#63533=CARTESIAN_POINT('Ctrl Pts',(-17.12616407896,-20.9460001987665,-5.54684314796685));
#63534=CARTESIAN_POINT('Ctrl Pts',(-17.1948942620563,-20.999513169412,-5.55115931070577));
#63535=CARTESIAN_POINT('Ctrl Pts',(-17.2661134846746,-21.0493576657609,
-5.55547547344469));
#63536=CARTESIAN_POINT('Ctrl Pts',(-17.3350127486071,-21.097578482884,-5.55965103763637));
#63537=CARTESIAN_POINT('Ctrl Pts',(-17.4062409575147,-21.1423659457519,
-5.56382660182805));
#63538=CARTESIAN_POINT('Ctrl Pts',(-17.4794157978407,-21.183505877136,-5.56800216601973));
#63539=CARTESIAN_POINT('Ctrl Pts',(-17.5562865253949,-21.2267236886533,
-5.57238862803227));
#63540=CARTESIAN_POINT('Ctrl Pts',(-17.6353051780177,-21.2659155519541,
-5.57677509004481));
#63541=CARTESIAN_POINT('Ctrl Pts',(-17.7160039105556,-21.3008899424784,
-5.58116155205735));
#63542=CARTESIAN_POINT('Ctrl Pts',(-17.7967026430936,-21.3358643330026,
-5.5855480140699));
#63543=CARTESIAN_POINT('Ctrl Pts',(-17.8790808853744,-21.3666211190642,
-5.58993447608243));
#63544=CARTESIAN_POINT('Ctrl Pts',(-17.9626538344086,-21.393029514944,-5.59432093809497));
#63545=CARTESIAN_POINT('Ctrl Pts',(-18.042381468173,-21.4182228213826,-5.59850557248802));
#63546=CARTESIAN_POINT('Ctrl Pts',(-18.123493045634,-21.4395528703718,-5.60269020688107));
#63547=CARTESIAN_POINT('Ctrl Pts',(-18.2055793173495,-21.4568695738795,
-5.60687484127412));
#63548=CARTESIAN_POINT('Ctrl Pts',(-18.2875487494174,-21.474161629203,-5.61105351935806));
#63549=CARTESIAN_POINT('Ctrl Pts',(-18.370489673737,-21.4874515917234,-5.615232197442));
#63550=CARTESIAN_POINT('Ctrl Pts',(-18.4539769469565,-21.4966388918203,
-5.61941087552594));
#63551=CARTESIAN_POINT('Ctrl Pts',(-18.5389606695472,-21.5059908676685,
-5.62366445341137));
#63552=CARTESIAN_POINT('Ctrl Pts',(-18.624510060566,-21.511091508697,-5.62791803129681));
#63553=CARTESIAN_POINT('Ctrl Pts',(-18.7101649534091,-21.5118890387191,
-5.63217160918224));
#63554=CARTESIAN_POINT('Ctrl Pts',(-18.7941592590127,-21.5126711070654,
-5.63634272316019));
#63555=CARTESIAN_POINT('Ctrl Pts',(-18.87825453103,-21.5093154194064,-5.64051383713815));
#63556=CARTESIAN_POINT('Ctrl Pts',(-18.9620126684401,-21.5018255279589,
-5.6446849511161));
#63557=CARTESIAN_POINT('Ctrl Pts',(-19.0457426999984,-21.4943381498168,
-5.64885466543647));
#63558=CARTESIAN_POINT('Ctrl Pts',(-19.1291353638018,-21.4827193639704,
-5.65302437975684));
#63559=CARTESIAN_POINT('Ctrl Pts',(-19.2117557819361,-21.4670247340387,
-5.65719409407722));
#63560=CARTESIAN_POINT('Ctrl Pts',(-19.2943732600814,-21.4513306625894,
-5.66136366002126));
#63561=CARTESIAN_POINT('Ctrl Pts',(-19.3762180954026,-21.4315611221138,
-5.66553322596531));
#63562=CARTESIAN_POINT('Ctrl Pts',(-19.4568650837657,-21.4078228907379,
-5.66970279190935));
#63563=CARTESIAN_POINT('Ctrl Pts',(-19.5403475207508,-21.3832500524311,
-5.67401895464827));
#63564=CARTESIAN_POINT('Ctrl Pts',(-19.6225458049915,-21.3544244012911,
-5.67833511738719));
#63565=CARTESIAN_POINT('Ctrl Pts',(-19.7030067527822,-21.3215201862534,
-5.68265128012611));
#63566=CARTESIAN_POINT('Ctrl Pts',(-19.7808466936617,-21.2896878225597,
-5.68682684431779));
#63567=CARTESIAN_POINT('Ctrl Pts',(-19.8570603406958,-21.2540387751659,
-5.69100240850947));
#63568=CARTESIAN_POINT('Ctrl Pts',(-19.9312606656523,-21.214778579199,-5.69517797270115));
#63569=CARTESIAN_POINT('Ctrl Pts',(-20.0092086726279,-21.173535444066,-5.69956443471369));
#63570=CARTESIAN_POINT('Ctrl Pts',(-20.0849341253745,-21.1283070744553,
-5.70395089672623));
#63571=CARTESIAN_POINT('Ctrl Pts',(-20.1580227463384,-21.0793831854912,
-5.70833735873878));
#63572=CARTESIAN_POINT('Ctrl Pts',(-20.2311113673023,-21.0304592965271,
-5.71272382075132));
#63573=CARTESIAN_POINT('Ctrl Pts',(-20.3015627371329,-20.977840296355,-5.71711028276386));
#63574=CARTESIAN_POINT('Ctrl Pts',(-20.3690044710744,-20.9218630357379,
-5.72149674477641));
#63575=CARTESIAN_POINT('Ctrl Pts',(-20.4324580482223,-20.8691959820087,
-5.72562381401755));
#63576=CARTESIAN_POINT('Ctrl Pts',(-20.493497997814,-20.8133485129555,-5.72975088325869));
#63577=CARTESIAN_POINT('Ctrl Pts',(-20.5517814829091,-20.7545732940418,
-5.73387795249983));
#63578=CARTESIAN_POINT('Ctrl Pts',(-20.6102782700971,-20.6955829734199,
-5.73802012571948));
#63579=CARTESIAN_POINT('Ctrl Pts',(-20.6659979620833,-20.6336436795686,
-5.74216229893913));
#63580=CARTESIAN_POINT('Ctrl Pts',(-20.7186255971236,-20.5690532580103,
-5.74630447215879));
#63581=CARTESIAN_POINT('Ctrl Pts',(-20.7709257203661,-20.5048647949491,
-5.75042086784546));
#63582=CARTESIAN_POINT('Ctrl Pts',(-20.8201718394842,-20.4380584608902,
-5.75453726353214));
#63583=CARTESIAN_POINT('Ctrl Pts',(-20.8660914253506,-20.368963709467,-5.75865365921881));
#63584=CARTESIAN_POINT('Ctrl Pts',(-20.9119829684086,-20.299911153783,-5.76276754104798));
#63585=CARTESIAN_POINT('Ctrl Pts',(-20.9545517475122,-20.228573347296,-5.76688142287715));
#63586=CARTESIAN_POINT('Ctrl Pts',(-20.993566969393,-20.1553108953334,-5.77099530470633));
#63587=CARTESIAN_POINT('Ctrl Pts',(-21.0325708263852,-20.0820697842621,
-5.77510798818761));
#63588=CARTESIAN_POINT('Ctrl Pts',(-21.0680229592545,-20.006905559054,-5.7792206716689));
#63589=CARTESIAN_POINT('Ctrl Pts',(-21.0997379788823,-19.9302043831808,
-5.78333335515018));
#63590=CARTESIAN_POINT('Ctrl Pts',(-21.1318415000294,-19.8525636359715,
-5.78749641803529));
#63591=CARTESIAN_POINT('Ctrl Pts',(-21.1601155043872,-19.7733484709675,
-5.7916594809204));
#63592=CARTESIAN_POINT('Ctrl Pts',(-21.1844181339265,-19.6929797358392,
-5.79582254380551));
#63593=CARTESIAN_POINT('Ctrl Pts',(-21.2084475698834,-19.6135144512045,
-5.79993880837766));
#63594=CARTESIAN_POINT('Ctrl Pts',(-21.2285944016387,-19.5329218806182,
-5.80405507294981));
#63595=CARTESIAN_POINT('Ctrl Pts',(-21.2447724368935,-19.45162162697,-5.80817133752195));
#63596=CARTESIAN_POINT('Ctrl Pts',(-21.2612263672263,-19.3689349046021,
-5.81235779956354));
#63597=CARTESIAN_POINT('Ctrl Pts',(-21.2735747867911,-19.2855166404038,
-5.81654426160514));
#63598=CARTESIAN_POINT('Ctrl Pts',(-21.281781944964,-19.2018142528271,-5.82073072364673));
#63599=CARTESIAN_POINT('Ctrl Pts',(-21.2899891031369,-19.1181118652504,
-5.82491718568832));
#63600=CARTESIAN_POINT('Ctrl Pts',(-21.2940550344004,-19.0341258661346,
-5.82910364772991));
#63601=CARTESIAN_POINT('Ctrl Pts',(-21.2939994369002,-18.9503020392335,
-5.8332901097715));
#63602=CARTESIAN_POINT('Ctrl Pts',(-21.2967673690372,-18.950300203358,-5.8332901097715));
#63603=CARTESIAN_POINT('Ctrl Pts',(-21.2975539709192,-18.8475231740461,
-5.83841759033362));
#63604=CARTESIAN_POINT('Ctrl Pts',(-21.2452320420947,-17.8958349639979,
-5.88593700645621));
#63605=CARTESIAN_POINT('Ctrl Pts',(-20.0538051353946,-16.2277743551153,
-5.97584835813928));
#63606=CARTESIAN_POINT('Ctrl Pts',(-18.0187464898779,-16.3260865960557,
-6.06521460732434));
#63607=CARTESIAN_POINT('Ctrl Pts',(-17.2449841505655,-16.8629690205255,
-6.11218892094892));
#63608=CARTESIAN_POINT('Ctrl Pts',(-17.1725993332886,-16.9194746534894,
-6.11677129901302));
#63609=CARTESIAN_POINT('',(-21.2939992944986,-18.9539005700933,-5.76670989019962));
#63610=CARTESIAN_POINT('Ctrl Pts',(-21.293999294499,-18.9539005695104,-5.76670989022851));
#63611=CARTESIAN_POINT('Ctrl Pts',(-21.2940618231948,-18.8696766480678,
-5.77088500205647));
#63612=CARTESIAN_POINT('Ctrl Pts',(-21.2899635861128,-18.7854119279347,
-5.77506011388444));
#63613=CARTESIAN_POINT('Ctrl Pts',(-21.2817191504239,-18.7015461508316,
-5.7792352257124));
#63614=CARTESIAN_POINT('Ctrl Pts',(-21.2734754980237,-18.6176883416611,
-5.78340994087069));
#63615=CARTESIAN_POINT('Ctrl Pts',(-21.2610864747303,-18.5342298557722,
-5.78758465602898));
#63616=CARTESIAN_POINT('Ctrl Pts',(-21.2446185572459,-18.4516056954637,
-5.79175937118727));
#63617=CARTESIAN_POINT('Ctrl Pts',(-21.2281473245846,-18.3689649019827,
-5.79593492676267));
#63618=CARTESIAN_POINT('Ctrl Pts',(-21.2075956572652,-18.2871592164316,
-5.80011048233806));
#63619=CARTESIAN_POINT('Ctrl Pts',(-21.1830809475489,-18.2066125085882,
-5.80428603791345));
#63620=CARTESIAN_POINT('Ctrl Pts',(-21.1585369190254,-18.1259694694636,
-5.8084665873195));
#63621=CARTESIAN_POINT('Ctrl Pts',(-21.1300205198882,-18.0465888526481,
-5.81264713672554));
#63622=CARTESIAN_POINT('Ctrl Pts',(-21.0976986239761,-17.9688780263805,
-5.81682768613158));
#63623=CARTESIAN_POINT('Ctrl Pts',(-21.065355928357,-17.8911171918331,-5.8210109257945));
#63624=CARTESIAN_POINT('Ctrl Pts',(-21.0292030575735,-17.8150287001824,
-5.82519416545742));
#63625=CARTESIAN_POINT('Ctrl Pts',(-20.9894534545794,-17.740996402059,-5.82937740512034));
#63626=CARTESIAN_POINT('Ctrl Pts',(-20.949632004209,-17.6668302906149,-5.83356820598567));
#63627=CARTESIAN_POINT('Ctrl Pts',(-20.9062010761476,-17.5947281861657,
-5.83775900685099));
#63628=CARTESIAN_POINT('Ctrl Pts',(-20.859418003607,-17.5250457926257,-5.84194980771632));
#63629=CARTESIAN_POINT('Ctrl Pts',(-20.8291383592866,-17.4799449051208,
-5.84466224092621));
#63630=CARTESIAN_POINT('Ctrl Pts',(-20.7974553185201,-17.435857034571,-5.84737467413609));
#63631=CARTESIAN_POINT('Ctrl Pts',(-20.7644472985012,-17.392870830236,-5.85008710734598));
#63632=CARTESIAN_POINT('Ctrl Pts',(-20.7135238341689,-17.3265534188316,
-5.85427174173903));
#63633=CARTESIAN_POINT('Ctrl Pts',(-20.6592531496868,-17.262610070515,-5.85845637613208));
#63634=CARTESIAN_POINT('Ctrl Pts',(-20.6018847443059,-17.2013982228989,
-5.86264101052513));
#63635=CARTESIAN_POINT('Ctrl Pts',(-20.5445979957492,-17.1402735027715,
-5.86681968860907));
#63636=CARTESIAN_POINT('Ctrl Pts',(-20.4842225962896,-17.0818728934348,
-5.87099836669301));
#63637=CARTESIAN_POINT('Ctrl Pts',(-20.4210494366143,-17.0265223453856,
-5.87517704477696));
#63638=CARTESIAN_POINT('Ctrl Pts',(-20.3567439434536,-16.9701796785424,
-5.87943062266239));
#63639=CARTESIAN_POINT('Ctrl Pts',(-20.2895396974698,-16.9169978755988,
-5.88368420054783));
#63640=CARTESIAN_POINT('Ctrl Pts',(-20.2197842460677,-16.867282951061,-5.88793777843326));
#63641=CARTESIAN_POINT('Ctrl Pts',(-20.1513811402077,-16.8185318473461,
-5.89210889241121));
#63642=CARTESIAN_POINT('Ctrl Pts',(-20.0805252582504,-16.7731146765031,
-5.89628000638917));
#63643=CARTESIAN_POINT('Ctrl Pts',(-20.0075777510545,-16.7312794610715,
-5.90045112036712));
#63644=CARTESIAN_POINT('Ctrl Pts',(-19.9346547220991,-16.6894582838504,
-5.90462083468749));
#63645=CARTESIAN_POINT('Ctrl Pts',(-19.8596418605523,-16.6512169036013,
-5.90879054900787));
#63646=CARTESIAN_POINT('Ctrl Pts',(-19.7829274662086,-16.6167588624227,
-5.91296026332824));
#63647=CARTESIAN_POINT('Ctrl Pts',(-19.7062158016923,-16.5823020474091,
-5.91712982927229));
#63648=CARTESIAN_POINT('Ctrl Pts',(-19.6278031447566,-16.5516284915072,
-5.92129939521634));
#63649=CARTESIAN_POINT('Ctrl Pts',(-19.5480992,-16.5248942147983,-5.92546896116038));
#63650=CARTESIAN_POINT('Ctrl Pts',(-19.4655929628713,-16.4972199939008,
-5.9297851238993));
#63651=CARTESIAN_POINT('Ctrl Pts',(-19.3817034451241,-16.4737673840696,
-5.93410128663822));
#63652=CARTESIAN_POINT('Ctrl Pts',(-19.2969019322694,-16.4546531248848,
-5.93841744937714));
#63653=CARTESIAN_POINT('Ctrl Pts',(-19.2148628197763,-16.4361615106825,
-5.94259301356882));
#63654=CARTESIAN_POINT('Ctrl Pts',(-19.1319706883696,-16.4217299783601,
-5.9467685777605));
#63655=CARTESIAN_POINT('Ctrl Pts',(-19.0486605152115,-16.411411729507,-5.95094414195218));
#63656=CARTESIAN_POINT('Ctrl Pts',(-18.9611425432584,-16.4005723304336,
-5.95533060396472));
#63657=CARTESIAN_POINT('Ctrl Pts',(-18.8731637715279,-16.3942727005953,
-5.95971706597726));
#63658=CARTESIAN_POINT('Ctrl Pts',(-18.7852297301449,-16.3925126461048,
-5.9641035279898));
#63659=CARTESIAN_POINT('Ctrl Pts',(-18.6972956887618,-16.3907525916143,
-5.96848999000234));
#63660=CARTESIAN_POINT('Ctrl Pts',(-18.609406955249,-16.3935320181048,-5.97287645201488));
#63661=CARTESIAN_POINT('Ctrl Pts',(-18.5220617179687,-16.4007880988421,
-5.97726291402742));
#63662=CARTESIAN_POINT('Ctrl Pts',(-18.4387429644685,-16.4077096851948,
-5.98144716675304));
#63663=CARTESIAN_POINT('Ctrl Pts',(-18.3556086019078,-16.4187300407395,
-5.98563141947867));
#63664=CARTESIAN_POINT('Ctrl Pts',(-18.273094108763,-16.4338328571314,-5.98981567220429));
#63665=CARTESIAN_POINT('Ctrl Pts',(-18.190691343874,-16.4489152236451,-5.99399425926754));
#63666=CARTESIAN_POINT('Ctrl Pts',(-18.1089072302701,-16.4680689925798,
-5.99817284633079));
#63667=CARTESIAN_POINT('Ctrl Pts',(-18.0281732667358,-16.4912260114733,
-6.00235143339404));
#63668=CARTESIAN_POINT('Ctrl Pts',(-17.9475320674901,-16.5143564226754,
-6.00652521921084));
#63669=CARTESIAN_POINT('Ctrl Pts',(-17.8679390598742,-16.541480815389,-6.01069900502764));
#63670=CARTESIAN_POINT('Ctrl Pts',(-17.7898152017669,-16.572480076405,-6.01487279084444));
#63671=CARTESIAN_POINT('Ctrl Pts',(-17.7117448631501,-16.603458101083,-6.01904371736965));
#63672=CARTESIAN_POINT('Ctrl Pts',(-17.6351421012726,-16.6383055523455,
-6.02321464389486));
#63673=CARTESIAN_POINT('Ctrl Pts',(-17.5604112612823,-16.6768539668067,
-6.02738557042007));
#63674=CARTESIAN_POINT('Ctrl Pts',(-17.4856945971113,-16.7153950689542,
-6.03155570575518));
#63675=CARTESIAN_POINT('Ctrl Pts',(-17.4128495626117,-16.7576355380395,
-6.0357258410903));
#63676=CARTESIAN_POINT('Ctrl Pts',(-17.3422580869924,-16.8033598608474,
-6.03989597642541));
#63677=CARTESIAN_POINT('Ctrl Pts',(-17.2847682206377,-16.8405978585563,
-6.04329214460284));
#63678=CARTESIAN_POINT('Ctrl Pts',(-17.2287727032861,-16.8801455850515,
-6.04668831278028));
#63679=CARTESIAN_POINT('Ctrl Pts',(-17.1744641548914,-16.9218650419685,
-6.05008448095771));
#63680=CARTESIAN_POINT('Ctrl Pts',(-17.1744641548914,-16.9218650419685,
-5.25018234058848));
#63681=CARTESIAN_POINT('Ctrl Pts',(-17.1078622797925,-16.9730281487153,
-5.25435377231504));
#63682=CARTESIAN_POINT('Ctrl Pts',(-17.0437276383886,-17.0275129995409,
-5.25852520404159));
#63683=CARTESIAN_POINT('Ctrl Pts',(-16.9824037471442,-17.0850477866369,
-5.26269663576815));
#63684=CARTESIAN_POINT('Ctrl Pts',(-16.9211031913488,-17.1425606801436,
-5.26686648014873));
#63685=CARTESIAN_POINT('Ctrl Pts',(-16.8626115968344,-17.2031208907266,
-5.27103632452931));
#63686=CARTESIAN_POINT('Ctrl Pts',(-16.8072380311628,-17.2664175144946,
-5.27520616890989));
#63687=CARTESIAN_POINT('Ctrl Pts',(-16.7518689259269,-17.329709039611,-5.27937567740234));
#63688=CARTESIAN_POINT('Ctrl Pts',(-16.6996176528133,-17.3957361932332,
-5.2835451858948));
#63689=CARTESIAN_POINT('Ctrl Pts',(-16.6507542226063,-17.4641535593445,
-5.28771469438725));
#63690=CARTESIAN_POINT('Ctrl Pts',(-16.6018800708253,-17.5325859375384,
-5.29188511774986));
#63691=CARTESIAN_POINT('Ctrl Pts',(-16.556395504268,-17.603409194585,-5.29605554111247));
#63692=CARTESIAN_POINT('Ctrl Pts',(-16.514527493463,-17.676248538027,-5.30022596447508));
#63693=CARTESIAN_POINT('Ctrl Pts',(-16.4726122042834,-17.7491701334243,
-5.30440109718101));
#63694=CARTESIAN_POINT('Ctrl Pts',(-16.4343218488226,-17.8241119583259,
-5.30857622988695));
#63695=CARTESIAN_POINT('Ctrl Pts',(-16.3998373803061,-17.9006747102711,
-5.31275136259289));
#63696=CARTESIAN_POINT('Ctrl Pts',(-16.3653298237343,-17.9772887225407,
-5.31692929063536));
#63697=CARTESIAN_POINT('Ctrl Pts',(-16.3346333926338,-18.0555253938272,
-5.32110721867783));
#63698=CARTESIAN_POINT('Ctrl Pts',(-16.307879983328,-18.134967770095,-5.32528514672029));
#63699=CARTESIAN_POINT('Ctrl Pts',(-16.2810838554183,-18.2145369962668,
-5.3294697458846));
#63700=CARTESIAN_POINT('Ctrl Pts',(-16.2582434356432,-18.2953153270739,
-5.3336543450489));
#63701=CARTESIAN_POINT('Ctrl Pts',(-16.2394399881205,-18.3768736250774,
-5.3378389442132));
#63702=CARTESIAN_POINT('Ctrl Pts',(-16.2341302779918,-18.3999040252453,
-5.33902058968222));
#63703=CARTESIAN_POINT('Ctrl Pts',(-16.2291421521855,-18.4229965796705,
-5.34020223515123));
#63704=CARTESIAN_POINT('Ctrl Pts',(-16.2244766916358,-18.4461415565825,
-5.34138388062024));
#63705=CARTESIAN_POINT('Ctrl Pts',(-16.2079546068079,-18.5281062989289,
-5.34556851501329));
#63706=CARTESIAN_POINT('Ctrl Pts',(-16.1954216323759,-18.6110338790213,
-5.34975314940633));
#63707=CARTESIAN_POINT('Ctrl Pts',(-16.1869832270606,-18.6945013429833,
-5.35393778379938));
#63708=CARTESIAN_POINT('Ctrl Pts',(-16.1785568327709,-18.7778500013414,
-5.35811646188331));
#63709=CARTESIAN_POINT('Ctrl Pts',(-16.1742134770096,-18.8617365633851,
-5.36229513996724));
#63710=CARTESIAN_POINT('Ctrl Pts',(-16.174007684269,-18.9457275683916,-5.36647381805118));
#63711=CARTESIAN_POINT('Ctrl Pts',(-16.1737982028414,-19.0312240517999,
-5.37072739593661));
#63712=CARTESIAN_POINT('Ctrl Pts',(-16.1778761703229,-19.1168282866473,
-5.37498097382205));
#63713=CARTESIAN_POINT('Ctrl Pts',(-16.1862438519478,-19.2020772082025,
-5.37923455170749));
#63714=CARTESIAN_POINT('Ctrl Pts',(-16.1944493097363,-19.2856734130638,
-5.38340566568544));
#63715=CARTESIAN_POINT('Ctrl Pts',(-16.2067795899914,-19.3689274796561,
-5.38757677966339));
#63716=CARTESIAN_POINT('Ctrl Pts',(-16.2231843067497,-19.4514041995496,
-5.39174789364134));
#63717=CARTESIAN_POINT('Ctrl Pts',(-16.2395835187467,-19.5338532435831,
-5.39591760796171));
#63718=CARTESIAN_POINT('Ctrl Pts',(-16.2600543622647,-19.6155250081436,
-5.40008732228208));
#63719=CARTESIAN_POINT('Ctrl Pts',(-16.2844950829499,-19.6959930519482,
-5.40425703660244));
#63720=CARTESIAN_POINT('Ctrl Pts',(-16.3089349339293,-19.7764582323547,
-5.40842660254649));
#63721=CARTESIAN_POINT('Ctrl Pts',(-16.3373442466931,-19.8557193372403,
-5.41259616849054));
#63722=CARTESIAN_POINT('Ctrl Pts',(-16.3695713807102,-19.9333650209191,
-5.41676573443458));
#63723=CARTESIAN_POINT('Ctrl Pts',(-16.4029315810029,-20.0137406310497,
-5.42108189717351));
#63724=CARTESIAN_POINT('Ctrl Pts',(-16.4403828646775,-20.0923846228539,
-5.42539805991243));
#63725=CARTESIAN_POINT('Ctrl Pts',(-16.4817035150007,-20.1688650474311,
-5.42971422265136));
#63726=CARTESIAN_POINT('Ctrl Pts',(-16.5216781494857,-20.2428541302221,
-5.43388978684304));
#63727=CARTESIAN_POINT('Ctrl Pts',(-16.5652736482193,-20.3148180591345,
-5.43806535103472));
#63728=CARTESIAN_POINT('Ctrl Pts',(-16.6122442629254,-20.3843940073146,
-5.44224091522641));
#63729=CARTESIAN_POINT('Ctrl Pts',(-16.6615872517182,-20.4574840712362,
-5.44662737723895));
#63730=CARTESIAN_POINT('Ctrl Pts',(-16.7146549198489,-20.5279381144878,
-5.4510138392515));
#63731=CARTESIAN_POINT('Ctrl Pts',(-16.7711149075846,-20.5953752200801,
-5.45540030126404));
#63732=CARTESIAN_POINT('Ctrl Pts',(-16.8275748953203,-20.6628123256725,
-5.45978676327659));
#63733=CARTESIAN_POINT('Ctrl Pts',(-16.8874267520076,-20.7272321203105,
-5.46417322528913));
#63734=CARTESIAN_POINT('Ctrl Pts',(-16.9502957329767,-20.788300380603,-5.46855968730168));
#63735=CARTESIAN_POINT('Ctrl Pts',(-17.0102720189371,-20.8465587997145,
-5.47274432169472));
#63736=CARTESIAN_POINT('Ctrl Pts',(-17.0732171288673,-20.9019841740837,
-5.47692895608777));
#63737=CARTESIAN_POINT('Ctrl Pts',(-17.1388325082967,-20.9542588927042,
-5.48111359048082));
#63738=CARTESIAN_POINT('Ctrl Pts',(-17.204354492355,-21.006459204733,-5.48529226856475));
#63739=CARTESIAN_POINT('Ctrl Pts',(-17.2725388396022,-21.0555174845771,
-5.48947094664869));
#63740=CARTESIAN_POINT('Ctrl Pts',(-17.3430505912408,-21.1011532616992,
-5.49364962473263));
#63741=CARTESIAN_POINT('Ctrl Pts',(-17.4148262153517,-21.1476070273285,
-5.49790320261807));
#63742=CARTESIAN_POINT('Ctrl Pts',(-17.4890131561474,-21.190514050739,-5.5021567805035));
#63743=CARTESIAN_POINT('Ctrl Pts',(-17.5652232755989,-21.2296217790709,
-5.50641035838894));
#63744=CARTESIAN_POINT('Ctrl Pts',(-17.6399559131731,-21.2679713277767,
-5.5105814723669));
#63745=CARTESIAN_POINT('Ctrl Pts',(-17.7166335547755,-21.3026673605994,
-5.51475258634485));
#63746=CARTESIAN_POINT('Ctrl Pts',(-17.7948629860233,-21.3335166740921,
-5.51892370032281));
#63747=CARTESIAN_POINT('Ctrl Pts',(-17.8730661666299,-21.3643556357998,
-5.52309341464318));
#63748=CARTESIAN_POINT('Ctrl Pts',(-17.9528196751245,-21.3913502731114,
-5.52726312896355));
#63749=CARTESIAN_POINT('Ctrl Pts',(-18.0337098641723,-21.4143553207574,
-5.53143284328393));
#63750=CARTESIAN_POINT('Ctrl Pts',(-18.1145971747999,-21.4373595497851,
-5.53560240922797));
#63751=CARTESIAN_POINT('Ctrl Pts',(-18.1966206428405,-21.4563743463907,
-5.53977197517201));
#63752=CARTESIAN_POINT('Ctrl Pts',(-18.2793523115258,-21.4713045626452,
-5.54394154111605));
#63753=CARTESIAN_POINT('Ctrl Pts',(-18.3649927236217,-21.4867597068849,
-5.54825770385497));
#63754=CARTESIAN_POINT('Ctrl Pts',(-18.4513915445807,-21.497837605271,-5.55257386659389));
#63755=CARTESIAN_POINT('Ctrl Pts',(-18.5380655626724,-21.5044908807416,
-5.55689002933282));
#63756=CARTESIAN_POINT('Ctrl Pts',(-18.6219161837412,-21.5109274264635,
-5.5610655935245));
#63757=CARTESIAN_POINT('Ctrl Pts',(-18.7060238760283,-21.5132232209822,
-5.56524115771618));
#63758=CARTESIAN_POINT('Ctrl Pts',(-18.7899505406875,-21.5113885084131,
-5.56941672190786));
#63759=CARTESIAN_POINT('Ctrl Pts',(-18.8781161416618,-21.5094611288736,
-5.5738031839204));
#63760=CARTESIAN_POINT('Ctrl Pts',(-18.9660813646935,-21.5029750554617,
-5.57818964593294));
#63761=CARTESIAN_POINT('Ctrl Pts',(-19.0533460188562,-21.492003566974,-5.58257610794549));
#63762=CARTESIAN_POINT('Ctrl Pts',(-19.140610673019,-21.4810320784863,-5.58696256995803));
#63763=CARTESIAN_POINT('Ctrl Pts',(-19.2271742005006,-21.4655753517935,
-5.59134903197057));
#63764=CARTESIAN_POINT('Ctrl Pts',(-19.3125527301388,-21.4457675790757,
-5.59573549398311));
#63765=CARTESIAN_POINT('Ctrl Pts',(-19.394002867067,-21.4268711913428,-5.59992012837616));
#63766=CARTESIAN_POINT('Ctrl Pts',(-19.4746778298126,-21.4039450190917,
-5.60410476276921));
#63767=CARTESIAN_POINT('Ctrl Pts',(-19.55414895591,-21.3770681825713,-5.60828939716226));
#63768=CARTESIAN_POINT('Ctrl Pts',(-19.6335069646959,-21.350229601901,-5.6124680752462));
#63769=CARTESIAN_POINT('Ctrl Pts',(-19.7116641083503,-21.3194516726887,
-5.61664675333015));
#63770=CARTESIAN_POINT('Ctrl Pts',(-19.7882032486926,-21.2848642288924,
-5.62082543141409));
#63771=CARTESIAN_POINT('Ctrl Pts',(-19.8661142981179,-21.2496568300237,
-5.62507900929953));
#63772=CARTESIAN_POINT('Ctrl Pts',(-19.9423482986086,-21.2105021111285,
-5.62933258718496));
#63773=CARTESIAN_POINT('Ctrl Pts',(-20.0164828014234,-21.167589732792,-5.63358616507039));
#63774=CARTESIAN_POINT('Ctrl Pts',(-20.0891800622396,-21.1255092946461,
-5.63775727904835));
#63775=CARTESIAN_POINT('Ctrl Pts',(-20.1598580881702,-21.079815837063,-5.6419283930263));
#63776=CARTESIAN_POINT('Ctrl Pts',(-20.2281415862037,-21.0307354137496,
-5.64609950700425));
#63777=CARTESIAN_POINT('Ctrl Pts',(-20.2964021710499,-20.9816714598463,
-5.65026922132462));
#63778=CARTESIAN_POINT('Ctrl Pts',(-20.3622694505382,-20.9292230656518,
-5.65443893564499));
#63779=CARTESIAN_POINT('Ctrl Pts',(-20.4253973801084,-20.8736594137782,
-5.65860864996536));
#63780=CARTESIAN_POINT('Ctrl Pts',(-20.4885230633161,-20.8180977390977,
-5.6627782159094));
#63781=CARTESIAN_POINT('Ctrl Pts',(-20.5489092456569,-20.7594213317292,
-5.66694778185344));
#63782=CARTESIAN_POINT('Ctrl Pts',(-20.6062442778983,-20.6979385338199,
-5.67111734779749));
#63783=CARTESIAN_POINT('Ctrl Pts',(-20.6655951391429,-20.6342940765832,
-5.67543351053641));
#63784=CARTESIAN_POINT('Ctrl Pts',(-20.7216759416721,-20.5676425973539,
-5.67974967327533));
#63785=CARTESIAN_POINT('Ctrl Pts',(-20.7741852955294,-20.4983647564225,
-5.68406583601425));
#63786=CARTESIAN_POINT('Ctrl Pts',(-20.8249841627079,-20.4313436338726,
-5.68824140020593));
#63787=CARTESIAN_POINT('Ctrl Pts',(-20.8724404611872,-20.3618650450197,
-5.69241696439762));
#63788=CARTESIAN_POINT('Ctrl Pts',(-20.9163256700511,-20.2903029066083,
-5.6965925285893));
#63789=CARTESIAN_POINT('Ctrl Pts',(-20.9624274164874,-20.2151263347086,
-5.70097899060184));
#63790=CARTESIAN_POINT('Ctrl Pts',(-21.0045875620259,-20.1376507144176,
-5.70536545261438));
#63791=CARTESIAN_POINT('Ctrl Pts',(-21.0425969786767,-20.0583362915701,
-5.70975191462692));
#63792=CARTESIAN_POINT('Ctrl Pts',(-21.0806063953274,-19.9790218687225,
-5.71413837663946));
#63793=CARTESIAN_POINT('Ctrl Pts',(-21.1144649298774,-19.897869208087,-5.718524838652));
#63794=CARTESIAN_POINT('Ctrl Pts',(-21.144023506431,-19.8153578044185,-5.72291130066454));
#63795=CARTESIAN_POINT('Ctrl Pts',(-21.1768030234138,-19.7238552940413,
-5.72777574688623));
#63796=CARTESIAN_POINT('Ctrl Pts',(-21.2043967060823,-19.6304025057852,
-5.73264019310792));
#63797=CARTESIAN_POINT('Ctrl Pts',(-21.2266026211961,-19.5355513454757,
-5.7375046393296));
#63798=CARTESIAN_POINT('Ctrl Pts',(-21.2488226674987,-19.4406398246877,
-5.74237218114127));
#63799=CARTESIAN_POINT('Ctrl Pts',(-21.2656479288596,-19.3443282665163,
-5.74723972295294));
#63800=CARTESIAN_POINT('Ctrl Pts',(-21.2769239065511,-19.2471914725919,
-5.75210726476461));
#63801=CARTESIAN_POINT('Ctrl Pts',(-21.2881998842426,-19.1500546786674,
-5.75697480657628));
#63802=CARTESIAN_POINT('Ctrl Pts',(-21.2939263955806,-19.0520927805187,
-5.76184234838795));
#63803=CARTESIAN_POINT('Ctrl Pts',(-21.2939992944986,-18.9539005700933,
-5.76670989019962));
#63804=CARTESIAN_POINT('Origin',(-18.734,-18.952,1.76670989022851));
#63805=CARTESIAN_POINT('',(-17.1718943060142,-16.9185142398779,-4.45010593052277));
#63806=CARTESIAN_POINT('',(-17.1769969348074,-16.9251725137323,-4.51667470085173));
#63807=CARTESIAN_POINT('',(-17.1744641548914,-16.9218650419685,1.76670989022851));
#63808=CARTESIAN_POINT('',(-21.2938494922829,-18.9508032548851,-5.03329016024732));
#63809=CARTESIAN_POINT('Ctrl Pts',(-17.1769969348074,-16.9251725137323,
-4.51667470085173));
#63810=CARTESIAN_POINT('Ctrl Pts',(-16.8552506861943,-17.1716046543912,
-4.53675462878232));
#63811=CARTESIAN_POINT('Ctrl Pts',(-16.0276178705895,-18.1629200290128,
-4.59922649227339));
#63812=CARTESIAN_POINT('Ctrl Pts',(-16.1629700483809,-20.5498410269921,
-4.70409029132494));
#63813=CARTESIAN_POINT('Ctrl Pts',(-18.6858816905041,-21.9787103574595,
-4.83126609800637));
#63814=CARTESIAN_POINT('Ctrl Pts',(-20.9008594909828,-20.8156360190963,
-4.94099937082189));
#63815=CARTESIAN_POINT('Ctrl Pts',(-21.288210216193,-19.4541225063383,-5.00834070807693));
#63816=CARTESIAN_POINT('Ctrl Pts',(-21.2903252254699,-18.9508059208324,
-5.0332901097715));
#63817=CARTESIAN_POINT('Ctrl Pts',(-21.2939997202205,-18.9508031412445,
-5.03329016239894));
#63818=CARTESIAN_POINT('Ctrl Pts',(-21.2939564765218,-18.8583078019835,
-5.03786858507833));
#63819=CARTESIAN_POINT('Ctrl Pts',(-21.2888961385929,-18.7659792628466,
-5.04244700775773));
#63820=CARTESIAN_POINT('Ctrl Pts',(-21.2788976615006,-18.6743385289801,
-5.04702543043713));
#63821=CARTESIAN_POINT('Ctrl Pts',(-21.2688681118673,-18.5824130006966,
-5.05161808160601));
#63822=CARTESIAN_POINT('Ctrl Pts',(-21.2538698091559,-18.4911798450256,
-5.05621073277489));
#63823=CARTESIAN_POINT('Ctrl Pts',(-21.2340326305246,-18.40114897993,-5.06080338394377));
#63824=CARTESIAN_POINT('Ctrl Pts',(-21.2141037578095,-18.3107019620212,
-5.06541726388461));
#63825=CARTESIAN_POINT('Ctrl Pts',(-21.1892913049386,-18.2214686542029,
-5.07003114382545));
#63826=CARTESIAN_POINT('Ctrl Pts',(-21.1597755903596,-18.1339457321084,
-5.0746450237663));
#63827=CARTESIAN_POINT('Ctrl Pts',(-21.1363775884172,-18.0645636578345,
-5.07830258630061));
#63828=CARTESIAN_POINT('Ctrl Pts',(-21.1100249393917,-17.9962560714796,
-5.08196014883493));
#63829=CARTESIAN_POINT('Ctrl Pts',(-21.0808281256644,-17.9292596866307,
-5.08561771136924));
#63830=CARTESIAN_POINT('Ctrl Pts',(-21.0474239145964,-17.8526088095457,
-5.08980234576229));
#63831=CARTESIAN_POINT('Ctrl Pts',(-21.0101982941979,-17.7774535557438,
-5.09398698015533));
#63832=CARTESIAN_POINT('Ctrl Pts',(-20.9693070771845,-17.7042010295369,
-5.09817161454838));
#63833=CARTESIAN_POINT('Ctrl Pts',(-20.9284740637572,-17.6310527692342,
-5.10235029263232));
#63834=CARTESIAN_POINT('Ctrl Pts',(-20.8839860396696,-17.5598022552459,
-5.10652897071627));
#63835=CARTESIAN_POINT('Ctrl Pts',(-20.8360465870686,-17.4908360304904,
-5.11070764880022));
#63836=CARTESIAN_POINT('Ctrl Pts',(-20.7872478542333,-17.4206336357213,
-5.11496122668565));
#63837=CARTESIAN_POINT('Ctrl Pts',(-20.7348729347517,-17.352798669429,-5.11921480457109));
#63838=CARTESIAN_POINT('Ctrl Pts',(-20.6791852047646,-17.2877120083456,
-5.12346838245653));
#63839=CARTESIAN_POINT('Ctrl Pts',(-20.6245770900889,-17.2238871791935,
-5.12763949643448));
#63840=CARTESIAN_POINT('Ctrl Pts',(-20.5667837820755,-17.1627054093254,
-5.13181061041243));
#63841=CARTESIAN_POINT('Ctrl Pts',(-20.5060958601737,-17.1044945839443,
-5.13598172439038));
#63842=CARTESIAN_POINT('Ctrl Pts',(-20.4454283026902,-17.0463032917677,
-5.14015143871076));
#63843=CARTESIAN_POINT('Ctrl Pts',(-20.3818683920876,-16.9910812823424,
-5.14432115303113));
#63844=CARTESIAN_POINT('Ctrl Pts',(-20.3157437934271,-16.9391198316952,
-5.1484908673515));
#63845=CARTESIAN_POINT('Ctrl Pts',(-20.2496215477636,-16.8871602300594,
-5.15266043329554));
#63846=CARTESIAN_POINT('Ctrl Pts',(-20.1809351577375,-16.8384612400848,
-5.15682999923958));
#63847=CARTESIAN_POINT('Ctrl Pts',(-20.1100445342429,-16.7932731901002,
-5.16099956518362));
#63848=CARTESIAN_POINT('Ctrl Pts',(-20.0366614838791,-16.7464963840235,
-5.16531572792255));
#63849=CARTESIAN_POINT('Ctrl Pts',(-19.9609167591474,-16.703482284346,-5.16963189066146));
#63850=CARTESIAN_POINT('Ctrl Pts',(-19.8832395142303,-16.6644579700185,
-5.17394805340038));
#63851=CARTESIAN_POINT('Ctrl Pts',(-19.8080925973962,-16.6267048686257,
-5.17812361759206));
#63852=CARTESIAN_POINT('Ctrl Pts',(-19.731137580502,-16.5926857570977,-5.18229918178375));
#63853=CARTESIAN_POINT('Ctrl Pts',(-19.6527837251096,-16.5625572895602,
-5.18647474597543));
#63854=CARTESIAN_POINT('Ctrl Pts',(-19.5704724027499,-16.5309071047511,
-5.19086120798797));
#63855=CARTESIAN_POINT('Ctrl Pts',(-19.4866177726054,-16.5035511069691,
-5.19524767000051));
#63856=CARTESIAN_POINT('Ctrl Pts',(-19.4017104542219,-16.4806111699446,
-5.19963413201305));
#63857=CARTESIAN_POINT('Ctrl Pts',(-19.3168031358384,-16.45767123292,-5.20402059402559));
#63858=CARTESIAN_POINT('Ctrl Pts',(-19.2308437124363,-16.439147404523,-5.20840705603813));
#63859=CARTESIAN_POINT('Ctrl Pts',(-19.1443308019265,-16.4250990060965,
-5.21279351805067));
#63860=CARTESIAN_POINT('Ctrl Pts',(-19.0590101764576,-16.4112442168689,
-5.21711952766357));
#63861=CARTESIAN_POINT('Ctrl Pts',(-18.9728228820038,-16.4016888933807,
-5.22144553727647));
#63862=CARTESIAN_POINT('Ctrl Pts',(-18.886240530398,-16.3965308022001,-5.22577154688938));
#63863=CARTESIAN_POINT('Ctrl Pts',(-18.8026253638558,-16.3915494792733,
-5.22994930375942));
#63864=CARTESIAN_POINT('Ctrl Pts',(-18.7186422840508,-16.3906689763345,
-5.23412706062947));
#63865=CARTESIAN_POINT('Ctrl Pts',(-18.6347264524453,-16.3939255752117,
-5.23830481749952));
#63866=CARTESIAN_POINT('Ctrl Pts',(-18.5508928195399,-16.3971789841283,
-5.24247848210023));
#63867=CARTESIAN_POINT('Ctrl Pts',(-18.4671267610676,-16.404561430684,-5.24665214670094));
#63868=CARTESIAN_POINT('Ctrl Pts',(-18.3838655026501,-16.4160572100764,
-5.25082581130166));
#63869=CARTESIAN_POINT('Ctrl Pts',(-18.3006608220041,-16.4275451778456,
-5.25499663980973));
#63870=CARTESIAN_POINT('Ctrl Pts',(-18.2179607144013,-16.4431408635637,
-5.2591674683178));
#63871=CARTESIAN_POINT('Ctrl Pts',(-18.1361979753704,-16.4627766794944,
-5.26333829682587));
#63872=CARTESIAN_POINT('Ctrl Pts',(-18.0544662678843,-16.4824050430121,
-5.26750754237265));
#63873=CARTESIAN_POINT('Ctrl Pts',(-17.9736716684704,-16.5060703811549,
-5.27167678791943));
#63874=CARTESIAN_POINT('Ctrl Pts',(-17.8942361136643,-16.5336541572376,
-5.27584603346621));
#63875=CARTESIAN_POINT('Ctrl Pts',(-17.8147812266298,-16.5612446463829,
-5.28001629368214));
#63876=CARTESIAN_POINT('Ctrl Pts',(-17.7366864815223,-16.5927553328241,
-5.28418655389806));
#63877=CARTESIAN_POINT('Ctrl Pts',(-17.6603570885801,-16.6280183092894,
-5.28835681411399));
#63878=CARTESIAN_POINT('Ctrl Pts',(-17.5840157549879,-16.6632868021469,
-5.29252772670794));
#63879=CARTESIAN_POINT('Ctrl Pts',(-17.5094407357015,-16.7023085494237,
-5.29669863930189));
#63880=CARTESIAN_POINT('Ctrl Pts',(-17.4370140419547,-16.7448689607018,
-5.30086955189584));
#63881=CARTESIAN_POINT('Ctrl Pts',(-17.3645257074469,-16.787465594207,-5.30504401426147));
#63882=CARTESIAN_POINT('Ctrl Pts',(-17.2941897360827,-16.8336066562081,
-5.3092184766271));
#63883=CARTESIAN_POINT('Ctrl Pts',(-17.226359753212,-16.883033860532,-5.31339293899273));
#63884=CARTESIAN_POINT('Ctrl Pts',(-17.2088933290245,-16.895761514006,-5.31446787558194));
#63885=CARTESIAN_POINT('Ctrl Pts',(-17.1915929037904,-16.9087068537485,
-5.31554281217115));
#63886=CARTESIAN_POINT('Ctrl Pts',(-17.1744641548914,-16.9218650419685,
-5.31661774876036));
#63887=CARTESIAN_POINT('',(-21.2942629789487,-18.9528355653121,-4.96670989022851));
#63888=CARTESIAN_POINT('Ctrl Pts',(-21.2939998636668,-18.952835479442,-4.96670989022851));
#63889=CARTESIAN_POINT('Ctrl Pts',(-21.2940269378476,-18.8698772454869,
-4.97085977152528));
#63890=CARTESIAN_POINT('Ctrl Pts',(-21.2900172964774,-18.7867551328103,
-4.97500965282205));
#63891=CARTESIAN_POINT('Ctrl Pts',(-21.2819493183893,-18.7038986680417,
-4.97915953411883));
#63892=CARTESIAN_POINT('Ctrl Pts',(-21.273892503302,-18.6211568449806,-4.98330367356456));
#63893=CARTESIAN_POINT('Ctrl Pts',(-21.2617885455565,-18.5386804021309,
-4.98744781301029));
#63894=CARTESIAN_POINT('Ctrl Pts',(-21.2456678375727,-18.456899329729,-4.99159195245603));
#63895=CARTESIAN_POINT('Ctrl Pts',(-21.2295645603719,-18.3752066844683,
-4.99573161098224));
#63896=CARTESIAN_POINT('Ctrl Pts',(-21.2094532518122,-18.294208373011,-4.99987126950845));
#63897=CARTESIAN_POINT('Ctrl Pts',(-21.1854159920051,-18.2143282341436,
-5.00401092803467));
#63898=CARTESIAN_POINT('Ctrl Pts',(-21.1613926712713,-18.1344944173246,
-5.00814818599592));
#63899=CARTESIAN_POINT('Ctrl Pts',(-21.1334480518403,-18.0557779336931,
-5.01228544395717));
#63900=CARTESIAN_POINT('Ctrl Pts',(-21.1017147974227,-17.9785902003445,
-5.01642270191842));
#63901=CARTESIAN_POINT('Ctrl Pts',(-21.069990038471,-17.9014231313041,-5.02055885227397));
#63902=CARTESIAN_POINT('Ctrl Pts',(-21.0344788364885,-17.8257844328049,
-5.02469500262952));
#63903=CARTESIAN_POINT('Ctrl Pts',(-20.9953624823967,-17.7520667838548,
-5.02883115298507));
#63904=CARTESIAN_POINT('Ctrl Pts',(-20.9562443890682,-17.678345857185,-5.03296748724695));
#63905=CARTESIAN_POINT('Ctrl Pts',(-20.9135210465752,-17.6065465624556,
-5.03710382150882));
#63906=CARTESIAN_POINT('Ctrl Pts',(-20.8674196102011,-17.5370368319954,
-5.0412401557707));
#63907=CARTESIAN_POINT('Ctrl Pts',(-20.8212714994527,-17.4674567279542,
-5.04538067777222));
#63908=CARTESIAN_POINT('Ctrl Pts',(-20.7717387262313,-17.4001712070023,
-5.04952119977375));
#63909=CARTESIAN_POINT('Ctrl Pts',(-20.7190913321281,-17.3355185113618,
-5.05366172177528));
#63910=CARTESIAN_POINT('Ctrl Pts',(-20.6664157771983,-17.2708312333193,
-5.05780445852121));
#63911=CARTESIAN_POINT('Ctrl Pts',(-20.6106225991452,-17.208779931402,-5.06194719526715));
#63912=CARTESIAN_POINT('Ctrl Pts',(-20.5520199344772,-17.1496672011409,
-5.06608993201309));
#63913=CARTESIAN_POINT('Ctrl Pts',(-20.493317306161,-17.0904536371683,-5.07023973538444));
#63914=CARTESIAN_POINT('Ctrl Pts',(-20.4317959684771,-17.034188968823,-5.07438953875579));
#63915=CARTESIAN_POINT('Ctrl Pts',(-20.3677981562822,-16.9811363353776,
-5.07853934212713));
#63916=CARTESIAN_POINT('Ctrl Pts',(-20.324139169833,-16.9449440949673,-5.08137031717055));
#63917=CARTESIAN_POINT('Ctrl Pts',(-20.2793283343474,-16.9102458437321,
-5.08420129221396));
#63918=CARTESIAN_POINT('Ctrl Pts',(-20.2334815623284,-16.8771132454428,
-5.08703226725737));
#63919=CARTESIAN_POINT('Ctrl Pts',(-20.1657126925719,-16.8281379601764,
-5.09121690165042));
#63920=CARTESIAN_POINT('Ctrl Pts',(-20.0954157767523,-16.7823951726099,
-5.09540153604348));
#63921=CARTESIAN_POINT('Ctrl Pts',(-20.0229321512533,-16.7401559934151,
-5.09958617043653));
#63922=CARTESIAN_POINT('Ctrl Pts',(-19.9505516972235,-16.6979769364637,
-5.10376484852047));
#63923=CARTESIAN_POINT('Ctrl Pts',(-19.8759911100092,-16.6592918118669,
-5.10794352660442));
#63924=CARTESIAN_POINT('Ctrl Pts',(-19.7996223782741,-16.6243297168797,
-5.11212220468836));
#63925=CARTESIAN_POINT('Ctrl Pts',(-19.721884791908,-16.5887409514667,-5.1163757825738));
#63926=CARTESIAN_POINT('Ctrl Pts',(-19.6422739922293,-16.5570102814914,
-5.12062936045923));
#63927=CARTESIAN_POINT('Ctrl Pts',(-19.5612105522306,-16.5293314914586,
-5.12488293834467));
#63928=CARTESIAN_POINT('Ctrl Pts',(-19.4817186851985,-16.5021893087813,
-5.12905405232262));
#63929=CARTESIAN_POINT('Ctrl Pts',(-19.4008304551545,-16.478943456341,-5.13322516630058));
#63930=CARTESIAN_POINT('Ctrl Pts',(-19.3189628776792,-16.4597282588495,
-5.13739628027853));
#63931=CARTESIAN_POINT('Ctrl Pts',(-19.2371227716601,-16.4405195092031,
-5.1415659945989));
#63932=CARTESIAN_POINT('Ctrl Pts',(-19.1543044183624,-16.4253388333996,
-5.14573570891928));
#63933=CARTESIAN_POINT('Ctrl Pts',(-19.0709381209924,-16.4142701675273,
-5.14990542323965));
#63934=CARTESIAN_POINT('Ctrl Pts',(-18.9875747901529,-16.4032018955255,
-5.1540749891837));
#63935=CARTESIAN_POINT('Ctrl Pts',(-18.9036640101516,-16.3962454022305,
-5.15824455512775));
#63936=CARTESIAN_POINT('Ctrl Pts',(-18.8196429975838,-16.3934329641448,
-5.1624141210718));
#63937=CARTESIAN_POINT('Ctrl Pts',(-18.7326679098654,-16.3905216442056,
-5.16673028381072));
#63938=CARTESIAN_POINT('Ctrl Pts',(-18.6455752209301,-16.3920512290413,
-5.17104644654963));
#63939=CARTESIAN_POINT('Ctrl Pts',(-18.5588499153532,-16.3979987376964,
-5.17536260928855));
#63940=CARTESIAN_POINT('Ctrl Pts',(-18.4749496774835,-16.4037525068827,
-5.17953817348023));
#63941=CARTESIAN_POINT('Ctrl Pts',(-18.3913937177404,-16.413640690019,-5.18371373767191));
#63942=CARTESIAN_POINT('Ctrl Pts',(-18.3086140512033,-16.4275898125371,
-5.18788930186359));
#63943=CARTESIAN_POINT('Ctrl Pts',(-18.2216533804995,-16.4422434720727,
-5.19227576387612));
#63944=CARTESIAN_POINT('Ctrl Pts',(-18.1355500550634,-16.461378961618,-5.19666222588866));
#63945=CARTESIAN_POINT('Ctrl Pts',(-18.0507884164764,-16.4848514572205,
-5.2010486879012));
#63946=CARTESIAN_POINT('Ctrl Pts',(-17.9660267778894,-16.508323952823,-5.20543514991373));
#63947=CARTESIAN_POINT('Ctrl Pts',(-17.8826073525323,-16.5361331988247,
-5.20982161192627));
#63948=CARTESIAN_POINT('Ctrl Pts',(-17.8009895271363,-16.5680764572817,
-5.21420807393881));
#63949=CARTESIAN_POINT('Ctrl Pts',(-17.723133526379,-16.5985474278393,-5.21839236074274));
#63950=CARTESIAN_POINT('Ctrl Pts',(-17.6466269368475,-16.6328931302907,
-5.22257664754668));
#63951=CARTESIAN_POINT('Ctrl Pts',(-17.571882376384,-16.6709733388491,-5.22676093435062));
#63952=CARTESIAN_POINT('Ctrl Pts',(-17.4972521228362,-16.7089953113144,
-5.23093882212142));
#63953=CARTESIAN_POINT('Ctrl Pts',(-17.4243789496429,-16.7507402336439,
-5.23511670989222));
#63954=CARTESIAN_POINT('Ctrl Pts',(-17.3536566219057,-16.7960194438374,
-5.23929459766302));
#63955=CARTESIAN_POINT('Ctrl Pts',(-17.2922215486713,-16.835352589157,-5.24292384530484));
#63956=CARTESIAN_POINT('Ctrl Pts',(-17.2324094154131,-16.8773518875695,
-5.24655309294666));
#63957=CARTESIAN_POINT('Ctrl Pts',(-17.1744641548914,-16.9218650419685,
-5.25018234058848));
#63958=CARTESIAN_POINT('Ctrl Pts',(-17.1718943060138,-16.9185142398782,
-4.45010593052279));
#63959=CARTESIAN_POINT('Ctrl Pts',(-17.1663500824386,-16.9227662676902,
-4.45045503163193));
#63960=CARTESIAN_POINT('Ctrl Pts',(-16.4898975644531,-17.4463825557267,
-4.49319606830155));
#63961=CARTESIAN_POINT('Ctrl Pts',(-15.7195029136897,-19.2278589222636,
-4.57832904053164));
#63962=CARTESIAN_POINT('Ctrl Pts',(-17.3342635996422,-21.6360321976239,
-4.70550484721307));
#63963=CARTESIAN_POINT('Ctrl Pts',(-20.2331955554845,-21.5817725214897,
-4.83268065389451));
#63964=CARTESIAN_POINT('Ctrl Pts',(-21.2762380205877,-19.8928505327429,
-4.91974900156632));
#63965=CARTESIAN_POINT('Ctrl Pts',(-21.298094862478,-18.9985742441059,-4.96442541367765));
#63966=CARTESIAN_POINT('Ctrl Pts',(-21.2979001547653,-18.9528367523378,
-4.96670989022851));
#63967=CARTESIAN_POINT('Origin',(-18.734,-18.952,1.76670989022851));
#63968=CARTESIAN_POINT('',(-17.1744641548915,-16.9218650419685,-3.65004595805791));
#63969=CARTESIAN_POINT('',(-17.1744641548914,-16.9218650419685,-3.71676815084982));
#63970=CARTESIAN_POINT('',(-17.1744641548914,-16.9218650419685,1.76670989022851));
#63971=CARTESIAN_POINT('',(-21.2939990418858,-18.954214846262,-4.23329008725046));
#63972=CARTESIAN_POINT('Ctrl Pts',(-17.1744641548914,-16.9218650419685,
-3.71676815084982));
#63973=CARTESIAN_POINT('Ctrl Pts',(-17.1078987377222,-16.9730001419821,
-3.72094076265801));
#63974=CARTESIAN_POINT('Ctrl Pts',(-17.0437863852809,-17.027462162245,-3.7251133744662));
#63975=CARTESIAN_POINT('Ctrl Pts',(-16.9824730190864,-17.0849827973123,
-3.72928598627439));
#63976=CARTESIAN_POINT('Ctrl Pts',(-16.9211916370527,-17.1424734266998,
-3.73345642143668));
#63977=CARTESIAN_POINT('Ctrl Pts',(-16.8627066771082,-17.2030191888223,
-3.73762685659898));
#63978=CARTESIAN_POINT('Ctrl Pts',(-16.8073301088088,-17.2663122678333,
-3.74179729176127));
#63979=CARTESIAN_POINT('Ctrl Pts',(-16.7519658159504,-17.3295913165336,
-3.74596680245438));
#63980=CARTESIAN_POINT('Ctrl Pts',(-16.6997088486859,-17.3956161261854,
-3.75013631314748));
#63981=CARTESIAN_POINT('Ctrl Pts',(-16.6508325531442,-17.4640438889671,
-3.75430582384059));
#63982=CARTESIAN_POINT('Ctrl Pts',(-16.601952430527,-17.5324770097288,-3.75847566101164));
#63983=CARTESIAN_POINT('Ctrl Pts',(-16.5564537715699,-17.6033130821118,
-3.76264549818268));
#63984=CARTESIAN_POINT('Ctrl Pts',(-16.5145672435831,-17.6761793857507,
-3.76681533535373));
#63985=CARTESIAN_POINT('Ctrl Pts',(-16.4726368174248,-17.7491220551721,
-3.77098954262265));
#63986=CARTESIAN_POINT('Ctrl Pts',(-16.4343263111264,-17.8240988048856,
-3.77516374989157));
#63987=CARTESIAN_POINT('Ctrl Pts',(-16.3998206964041,-17.9007117528173,
-3.7793379571605));
#63988=CARTESIAN_POINT('Ctrl Pts',(-16.365296345968,-17.9773662997259,-3.78351443092296));
#63989=CARTESIAN_POINT('Ctrl Pts',(-16.3345811690697,-18.0556583854633,
-3.78769090468543));
#63990=CARTESIAN_POINT('Ctrl Pts',(-16.3078112708355,-18.1351718354053,
-3.7918673784479));
#63991=CARTESIAN_POINT('Ctrl Pts',(-16.2809948736771,-18.2148233990543,
-3.7960511066846));
#63992=CARTESIAN_POINT('Ctrl Pts',(-16.2581375680449,-18.295700121177,-3.8002348349213));
#63993=CARTESIAN_POINT('Ctrl Pts',(-16.2393249922832,-18.3773726373784,
-3.80441856315799));
#63994=CARTESIAN_POINT('Ctrl Pts',(-16.2251740524992,-18.4388072263162,
-3.80756559029029));
#63995=CARTESIAN_POINT('Ctrl Pts',(-16.2133106237547,-18.5006918164137,
-3.81071261742259));
#63996=CARTESIAN_POINT('Ctrl Pts',(-16.2037517912764,-18.5628419315354,
-3.81385964455489));
#63997=CARTESIAN_POINT('Ctrl Pts',(-16.1910413132713,-18.645483579777,-3.818044278948));
#63998=CARTESIAN_POINT('Ctrl Pts',(-16.182360236898,-18.7289023900138,-3.82222891334111));
#63999=CARTESIAN_POINT('Ctrl Pts',(-16.1777943305987,-18.812670980335,-3.82641354773422));
#64000=CARTESIAN_POINT('Ctrl Pts',(-16.1732349233019,-18.8963203364364,
-3.83059222581822));
#64001=CARTESIAN_POINT('Ctrl Pts',(-16.1727790761929,-18.9803180282762,
-3.83477090390222));
#64002=CARTESIAN_POINT('Ctrl Pts',(-16.1764611917473,-19.0642285359493,
-3.83894958198623));
#64003=CARTESIAN_POINT('Ctrl Pts',(-16.1802093065767,-19.1496430791654,
-3.84320315987165));
#64004=CARTESIAN_POINT('Ctrl Pts',(-16.1882452624471,-19.2349668053837,
-3.84745673775707));
#64005=CARTESIAN_POINT('Ctrl Pts',(-16.2005498883094,-19.319737041342,-3.85171031564249));
#64006=CARTESIAN_POINT('Ctrl Pts',(-16.2126159649891,-19.4028638408622,
-3.8558814296205));
#64007=CARTESIAN_POINT('Ctrl Pts',(-16.2287866065493,-19.4854579433578,
-3.86005254359851));
#64008=CARTESIAN_POINT('Ctrl Pts',(-16.2489913365584,-19.5670869390747,
-3.86422365757652));
#64009=CARTESIAN_POINT('Ctrl Pts',(-16.2691892866753,-19.6486885433937,
-3.86839337189695));
#64010=CARTESIAN_POINT('Ctrl Pts',(-16.2934185263771,-19.7293252379219,
-3.87256308621738));
#64011=CARTESIAN_POINT('Ctrl Pts',(-16.3215576717043,-19.8085757483417,
-3.87673280053781));
#64012=CARTESIAN_POINT('Ctrl Pts',(-16.3496958157199,-19.8878234386882,
-3.88090236648191));
#64013=CARTESIAN_POINT('Ctrl Pts',(-16.3817434340022,-19.9656846097684,
-3.88507193242601));
#64014=CARTESIAN_POINT('Ctrl Pts',(-16.4175300086123,-20.0417553757611,
-3.88924149837011));
#64015=CARTESIAN_POINT('Ctrl Pts',(-16.4545747950371,-20.1205006960405,
-3.89355766110896));
#64016=CARTESIAN_POINT('Ctrl Pts',(-16.4956261286209,-20.1973268901834,
-3.89787382384781));
#64017=CARTESIAN_POINT('Ctrl Pts',(-16.5404425366712,-20.2718127348509,
-3.90218998658666));
#64018=CARTESIAN_POINT('Ctrl Pts',(-16.5837990549445,-20.3438722109651,
-3.90636555077841));
#64019=CARTESIAN_POINT('Ctrl Pts',(-16.6306788183654,-20.4137411050177,
-3.91054111497015));
#64020=CARTESIAN_POINT('Ctrl Pts',(-16.6808195479049,-20.4810683539772,
-3.91471667916189));
#64021=CARTESIAN_POINT('Ctrl Pts',(-16.7334927664927,-20.551796142223,-3.9191031411743));
#64022=CARTESIAN_POINT('Ctrl Pts',(-16.789764658884,-20.6197183310682,-3.9234896031867));
#64023=CARTESIAN_POINT('Ctrl Pts',(-16.8492855900872,-20.6844697957156,
-3.92787606519911));
#64024=CARTESIAN_POINT('Ctrl Pts',(-16.9088065212903,-20.7492212603631,
-3.93226252721152));
#64025=CARTESIAN_POINT('Ctrl Pts',(-16.9715760238564,-20.8108016487772,
-3.93664898922392));
#64026=CARTESIAN_POINT('Ctrl Pts',(-17.0372042845901,-20.8688944415816,
-3.94103545123633));
#64027=CARTESIAN_POINT('Ctrl Pts',(-17.0998128917647,-20.9243142988764,
-3.94522008562936));
#64028=CARTESIAN_POINT('Ctrl Pts',(-17.1652560078682,-20.9767667301136,
-3.94940472002239));
#64029=CARTESIAN_POINT('Ctrl Pts',(-17.2332206971795,-21.0259482838841,
-3.95358935441542));
#64030=CARTESIAN_POINT('Ctrl Pts',(-17.3010886471678,-21.0750598338001,
-3.95776803249934));
#64031=CARTESIAN_POINT('Ctrl Pts',(-17.3714706716863,-21.1209094865295,
-3.96194671058326));
#64032=CARTESIAN_POINT('Ctrl Pts',(-17.4440191888247,-21.1632325763699,
-3.96612538866718));
#64033=CARTESIAN_POINT('Ctrl Pts',(-17.5178680859937,-21.206314277179,-3.97037896655262));
#64034=CARTESIAN_POINT('Ctrl Pts',(-17.5939615474698,-21.2457414247196,
-3.97463254443806));
#64035=CARTESIAN_POINT('Ctrl Pts',(-17.6719001613339,-21.2812797025487,
-3.9788861223235));
#64036=CARTESIAN_POINT('Ctrl Pts',(-17.7483277830831,-21.3161290015147,
-3.98305723630144));
#64037=CARTESIAN_POINT('Ctrl Pts',(-17.8265292140563,-21.3472386721818,
-3.98722835027937));
#64038=CARTESIAN_POINT('Ctrl Pts',(-17.906102718525,-21.3744339188771,-3.9913994642573));
#64039=CARTESIAN_POINT('Ctrl Pts',(-17.9856495213358,-21.4016200399448,
-3.99556917857765));
#64040=CARTESIAN_POINT('Ctrl Pts',(-18.0665670483056,-21.4248941970682,
-3.999738892898));
#64041=CARTESIAN_POINT('Ctrl Pts',(-18.1484353715664,-21.4441304271501,
-4.00390860721835));
#64042=CARTESIAN_POINT('Ctrl Pts',(-18.2303007816012,-21.4633659727244,
-4.00807817316238));
#64043=CARTESIAN_POINT('Ctrl Pts',(-18.3131164726259,-21.4785637725468,
-4.01224773910642));
#64044=CARTESIAN_POINT('Ctrl Pts',(-18.3964505424552,-21.4896485894842,
-4.01641730505045));
#64045=CARTESIAN_POINT('Ctrl Pts',(-18.4827145353767,-21.5011231349106,
-4.02073346778939));
#64046=CARTESIAN_POINT('Ctrl Pts',(-18.5695335149128,-21.5081900216474,
-4.02504963052834));
#64047=CARTESIAN_POINT('Ctrl Pts',(-18.656422594307,-21.5108242898108,-4.02936579326728));
#64048=CARTESIAN_POINT('Ctrl Pts',(-18.7404812710781,-21.5133727469659,
-4.03354135745894));
#64049=CARTESIAN_POINT('Ctrl Pts',(-18.8246050807773,-21.5117729919952,
-4.0377169216506));
#64050=CARTESIAN_POINT('Ctrl Pts',(-18.9083568682882,-21.5060555362953,
-4.04189248584226));
#64051=CARTESIAN_POINT('Ctrl Pts',(-18.9963387594866,-21.5000493054998,
-4.04627894785484));
#64052=CARTESIAN_POINT('Ctrl Pts',(-19.0839094794603,-21.4894985417946,
-4.05066540986743));
#64053=CARTESIAN_POINT('Ctrl Pts',(-19.1705727652476,-21.474499597749,-4.05505187188001));
#64054=CARTESIAN_POINT('Ctrl Pts',(-19.2572360510348,-21.4595006537035,
-4.0594383338926));
#64055=CARTESIAN_POINT('Ctrl Pts',(-19.3429913536082,-21.4400537318181,
-4.06382479590518));
#64056=CARTESIAN_POINT('Ctrl Pts',(-19.4273615317731,-21.4163152773656,
-4.06821125791777));
#64057=CARTESIAN_POINT('Ctrl Pts',(-19.5078497129731,-21.3936690643915,
-4.07239589231081));
#64058=CARTESIAN_POINT('Ctrl Pts',(-19.5873770243866,-21.3670332665356,
-4.07658052670385));
#64059=CARTESIAN_POINT('Ctrl Pts',(-19.6655189252301,-21.336506760724,-4.08076516109689));
#64060=CARTESIAN_POINT('Ctrl Pts',(-19.7435496007498,-21.3060237056149,
-4.08494383918084));
#64061=CARTESIAN_POINT('Ctrl Pts',(-19.820198357802,-21.2716611086064,-4.08912251726478));
#64062=CARTESIAN_POINT('Ctrl Pts',(-19.8950545149195,-21.2335679725542,
-4.09330119534872));
#64063=CARTESIAN_POINT('Ctrl Pts',(-19.9712524148552,-21.1947920444153,
-4.09755477323416));
#64064=CARTESIAN_POINT('Ctrl Pts',(-20.0455923539257,-21.152150652534,-4.10180835111959));
#64065=CARTESIAN_POINT('Ctrl Pts',(-20.1176611149874,-21.1058528080795,
-4.10606192900503));
#64066=CARTESIAN_POINT('Ctrl Pts',(-20.1883326824852,-21.0604525376826,
-4.11023304298298));
#64067=CARTESIAN_POINT('Ctrl Pts',(-20.2568199436825,-21.0115365845692,
-4.11440415696092));
#64068=CARTESIAN_POINT('Ctrl Pts',(-20.3227584711504,-20.9593481313285,
-4.11857527093886));
#64069=CARTESIAN_POINT('Ctrl Pts',(-20.3886748723086,-20.9071771904272,
-4.12274498525923));
#64070=CARTESIAN_POINT('Ctrl Pts',(-20.4520438778608,-20.8517362155432,
-4.1269146995796));
#64071=CARTESIAN_POINT('Ctrl Pts',(-20.512532273786,-20.7933101181229,-4.13108441389997));
#64072=CARTESIAN_POINT('Ctrl Pts',(-20.5730185172742,-20.7348860997541,
-4.13525397984399));
#64073=CARTESIAN_POINT('Ctrl Pts',(-20.6306240246485,-20.6734774902644,
-4.13942354578802));
#64074=CARTESIAN_POINT('Ctrl Pts',(-20.6850517529254,-20.6094067266084,
-4.14359311173205));
#64075=CARTESIAN_POINT('Ctrl Pts',(-20.7413930929849,-20.5430833139418,
-4.14790927447098));
#64076=CARTESIAN_POINT('Ctrl Pts',(-20.7943286933419,-20.47390746331,-4.1522254372099));
#64077=CARTESIAN_POINT('Ctrl Pts',(-20.8435751066795,-20.4022733774286,
-4.15654159994883));
#64078=CARTESIAN_POINT('Ctrl Pts',(-20.8912173232822,-20.3329727643606,
-4.16071716414051));
#64079=CARTESIAN_POINT('Ctrl Pts',(-20.9354068051746,-20.261372036261,-4.16489272833218));
#64080=CARTESIAN_POINT('Ctrl Pts',(-20.9759325838393,-20.1878552866415,
-4.16906829252385));
#64081=CARTESIAN_POINT('Ctrl Pts',(-21.0185052232437,-20.1106253807678,
-4.17345475453641));
#64082=CARTESIAN_POINT('Ctrl Pts',(-21.0570340704736,-20.0312813353546,
-4.17784121654897));
#64083=CARTESIAN_POINT('Ctrl Pts',(-21.0913315250628,-19.9502925828359,
-4.18222767856152));
#64084=CARTESIAN_POINT('Ctrl Pts',(-21.125628979652,-19.8693038303172,-4.18661414057408));
#64085=CARTESIAN_POINT('Ctrl Pts',(-21.1556949146933,-19.7866709419479,
-4.19100060258664));
#64086=CARTESIAN_POINT('Ctrl Pts',(-21.1814026084241,-19.7028797988221,
-4.19538706459919));
#64087=CARTESIAN_POINT('Ctrl Pts',(-21.2113658472603,-19.6052182170354,
-4.20049964335886));
#64088=CARTESIAN_POINT('Ctrl Pts',(-21.235501378659,-19.5056900725396,-4.20561222211854));
#64089=CARTESIAN_POINT('Ctrl Pts',(-21.253614967081,-19.4049242957285,-4.2107248008782));
#64090=CARTESIAN_POINT('Ctrl Pts',(-21.2714816855059,-19.3055318551366,
-4.21576770033001));
#64091=CARTESIAN_POINT('Ctrl Pts',(-21.283489454374,-19.2049352741372,-4.22081059978182));
#64092=CARTESIAN_POINT('Ctrl Pts',(-21.2894978367355,-19.1037590407195,
-4.22585349923363));
#64093=CARTESIAN_POINT('Ctrl Pts',(-21.2924512874039,-19.0540253526423,
-4.22833236190591));
#64094=CARTESIAN_POINT('Ctrl Pts',(-21.2939558375883,-19.0041519285412,
-4.23081122457819));
#64095=CARTESIAN_POINT('Ctrl Pts',(-21.2939990418858,-18.954214846262,-4.23329008725046));
#64096=CARTESIAN_POINT('Ctrl Pts',(-21.2923872764654,-18.9542129983989,
-4.2332901097715));
#64097=CARTESIAN_POINT('Ctrl Pts',(-21.2874612769029,-18.3551143891762,
-4.26304769694121));
#64098=CARTESIAN_POINT('Ctrl Pts',(-20.7784813193811,-16.8950156348367,
-4.3351972196714));
#64099=CARTESIAN_POINT('Ctrl Pts',(-18.7708036927661,-16.1157767610087,
-4.42965875003148));
#64100=CARTESIAN_POINT('Ctrl Pts',(-17.5345084148665,-16.6513470387785,
-4.49436269322185));
#64101=CARTESIAN_POINT('Ctrl Pts',(-17.1769969348074,-16.9251725137323,
-4.51667470085173));
#64102=CARTESIAN_POINT('',(-21.2939989159607,-18.9496440968075,-4.16670989022851));
#64103=CARTESIAN_POINT('Ctrl Pts',(-21.2939116738757,-18.9496434105868,
-4.1667099283594));
#64104=CARTESIAN_POINT('Ctrl Pts',(-21.2957663705073,-18.7480072535544,
-4.17674049240205));
#64105=CARTESIAN_POINT('Ctrl Pts',(-21.1817725642886,-17.6962740222633,
-4.22916299200517));
#64106=CARTESIAN_POINT('Ctrl Pts',(-19.7363287120773,-16.0997001271578,
-4.32362832605963));
#64107=CARTESIAN_POINT('Ctrl Pts',(-17.839594487521,-16.4064353701673,-4.40806309607145));
#64108=CARTESIAN_POINT('Ctrl Pts',(-17.1718943060138,-16.9185142398782,
-4.45010593052279));
#64109=CARTESIAN_POINT('Ctrl Pts',(-17.1744641548914,-16.9218650419685,
-3.65004595805791));
#64110=CARTESIAN_POINT('Ctrl Pts',(-17.1077768163659,-16.9730938011375,
-3.65422167904487));
#64111=CARTESIAN_POINT('Ctrl Pts',(-17.0436659066504,-17.0275737769818,
-3.65839740003182));
#64112=CARTESIAN_POINT('Ctrl Pts',(-16.9824501210915,-17.0850042791438,
-3.66257312101877));
#64113=CARTESIAN_POINT('Ctrl Pts',(-16.9200836608067,-17.1435143039604,
-3.66682733314258));
#64114=CARTESIAN_POINT('Ctrl Pts',(-16.8607226247173,-17.2050865495661,
-3.67108154526638));
#64115=CARTESIAN_POINT('Ctrl Pts',(-16.8046620040762,-17.2693666776494,
-3.67533575739019));
#64116=CARTESIAN_POINT('Ctrl Pts',(-16.7486013834351,-17.3336468057327,
-3.67958996951399));
#64117=CARTESIAN_POINT('Ctrl Pts',(-16.6958414336857,-17.4006343840734,
-3.68384418163779));
#64118=CARTESIAN_POINT('Ctrl Pts',(-16.6466304638567,-17.4699445288448,
-3.6880983937616));
#64119=CARTESIAN_POINT('Ctrl Pts',(-16.5982243404926,-17.538121104715,-3.69228302815506));
#64120=CARTESIAN_POINT('Ctrl Pts',(-16.5530717694468,-17.6087985715455,
-3.69646766254853));
#64121=CARTESIAN_POINT('Ctrl Pts',(-16.5114409937958,-17.6816333348436,
-3.70065229694199));
#64122=CARTESIAN_POINT('Ctrl Pts',(-16.469869474401,-17.7543644268713,-3.70483097502635));
#64123=CARTESIAN_POINT('Ctrl Pts',(-16.4318100196565,-17.8292463201219,
-3.70900965311071));
#64124=CARTESIAN_POINT('Ctrl Pts',(-16.3974886040354,-17.9059051206856,
-3.71318833119507));
#64125=CARTESIAN_POINT('Ctrl Pts',(-16.3625520017101,-17.9839379751461,
-3.7174419090804));
#64126=CARTESIAN_POINT('Ctrl Pts',(-16.3314890444372,-18.0638116724915,
-3.72169548696573));
#64127=CARTESIAN_POINT('Ctrl Pts',(-16.3044899883694,-18.1451040318687,
-3.72594906485107));
#64128=CARTESIAN_POINT('Ctrl Pts',(-16.2780143616844,-18.2248203802406,
-3.73012017882945));
#64129=CARTESIAN_POINT('Ctrl Pts',(-16.2554466207296,-18.3059004177645,
-3.73429129280783));
#64130=CARTESIAN_POINT('Ctrl Pts',(-16.2369175937362,-18.3879260187458,
-3.73846240678621));
#64131=CARTESIAN_POINT('Ctrl Pts',(-16.2183947843368,-18.4699240952445,
-3.74263212110702));
#64132=CARTESIAN_POINT('Ctrl Pts',(-16.2039080986716,-18.5528666566986,
-3.74680183542783));
#64133=CARTESIAN_POINT('Ctrl Pts',(-16.1935378668542,-18.6363227121694,
-3.75097154974863));
#64134=CARTESIAN_POINT('Ctrl Pts',(-16.1831680040541,-18.7197757979158,
-3.75514111569312));
#64135=CARTESIAN_POINT('Ctrl Pts',(-16.1769143597415,-18.8037418847219,
-3.75931068163761));
#64136=CARTESIAN_POINT('Ctrl Pts',(-16.174805548368,-18.8877835010606,-3.76348024758209));
#64137=CARTESIAN_POINT('Ctrl Pts',(-16.1726225937887,-18.9747799169337,
-3.7677964103205));
#64138=CARTESIAN_POINT('Ctrl Pts',(-16.1748813730051,-19.0618567451386,
-3.77211257305891));
#64139=CARTESIAN_POINT('Ctrl Pts',(-16.1815548449752,-19.1485292105273,
-3.77642873579733));
#64140=CARTESIAN_POINT('Ctrl Pts',(-16.1880109292993,-19.2323783294909,
-3.78060429998945));
#64141=CARTESIAN_POINT('Ctrl Pts',(-16.1985983999138,-19.3158485639561,
-3.78477986418157));
#64142=CARTESIAN_POINT('Ctrl Pts',(-16.2132401674605,-19.3985085292081,
-3.78895542837369));
#64143=CARTESIAN_POINT('Ctrl Pts',(-16.2286214558734,-19.485343452771,-3.79334189038525));
#64144=CARTESIAN_POINT('Ctrl Pts',(-16.2484772384201,-19.5712835336828,
-3.7977283523968));
#64145=CARTESIAN_POINT('Ctrl Pts',(-16.272658640717,-19.6558456599874,-3.80211481440836));
#64146=CARTESIAN_POINT('Ctrl Pts',(-16.2968400430139,-19.7404077862919,
-3.80650127641991));
#64147=CARTESIAN_POINT('Ctrl Pts',(-16.3253468050044,-19.8235914337677,
-3.81088773843147));
#64148=CARTESIAN_POINT('Ctrl Pts',(-16.3579723492966,-19.9049389293615,
-3.81527420044303));
#64149=CARTESIAN_POINT('Ctrl Pts',(-16.3890967439393,-19.9825435061125,
-3.81945883483596));
#64150=CARTESIAN_POINT('Ctrl Pts',(-16.4240850782656,-20.0587660450939,
-3.8236434692289));
#64151=CARTESIAN_POINT('Ctrl Pts',(-16.4627936385718,-20.133195015147,-3.82782810362183));
#64152=CARTESIAN_POINT('Ctrl Pts',(-16.5014471020335,-20.2075180447734,
-3.83200678170565));
#64153=CARTESIAN_POINT('Ctrl Pts',(-16.5438100629347,-20.280052171735,-3.83618545978947));
#64154=CARTESIAN_POINT('Ctrl Pts',(-16.5896904513639,-20.3504050055789,
-3.84036413787329));
#64155=CARTESIAN_POINT('Ctrl Pts',(-16.6363932127838,-20.4220188634104,
-3.84461771575875));
#64156=CARTESIAN_POINT('Ctrl Pts',(-16.6867405623481,-20.49137201211,-3.84887129364422));
#64157=CARTESIAN_POINT('Ctrl Pts',(-16.7404804948179,-20.5580759578732,
-3.85312487152969));
#64158=CARTESIAN_POINT('Ctrl Pts',(-16.79317857383,-20.6234867174835,-3.85729598550753));
#64159=CARTESIAN_POINT('Ctrl Pts',(-16.8491385640368,-20.6863497027056,
-3.86146709948537));
#64160=CARTESIAN_POINT('Ctrl Pts',(-16.9080797027391,-20.7463285841926,
-3.86563821346321));
#64161=CARTESIAN_POINT('Ctrl Pts',(-16.967001063173,-20.8062873391867,-3.86980792778346));
#64162=CARTESIAN_POINT('Ctrl Pts',(-17.028901263212,-20.8633635846445,-3.87397764210372));
#64163=CARTESIAN_POINT('Ctrl Pts',(-17.0934613888496,-20.9172564884321,
-3.87814735642397));
#64164=CARTESIAN_POINT('Ctrl Pts',(-17.1580192171609,-20.9711474744791,
-3.88231692236791));
#64165=CARTESIAN_POINT('Ctrl Pts',(-17.2252364291759,-21.0218550499285,
-3.88648648831184));
#64166=CARTESIAN_POINT('Ctrl Pts',(-17.2947606690316,-21.0691183595145,
-3.89065605425577));
#64167=CARTESIAN_POINT('Ctrl Pts',(-17.3667292953974,-21.1180433887629,
-3.89497221699483));
#64168=CARTESIAN_POINT('Ctrl Pts',(-17.4411697620694,-21.1632771484776,
-3.89928837973389));
#64169=CARTESIAN_POINT('Ctrl Pts',(-17.5176598130617,-21.2045799763025,
-3.90360454247294));
#64170=CARTESIAN_POINT('Ctrl Pts',(-17.5916582086839,-21.2445373688529,
-3.90778010666451));
#64171=CARTESIAN_POINT('Ctrl Pts',(-17.6675742634434,-21.2808158363469,
-3.91195567085607));
#64172=CARTESIAN_POINT('Ctrl Pts',(-17.7450035240558,-21.3132466983714,
-3.91613123504764));
#64173=CARTESIAN_POINT('Ctrl Pts',(-17.8263435525583,-21.3473155661427,
-3.92051769706044));
#64174=CARTESIAN_POINT('Ctrl Pts',(-17.9093531188135,-21.3771377310941,
-3.92490415907325));
#64175=CARTESIAN_POINT('Ctrl Pts',(-17.9935454192395,-21.4025768736832,
-3.92929062108605));
#64176=CARTESIAN_POINT('Ctrl Pts',(-18.0777377196656,-21.4280160162723,
-3.93367708309886));
#64177=CARTESIAN_POINT('Ctrl Pts',(-18.1631121727114,-21.4490720714144,
-3.93806354511166));
#64178=CARTESIAN_POINT('Ctrl Pts',(-18.249172131343,-21.4656710082613,-3.94245000712447));
#64179=CARTESIAN_POINT('Ctrl Pts',(-18.3312723437006,-21.4815062034173,
-3.94663464151747));
#64180=CARTESIAN_POINT('Ctrl Pts',(-18.4143019582715,-21.4933443659487,
-3.95081927591047));
#64181=CARTESIAN_POINT('Ctrl Pts',(-18.4978371529754,-21.5010835823262,
-3.95500391030347));
#64182=CARTESIAN_POINT('Ctrl Pts',(-18.5812534456692,-21.5088117828872,
-3.95918258838737));
#64183=CARTESIAN_POINT('Ctrl Pts',(-18.6651734349296,-21.5124525840588,
-3.96336126647127));
#64184=CARTESIAN_POINT('Ctrl Pts',(-18.7491632186829,-21.511955092731,-3.96753994455516));
#64185=CARTESIAN_POINT('Ctrl Pts',(-18.8346584589487,-21.5114486842287,
-3.97179352244061));
#64186=CARTESIAN_POINT('Ctrl Pts',(-18.920225547037,-21.5066540748902,-3.97604710032606));
#64187=CARTESIAN_POINT('Ctrl Pts',(-19.0054014154825,-21.4975728769128,
-3.9803006782115));
#64188=CARTESIAN_POINT('Ctrl Pts',(-19.0889259835099,-21.4886677356789,
-3.9844717921894));
#64189=CARTESIAN_POINT('Ctrl Pts',(-19.1720738871333,-21.4756407813847,
-3.9886429061673));
#64190=CARTESIAN_POINT('Ctrl Pts',(-19.2544103550736,-21.4585460423324,
-3.9928140201452));
#64191=CARTESIAN_POINT('Ctrl Pts',(-19.3367191942171,-21.4414570395848,
-3.99698373446553));
#64192=CARTESIAN_POINT('Ctrl Pts',(-19.4182166883875,-21.4203030563999,
-4.00115344878585));
#64193=CARTESIAN_POINT('Ctrl Pts',(-19.4984772632651,-21.3951894142597,
-4.00532316310618));
#64194=CARTESIAN_POINT('Ctrl Pts',(-19.5787349821266,-21.3700766657708,
-4.00949272905015));
#64195=CARTESIAN_POINT('Ctrl Pts',(-19.6577554304208,-21.3410046766653,
-4.01366229499412));
#64196=CARTESIAN_POINT('Ctrl Pts',(-19.7351285466046,-21.3081285264546,
-4.0178318609381));
#64197=CARTESIAN_POINT('Ctrl Pts',(-19.815222006106,-21.2740964913586,-4.02214802367708));
#64198=CARTESIAN_POINT('Ctrl Pts',(-19.8935496523612,-21.2359880155544,
-4.02646418641606));
#64199=CARTESIAN_POINT('Ctrl Pts',(-19.9696814080998,-21.1940284248146,
-4.03078034915504));
#64200=CARTESIAN_POINT('Ctrl Pts',(-20.0433331799007,-21.1534356633309,
-4.03495591334667));
#64201=CARTESIAN_POINT('Ctrl Pts',(-20.1149295504515,-21.1092391216322,
-4.03913147753829));
#64202=CARTESIAN_POINT('Ctrl Pts',(-20.1841097633271,-21.061687577416,-4.04330704172992));
#64203=CARTESIAN_POINT('Ctrl Pts',(-20.2567841042977,-21.0117343177424,
-4.04769350374258));
#64204=CARTESIAN_POINT('Ctrl Pts',(-20.3267913293724,-20.9580785813378,
-4.05207996575524));
#64205=CARTESIAN_POINT('Ctrl Pts',(-20.3937533178434,-20.9010559057933,
-4.0564664277679));
#64206=CARTESIAN_POINT('Ctrl Pts',(-20.4607153063143,-20.8440332302489,
-4.06085288978057));
#64207=CARTESIAN_POINT('Ctrl Pts',(-20.524631688673,-20.7836440693278,-4.06523935179323));
#64208=CARTESIAN_POINT('Ctrl Pts',(-20.5851713910718,-20.7202659530956,
-4.06962581380589));
#64209=CARTESIAN_POINT('Ctrl Pts',(-20.6421808499863,-20.66058359639,-4.07375648865202));
#64210=CARTESIAN_POINT('Ctrl Pts',(-20.6964202744403,-20.5980163329693,
-4.07788716349815));
#64211=CARTESIAN_POINT('Ctrl Pts',(-20.747578131795,-20.5328551822216,-4.08201783834428));
#64212=CARTESIAN_POINT('Ctrl Pts',(-20.7986699217385,-20.467778183328,-4.08614317866296));
#64213=CARTESIAN_POINT('Ctrl Pts',(-20.8466877493678,-20.4001143092104,
-4.09026851898165));
#64214=CARTESIAN_POINT('Ctrl Pts',(-20.8913569516645,-20.3301911997632,
-4.09439385930034));
#64215=CARTESIAN_POINT('Ctrl Pts',(-20.9359826817961,-20.2603361396387,
-4.09851518482882));
#64216=CARTESIAN_POINT('Ctrl Pts',(-20.9772659998208,-20.188226602647,-4.10263651035731));
#64217=CARTESIAN_POINT('Ctrl Pts',(-21.0149735460513,-20.1142218730579,
-4.10675783588579));
#64218=CARTESIAN_POINT('Ctrl Pts',(-21.0526563884391,-20.0402656271644,
-4.11087646135587));
#64219=CARTESIAN_POINT('Ctrl Pts',(-21.0867678956212,-19.9644170734847,
-4.11499508682595));
#64220=CARTESIAN_POINT('Ctrl Pts',(-21.1171197545789,-19.8870616211436,
-4.11911371229603));
#64221=CARTESIAN_POINT('Ctrl Pts',(-21.1474714047475,-19.8097067009274,
-4.12323230943426));
#64222=CARTESIAN_POINT('Ctrl Pts',(-21.1740632676919,-19.730845335542,-4.12735090657249));
#64223=CARTESIAN_POINT('Ctrl Pts',(-21.1967549321189,-19.6508834983916,
-4.13146950371072));
#64224=CARTESIAN_POINT('Ctrl Pts',(-21.2194452848828,-19.5709262833344,
-4.13558786277862));
#64225=CARTESIAN_POINT('Ctrl Pts',(-21.238235765403,-19.4898691801177,-4.13970622184653));
#64226=CARTESIAN_POINT('Ctrl Pts',(-21.2530362470693,-19.4081319830388,
-4.14382458091443));
#64227=CARTESIAN_POINT('Ctrl Pts',(-21.2678499327185,-19.3263218655936,
-4.14794661410211));
#64228=CARTESIAN_POINT('Ctrl Pts',(-21.2786664327327,-19.2438309098082,
-4.15206864728979));
#64229=CARTESIAN_POINT('Ctrl Pts',(-21.2854471635996,-19.1610869947161,
-4.15619068047747));
#64230=CARTESIAN_POINT('Ctrl Pts',(-21.2912151852698,-19.090700969273,-4.15969708372782));
#64231=CARTESIAN_POINT('Ctrl Pts',(-21.2940637843831,-19.0201321760509,
-4.16320348697816));
#64232=CARTESIAN_POINT('Ctrl Pts',(-21.2939989159607,-18.9496440968075,
-4.16670989022851));
#64233=CARTESIAN_POINT('Origin',(-18.734,-18.952,1.76670989022851));
#64234=CARTESIAN_POINT('',(-17.1767158332877,-16.9247660182631,-2.85017128494026));
#64235=CARTESIAN_POINT('',(-17.1744641548914,-16.9218650419685,-2.9166563088035));
#64236=CARTESIAN_POINT('',(-17.1744641548914,-16.9218650419685,1.76670989022851));
#64237=CARTESIAN_POINT('',(-21.2939999971965,-18.9521198080496,-3.43329010980363));
#64238=CARTESIAN_POINT('Ctrl Pts',(-17.1744641548914,-16.9218650419685,
-2.9166563088035));
#64239=CARTESIAN_POINT('Ctrl Pts',(-17.1375640854123,-16.9502114239723,
-2.91898053846395));
#64240=CARTESIAN_POINT('Ctrl Pts',(-17.1014709448253,-16.9795381858104,
-2.9213047681244));
#64241=CARTESIAN_POINT('Ctrl Pts',(-17.0662376770538,-17.0097927931961,
-2.92362899778485));
#64242=CARTESIAN_POINT('Ctrl Pts',(-17.0028023176014,-17.0642643769008,
-2.92781363217407));
#64243=CARTESIAN_POINT('Ctrl Pts',(-16.9419203976444,-17.1219484370566,
-2.93199826656328));
#64244=CARTESIAN_POINT('Ctrl Pts',(-16.8839351856056,-17.1825763134456,
-2.9361829009525));
#64245=CARTESIAN_POINT('Ctrl Pts',(-16.8260325083402,-17.2431178935555,
-2.94036157903253));
#64246=CARTESIAN_POINT('Ctrl Pts',(-16.7710186644549,-17.3065946373125,
-2.94454025711256));
#64247=CARTESIAN_POINT('Ctrl Pts',(-16.7192032202856,-17.3726982756761,
-2.9487189351926));
#64248=CARTESIAN_POINT('Ctrl Pts',(-16.6664590214574,-17.4399867743277,
-2.952972513079));
#64249=CARTESIAN_POINT('Ctrl Pts',(-16.6170293785859,-17.5099969539576,
-2.95722609096541));
#64250=CARTESIAN_POINT('Ctrl Pts',(-16.5712008555433,-17.5823650629685,
-2.96147966885181));
#64251=CARTESIAN_POINT('Ctrl Pts',(-16.5262608079009,-17.6533301748861,
-2.96565078282569));
#64252=CARTESIAN_POINT('Ctrl Pts',(-16.4847837540971,-17.7265621993711,
-2.96982189679958));
#64253=CARTESIAN_POINT('Ctrl Pts',(-16.4469976092765,-17.8016869709401,
-2.97399301077346));
#64254=CARTESIAN_POINT('Ctrl Pts',(-16.4092241439622,-17.8767865336655,
-2.97816272508971));
#64255=CARTESIAN_POINT('Ctrl Pts',(-16.3751393344499,-17.9537771714644,
-2.98233243940597));
#64256=CARTESIAN_POINT('Ctrl Pts',(-16.3449251982367,-18.0322600413271,
-2.98650215372222));
#64257=CARTESIAN_POINT('Ctrl Pts',(-16.3147121371724,-18.1107401184316,
-2.9906717196621));
#64258=CARTESIAN_POINT('Ctrl Pts',(-16.2883696400365,-18.1907118923997,
-2.99484128560198));
#64259=CARTESIAN_POINT('Ctrl Pts',(-16.2660311035624,-18.2717577444641,
-2.99901085154186));
#64260=CARTESIAN_POINT('Ctrl Pts',(-16.2429071716547,-18.355653068883,-3.00332701428556));
#64261=CARTESIAN_POINT('Ctrl Pts',(-16.2240741377505,-18.4406988974033,
-3.00764317702926));
#64262=CARTESIAN_POINT('Ctrl Pts',(-16.2096228114113,-18.5264182690326,
-3.01195933977297));
#64263=CARTESIAN_POINT('Ctrl Pts',(-16.1956422355373,-18.6093453409713,
-3.01613490396041));
#64264=CARTESIAN_POINT('Ctrl Pts',(-16.185762291265,-18.6929022752325,-3.02031046814786));
#64265=CARTESIAN_POINT('Ctrl Pts',(-16.1800123293529,-18.7766518372414,
-3.0244860323353));
#64266=CARTESIAN_POINT('Ctrl Pts',(-16.173971950515,-18.8646313908073,-3.02887249435713));
#64267=CARTESIAN_POINT('Ctrl Pts',(-16.172489739197,-18.9528229589758,-3.03325895637896));
#64268=CARTESIAN_POINT('Ctrl Pts',(-16.1755378747839,-19.0407217776812,
-3.0376454184008));
#64269=CARTESIAN_POINT('Ctrl Pts',(-16.1785860103708,-19.1286205963865,
-3.04203188042263));
#64270=CARTESIAN_POINT('Ctrl Pts',(-16.1861643670755,-19.216226094126,-3.04641834244446));
#64271=CARTESIAN_POINT('Ctrl Pts',(-16.1981829862586,-19.3030442604849,
-3.05080480446629));
#64272=CARTESIAN_POINT('Ctrl Pts',(-16.2096486109408,-19.3858677941965,
-3.05498943886226));
#64273=CARTESIAN_POINT('Ctrl Pts',(-16.2251975483163,-19.4682831419491,
-3.05917407325822));
#64274=CARTESIAN_POINT('Ctrl Pts',(-16.2447897023432,-19.5498562486412,
-3.06335870765419));
#64275=CARTESIAN_POINT('Ctrl Pts',(-16.264353969364,-19.6313132461135,-3.06753738574109));
#64276=CARTESIAN_POINT('Ctrl Pts',(-16.2879499152426,-19.7119299402847,
-3.07171606382799));
#64277=CARTESIAN_POINT('Ctrl Pts',(-16.3154858968853,-19.7912791746703,
-3.07589474191489));
#64278=CARTESIAN_POINT('Ctrl Pts',(-16.3435154411845,-19.872050686984,-3.0801483197996));
#64279=CARTESIAN_POINT('Ctrl Pts',(-16.3756275947397,-19.9515083765662,
-3.0844018976843));
#64280=CARTESIAN_POINT('Ctrl Pts',(-16.411671611611,-20.0292143967114,-3.088655475569));
#64281=CARTESIAN_POINT('Ctrl Pts',(-16.4470168449129,-20.105413934094,-3.09282658954999));
#64282=CARTESIAN_POINT('Ctrl Pts',(-16.4861426458315,-20.1799286784567,
-3.09699770353098));
#64283=CARTESIAN_POINT('Ctrl Pts',(-16.528857766552,-20.252364460551,-3.10116881751197));
#64284=CARTESIAN_POINT('Ctrl Pts',(-16.5715585538015,-20.3247759361195,
-3.1053385318354));
#64285=CARTESIAN_POINT('Ctrl Pts',(-16.6178460353525,-20.3951094389607,
-3.10950824615883));
#64286=CARTESIAN_POINT('Ctrl Pts',(-16.6674833699697,-20.4629960350075,
-3.11367796048227));
#64287=CARTESIAN_POINT('Ctrl Pts',(-16.7171189382778,-20.5308802153581,
-3.11784752642939));
#64288=CARTESIAN_POINT('Ctrl Pts',(-16.7701038504332,-20.596317291184,-3.12201709237651));
#64289=CARTESIAN_POINT('Ctrl Pts',(-16.8261591602626,-20.6589690478243,
-3.12618665832363));
#64290=CARTESIAN_POINT('Ctrl Pts',(-16.8841853055431,-20.7238235628371,
-3.13050282105897));
#64291=CARTESIAN_POINT('Ctrl Pts',(-16.9455014243904,-20.7856928577369,
-3.13481898379432));
#64292=CARTESIAN_POINT('Ctrl Pts',(-17.0097556215867,-20.8442424061177,
-3.13913514652966));
#64293=CARTESIAN_POINT('Ctrl Pts',(-17.0719167451653,-20.9008847092073,
-3.14331071072443));
#64294=CARTESIAN_POINT('Ctrl Pts',(-17.1368270773973,-20.9544199625766,
-3.14748627491921));
#64295=CARTESIAN_POINT('Ctrl Pts',(-17.2041348602072,-21.0045868200996,
-3.15166183911398));
#64296=CARTESIAN_POINT('Ctrl Pts',(-17.2748421989537,-21.0572874862135,
-3.15604830111961));
#64297=CARTESIAN_POINT('Ctrl Pts',(-17.3481950580325,-21.1062702142998,
-3.16043476312523));
#64298=CARTESIAN_POINT('Ctrl Pts',(-17.4237539519795,-21.1512851778809,
-3.16482122513085));
#64299=CARTESIAN_POINT('Ctrl Pts',(-17.4993128459265,-21.1963001414621,
-3.16920768713647));
#64300=CARTESIAN_POINT('Ctrl Pts',(-17.5770772261123,-21.2373471369617,
-3.1735941491421));
#64301=CARTESIAN_POINT('Ctrl Pts',(-17.6565830150582,-21.2742344068933,
-3.17798061114772));
#64302=CARTESIAN_POINT('Ctrl Pts',(-17.7324306249074,-21.3094244389056,
-3.18216524554016));
#64303=CARTESIAN_POINT('Ctrl Pts',(-17.8101452346756,-21.3409601078314,
-3.1863498799326));
#64304=CARTESIAN_POINT('Ctrl Pts',(-17.889340169487,-21.3686401823022,-3.19053451432504));
#64305=CARTESIAN_POINT('Ctrl Pts',(-17.968422380111,-21.3962808576131,-3.19471319240837));
#64306=CARTESIAN_POINT('Ctrl Pts',(-18.0489802999383,-21.4200766888,-3.19889187049171));
#64307=CARTESIAN_POINT('Ctrl Pts',(-18.1306051532971,-21.4398735214983,
-3.20307054857504));
#64308=CARTESIAN_POINT('Ctrl Pts',(-18.2136930735046,-21.4600251981986,
-3.20732412646063));
#64309=CARTESIAN_POINT('Ctrl Pts',(-18.2978861156725,-21.4760328992744,
-3.21157770434622));
#64310=CARTESIAN_POINT('Ctrl Pts',(-18.3827345240933,-21.4877863800873,
-3.21583128223181));
#64311=CARTESIAN_POINT('Ctrl Pts',(-18.4659379805337,-21.4993119967374,
-3.22000239620915));
#64312=CARTESIAN_POINT('Ctrl Pts',(-18.5497711422163,-21.5067468078098,
-3.22417351018649));
#64313=CARTESIAN_POINT('Ctrl Pts',(-18.6337990563677,-21.5100382661124,
-3.22834462416383));
#64314=CARTESIAN_POINT('Ctrl Pts',(-18.717798774141,-21.5133286199344,-3.23251433848359));
#64315=CARTESIAN_POINT('Ctrl Pts',(-18.801992655297,-21.5124783642369,-3.23668405280335));
#64316=CARTESIAN_POINT('Ctrl Pts',(-18.8859422870023,-21.5074869480043,
-3.24085376712312));
#64317=CARTESIAN_POINT('Ctrl Pts',(-18.9698889314194,-21.5024957093878,
-3.24502333306655));
#64318=CARTESIAN_POINT('Ctrl Pts',(-19.0535908844953,-21.4933636313811,
-3.24919289900999));
#64319=CARTESIAN_POINT('Ctrl Pts',(-19.1366127729516,-21.4801421943902,
-3.25336246495342));
#64320=CARTESIAN_POINT('Ctrl Pts',(-19.2225536086144,-21.4664559079809,
-3.25767862769307));
#64321=CARTESIAN_POINT('Ctrl Pts',(-19.3077651468763,-21.4483874314135,
-3.26199479043271));
#64322=CARTESIAN_POINT('Ctrl Pts',(-19.3917756297605,-21.4260515800794,
-3.26631095317236));
#64323=CARTESIAN_POINT('Ctrl Pts',(-19.4730494799758,-21.4044433167598,
-3.27048651736344));
#64324=CARTESIAN_POINT('Ctrl Pts',(-19.5531988875815,-21.378841616957,-3.27466208155452));
#64325=CARTESIAN_POINT('Ctrl Pts',(-19.6318137018703,-21.3494007918439,
-3.2788376457456));
#64326=CARTESIAN_POINT('Ctrl Pts',(-19.7143991635779,-21.3184729806291,
-3.28322410775952));
#64327=CARTESIAN_POINT('Ctrl Pts',(-19.7952903977543,-21.2833082561225,
-3.28761056977345));
#64328=CARTESIAN_POINT('Ctrl Pts',(-19.8740394547188,-21.2441409297171,
-3.29199703178738));
#64329=CARTESIAN_POINT('Ctrl Pts',(-19.9527885116833,-21.2049736033117,
-3.2963834938013));
#64330=CARTESIAN_POINT('Ctrl Pts',(-20.0293949232976,-21.161804026126,-3.30076995581523));
#64331=CARTESIAN_POINT('Ctrl Pts',(-20.103446255522,-21.1149186191895,-3.30515641782916));
#64332=CARTESIAN_POINT('Ctrl Pts',(-20.1740903761505,-21.070190479346,-3.30934105222176));
#64333=CARTESIAN_POINT('Ctrl Pts',(-20.2426723273843,-21.0219144506012,
-3.31352568661436));
#64334=CARTESIAN_POINT('Ctrl Pts',(-20.3088136057118,-20.97030674261,-3.31771032100697));
#64335=CARTESIAN_POINT('Ctrl Pts',(-20.374860740116,-20.9187724918035,-3.32188899909045));
#64336=CARTESIAN_POINT('Ctrl Pts',(-20.4384737424745,-20.8639162618918,
-3.32606767717394));
#64337=CARTESIAN_POINT('Ctrl Pts',(-20.4993017308436,-20.8059983276909,
-3.33024635525743));
#64338=CARTESIAN_POINT('Ctrl Pts',(-20.5612200171964,-20.7470422561363,
-3.33449993314298));
#64339=CARTESIAN_POINT('Ctrl Pts',(-20.6202520574043,-20.6849138964936,
-3.33875351102852));
#64340=CARTESIAN_POINT('Ctrl Pts',(-20.6760617089388,-20.6199317488056,
-3.34300708891407));
#64341=CARTESIAN_POINT('Ctrl Pts',(-20.7307893814671,-20.5562094068616,
-3.34717820289155));
#64342=CARTESIAN_POINT('Ctrl Pts',(-20.7824181813927,-20.4897433069906,
-3.35134931686903));
#64343=CARTESIAN_POINT('Ctrl Pts',(-20.8306684931562,-20.4208707328441,
-3.3555204308465));
#64344=CARTESIAN_POINT('Ctrl Pts',(-20.8789026140616,-20.352021269555,-3.3596901451664));
#64345=CARTESIAN_POINT('Ctrl Pts',(-20.923760234583,-20.2807673121879,-3.36385985948629));
#64346=CARTESIAN_POINT('Ctrl Pts',(-20.965003586852,-20.2074771983009,-3.36802957380619));
#64347=CARTESIAN_POINT('Ctrl Pts',(-21.0062454715054,-20.1341896923909,
-3.37219913974974));
#64348=CARTESIAN_POINT('Ctrl Pts',(-21.0438731187515,-20.0588665753507,
-3.3763687056933));
#64349=CARTESIAN_POINT('Ctrl Pts',(-21.0776941561667,-19.9819017925755,
-3.38053827163685));
#64350=CARTESIAN_POINT('Ctrl Pts',(-21.1127042995432,-19.9022310229647,
-3.38485443437633));
#64351=CARTESIAN_POINT('Ctrl Pts',(-21.1436349596428,-19.8208014806364,
-3.38917059711581));
#64352=CARTESIAN_POINT('Ctrl Pts',(-21.1703273243944,-19.7380719867856,
-3.39348675985529));
#64353=CARTESIAN_POINT('Ctrl Pts',(-21.1961501881654,-19.6580373975152,
-3.39766232404647));
#64354=CARTESIAN_POINT('Ctrl Pts',(-21.2180065643708,-19.5767867151054,
-3.40183788823765));
#64355=CARTESIAN_POINT('Ctrl Pts',(-21.2358041974883,-19.4947483371046,
-3.40601345242883));
#64356=CARTESIAN_POINT('Ctrl Pts',(-21.2545007467516,-19.4085663956271,
-3.41039991444246));
#64357=CARTESIAN_POINT('Ctrl Pts',(-21.2687176692139,-19.3215156705805,
-3.41478637645609));
#64358=CARTESIAN_POINT('Ctrl Pts',(-21.2784095170101,-19.2340996450695,
-3.41917283846971));
#64359=CARTESIAN_POINT('Ctrl Pts',(-21.2881013648063,-19.1466836195585,
-3.42355930048334));
#64360=CARTESIAN_POINT('Ctrl Pts',(-21.293268179777,-19.0589028772671,-3.42794576249697));
#64361=CARTESIAN_POINT('Ctrl Pts',(-21.2939275539577,-18.9712592442245,
-3.43233222451059));
#64362=CARTESIAN_POINT('Ctrl Pts',(-21.2939755504833,-18.9648795739236,
-3.43265151959756));
#64363=CARTESIAN_POINT('Ctrl Pts',(-21.2939996986147,-18.958499723977,-3.43297081468453));
#64364=CARTESIAN_POINT('Ctrl Pts',(-21.2939999971965,-18.9521198086916,
-3.4332901097715));
#64365=CARTESIAN_POINT('Ctrl Pts',(-21.2939999971965,-18.9521198080496,
-3.43329010980363));
#64366=CARTESIAN_POINT('Ctrl Pts',(-21.294003905102,-18.8686175883755,-3.43746913841141));
#64367=CARTESIAN_POINT('Ctrl Pts',(-21.2899179933662,-18.784957797327,-3.44164816701919));
#64368=CARTESIAN_POINT('Ctrl Pts',(-21.2817219740999,-18.7015748760837,
-3.44582719562697));
#64369=CARTESIAN_POINT('Ctrl Pts',(-21.2735376207105,-18.6183106386626,
-3.45000027597723));
#64370=CARTESIAN_POINT('Ctrl Pts',(-21.2612548239782,-18.5353229435677,
-3.45417335632749));
#64371=CARTESIAN_POINT('Ctrl Pts',(-21.2449053023278,-18.4530465324881,
-3.45834643667775));
#64372=CARTESIAN_POINT('Ctrl Pts',(-21.228391285294,-18.3699423241145,-3.46256150311585));
#64373=CARTESIAN_POINT('Ctrl Pts',(-21.2077282378307,-18.287564271427,-3.46677656955394));
#64374=CARTESIAN_POINT('Ctrl Pts',(-21.1830026840864,-18.2063554108441,
-3.47099163599204));
#64375=CARTESIAN_POINT('Ctrl Pts',(-21.1585674190593,-18.1260999774808,
-3.47515721572331));
#64376=CARTESIAN_POINT('Ctrl Pts',(-21.1301646741428,-18.0469868800103,
-3.47932279545459));
#64377=CARTESIAN_POINT('Ctrl Pts',(-21.0979289771719,-17.9694320426113,
-3.48348837518587));
#64378=CARTESIAN_POINT('Ctrl Pts',(-21.0657039544922,-17.8919028861496,
-3.48765257555777));
#64379=CARTESIAN_POINT('Ctrl Pts',(-21.0296486772609,-17.815931390789,-3.49181677592968));
#64380=CARTESIAN_POINT('Ctrl Pts',(-20.9899463178963,-17.7419147919381,
-3.49598097630159));
#64381=CARTESIAN_POINT('Ctrl Pts',(-20.9502451090693,-17.6679003380199,
-3.50014505599882));
#64382=CARTESIAN_POINT('Ctrl Pts',(-20.9068972472216,-17.5958410741357,
-3.50430913569606));
#64383=CARTESIAN_POINT('Ctrl Pts',(-20.8601318431732,-17.5261096166098,
-3.50847321539329));
#64384=CARTESIAN_POINT('Ctrl Pts',(-20.8123689128482,-17.4548907569624,
-3.51272611670985));
#64385=CARTESIAN_POINT('Ctrl Pts',(-20.7610412266544,-17.3861005826242,
-3.51697901802641));
#64386=CARTESIAN_POINT('Ctrl Pts',(-20.7064383509254,-17.3201032655836,
-3.52123191934298));
#64387=CARTESIAN_POINT('Ctrl Pts',(-20.6528987388226,-17.2553910923328,
-3.52540200532764));
#64388=CARTESIAN_POINT('Ctrl Pts',(-20.5962107113946,-17.1933642853479,
-3.52957209131231));
#64389=CARTESIAN_POINT('Ctrl Pts',(-20.5366855500211,-17.1343298407728,
-3.53374217729697));
#64390=CARTESIAN_POINT('Ctrl Pts',(-20.4753871892412,-17.0735368147901,
-3.53803648627948));
#64391=CARTESIAN_POINT('Ctrl Pts',(-20.4110803806519,-17.0159176096093,
-3.54233079526199));
#64392=CARTESIAN_POINT('Ctrl Pts',(-20.344141220394,-16.9617625140732,-3.5466251042445));
#64393=CARTESIAN_POINT('Ctrl Pts',(-20.277202060136,-16.9076074185371,-3.55091941322701));
#64394=CARTESIAN_POINT('Ctrl Pts',(-20.2076310154015,-16.8569166856669,
-3.55521372220952));
#64395=CARTESIAN_POINT('Ctrl Pts',(-20.1358342086541,-16.8099307080659,
-3.55950803119203));
#64396=CARTESIAN_POINT('Ctrl Pts',(-20.065871057879,-16.7641447297733,-3.56369266558497));
#64397=CARTESIAN_POINT('Ctrl Pts',(-19.9935321931096,-16.7217048000893,
-3.56787729997791));
#64398=CARTESIAN_POINT('Ctrl Pts',(-19.9191711337668,-16.6828659396841,
-3.57206193437085));
#64399=CARTESIAN_POINT('Ctrl Pts',(-19.844915918188,-16.6440823615894,-3.57624061245468));
#64400=CARTESIAN_POINT('Ctrl Pts',(-19.7686446296087,-16.6088898827212,
-3.58041929053851));
#64401=CARTESIAN_POINT('Ctrl Pts',(-19.6907394622033,-16.5775001365629,
-3.58459796862235));
#64402=CARTESIAN_POINT('Ctrl Pts',(-19.6114379006591,-16.545547751763,-3.58885154650781));
#64403=CARTESIAN_POINT('Ctrl Pts',(-19.5304437130242,-16.5175360325718,
-3.59310512439327));
#64404=CARTESIAN_POINT('Ctrl Pts',(-19.4481859912091,-16.4936390887502,
-3.59735870227874));
#64405=CARTESIAN_POINT('Ctrl Pts',(-19.3675229958468,-16.4702054338166,
-3.60152981625657));
#64406=CARTESIAN_POINT('Ctrl Pts',(-19.2856454833716,-16.4507285663624,
-3.60570093023441));
#64407=CARTESIAN_POINT('Ctrl Pts',(-19.202976239882,-16.4353233647474,-3.60987204421224));
#64408=CARTESIAN_POINT('Ctrl Pts',(-19.1203347368553,-16.4199233324967,
-3.6140417585325));
#64409=CARTESIAN_POINT('Ctrl Pts',(-19.0369024823163,-16.408592336823,-3.61821147285276));
#64410=CARTESIAN_POINT('Ctrl Pts',(-18.9531132034113,-16.4013943064262,
-3.62238118717302));
#64411=CARTESIAN_POINT('Ctrl Pts',(-18.8693269060884,-16.3941965321663,
-3.62655075311694));
#64412=CARTESIAN_POINT('Ctrl Pts',(-18.785184068077,-16.3911314692988,-3.63072031906087));
#64413=CARTESIAN_POINT('Ctrl Pts',(-18.7011229313378,-16.3922111223079,
-3.63488988500479));
#64414=CARTESIAN_POINT('Ctrl Pts',(-18.6141063087262,-16.3933287345849,
-3.63920604774385));
#64415=CARTESIAN_POINT('Ctrl Pts',(-18.5271777668963,-16.398887935209,-3.6435222104829));
#64416=CARTESIAN_POINT('Ctrl Pts',(-18.4408207068908,-16.4088433193977,
-3.64783837322196));
#64417=CARTESIAN_POINT('Ctrl Pts',(-18.3572767190367,-16.418474407993,-3.65201393741352));
#64418=CARTESIAN_POINT('Ctrl Pts',(-18.2742680097319,-16.4322195436239,
-3.65618950160509));
#64419=CARTESIAN_POINT('Ctrl Pts',(-18.1922227301014,-16.4499853338117,
-3.66036506579666));
#64420=CARTESIAN_POINT('Ctrl Pts',(-18.1060335384334,-16.4686484318294,
-3.66475152780946));
#64421=CARTESIAN_POINT('Ctrl Pts',(-18.0209082233736,-16.4917488722623,
-3.66913798982226));
#64422=CARTESIAN_POINT('Ctrl Pts',(-17.9373239039191,-16.5191195676866,
-3.67352445183506));
#64423=CARTESIAN_POINT('Ctrl Pts',(-17.8537395844646,-16.5464902631109,
-3.67791091384786));
#64424=CARTESIAN_POINT('Ctrl Pts',(-17.7716967745984,-16.578130933778,-3.68229737586066));
#64425=CARTESIAN_POINT('Ctrl Pts',(-17.6916449845523,-16.6138177954293,
-3.68668383787345));
#64426=CARTESIAN_POINT('Ctrl Pts',(-17.6152736995718,-16.6478638983293,
-3.6908686254996));
#64427=CARTESIAN_POINT('Ctrl Pts',(-17.5404300949984,-16.6857190326274,
-3.69505341312575));
#64428=CARTESIAN_POINT('Ctrl Pts',(-17.4675200004886,-16.7272239638926,
-3.6992382007519));
#64429=CARTESIAN_POINT('Ctrl Pts',(-17.3947226532098,-16.7686647124668,
-3.70341651707638));
#64430=CARTESIAN_POINT('Ctrl Pts',(-17.3238532703242,-16.813743815844,-3.70759483340085));
#64431=CARTESIAN_POINT('Ctrl Pts',(-17.2552965767961,-16.8622545164051,
-3.71177314972532));
#64432=CARTESIAN_POINT('Ctrl Pts',(-17.2279776972385,-16.8815853492922,
-3.71343815010015));
#64433=CARTESIAN_POINT('Ctrl Pts',(-17.2010258025195,-16.9014605652034,
-3.71510315047499));
#64434=CARTESIAN_POINT('Ctrl Pts',(-17.1744641548914,-16.9218650419685,
-3.71676815084982));
#64435=CARTESIAN_POINT('',(-21.2936055506457,-18.9523823947329,-3.36670986511492));
#64436=CARTESIAN_POINT('Ctrl Pts',(-21.2939999715072,-18.9523819467093,
-3.36670989022851));
#64437=CARTESIAN_POINT('Ctrl Pts',(-21.2940130064034,-18.8650154810554,
-3.3710315430356));
#64438=CARTESIAN_POINT('Ctrl Pts',(-21.2895493128086,-18.777713537132,-3.37535319584269));
#64439=CARTESIAN_POINT('Ctrl Pts',(-21.2806546261691,-18.690944038544,-3.37967484864978));
#64440=CARTESIAN_POINT('Ctrl Pts',(-21.2713805337795,-18.6004733587877,
-3.3841808429622));
#64441=CARTESIAN_POINT('Ctrl Pts',(-21.2572890869443,-18.5105820575898,
-3.38868683727461));
#64442=CARTESIAN_POINT('Ctrl Pts',(-21.2384911684206,-18.4217887333304,
-3.39319283158702));
#64443=CARTESIAN_POINT('Ctrl Pts',(-21.2204017935412,-18.3363422660907,
-3.39752898296562));
#64444=CARTESIAN_POINT('Ctrl Pts',(-21.1979545494933,-18.2519128648075,
-3.40186513434422));
#64445=CARTESIAN_POINT('Ctrl Pts',(-21.1712990035407,-18.1689459997295,
-3.40620128572282));
#64446=CARTESIAN_POINT('Ctrl Pts',(-21.1446099328527,-18.0858747870536,
-3.41054289068799));
#64447=CARTESIAN_POINT('Ctrl Pts',(-21.1137021554184,-18.0042701592823,
-3.41488449565315));
#64448=CARTESIAN_POINT('Ctrl Pts',(-21.078773161122,-17.9245571437388,-3.41922610061831));
#64449=CARTESIAN_POINT('Ctrl Pts',(-21.043770395337,-17.8446757709914,-3.42357687523372));
#64450=CARTESIAN_POINT('Ctrl Pts',(-21.004729634837,-17.7666943545291,-3.42792764984912));
#64451=CARTESIAN_POINT('Ctrl Pts',(-20.9618940508663,-17.6910130460174,
-3.43227842446453));
#64452=CARTESIAN_POINT('Ctrl Pts',(-20.9570751477607,-17.6824990756493,
-3.4327678764426));
#64453=CARTESIAN_POINT('Ctrl Pts',(-20.9522082623988,-17.6740141830165,
-3.43325732842066));
#64454=CARTESIAN_POINT('Ctrl Pts',(-20.9472937739975,-17.6655589131313,
-3.43374678039873));
#64455=CARTESIAN_POINT('Ctrl Pts',(-20.9052767057113,-17.5932694654538,
-3.43793141479118));
#64456=CARTESIAN_POINT('Ctrl Pts',(-20.8596361007271,-17.5229061642046,
-3.44211604918361));
#64457=CARTESIAN_POINT('Ctrl Pts',(-20.8105736599317,-17.4548554395524,
-3.44630068357606));
#64458=CARTESIAN_POINT('Ctrl Pts',(-20.7615810534481,-17.3869015766837,
-3.45047936165939));
#64459=CARTESIAN_POINT('Ctrl Pts',(-20.709176552354,-17.3212541220957,-3.45465803974273));
#64460=CARTESIAN_POINT('Ctrl Pts',(-20.6536069384427,-17.258273575254,-3.45883671782607));
#64461=CARTESIAN_POINT('Ctrl Pts',(-20.597041279129,-17.1941641473619,-3.46309029571166));
#64462=CARTESIAN_POINT('Ctrl Pts',(-20.5371961639064,-17.132818593104,-3.46734387359724));
#64463=CARTESIAN_POINT('Ctrl Pts',(-20.47437711685,-17.0745848910949,-3.47159745148283));
#64464=CARTESIAN_POINT('Ctrl Pts',(-20.4127759396133,-17.0174801630435,
-3.47576856546017));
#64465=CARTESIAN_POINT('Ctrl Pts',(-20.3483154653818,-16.9633680324696,
-3.47993967943751));
#64466=CARTESIAN_POINT('Ctrl Pts',(-20.2813221318917,-16.9125407039713,
-3.48411079341485));
#64467=CARTESIAN_POINT('Ctrl Pts',(-20.2143512786617,-16.8617304310738,
-3.48828050773461));
#64468=CARTESIAN_POINT('Ctrl Pts',(-20.144849620325,-16.8142030489945,-3.49245022205437));
#64469=CARTESIAN_POINT('Ctrl Pts',(-20.0731762130978,-16.7702101223369,
-3.49661993637414));
#64470=CARTESIAN_POINT('Ctrl Pts',(-20.0015053563181,-16.7262187611365,
-3.50078950231757));
#64471=CARTESIAN_POINT('Ctrl Pts',(-19.9276632968148,-16.6857618452166,
-3.504959068261));
#64472=CARTESIAN_POINT('Ctrl Pts',(-19.852036401666,-16.6490465474635,-3.50912863420443));
#64473=CARTESIAN_POINT('Ctrl Pts',(-19.7737505581551,-16.6110403851227,
-3.51344479694407));
#64474=CARTESIAN_POINT('Ctrl Pts',(-19.6935525085948,-16.5770440773061,
-3.51776095968372));
#64475=CARTESIAN_POINT('Ctrl Pts',(-19.6118947218445,-16.5472337208457,
-3.52207712242336));
#64476=CARTESIAN_POINT('Ctrl Pts',(-19.5328969289333,-16.5183944336205,
-3.52625268661445));
#64477=CARTESIAN_POINT('Ctrl Pts',(-19.4525335041398,-16.4934726654687,
-3.53042825080553));
#64478=CARTESIAN_POINT('Ctrl Pts',(-19.3712290384546,-16.4725768508481,
-3.53460381499661));
#64479=CARTESIAN_POINT('Ctrl Pts',(-19.2858180774515,-16.4506256382961,
-3.53899027701054));
#64480=CARTESIAN_POINT('Ctrl Pts',(-19.1993690855433,-16.4331178853207,
-3.54337673902446));
#64481=CARTESIAN_POINT('Ctrl Pts',(-19.1123834602669,-16.4201180997139,
-3.54776320103839));
#64482=CARTESIAN_POINT('Ctrl Pts',(-19.0253978349906,-16.4071183141071,
-3.55214966305231));
#64483=CARTESIAN_POINT('Ctrl Pts',(-18.937876161197,-16.3986264761921,-3.55653612506623));
#64484=CARTESIAN_POINT('Ctrl Pts',(-18.8503205710795,-16.3946440363642,
-3.56092258708016));
#64485=CARTESIAN_POINT('Ctrl Pts',(-18.7668123251306,-16.3908456887752,
-3.5651062805281));
#64486=CARTESIAN_POINT('Ctrl Pts',(-18.68296246577,-16.3911349078501,-3.56928997397603));
#64487=CARTESIAN_POINT('Ctrl Pts',(-18.5992048029022,-16.3955512414994,
-3.57347366742397));
#64488=CARTESIAN_POINT('Ctrl Pts',(-18.5155577245137,-16.3999617443035,
-3.57765183717956));
#64489=CARTESIAN_POINT('Ctrl Pts',(-18.432003055976,-16.4084885197961,-3.58183000693514));
#64490=CARTESIAN_POINT('Ctrl Pts',(-18.3489773389922,-16.4211192144808,
-3.58600817669073));
#64491=CARTESIAN_POINT('Ctrl Pts',(-18.2660363238864,-16.4337370234765,
-3.59018208392577));
#64492=CARTESIAN_POINT('Ctrl Pts',(-18.1836236408616,-16.4504503679989,
-3.59435599116082));
#64493=CARTESIAN_POINT('Ctrl Pts',(-18.1021720696082,-16.4711949963012,
-3.59852989839586));
#64494=CARTESIAN_POINT('Ctrl Pts',(-18.0183963696073,-16.4925315491822,
-3.6028229033677));
#64495=CARTESIAN_POINT('Ctrl Pts',(-17.935637962523,-16.5181329065888,-3.60711590833953));
#64496=CARTESIAN_POINT('Ctrl Pts',(-17.8543574201688,-16.5478725217352,
-3.61140891331137));
#64497=CARTESIAN_POINT('Ctrl Pts',(-17.7754110233124,-16.5767580999032,
-3.61557863541702));
#64498=CARTESIAN_POINT('Ctrl Pts',(-17.6978592079438,-16.6095472799744,
-3.61974835752268));
#64499=CARTESIAN_POINT('Ctrl Pts',(-17.6221076630951,-16.6460738452561,
-3.62391807962833));
#64500=CARTESIAN_POINT('Ctrl Pts',(-17.5429965894828,-16.6842203385134,
-3.62827272603326));
#64501=CARTESIAN_POINT('Ctrl Pts',(-17.4658496781218,-16.7264432229003,
-3.63262737243819));
#64502=CARTESIAN_POINT('Ctrl Pts',(-17.3911026572817,-16.7724985141275,
-3.63698201884312));
#64503=CARTESIAN_POINT('Ctrl Pts',(-17.3163556364417,-16.8185538053548,
-3.64133666524805));
#64504=CARTESIAN_POINT('Ctrl Pts',(-17.2440089783775,-16.8684411823186,
-3.64569131165298));
#64505=CARTESIAN_POINT('Ctrl Pts',(-17.1744641548914,-16.9218650419685,
-3.65004595805791));
#64506=CARTESIAN_POINT('Ctrl Pts',(-17.1767158332876,-16.9247660182631,
-2.85017128494026));
#64507=CARTESIAN_POINT('Ctrl Pts',(-16.7788811275464,-17.2333456901826,
-2.87512870785117));
#64508=CARTESIAN_POINT('Ctrl Pts',(-15.9356499015846,-18.3705873270218,
-2.94247806632256));
#64509=CARTESIAN_POINT('Ctrl Pts',(-16.3642905680513,-20.8355519717216,
-3.05221936035442));
#64510=CARTESIAN_POINT('Ctrl Pts',(-19.0350903593913,-21.9640815770127,
-3.17939516703586));
#64511=CARTESIAN_POINT('Ctrl Pts',(-21.0089153287167,-20.6164715882702,
-3.28422525530707));
#64512=CARTESIAN_POINT('Ctrl Pts',(-21.2903730986671,-19.3569817773889,
-3.34666340801782));
#64513=CARTESIAN_POINT('Ctrl Pts',(-21.2898370719784,-18.9523866753572,
-3.36670962516808));
#64514=CARTESIAN_POINT('Origin',(-18.734,-18.952,1.76670989022851));
#64515=CARTESIAN_POINT('',(-17.1744641548914,-16.9218650419685,-2.05017637359282));
#64516=CARTESIAN_POINT('',(-17.1744641548914,-16.9218650419685,-2.11663751509287));
#64517=CARTESIAN_POINT('',(-17.1744641548914,-16.9218650419685,1.76670989022851));
#64518=CARTESIAN_POINT('',(-21.2939989850553,-18.9497204131755,-2.63329010980608));
#64519=CARTESIAN_POINT('Ctrl Pts',(-17.1744641548914,-16.9218650419685,
-2.11663751509287));
#64520=CARTESIAN_POINT('Ctrl Pts',(-17.1077528165205,-16.9731122376552,
-2.12081218003139));
#64521=CARTESIAN_POINT('Ctrl Pts',(-17.0436083247207,-17.0276217853659,
-2.1249868449699));
#64522=CARTESIAN_POINT('Ctrl Pts',(-16.9823525759525,-17.085095797362,-2.12916150990842));
#64523=CARTESIAN_POINT('Ctrl Pts',(-16.9210594741501,-17.1426048563336,
-2.13333872050844));
#64524=CARTESIAN_POINT('Ctrl Pts',(-16.8626589411317,-17.2030816470779,
-2.13751593110846));
#64525=CARTESIAN_POINT('Ctrl Pts',(-16.8074345510184,-17.2661929022601,
-2.14169314170848));
#64526=CARTESIAN_POINT('Ctrl Pts',(-16.7521184201283,-17.3294090001678,
-2.14587729164354));
#64527=CARTESIAN_POINT('Ctrl Pts',(-16.6999892500854,-17.3952679385715,
-2.15006144157861));
#64528=CARTESIAN_POINT('Ctrl Pts',(-16.6512887918949,-17.4634053528132,
-2.15424559151367));
#64529=CARTESIAN_POINT('Ctrl Pts',(-16.6267354913389,-17.4977581797299,
-2.15635511357453));
#64530=CARTESIAN_POINT('Ctrl Pts',(-16.6030530181617,-17.5326897371648,
-2.15846463563539));
#64531=CARTESIAN_POINT('Ctrl Pts',(-16.5802679097402,-17.5681509896722,
-2.16057415769624));
#64532=CARTESIAN_POINT('Ctrl Pts',(-16.5350693576943,-17.6384950599053,
-2.16475879183957));
#64533=CARTESIAN_POINT('Ctrl Pts',(-16.493236628805,-17.7111867434462,-2.1689434259829));
#64534=CARTESIAN_POINT('Ctrl Pts',(-16.4550217747166,-17.78587039799,-2.17312806012622));
#64535=CARTESIAN_POINT('Ctrl Pts',(-16.4168613147862,-17.860447749511,-2.17730673795607));
#64536=CARTESIAN_POINT('Ctrl Pts',(-16.3823087086902,-17.9370110341541,
-2.18148541578591));
#64537=CARTESIAN_POINT('Ctrl Pts',(-16.3515723823109,-18.015176299151,-2.18566409361575));
#64538=CARTESIAN_POINT('Ctrl Pts',(-16.3202851270053,-18.094742626363,-2.18991767156416));
#64539=CARTESIAN_POINT('Ctrl Pts',(-16.2929525719636,-18.17596852444,-2.19417124951258));
#64540=CARTESIAN_POINT('Ctrl Pts',(-16.2697452280173,-18.2584234586145,
-2.19842482746099));
#64541=CARTESIAN_POINT('Ctrl Pts',(-16.2469878054909,-18.3392798366959,
-2.20259594117589));
#64542=CARTESIAN_POINT('Ctrl Pts',(-16.2281972006544,-18.4213175582041,
-2.20676705489078));
#64543=CARTESIAN_POINT('Ctrl Pts',(-16.2134847477736,-18.5041128900111,
-2.21093816860568));
#64544=CARTESIAN_POINT('Ctrl Pts',(-16.1987772318086,-18.5868804389882,
-2.21510788266023));
#64545=CARTESIAN_POINT('Ctrl Pts',(-16.1881452304225,-18.6704046408108,
-2.21927759671478));
#64546=CARTESIAN_POINT('Ctrl Pts',(-16.1816490383963,-18.7542512482957,
-2.22344731076934));
#64547=CARTESIAN_POINT('Ctrl Pts',(-16.1751530775363,-18.8380948721096,
-2.22761687644513));
#64548=CARTESIAN_POINT('Ctrl Pts',(-16.1727926681059,-18.9222604200508,
-2.23178644212093));
#64549=CARTESIAN_POINT('Ctrl Pts',(-16.1745761446872,-19.0063095650504,
-2.23595600779672));
#64550=CARTESIAN_POINT('Ctrl Pts',(-16.1764223263562,-19.0933137861386,
-2.24027217084513));
#64551=CARTESIAN_POINT('Ctrl Pts',(-16.1827092038591,-19.1801927391925,
-2.24458833389355));
#64552=CARTESIAN_POINT('Ctrl Pts',(-16.1933873263743,-19.2664634201504,
-2.24890449694196));
#64553=CARTESIAN_POINT('Ctrl Pts',(-16.2037176087591,-19.3499238313372,
-2.25308006086206));
#64554=CARTESIAN_POINT('Ctrl Pts',(-16.218157311486,-19.4328145349869,-2.25725562478215));
#64555=CARTESIAN_POINT('Ctrl Pts',(-16.2366094603544,-19.5147081770233,
-2.26143118870225));
#64556=CARTESIAN_POINT('Ctrl Pts',(-16.2559935873087,-19.600738089599,-2.26581765131482));
#64557=CARTESIAN_POINT('Ctrl Pts',(-16.2798059943325,-19.6856670076962,
-2.27020411392739));
#64558=CARTESIAN_POINT('Ctrl Pts',(-16.3078756047366,-19.7690192278692,
-2.27459057653996));
#64559=CARTESIAN_POINT('Ctrl Pts',(-16.3359452151407,-19.8523714480422,
-2.27897703915254));
#64560=CARTESIAN_POINT('Ctrl Pts',(-16.3682717448824,-19.9341464586679,
-2.28336350176511));
#64561=CARTESIAN_POINT('Ctrl Pts',(-16.4046276535555,-20.0138966388589,
-2.28774996437768));
#64562=CARTESIAN_POINT('Ctrl Pts',(-16.4393107693605,-20.0899773871051,
-2.29193459890665));
#64563=CARTESIAN_POINT('Ctrl Pts',(-16.4777897133297,-20.1644987286687,
-2.29611923343562));
#64564=CARTESIAN_POINT('Ctrl Pts',(-16.5199018772369,-20.2370562255314,
-2.30030386796459));
#64565=CARTESIAN_POINT('Ctrl Pts',(-16.5619540997103,-20.3095104458109,
-2.30448254618615));
#64566=CARTESIAN_POINT('Ctrl Pts',(-16.6076290410699,-20.380005979242,-2.30866122440772));
#64567=CARTESIAN_POINT('Ctrl Pts',(-16.6567166746768,-20.4481597462618,
-2.31283990262929));
#64568=CARTESIAN_POINT('Ctrl Pts',(-16.7066841667901,-20.5175351177317,
-2.31709348048053));
#64569=CARTESIAN_POINT('Ctrl Pts',(-16.7601876992645,-20.5844835062087,
-2.32134705833178));
#64570=CARTESIAN_POINT('Ctrl Pts',(-16.8169575547711,-20.6486284988738,
-2.32560063618302));
#64571=CARTESIAN_POINT('Ctrl Pts',(-16.8726268181782,-20.7115299183165,
-2.32977175030178));
#64572=CARTESIAN_POINT('Ctrl Pts',(-16.931436568049,-20.7717353099527,-2.33394286442054));
#64573=CARTESIAN_POINT('Ctrl Pts',(-16.9930907749213,-20.8289217005608,
-2.3381139785393));
#64574=CARTESIAN_POINT('Ctrl Pts',(-17.0547242931429,-20.8860889017359,
-2.34228369300136));
#64575=CARTESIAN_POINT('Ctrl Pts',(-17.1192000357421,-20.9402388012432,
-2.34645340746342));
#64576=CARTESIAN_POINT('Ctrl Pts',(-17.1861855059002,-20.9910856509364,
-2.35062312192549));
#64577=CARTESIAN_POINT('Ctrl Pts',(-17.253168592439,-21.041930691289,-2.35479268801191));
#64578=CARTESIAN_POINT('Ctrl Pts',(-17.3226608620329,-21.0894726380556,
-2.35896225409833));
#64579=CARTESIAN_POINT('Ctrl Pts',(-17.3942982622585,-21.1334672250329,
-2.36313182018476));
#64580=CARTESIAN_POINT('Ctrl Pts',(-17.4684543397166,-21.1790086041077,
-2.36744798275762));
#64581=CARTESIAN_POINT('Ctrl Pts',(-17.5449087502468,-21.2207482563335,
-2.37176414533048));
#64582=CARTESIAN_POINT('Ctrl Pts',(-17.6232285972719,-21.2584663212112,
-2.37608030790335));
#64583=CARTESIAN_POINT('Ctrl Pts',(-17.6989971890216,-21.2949557267432,
-2.38025587223768));
#64584=CARTESIAN_POINT('Ctrl Pts',(-17.7765110983774,-21.3276813875021,
-2.38443143657202));
#64585=CARTESIAN_POINT('Ctrl Pts',(-17.8553584978293,-21.3564935247705,
-2.38860700090636));
#64586=CARTESIAN_POINT('Ctrl Pts',(-17.9381882831052,-21.3867608913529,
-2.39299346259849));
#64587=CARTESIAN_POINT('Ctrl Pts',(-18.0224892495074,-21.4127088296275,
-2.39737992429061));
#64588=CARTESIAN_POINT('Ctrl Pts',(-18.1077688055337,-21.4342236988389,
-2.40176638598274));
#64589=CARTESIAN_POINT('Ctrl Pts',(-18.1930483615599,-21.4557385680502,
-2.40615284767487));
#64590=CARTESIAN_POINT('Ctrl Pts',(-18.2793059232703,-21.4728203301016,
-2.41053930936699));
#64591=CARTESIAN_POINT('Ctrl Pts',(-18.3660419494156,-21.4854180217663,
-2.41492577105912));
#64592=CARTESIAN_POINT('Ctrl Pts',(-18.4487871282886,-21.4974360758149,
-2.41911040544306));
#64593=CARTESIAN_POINT('Ctrl Pts',(-18.5322757027619,-21.5054183621378,
-2.42329503982701));
#64594=CARTESIAN_POINT('Ctrl Pts',(-18.6160795877487,-21.5092826938715,
-2.42747967421095));
#64595=CARTESIAN_POINT('Ctrl Pts',(-18.6997641882823,-21.5131415252074,
-2.43165835228601));
#64596=CARTESIAN_POINT('Ctrl Pts',(-18.7837627522466,-21.5128940235268,
-2.43583703036108));
#64597=CARTESIAN_POINT('Ctrl Pts',(-18.867639486945,-21.5085094342734,-2.44001570843614));
#64598=CARTESIAN_POINT('Ctrl Pts',(-18.9530196520584,-21.504046254397,-2.44426928632383));
#64599=CARTESIAN_POINT('Ctrl Pts',(-19.0382731002339,-21.4952961442205,
-2.44852286421151));
#64600=CARTESIAN_POINT('Ctrl Pts',(-19.1229373349508,-21.4822821481964,
-2.45277644209919));
#64601=CARTESIAN_POINT('Ctrl Pts',(-19.2059601880607,-21.469520453912,-2.45694755606889));
#64602=CARTESIAN_POINT('Ctrl Pts',(-19.2884159943129,-21.4526587990527,
-2.46111867003858));
#64603=CARTESIAN_POINT('Ctrl Pts',(-19.3698729492297,-21.4317712782509,
-2.46528978400827));
#64604=CARTESIAN_POINT('Ctrl Pts',(-19.4513025704834,-21.4108907664571,
-2.46945949832063));
#64605=CARTESIAN_POINT('Ctrl Pts',(-19.531733560818,-21.3859871858369,-2.47362921263299));
#64606=CARTESIAN_POINT('Ctrl Pts',(-19.6107456770632,-21.3571854435264,
-2.47779892694536));
#64607=CARTESIAN_POINT('Ctrl Pts',(-19.6897549817234,-21.3283847261035,
-2.48196849288167));
#64608=CARTESIAN_POINT('Ctrl Pts',(-19.7673450807596,-21.2956862811396,
-2.48613805881798));
#64609=CARTESIAN_POINT('Ctrl Pts',(-19.8431135302991,-21.2592640024296,
-2.4903076247543));
#64610=CARTESIAN_POINT('Ctrl Pts',(-19.9215459053798,-21.2215611611752,
-2.49462378750315));
#64611=CARTESIAN_POINT('Ctrl Pts',(-19.9980256738089,-21.1798679825043,
-2.498939950252));
#64612=CARTESIAN_POINT('Ctrl Pts',(-20.0721336489201,-21.1344294576522,
-2.50325611300086));
#64613=CARTESIAN_POINT('Ctrl Pts',(-20.1438275642515,-21.0904710881427,
-2.50743167718554));
#64614=CARTESIAN_POINT('Ctrl Pts',(-20.2133014733422,-21.0430079392836,
-2.51160724137021));
#64615=CARTESIAN_POINT('Ctrl Pts',(-20.2802065215954,-20.9923052204452,
-2.51578280555489));
#64616=CARTESIAN_POINT('Ctrl Pts',(-20.3504907851969,-20.9390416274998,
-2.52016926758584));
#64617=CARTESIAN_POINT('Ctrl Pts',(-20.4179394151663,-20.8822029788412,
-2.52455572961678));
#64618=CARTESIAN_POINT('Ctrl Pts',(-20.482190227081,-20.8221419544886,-2.52894219164772));
#64619=CARTESIAN_POINT('Ctrl Pts',(-20.5464410389958,-20.7620809301359,
-2.53332865367867));
#64620=CARTESIAN_POINT('Ctrl Pts',(-20.6074936847468,-20.6987980004696,
-2.53771511570961));
#64621=CARTESIAN_POINT('Ctrl Pts',(-20.6650349200516,-20.6326856153193,
-2.54210157774055));
#64622=CARTESIAN_POINT('Ctrl Pts',(-20.7194682477086,-20.5701440813393,
-2.54625111891256));
#64623=CARTESIAN_POINT('Ctrl Pts',(-20.7709705307815,-20.5048282635486,
-2.55040066008456));
#64624=CARTESIAN_POINT('Ctrl Pts',(-20.8192426277936,-20.4370465256121,
-2.55455020125656));
#64625=CARTESIAN_POINT('Ctrl Pts',(-20.8674506257188,-20.3693547930364,
-2.55869423237583));
#64626=CARTESIAN_POINT('Ctrl Pts',(-20.9124366796727,-20.2992040148273,
-2.5628382634951));
#64627=CARTESIAN_POINT('Ctrl Pts',(-20.9539402798274,-20.226937313753,-2.56698229461437));
#64628=CARTESIAN_POINT('Ctrl Pts',(-20.9954017278076,-20.1547440086875,
-2.57112211694398));
#64629=CARTESIAN_POINT('Ctrl Pts',(-21.0333875106771,-20.0804394498645,
-2.57526193927359));
#64630=CARTESIAN_POINT('Ctrl Pts',(-21.0676798966755,-20.0043963796272,
-2.5794017616032));
#64631=CARTESIAN_POINT('Ctrl Pts',(-21.1019481578627,-19.9284068059507,
-2.5835386715536));
#64632=CARTESIAN_POINT('Ctrl Pts',(-21.1325279904582,-19.8506815753028,
-2.58767558150399));
#64633=CARTESIAN_POINT('Ctrl Pts',(-21.1592478841602,-19.771617410977,-2.59181249145439));
#64634=CARTESIAN_POINT('Ctrl Pts',(-21.185962767488,-19.6925680723481,-2.59594862567316));
#64635=CARTESIAN_POINT('Ctrl Pts',(-21.2088189905539,-19.6121807387845,
-2.60008475989194));
#64636=CARTESIAN_POINT('Ctrl Pts',(-21.2276938748169,-19.5308703297809,
-2.60422089411071));
#64637=CARTESIAN_POINT('Ctrl Pts',(-21.2465668271854,-19.4495682431134,
-2.60835660498518));
#64638=CARTESIAN_POINT('Ctrl Pts',(-21.2614591515706,-19.3673437264561,
-2.61249231585964));
#64639=CARTESIAN_POINT('Ctrl Pts',(-21.2722989879432,-19.2846232821176,
-2.61662802673411));
#64640=CARTESIAN_POINT('Ctrl Pts',(-21.2831447249165,-19.2018578093952,
-2.62076598885829));
#64641=CARTESIAN_POINT('Ctrl Pts',(-21.2899335186421,-19.1185963356274,
-2.62490395098247));
#64642=CARTESIAN_POINT('Ctrl Pts',(-21.2926453380223,-19.0352708485401,
-2.62904191310665));
#64643=CARTESIAN_POINT('Ctrl Pts',(-21.2935733586036,-19.0067557610229,
-2.6304579786616));
#64644=CARTESIAN_POINT('Ctrl Pts',(-21.2940243746442,-18.9782331861905,
-2.63187404421655));
#64645=CARTESIAN_POINT('Ctrl Pts',(-21.2939989850559,-18.9497204138719,
-2.6332901097715));
#64646=CARTESIAN_POINT('Ctrl Pts',(-21.2939989850553,-18.9497204131756,
-2.63329010980608));
#64647=CARTESIAN_POINT('Ctrl Pts',(-21.2939071256071,-18.8465613267959,
-2.63841342883209));
#64648=CARTESIAN_POINT('Ctrl Pts',(-21.287576105512,-18.7436786900576,-2.6435367478581));
#64649=CARTESIAN_POINT('Ctrl Pts',(-21.275128076311,-18.6417289897787,-2.64866006688411));
#64650=CARTESIAN_POINT('Ctrl Pts',(-21.262474961387,-18.538099631808,-2.65386779441926));
#64651=CARTESIAN_POINT('Ctrl Pts',(-21.243501668497,-18.4354341184935,-2.65907552195442));
#64652=CARTESIAN_POINT('Ctrl Pts',(-21.2183850428296,-18.3343990293364,
-2.66428324948958));
#64653=CARTESIAN_POINT('Ctrl Pts',(-21.2103562166424,-18.3021019691982,
-2.66594796113372));
#64654=CARTESIAN_POINT('Ctrl Pts',(-21.2017000060005,-18.2699713447231,
-2.66761267277785));
#64655=CARTESIAN_POINT('Ctrl Pts',(-21.1924232051049,-18.2380284707345,
-2.66927738442199));
#64656=CARTESIAN_POINT('Ctrl Pts',(-21.1691038390101,-18.1577327328991,
-2.67346201883518));
#64657=CARTESIAN_POINT('Ctrl Pts',(-21.1418030734485,-18.078431236944,-2.67764665324838));
#64658=CARTESIAN_POINT('Ctrl Pts',(-21.1106233366666,-18.0005476808522,
-2.68183128766158));
#64659=CARTESIAN_POINT('Ctrl Pts',(-21.0794879803785,-17.922774982357,-2.68600996576594));
#64660=CARTESIAN_POINT('Ctrl Pts',(-21.0444847892945,-17.8464166382494,
-2.69018864387031));
#64661=CARTESIAN_POINT('Ctrl Pts',(-21.0057661997858,-17.7718820679649,
-2.69436732197467));
#64662=CARTESIAN_POINT('Ctrl Pts',(-20.9663536076263,-17.6960115195364,
-2.69862089985503));
#64663=CARTESIAN_POINT('Ctrl Pts',(-20.923091244402,-17.6220312333054,-2.7028744777354));
#64664=CARTESIAN_POINT('Ctrl Pts',(-20.8761915739221,-17.5503526618235,
-2.70712805561576));
#64665=CARTESIAN_POINT('Ctrl Pts',(-20.8302011447859,-17.4800637188825,
-2.71129916961464));
#64666=CARTESIAN_POINT('Ctrl Pts',(-20.7807134458741,-17.4119884433551,
-2.71547028361352));
#64667=CARTESIAN_POINT('Ctrl Pts',(-20.727974702693,-17.3464892136705,-2.7196413976124));
#64668=CARTESIAN_POINT('Ctrl Pts',(-20.6752536565046,-17.2810119628826,
-2.72381111195385));
#64669=CARTESIAN_POINT('Ctrl Pts',(-20.6192840209005,-17.2181093992114,
-2.7279808262953));
#64670=CARTESIAN_POINT('Ctrl Pts',(-20.560353487424,-17.1581123393662,-2.73215054063674));
#64671=CARTESIAN_POINT('Ctrl Pts',(-20.5014250509472,-17.0981174144723,
-2.73632010660198));
#64672=CARTESIAN_POINT('Ctrl Pts',(-20.4395362490537,-17.0410281154373,
-2.74048967256722));
#64673=CARTESIAN_POINT('Ctrl Pts',(-20.3750119946106,-16.987138774991,-2.74465923853245));
#64674=CARTESIAN_POINT('Ctrl Pts',(-20.308219147702,-16.9313547524166,-2.7489754012467));
#64675=CARTESIAN_POINT('Ctrl Pts',(-20.2386024799444,-16.8790002342649,
-2.75329156396095));
#64676=CARTESIAN_POINT('Ctrl Pts',(-20.1665585535975,-16.8303553571546,
-2.75760772667519));
#64677=CARTESIAN_POINT('Ctrl Pts',(-20.0968614498202,-16.7832950812909,
-2.76178329088814));
#64678=CARTESIAN_POINT('Ctrl Pts',(-20.0248932222052,-16.7397066785479,
-2.76595885510109));
#64679=CARTESIAN_POINT('Ctrl Pts',(-19.9510397172924,-16.6997978939418,
-2.77013441931403));
#64680=CARTESIAN_POINT('Ctrl Pts',(-19.8734560486543,-16.6578734121683,
-2.77452088127893));
#64681=CARTESIAN_POINT('Ctrl Pts',(-19.7937921742853,-16.6200102829178,
-2.77890734324383));
#64682=CARTESIAN_POINT('Ctrl Pts',(-19.7125190809675,-16.5863921694029,
-2.78329380520873));
#64683=CARTESIAN_POINT('Ctrl Pts',(-19.6312459876497,-16.552774055888,-2.78768026717362));
#64684=CARTESIAN_POINT('Ctrl Pts',(-19.5483642476805,-16.5234010802283,
-2.79206672913852));
#64685=CARTESIAN_POINT('Ctrl Pts',(-19.464360786173,-16.4983958913426,-2.79645319110342));
#64686=CARTESIAN_POINT('Ctrl Pts',(-19.3842194543361,-16.4745403370097,
-2.80063798179669));
#64687=CARTESIAN_POINT('Ctrl Pts',(-19.3027589678988,-16.4545709643748,
-2.80482277248996));
#64688=CARTESIAN_POINT('Ctrl Pts',(-19.2203910787736,-16.4386310023219,
-2.80900756318323));
#64689=CARTESIAN_POINT('Ctrl Pts',(-19.138141261341,-16.4227138896867,-2.81318635511502));
#64690=CARTESIAN_POINT('Ctrl Pts',(-19.0549870728687,-16.4108148007743,
-2.81736514704681));
#64691=CARTESIAN_POINT('Ctrl Pts',(-18.9713553167887,-16.4030271767647,
-2.82154393897861));
#64692=CARTESIAN_POINT('Ctrl Pts',(-18.8878237953098,-16.3952488864033,
-2.82571772253126));
#64693=CARTESIAN_POINT('Ctrl Pts',(-18.8038162997764,-16.3915723068654,
-2.82989150608392));
#64694=CARTESIAN_POINT('Ctrl Pts',(-18.7197682827838,-16.3920395592461,
-2.83406528963658));
#64695=CARTESIAN_POINT('Ctrl Pts',(-18.6357753750601,-16.392506505255,-2.8382363364898));
#64696=CARTESIAN_POINT('Ctrl Pts',(-18.5517424573058,-16.3971118856058,
-2.84240738334303));
#64697=CARTESIAN_POINT('Ctrl Pts',(-18.4681074911956,-16.4058458071512,
-2.84657843019625));
#64698=CARTESIAN_POINT('Ctrl Pts',(-18.3845022745217,-16.4145766219907,
-2.85074799338423));
#64699=CARTESIAN_POINT('Ctrl Pts',(-18.3012951853525,-16.4274330128497,
-2.85491755657221));
#64700=CARTESIAN_POINT('Ctrl Pts',(-18.2189201971835,-16.444353135561,-2.85908711976019));
#64701=CARTESIAN_POINT('Ctrl Pts',(-18.1365498000672,-16.4612723152535,
-2.8632564505635));
#64702=CARTESIAN_POINT('Ctrl Pts',(-18.055011861932,-16.4822546823771,-2.86742578136681));
#64703=CARTESIAN_POINT('Ctrl Pts',(-17.9747299315152,-16.5071873357856,
-2.87159511217012));
#64704=CARTESIAN_POINT('Ctrl Pts',(-17.894383666535,-16.5321399691742,-2.87576778409983));
#64705=CARTESIAN_POINT('Ctrl Pts',(-17.8152958594281,-16.5610490742598,
-2.87994045602953));
#64706=CARTESIAN_POINT('Ctrl Pts',(-17.7378740400419,-16.5937521182247,
-2.88411312795923));
#64707=CARTESIAN_POINT('Ctrl Pts',(-17.6604189341378,-16.6264692224438,
-2.8882875938757));
#64708=CARTESIAN_POINT('Ctrl Pts',(-17.5846316580742,-16.6629833163545,
-2.89246205979216));
#64709=CARTESIAN_POINT('Ctrl Pts',(-17.5108968677673,-16.7030849887285,
-2.89663652570862));
#64710=CARTESIAN_POINT('Ctrl Pts',(-17.4370550940829,-16.7432448454728,
-2.90081704844658));
#64711=CARTESIAN_POINT('Ctrl Pts',(-17.3652721468036,-16.7870024370522,
-2.90499757118454));
#64712=CARTESIAN_POINT('Ctrl Pts',(-17.2959049510485,-16.8341041975156,
-2.9091780939225));
#64713=CARTESIAN_POINT('Ctrl Pts',(-17.2545430745508,-16.8621897670402,
-2.91167083221616));
#64714=CARTESIAN_POINT('Ctrl Pts',(-17.2140395108878,-16.8914635230867,
-2.91416357050983));
#64715=CARTESIAN_POINT('Ctrl Pts',(-17.1744641548914,-16.9218650419685,
-2.9166563088035));
#64716=CARTESIAN_POINT('',(-21.2939990581247,-18.9541959965425,-2.56670989022851));
#64717=CARTESIAN_POINT('Ctrl Pts',(-21.2953147714723,-18.9541844553181,
-2.56671052139392));
#64718=CARTESIAN_POINT('Ctrl Pts',(-21.288986792687,-18.2584132339351,-2.60137099436598));
#64719=CARTESIAN_POINT('Ctrl Pts',(-20.6359183782719,-16.7012242333178,
-2.67842340289853));
#64720=CARTESIAN_POINT('Ctrl Pts',(-18.5512406649392,-16.1584580776078,
-2.77291032408065));
#64721=CARTESIAN_POINT('Ctrl Pts',(-17.4546313149639,-16.7092014460441,
-2.8327367722907));
#64722=CARTESIAN_POINT('Ctrl Pts',(-17.1767158332876,-16.9247660182631,
-2.85017128494026));
#64723=CARTESIAN_POINT('Ctrl Pts',(-17.1744641548914,-16.9218650419685,
-2.05017637359282));
#64724=CARTESIAN_POINT('Ctrl Pts',(-17.1080052683081,-16.9729183059117,
-2.05435390665174));
#64725=CARTESIAN_POINT('Ctrl Pts',(-17.0439627308144,-17.0273100309957,
-2.05853143971067));
#64726=CARTESIAN_POINT('Ctrl Pts',(-16.9826883158293,-17.0847808417631,
-2.06270897276959));
#64727=CARTESIAN_POINT('Ctrl Pts',(-16.9214786472874,-17.1421909252172,
-2.06688209158143));
#64728=CARTESIAN_POINT('Ctrl Pts',(-16.8630316217416,-17.2026733145463,
-2.07105521039328));
#64729=CARTESIAN_POINT('Ctrl Pts',(-16.8076661469867,-17.2659282676188,
-2.07522832920512));
#64730=CARTESIAN_POINT('Ctrl Pts',(-16.7523324560721,-17.3291469077122,
-2.07939905234092));
#64731=CARTESIAN_POINT('Ctrl Pts',(-16.700077106004,-17.3951346061225,-2.08356977547672));
#64732=CARTESIAN_POINT('Ctrl Pts',(-16.6511815089029,-17.4635554652107,
-2.08774049861252));
#64733=CARTESIAN_POINT('Ctrl Pts',(-16.6022993137412,-17.5319575706226,
-2.09191007858244));
#64734=CARTESIAN_POINT('Ctrl Pts',(-16.5567753097313,-17.6027911379656,
-2.09607965855236));
#64735=CARTESIAN_POINT('Ctrl Pts',(-16.5148491823605,-17.6756890470696,
-2.10024923852227));
#64736=CARTESIAN_POINT('Ctrl Pts',(-16.4729219698532,-17.7485888429253,
-2.10441892640972));
#64737=CARTESIAN_POINT('Ctrl Pts',(-16.434593047127,-17.8235526871958,-2.10858861429716));
#64738=CARTESIAN_POINT('Ctrl Pts',(-16.4000568074652,-17.9001876716732,
-2.11275830218461));
#64739=CARTESIAN_POINT('Ctrl Pts',(-16.3654854752132,-17.9769005256618,
-2.11693222693019));
#64740=CARTESIAN_POINT('Ctrl Pts',(-16.3347147131887,-18.0552874912678,
-2.12110615167577));
#64741=CARTESIAN_POINT('Ctrl Pts',(-16.307891067568,-18.1349348569584,-2.12528007642135));
#64742=CARTESIAN_POINT('Ctrl Pts',(-16.2810541182091,-18.2146217253965,
-2.12945607131067));
#64743=CARTESIAN_POINT('Ctrl Pts',(-16.2581683100149,-18.2955697959418,
-2.13363206619998));
#64744=CARTESIAN_POINT('Ctrl Pts',(-16.239329813502,-18.3773517070432,-2.13780806108929));
#64745=CARTESIAN_POINT('Ctrl Pts',(-16.2204575476003,-18.4592802182279,
-2.14199154175622));
#64746=CARTESIAN_POINT('Ctrl Pts',(-16.205647171031,-18.542045102734,-2.14617502242315));
#64747=CARTESIAN_POINT('Ctrl Pts',(-16.1949433667954,-18.6252104448122,
-2.15035850309007));
#64748=CARTESIAN_POINT('Ctrl Pts',(-16.1850243937153,-18.7022778846793,
-2.15423523992151));
#64749=CARTESIAN_POINT('Ctrl Pts',(-16.1786313142725,-18.7796888613376,
-2.15811197675294));
#64750=CARTESIAN_POINT('Ctrl Pts',(-16.1757597065435,-18.8570968865864,
-2.16198871358438));
#64751=CARTESIAN_POINT('Ctrl Pts',(-16.172660029791,-18.9406528172576,-2.16617334887092));
#64752=CARTESIAN_POINT('Ctrl Pts',(-16.1736524807757,-19.0245162611934,
-2.17035798415747));
#64753=CARTESIAN_POINT('Ctrl Pts',(-16.1787729919005,-19.1082527986266,
-2.17454261944402));
#64754=CARTESIAN_POINT('Ctrl Pts',(-16.1838862146257,-19.1918701476969,
-2.17872129843186));
#64755=CARTESIAN_POINT('Ctrl Pts',(-16.1931157985219,-19.2753604938156,
-2.18289997741971));
#64756=CARTESIAN_POINT('Ctrl Pts',(-16.2064457143536,-19.3582872544277,
-2.18707865640756));
#64757=CARTESIAN_POINT('Ctrl Pts',(-16.2200145556947,-19.4427003949071,
-2.19133223406832));
#64758=CARTESIAN_POINT('Ctrl Pts',(-16.2378321873097,-19.5265290651159,
-2.19558581172908));
#64759=CARTESIAN_POINT('Ctrl Pts',(-16.2598262336471,-19.6093158859262,
-2.19983938938984));
#64760=CARTESIAN_POINT('Ctrl Pts',(-16.2813938883893,-19.6904977449191,
-2.20401050429063));
#64761=CARTESIAN_POINT('Ctrl Pts',(-16.3069773456877,-19.7706773249541,
-2.20818161919142));
#64762=CARTESIAN_POINT('Ctrl Pts',(-16.3364567550223,-19.8494332222854,
-2.21235273409221));
#64763=CARTESIAN_POINT('Ctrl Pts',(-16.3659262722942,-19.9281626924159,
-2.21652244934048));
#64764=CARTESIAN_POINT('Ctrl Pts',(-16.3992889841105,-20.0054689981388,
-2.22069216458874));
#64765=CARTESIAN_POINT('Ctrl Pts',(-16.4363757553429,-20.0809476650243,
-2.224861879837));
#64766=CARTESIAN_POINT('Ctrl Pts',(-16.4734612069031,-20.1564236461247,
-2.22903144671276));
#64767=CARTESIAN_POINT('Ctrl Pts',(-16.5142702507692,-20.2300717051833,
-2.23320101358851));
#64768=CARTESIAN_POINT('Ctrl Pts',(-16.5585869497193,-20.3015103040246,
-2.23737058046427));
#64769=CARTESIAN_POINT('Ctrl Pts',(-16.6044617473107,-20.3754605606929,
-2.2416867421144));
#64770=CARTESIAN_POINT('Ctrl Pts',(-16.6540951659904,-20.4470426511764,
-2.24600290376453));
#64771=CARTESIAN_POINT('Ctrl Pts',(-16.7071987886738,-20.515865994824,-2.25031906541466));
#64772=CARTESIAN_POINT('Ctrl Pts',(-16.758572590857,-20.5824474569441,-2.25449463053808));
#64773=CARTESIAN_POINT('Ctrl Pts',(-16.8131936465655,-20.646446814372,-2.25867019566151));
#64774=CARTESIAN_POINT('Ctrl Pts',(-16.8707609580349,-20.7075455768783,
-2.26284576078493));
#64775=CARTESIAN_POINT('Ctrl Pts',(-16.9312358151196,-20.7717302475935,
-2.26723222069841));
#64776=CARTESIAN_POINT('Ctrl Pts',(-16.994961954188,-20.8327132054428,-2.27161868061189));
#64777=CARTESIAN_POINT('Ctrl Pts',(-17.0615499837251,-20.8901720622953,
-2.27600514052537));
#64778=CARTESIAN_POINT('Ctrl Pts',(-17.1281380132622,-20.9476309191478,
-2.28039160043886));
#64779=CARTESIAN_POINT('Ctrl Pts',(-17.1975874283579,-21.0015653791984,
-2.28477806035234));
#64780=CARTESIAN_POINT('Ctrl Pts',(-17.2694745299266,-21.0517059669168,
-2.28916452026582));
#64781=CARTESIAN_POINT('Ctrl Pts',(-17.3380540324737,-21.0995395349439,
-2.29334915467512));
#64782=CARTESIAN_POINT('Ctrl Pts',(-17.4091070955212,-21.1440987240517,
-2.29753378908443));
#64783=CARTESIAN_POINT('Ctrl Pts',(-17.4822878905414,-21.1851181775792,
-2.30171842349373));
#64784=CARTESIAN_POINT('Ctrl Pts',(-17.5553645218076,-21.2260792450197,
-2.30589710159675));
#64785=CARTESIAN_POINT('Ctrl Pts',(-17.6305624715103,-21.2635103616649,
-2.31007577969977));
#64786=CARTESIAN_POINT('Ctrl Pts',(-17.7075059666942,-21.2971886916808,
-2.31425445780279));
#64787=CARTESIAN_POINT('Ctrl Pts',(-17.7858286182921,-21.331470681366,-2.31850803568381));
#64788=CARTESIAN_POINT('Ctrl Pts',(-17.8659596132195,-21.3618637479389,
-2.32276161356483));
#64789=CARTESIAN_POINT('Ctrl Pts',(-17.947475192358,-21.3881811769579,-2.32701519144585));
#64790=CARTESIAN_POINT('Ctrl Pts',(-18.0274104335102,-21.4139883914482,
-2.33118630544973));
#64791=CARTESIAN_POINT('Ctrl Pts',(-18.1086765942978,-21.4358764386359,
-2.33535741945361));
#64792=CARTESIAN_POINT('Ctrl Pts',(-18.1908544682179,-21.453717995959,-2.33952853345749));
#64793=CARTESIAN_POINT('Ctrl Pts',(-18.2730047666085,-21.471553566386,-2.3436982478063));
#64794=CARTESIAN_POINT('Ctrl Pts',(-18.3560657213573,-21.4853452461106,
-2.3478679621551));
#64795=CARTESIAN_POINT('Ctrl Pts',(-18.4396056840043,-21.4950163166424,
-2.35203767650391));
#64796=CARTESIAN_POINT('Ctrl Pts',(-18.5231426739907,-21.5046870430418,
-2.35620724247888));
#64797=CARTESIAN_POINT('Ctrl Pts',(-18.6071581809069,-21.5102373997233,
-2.36037680845384));
#64798=CARTESIAN_POINT('Ctrl Pts',(-18.6912145089616,-21.5116424363095,
-2.36454637442881));
#64799=CARTESIAN_POINT('Ctrl Pts',(-18.7782261525852,-21.5130968722283,
-2.36886253713868));
#64800=CARTESIAN_POINT('Ctrl Pts',(-18.8652810139474,-21.5101090568401,
-2.37317869984855));
#64801=CARTESIAN_POINT('Ctrl Pts',(-18.9518945613347,-21.5027100893949,
-2.37749486255842));
#64802=CARTESIAN_POINT('Ctrl Pts',(-19.0356866828293,-21.4955521424246,
-2.38167042678695));
#64803=CARTESIAN_POINT('Ctrl Pts',(-19.1190653399573,-21.4842661264592,
-2.38584599101548));
#64804=CARTESIAN_POINT('Ctrl Pts',(-19.2015998086145,-21.4689327402582,
-2.39002155524401));
#64805=CARTESIAN_POINT('Ctrl Pts',(-19.2883028950859,-21.4528249015417,
-2.39440801719455));
#64806=CARTESIAN_POINT('Ctrl Pts',(-19.3740737042372,-21.4322502184736,
-2.39879447914509));
#64807=CARTESIAN_POINT('Ctrl Pts',(-19.4584303876454,-21.4073616054374,
-2.40318094109563));
#64808=CARTESIAN_POINT('Ctrl Pts',(-19.5427870710536,-21.3824729924011,
-2.40756740304617));
#64809=CARTESIAN_POINT('Ctrl Pts',(-19.6257291066931,-21.3532707138335,
-2.41195386499671));
#64810=CARTESIAN_POINT('Ctrl Pts',(-19.7068005673137,-21.3199651720906,
-2.41634032694725));
#64811=CARTESIAN_POINT('Ctrl Pts',(-19.7841418063303,-21.2881920691418,
-2.42052496109048));
#64812=CARTESIAN_POINT('Ctrl Pts',(-19.8600687027268,-21.2525667345391,
-2.4247095952337));
#64813=CARTESIAN_POINT('Ctrl Pts',(-19.9341709431478,-21.2132363227278,
-2.42889422937693));
#64814=CARTESIAN_POINT('Ctrl Pts',(-20.0081677081176,-21.1739618929342,
-2.43307290720666));
#64815=CARTESIAN_POINT('Ctrl Pts',(-20.0803445730473,-21.1309930750319,
-2.4372515850364));
#64816=CARTESIAN_POINT('Ctrl Pts',(-20.1503107695072,-21.0845252177121,
-2.44143026286614));
#64817=CARTESIAN_POINT('Ctrl Pts',(-20.2215310651425,-21.0372244538674,
-2.44568384081458));
#64818=CARTESIAN_POINT('Ctrl Pts',(-20.2904602140006,-20.9862981588784,
-2.44993741876302));
#64819=CARTESIAN_POINT('Ctrl Pts',(-20.3567118459237,-20.932001582095,-2.45419099671146));
#64820=CARTESIAN_POINT('Ctrl Pts',(-20.4216790556215,-20.8787576545515,
-2.45836211042625));
#64821=CARTESIAN_POINT('Ctrl Pts',(-20.4840712679219,-20.8222732635721,
-2.46253322414104));
#64822=CARTESIAN_POINT('Ctrl Pts',(-20.5435545161742,-20.7628319781232,
-2.46670433785583));
#64823=CARTESIAN_POINT('Ctrl Pts',(-20.6030178042074,-20.7034106388123,
-2.47087405191028));
#64824=CARTESIAN_POINT('Ctrl Pts',(-20.6595737416717,-20.6410347004966,
-2.47504376596472));
#64825=CARTESIAN_POINT('Ctrl Pts',(-20.7129241773316,-20.5760255848885,
-2.47921348001916));
#64826=CARTESIAN_POINT('Ctrl Pts',(-20.7662727145228,-20.5110187826217,
-2.48338304569485));
#64827=CARTESIAN_POINT('Ctrl Pts',(-20.8164156855257,-20.4433793455188,
-2.48755261137053));
#64828=CARTESIAN_POINT('Ctrl Pts',(-20.8630951945853,-20.3734618012432,
-2.49172217704622));
#64829=CARTESIAN_POINT('Ctrl Pts',(-20.9114159041743,-20.3010860325135,
-2.49603834009476));
#64830=CARTESIAN_POINT('Ctrl Pts',(-20.9560247758173,-20.226269417489,-2.5003545031433));
#64831=CARTESIAN_POINT('Ctrl Pts',(-20.9966856911225,-20.1494362042253,
-2.50467066619184));
#64832=CARTESIAN_POINT('Ctrl Pts',(-21.036022076007,-20.0751058349709,-2.50884623011182));
#64833=CARTESIAN_POINT('Ctrl Pts',(-21.0716636082435,-19.9988886784647,
-2.5130217940318));
#64834=CARTESIAN_POINT('Ctrl Pts',(-21.1034449999269,-19.9211905861704,
-2.51719735795179));
#64835=CARTESIAN_POINT('Ctrl Pts',(-21.1368316008925,-19.839568131463,-2.52158382056461));
#64836=CARTESIAN_POINT('Ctrl Pts',(-21.1659576672678,-19.756311755636,-2.52597028317742));
#64837=CARTESIAN_POINT('Ctrl Pts',(-21.1906909603509,-19.6719093868885,
-2.53035674579024));
#64838=CARTESIAN_POINT('Ctrl Pts',(-21.215424253434,-19.5875070181411,-2.53474320840306));
#64839=CARTESIAN_POINT('Ctrl Pts',(-21.2357647130118,-19.5019592385496,
-2.53912967101588));
#64840=CARTESIAN_POINT('Ctrl Pts',(-21.2516424693651,-19.4157632978678,
-2.54351613362869));
#64841=CARTESIAN_POINT('Ctrl Pts',(-21.2744558895146,-19.2919155598001,
-2.54981867489014));
#64842=CARTESIAN_POINT('Ctrl Pts',(-21.2881358177162,-19.1663368452798,
-2.55612121615159));
#64843=CARTESIAN_POINT('Ctrl Pts',(-21.2924829866165,-19.0401181433864,
-2.56242375741304));
#64844=CARTESIAN_POINT('Ctrl Pts',(-21.2934684379609,-19.0115058689788,
-2.56385246835153));
#64845=CARTESIAN_POINT('Ctrl Pts',(-21.2939744691011,-18.982860830915,-2.56528117929002));
#64846=CARTESIAN_POINT('Ctrl Pts',(-21.2939990581247,-18.9541959965425,
-2.56670989022851));
#64847=CARTESIAN_POINT('Origin',(-18.734,-18.952,1.76670989022851));
#64848=CARTESIAN_POINT('',(-17.1744641548914,-16.9218650419685,-1.2500388607805));
#64849=CARTESIAN_POINT('',(-17.1763037562513,-16.9242236971174,-1.31677679576761));
#64850=CARTESIAN_POINT('',(-17.1744641548914,-16.9218650419685,1.76670989022851));
#64851=CARTESIAN_POINT('',(-21.2937660511389,-18.9530076677181,-1.83329006740113));
#64852=CARTESIAN_POINT('Ctrl Pts',(-17.1763037562512,-16.9242236971175,
-1.31677679576762));
#64853=CARTESIAN_POINT('Ctrl Pts',(-16.7482596907349,-17.2576787930677,
-1.34369096971429));
#64854=CARTESIAN_POINT('Ctrl Pts',(-15.9020682097871,-18.4571854904752,
-1.41299707922144));
#64855=CARTESIAN_POINT('Ctrl Pts',(-16.4540143580209,-20.9432205748173,
-1.52469512428907));
#64856=CARTESIAN_POINT('Ctrl Pts',(-19.1741877112253,-21.9469162432243,
-1.65187093097051));
#64857=CARTESIAN_POINT('Ctrl Pts',(-21.0477247446925,-20.5363391578402,
-1.75473569408639));
#64858=CARTESIAN_POINT('Ctrl Pts',(-21.2914430930582,-19.3178333754147,
-1.81520852164178));
#64859=CARTESIAN_POINT('Ctrl Pts',(-21.2901593318677,-18.9530194399495,
-1.8332894136367));
#64860=CARTESIAN_POINT('Ctrl Pts',(-21.293999801981,-18.9530069047618,-1.83329010977149));
#64861=CARTESIAN_POINT('Ctrl Pts',(-21.2940336318731,-18.8669962707737,
-1.83754657623943));
#64862=CARTESIAN_POINT('Ctrl Pts',(-21.2897284501564,-18.7810104793984,
-1.84180304270736));
#64863=CARTESIAN_POINT('Ctrl Pts',(-21.2811180404876,-18.6955049945465,
-1.8460595091753));
#64864=CARTESIAN_POINT('Ctrl Pts',(-21.272502628509,-18.6099498343665,-1.85031844848306));
#64865=CARTESIAN_POINT('Ctrl Pts',(-21.2595770560965,-18.5248759662227,
-1.85457738779083));
#64866=CARTESIAN_POINT('Ctrl Pts',(-21.2424267247842,-18.4407316102198,
-1.8588363270986));
#64867=CARTESIAN_POINT('Ctrl Pts',(-21.2252479656664,-18.3564477793963,
-1.8631023258792));
#64868=CARTESIAN_POINT('Ctrl Pts',(-21.2038305496871,-18.273096962458,-1.8673683246598));
#64869=CARTESIAN_POINT('Ctrl Pts',(-21.1783105998859,-18.191115191842,-1.87163432344041));
#64870=CARTESIAN_POINT('Ctrl Pts',(-21.1527682035212,-18.1090613125802,
-1.87590407446243));
#64871=CARTESIAN_POINT('Ctrl Pts',(-21.1231162337396,-18.0283792845701,
-1.88017382548446));
#64872=CARTESIAN_POINT('Ctrl Pts',(-21.0895392521437,-17.949485744934,-1.88444357650648));
#64873=CARTESIAN_POINT('Ctrl Pts',(-21.0558918636089,-17.8704267749242,
-1.88872228068881));
#64874=CARTESIAN_POINT('Ctrl Pts',(-21.0183032087881,-17.7931641756621,
-1.89300098487114));
#64875=CARTESIAN_POINT('Ctrl Pts',(-20.9770042486984,-17.7180907892714,
-1.89727968905346));
#64876=CARTESIAN_POINT('Ctrl Pts',(-20.9482314701846,-17.6657875372232,
-1.90026064081344));
#64877=CARTESIAN_POINT('Ctrl Pts',(-20.917658721245,-17.614546342522,-1.90324159257341));
#64878=CARTESIAN_POINT('Ctrl Pts',(-20.8853760799725,-17.5644910946152,
-1.90622254433338));
#64879=CARTESIAN_POINT('Ctrl Pts',(-20.8400579766697,-17.4942239539453,
-1.91040717961954));
#64880=CARTESIAN_POINT('Ctrl Pts',(-20.7912093745918,-17.4260486192458,
-1.9145918149057));
#64881=CARTESIAN_POINT('Ctrl Pts',(-20.7390496453448,-17.3603417704474,
-1.91877645019186));
#64882=CARTESIAN_POINT('Ctrl Pts',(-20.6869641588708,-17.294728447032,-1.92295512917932));
#64883=CARTESIAN_POINT('Ctrl Pts',(-20.6315771902452,-17.2315769876738,
-1.92713380816678));
#64884=CARTESIAN_POINT('Ctrl Pts',(-20.5731519433967,-17.1712360827161,
-1.93131248715424));
#64885=CARTESIAN_POINT('Ctrl Pts',(-20.513679481987,-17.1098136269271,-1.9355660648151));
#64886=CARTESIAN_POINT('Ctrl Pts',(-20.4510590117389,-17.05130387858,-1.93981964247596));
#64887=CARTESIAN_POINT('Ctrl Pts',(-20.3856118360818,-16.9960403013062,
-1.94407322013681));
#64888=CARTESIAN_POINT('Ctrl Pts',(-20.321433464053,-16.94184810147,-1.94824433503721));
#64889=CARTESIAN_POINT('Ctrl Pts',(-20.2545373771257,-16.8907776413735,
-1.9524154499376));
#64890=CARTESIAN_POINT('Ctrl Pts',(-20.1852631886002,-16.8431057026456,
-1.95658656483799));
#64891=CARTESIAN_POINT('Ctrl Pts',(-20.1160122456088,-16.7954497606359,
-1.96075628008585));
#64892=CARTESIAN_POINT('Ctrl Pts',(-20.0443851644975,-16.751190335713,-1.96492599533372));
#64893=CARTESIAN_POINT('Ctrl Pts',(-19.9707522609747,-16.7105621032529,
-1.96909571058158));
#64894=CARTESIAN_POINT('Ctrl Pts',(-19.8971219775585,-16.6699353164821,
-1.97326527745694));
#64895=CARTESIAN_POINT('Ctrl Pts',(-19.8214864168391,-16.6329396867698,
-1.9774348443323));
#64896=CARTESIAN_POINT('Ctrl Pts',(-19.7442411213498,-16.5997642812138,
-1.98160441120766));
#64897=CARTESIAN_POINT('Ctrl Pts',(-19.6642800145859,-16.5654224856546,
-1.98592057285825));
#64898=CARTESIAN_POINT('Ctrl Pts',(-19.5825943566344,-16.5351747549186,
-1.99023673450885));
#64899=CARTESIAN_POINT('Ctrl Pts',(-19.4996442818956,-16.5091760534986,
-1.99455289615945));
#64900=CARTESIAN_POINT('Ctrl Pts',(-19.4193962589829,-16.4840242450908,
-1.99872846128247));
#64901=CARTESIAN_POINT('Ctrl Pts',(-19.3379653976298,-16.462848969509,-2.0029040264055));
#64902=CARTESIAN_POINT('Ctrl Pts',(-19.2557808529988,-16.4457388920059,
-2.00707959152852));
#64903=CARTESIAN_POINT('Ctrl Pts',(-19.169445422947,-16.4277646377701,-2.01146605144291));
#64904=CARTESIAN_POINT('Ctrl Pts',(-19.082278749795,-16.414277123413,-2.01585251135729));
#64905=CARTESIAN_POINT('Ctrl Pts',(-18.9947846786654,-16.4053175794039,
-2.02023897127167));
#64906=CARTESIAN_POINT('Ctrl Pts',(-18.9072906075359,-16.3963580353947,
-2.02462543118606));
#64907=CARTESIAN_POINT('Ctrl Pts',(-18.8194697217397,-16.3919264150073,
-2.02901189110044));
#64908=CARTESIAN_POINT('Ctrl Pts',(-18.7318236815548,-16.3920009250709,
-2.03339835101482));
#64909=CARTESIAN_POINT('Ctrl Pts',(-18.6482254298241,-16.3920719940095,
-2.03758222948047));
#64910=CARTESIAN_POINT('Ctrl Pts',(-18.5644751184203,-16.3962424237152,
-2.04176610794612));
#64911=CARTESIAN_POINT('Ctrl Pts',(-18.481007980681,-16.4045316413818,-2.04594998641176));
#64912=CARTESIAN_POINT('Ctrl Pts',(-18.3976520608444,-16.4128098138703,
-2.05012828996254));
#64913=CARTESIAN_POINT('Ctrl Pts',(-18.3145790190413,-16.4251958328771,
-2.05430659351331));
#64914=CARTESIAN_POINT('Ctrl Pts',(-18.2322243990186,-16.4416571456752,
-2.05848489706408));
#64915=CARTESIAN_POINT('Ctrl Pts',(-18.1499547982016,-16.4581014645543,
-2.06265888712218));
#64916=CARTESIAN_POINT('Ctrl Pts',(-18.0684025947205,-16.478612631518,-2.06683287718028));
#64917=CARTESIAN_POINT('Ctrl Pts',(-17.987997155221,-16.5031064221609,-2.07100686723839));
#64918=CARTESIAN_POINT('Ctrl Pts',(-17.9076457851775,-16.527583741705,-2.0751780504544));
#64919=CARTESIAN_POINT('Ctrl Pts',(-17.8284400864782,-16.5560382324587,
-2.07934923367041));
#64920=CARTESIAN_POINT('Ctrl Pts',(-17.7507969267065,-16.5883351090592,
-2.08352041688642));
#64921=CARTESIAN_POINT('Ctrl Pts',(-17.6731854101898,-16.620618823157,-2.08768990014826));
#64922=CARTESIAN_POINT('Ctrl Pts',(-17.5971355906324,-16.6567416327186,
-2.09185938341009));
#64923=CARTESIAN_POINT('Ctrl Pts',(-17.5230455881934,-16.6965201369717,
-2.09602886667192));
#64924=CARTESIAN_POINT('Ctrl Pts',(-17.448941785493,-16.7363060505073,-2.10019912655621));
#64925=CARTESIAN_POINT('Ctrl Pts',(-17.3767989370841,-16.7797488058129,
-2.10436938644049));
#64926=CARTESIAN_POINT('Ctrl Pts',(-17.3069908375485,-16.8266188929325,
-2.10853964632478));
#64927=CARTESIAN_POINT('Ctrl Pts',(-17.2618060573289,-16.8569565557462,
-2.11123893591414));
#64928=CARTESIAN_POINT('Ctrl Pts',(-17.217598927097,-16.8887292038021,-2.11393822550351));
#64929=CARTESIAN_POINT('Ctrl Pts',(-17.1744641548914,-16.9218650419685,
-2.11663751509287));
#64930=CARTESIAN_POINT('',(-21.2939995273704,-18.9504444089713,-1.76670989019937));
#64931=CARTESIAN_POINT('Ctrl Pts',(-21.29399952737,-18.9504444083884,-1.7667098902285));
#64932=CARTESIAN_POINT('Ctrl Pts',(-21.2939437779003,-18.8586988530854,
-1.77129369133236));
#64933=CARTESIAN_POINT('Ctrl Pts',(-21.2889563823031,-18.7671041917188,
-1.77587749243622));
#64934=CARTESIAN_POINT('Ctrl Pts',(-21.2790836671927,-18.6760486872856,
-1.78046129354008));
#64935=CARTESIAN_POINT('Ctrl Pts',(-21.2700706759119,-18.5929223680962,
-1.78464593362342));
#64936=CARTESIAN_POINT('Ctrl Pts',(-21.2569640808322,-18.5100833893621,
-1.78883057370677));
#64937=CARTESIAN_POINT('Ctrl Pts',(-21.2397911341478,-18.4279668025532,
-1.79301521379011));
#64938=CARTESIAN_POINT('Ctrl Pts',(-21.2226426307479,-18.3459670972049,
-1.79719389762437));
#64939=CARTESIAN_POINT('Ctrl Pts',(-21.2014393656626,-18.2646881878446,
-1.80137258145863));
#64940=CARTESIAN_POINT('Ctrl Pts',(-21.1762603194833,-18.1845597535461,
-1.80555126529289));
#64941=CARTESIAN_POINT('Ctrl Pts',(-21.1506300008844,-18.1029952143143,
-1.80980484174825));
#64942=CARTESIAN_POINT('Ctrl Pts',(-21.1208800336003,-18.0226232755941,
-1.81405841820361));
#64943=CARTESIAN_POINT('Ctrl Pts',(-21.0871481586077,-17.9438860463016,
-1.81831199465897));
#64944=CARTESIAN_POINT('Ctrl Pts',(-21.0540701842775,-17.866675157493,-1.82248311449243));
#64945=CARTESIAN_POINT('Ctrl Pts',(-21.0171634947162,-17.7910366074843,
-1.82665423432589));
#64946=CARTESIAN_POINT('Ctrl Pts',(-20.9766076064455,-17.7173700459194,
-1.83082535415935));
#64947=CARTESIAN_POINT('Ctrl Pts',(-20.9360653268187,-17.6437282033794,
-1.83499507436165));
#64948=CARTESIAN_POINT('Ctrl Pts',(-20.8918765020354,-17.5720574377846,
-1.83916479456395));
#64949=CARTESIAN_POINT('Ctrl Pts',(-20.8442669678557,-17.5027335219578,
-1.84333451476625));
#64950=CARTESIAN_POINT('Ctrl Pts',(-20.7966591276122,-17.4334120726597,
-1.84750408661088));
#64951=CARTESIAN_POINT('Ctrl Pts',(-20.7456310810944,-17.3664376858416,
-1.8516736584555));
#64952=CARTESIAN_POINT('Ctrl Pts',(-20.6914516584179,-17.3021566726028,
-1.85584323030013));
#64953=CARTESIAN_POINT('Ctrl Pts',(-20.6353675232618,-17.2356158189659,
-1.86015938612691));
#64954=CARTESIAN_POINT('Ctrl Pts',(-20.5759066443104,-17.1719616467127,
-1.8644755419537));
#64955=CARTESIAN_POINT('Ctrl Pts',(-20.5134108747745,-17.111538933111,-1.86879169778048));
#64956=CARTESIAN_POINT('Ctrl Pts',(-20.4529507162969,-17.0530843070278,
-1.87296726785888));
#64957=CARTESIAN_POINT('Ctrl Pts',(-20.3896507223166,-16.9976541361553,
-1.87714283793729));
#64958=CARTESIAN_POINT('Ctrl Pts',(-20.3238547745764,-16.9455200485037,
-1.88131840801569));
#64959=CARTESIAN_POINT('Ctrl Pts',(-20.2547359371302,-16.8907530354344,
-1.88570485671667));
#64960=CARTESIAN_POINT('Ctrl Pts',(-20.182862878563,-16.8396241326094,-1.89009130541764));
#64961=CARTESIAN_POINT('Ctrl Pts',(-20.1086675044515,-16.7923960427418,
-1.89447775411861));
#64962=CARTESIAN_POINT('Ctrl Pts',(-20.03447213034,-16.7451679528743,-1.89886420281958));
#64963=CARTESIAN_POINT('Ctrl Pts',(-19.9579549830438,-16.7018408956605,
-1.90325065152055));
#64964=CARTESIAN_POINT('Ctrl Pts',(-19.8795742651273,-16.6626202580004,
-1.90763710022152));
#64965=CARTESIAN_POINT('Ctrl Pts',(-19.8047997208725,-16.6252041002467,
-1.91182173531074));
#64966=CARTESIAN_POINT('Ctrl Pts',(-19.7280509965214,-16.5913855369158,
-1.91600637039996));
#64967=CARTESIAN_POINT('Ctrl Pts',(-19.649708651428,-16.5613771385474,-1.92019100548918));
#64968=CARTESIAN_POINT('Ctrl Pts',(-19.5714778164139,-16.5314114532082,
-1.92436968429779));
#64969=CARTESIAN_POINT('Ctrl Pts',(-19.4916582921575,-16.5052453236535,
-1.9285483631064));
#64970=CARTESIAN_POINT('Ctrl Pts',(-19.4106541203679,-16.4830449170977,
-1.93272704191501));
#64971=CARTESIAN_POINT('Ctrl Pts',(-19.3281980247581,-16.4604465890721,
-1.93698061962285));
#64972=CARTESIAN_POINT('Ctrl Pts',(-19.2445148259725,-16.4419577675855,
-1.94123419733068));
#64973=CARTESIAN_POINT('Ctrl Pts',(-19.1600508251799,-16.4277019402686,
-1.94548777503851));
#64974=CARTESIAN_POINT('Ctrl Pts',(-19.0772243047194,-16.4137224867517,
-1.94965888980624));
#64975=CARTESIAN_POINT('Ctrl Pts',(-18.9936474609865,-16.4038134443357,
-1.95383000457398));
#64976=CARTESIAN_POINT('Ctrl Pts',(-18.9097535040447,-16.3980401910335,
-1.95800111934171));
#64977=CARTESIAN_POINT('Ctrl Pts',(-18.8258876980693,-16.3922688749706,
-1.96217083447453));
#64978=CARTESIAN_POINT('Ctrl Pts',(-18.7417054487798,-16.3906306234225,
-1.96634054960734));
#64979=CARTESIAN_POINT('Ctrl Pts',(-18.6576449613786,-16.3931389431864,
-1.97051026474016));
#64980=CARTESIAN_POINT('Ctrl Pts',(-18.5735874647729,-16.3956471737067,
-1.97467983151832));
#64981=CARTESIAN_POINT('Ctrl Pts',(-18.4896521812446,-16.4023016676361,
-1.97884939829647));
#64982=CARTESIAN_POINT('Ctrl Pts',(-18.4062758154027,-16.4130638332502,
-1.98301896507463));
#64983=CARTESIAN_POINT('Ctrl Pts',(-18.319968075054,-16.4242043787278,-1.98733512689366));
#64984=CARTESIAN_POINT('Ctrl Pts',(-18.2342598093425,-16.439746750557,-1.99165128871268));
#64985=CARTESIAN_POINT('Ctrl Pts',(-18.1496259627856,-16.4595901250738,
-1.99596745053171));
#64986=CARTESIAN_POINT('Ctrl Pts',(-18.0677490201717,-16.4787871118902,
-2.00014301560344));
#64987=CARTESIAN_POINT('Ctrl Pts',(-17.9868780138239,-16.502009022233,-2.00431858067517));
#64988=CARTESIAN_POINT('Ctrl Pts',(-17.9074274756713,-16.5291137331635,
-2.0084941457469));
#64989=CARTESIAN_POINT('Ctrl Pts',(-17.8239641319307,-16.5575874207934,
-2.01288060593957));
#64990=CARTESIAN_POINT('Ctrl Pts',(-17.742069063372,-16.590346235575,-2.01726706613225));
#64991=CARTESIAN_POINT('Ctrl Pts',(-17.662196947742,-16.6271692067657,-2.02165352632493));
#64992=CARTESIAN_POINT('Ctrl Pts',(-17.5823248321119,-16.6639921779564,
-2.0260399865176));
#64993=CARTESIAN_POINT('Ctrl Pts',(-17.504476147719,-16.7048789684268,-2.03042644671028));
#64994=CARTESIAN_POINT('Ctrl Pts',(-17.4290716122241,-16.7495554711238,
-2.03481290690295));
#64995=CARTESIAN_POINT('Ctrl Pts',(-17.3571349233601,-16.792177306176,-2.03899763425421));
#64996=CARTESIAN_POINT('Ctrl Pts',(-17.2871547394863,-16.8384065836607,
-2.04318236160547));
#64997=CARTESIAN_POINT('Ctrl Pts',(-17.2195158141186,-16.8880383601638,
-2.04736708895673));
#64998=CARTESIAN_POINT('Ctrl Pts',(-17.2043800615047,-16.8991446024179,
-2.04830351716876));
#64999=CARTESIAN_POINT('Ctrl Pts',(-17.1893614580268,-16.9104210351831,
-2.04923994538079));
#65000=CARTESIAN_POINT('Ctrl Pts',(-17.1744641548914,-16.9218650419685,
-2.05017637359282));
#65001=CARTESIAN_POINT('Ctrl Pts',(-17.1744641548914,-16.9218650419685,
-1.2500388607805));
#65002=CARTESIAN_POINT('Ctrl Pts',(-17.1078165570043,-16.9730632726498,
-1.25422272801441));
#65003=CARTESIAN_POINT('Ctrl Pts',(-17.0437742835163,-17.0274842711545,
-1.25840659524833));
#65004=CARTESIAN_POINT('Ctrl Pts',(-16.9826475255332,-17.0848191008424,
-1.26259046248224));
#65005=CARTESIAN_POINT('Ctrl Pts',(-16.9380009581382,-17.1266960696561,
-1.26564633059294));
#65006=CARTESIAN_POINT('Ctrl Pts',(-16.8949089970119,-17.1701266834957,
-1.26870219870364));
#65007=CARTESIAN_POINT('Ctrl Pts',(-16.8534788456906,-17.2149795084125,
-1.27175806681434));
#65008=CARTESIAN_POINT('Ctrl Pts',(-16.7967468035303,-17.2763983609397,
-1.2759425950616));
#65009=CARTESIAN_POINT('Ctrl Pts',(-16.7429212561054,-17.3407138418484,
-1.28012712330885));
#65010=CARTESIAN_POINT('Ctrl Pts',(-16.6923122163234,-17.4076195436403,
-1.28431165155611));
#65011=CARTESIAN_POINT('Ctrl Pts',(-16.6417752336977,-17.4744299850868,
-1.2884902218716));
#65012=CARTESIAN_POINT('Ctrl Pts',(-16.5944459372434,-17.5438229582135,
-1.29266879218709));
#65013=CARTESIAN_POINT('Ctrl Pts',(-16.5505962988509,-17.6154565933691,
-1.29684736250257));
#65014=CARTESIAN_POINT('Ctrl Pts',(-16.5059592554184,-17.6883765489466,
-1.30110096712729));
#65015=CARTESIAN_POINT('Ctrl Pts',(-16.4649284015663,-17.7636180793202,
-1.30535457175201));
#65016=CARTESIAN_POINT('Ctrl Pts',(-16.4277464893493,-17.8407868140581,
-1.30960817637672));
#65017=CARTESIAN_POINT('Ctrl Pts',(-16.3912866203068,-17.9164569933188,
-1.31377917938137));
#65018=CARTESIAN_POINT('Ctrl Pts',(-16.3585277513987,-17.9939797629346,
-1.31795018238602));
#65019=CARTESIAN_POINT('Ctrl Pts',(-16.3296531528721,-18.0729572031431,
-1.32212118539066));
#65020=CARTESIAN_POINT('Ctrl Pts',(-16.3007882503651,-18.1519081229202,
-1.32629078778269));
#65021=CARTESIAN_POINT('Ctrl Pts',(-16.2758051856693,-18.2323123114455,
-1.33046039017473));
#65022=CARTESIAN_POINT('Ctrl Pts',(-16.2548387934267,-18.3137526249001,
-1.33462999256676));
#65023=CARTESIAN_POINT('Ctrl Pts',(-16.2338731513477,-18.3951900244743,
-1.33879944577318));
#65024=CARTESIAN_POINT('Ctrl Pts',(-16.2169240098583,-18.477663029525,-1.3429688989796));
#65025=CARTESIAN_POINT('Ctrl Pts',(-16.2040757430117,-18.5607414487807,
-1.34713835218602));
#65026=CARTESIAN_POINT('Ctrl Pts',(-16.1907749845688,-18.6467457324343,
-1.3514546456285));
#65027=CARTESIAN_POINT('Ctrl Pts',(-16.181869424783,-18.7333983482173,-1.35577093907098));
#65028=CARTESIAN_POINT('Ctrl Pts',(-16.1773942991259,-18.8202149846984,
-1.36008723251346));
#65029=CARTESIAN_POINT('Ctrl Pts',(-16.1730651991088,-18.90419874991,-1.36426268309241));
#65030=CARTESIAN_POINT('Ctrl Pts',(-16.1728817996142,-18.9883355251162,
-1.36843813367136));
#65031=CARTESIAN_POINT('Ctrl Pts',(-16.1768228581885,-19.0721876258056,
-1.37261358425031));
#65032=CARTESIAN_POINT('Ctrl Pts',(-16.1809633215807,-19.1602823716003,
-1.37700029912456));
#65033=CARTESIAN_POINT('Ctrl Pts',(-16.1896565615449,-19.2480622945844,
-1.3813870139988));
#65034=CARTESIAN_POINT('Ctrl Pts',(-16.2028167371298,-19.3350290978058,
-1.38577372887305));
#65035=CARTESIAN_POINT('Ctrl Pts',(-16.2159769127148,-19.4219959010273,
-1.39016044374729));
#65036=CARTESIAN_POINT('Ctrl Pts',(-16.2336038329925,-19.5081490310293,
-1.39454715862153));
#65037=CARTESIAN_POINT('Ctrl Pts',(-16.2555511525982,-19.593008042705,-1.39893387349578));
#65038=CARTESIAN_POINT('Ctrl Pts',(-16.276487610888,-19.6739585729016,-1.40311854272393));
#65039=CARTESIAN_POINT('Ctrl Pts',(-16.3014331778146,-19.7540329167562,
-1.40730321195209));
#65040=CARTESIAN_POINT('Ctrl Pts',(-16.3302979840591,-19.8328045291445,
-1.41148788118024));
#65041=CARTESIAN_POINT('Ctrl Pts',(-16.3591217073558,-19.9114640268001,
-1.41566659441667));
#65042=CARTESIAN_POINT('Ctrl Pts',(-16.3918534329631,-19.988824047698,-1.4198453076531));
#65043=CARTESIAN_POINT('Ctrl Pts',(-16.4283528834957,-20.064470841935,-1.42402402088953));
#65044=CARTESIAN_POINT('Ctrl Pts',(-16.4655061714862,-20.1414727444521,
-1.42827759002651));
#65045=CARTESIAN_POINT('Ctrl Pts',(-16.506563383349,-20.2166989674673,-1.4325311591635));
#65046=CARTESIAN_POINT('Ctrl Pts',(-16.551324307012,-20.2897319683851,-1.43678472830049));
#65047=CARTESIAN_POINT('Ctrl Pts',(-16.595217918491,-20.3613498418582,-1.4409558779511));
#65048=CARTESIAN_POINT('Ctrl Pts',(-16.642672740131,-20.430858319068,-1.44512702760171));
#65049=CARTESIAN_POINT('Ctrl Pts',(-16.6934533571751,-20.4978878997056,
-1.44929817725232));
#65050=CARTESIAN_POINT('Ctrl Pts',(-16.7442169358474,-20.564894989972,-1.45346792736108));
#65051=CARTESIAN_POINT('Ctrl Pts',(-16.7983038161653,-20.6294244691448,
-1.45763767746983));
#65052=CARTESIAN_POINT('Ctrl Pts',(-16.8554362029378,-20.6911371597339,
-1.46180742757859));
#65053=CARTESIAN_POINT('Ctrl Pts',(-16.9125665576473,-20.7528476553495,
-1.46597702937926));
#65054=CARTESIAN_POINT('Ctrl Pts',(-16.9727418902975,-20.8117412245847,
-1.47014663117994));
#65055=CARTESIAN_POINT('Ctrl Pts',(-17.0356461226138,-20.8675140582014,
-1.47431623298061));
#65056=CARTESIAN_POINT('Ctrl Pts',(-17.100760794443,-20.9252467357051,-1.47863235358033));
#65057=CARTESIAN_POINT('Ctrl Pts',(-17.1687993304482,-20.9796349174704,
-1.48294847418005));
#65058=CARTESIAN_POINT('Ctrl Pts',(-17.2393736359262,-21.0303868821313,
-1.48726459477976));
#65059=CARTESIAN_POINT('Ctrl Pts',(-17.3076502404839,-21.0794865055453,
-1.49144019463036));
#65060=CARTESIAN_POINT('Ctrl Pts',(-17.3782996119825,-21.1251828324923,
-1.49561579448095));
#65061=CARTESIAN_POINT('Ctrl Pts',(-17.4509422068433,-21.1672568021383,
-1.49979139433154));
#65062=CARTESIAN_POINT('Ctrl Pts',(-17.5272517449746,-21.2114546339639,
-1.50417777530582));
#65063=CARTESIAN_POINT('Ctrl Pts',(-17.6057605149863,-21.2516545112966,
-1.5085641562801));
#65064=CARTESIAN_POINT('Ctrl Pts',(-17.6860031954809,-21.2876589429362,
-1.51295053725438));
#65065=CARTESIAN_POINT('Ctrl Pts',(-17.7662458759755,-21.3236633745758,
-1.51733691822866));
#65066=CARTESIAN_POINT('Ctrl Pts',(-17.8482218986034,-21.3554722215575,
-1.52172329920294));
#65067=CARTESIAN_POINT('Ctrl Pts',(-17.9314482087024,-21.3829485025983,
-1.52610968017722));
#65068=CARTESIAN_POINT('Ctrl Pts',(-18.01084679095,-21.4091611000027,-1.53029432359276));
#65069=CARTESIAN_POINT('Ctrl Pts',(-18.0916786888191,-21.4315284615327,
-1.53447896700831));
#65070=CARTESIAN_POINT('Ctrl Pts',(-18.1735366063454,-21.4498952708977,
-1.53866361042385));
#65071=CARTESIAN_POINT('Ctrl Pts',(-18.2552780145749,-21.4682359385759,
-1.54284229778925));
#65072=CARTESIAN_POINT('Ctrl Pts',(-18.3380420967243,-21.4825872643746,
-1.54702098515466));
#65073=CARTESIAN_POINT('Ctrl Pts',(-18.4214050302511,-21.4928432428797,
-1.55119967252006));
#65074=CARTESIAN_POINT('Ctrl Pts',(-18.5062619503251,-21.5032830236249,
-1.5554532481175));
#65075=CARTESIAN_POINT('Ctrl Pts',(-18.5917389405056,-21.5094790670787,
-1.55970682371494));
#65076=CARTESIAN_POINT('Ctrl Pts',(-18.6773765369535,-21.5113737092173,
-1.56396039931238));
#65077=CARTESIAN_POINT('Ctrl Pts',(-18.7613541250249,-21.513231625409,-1.56813152314313));
#65078=CARTESIAN_POINT('Ctrl Pts',(-18.8454856674055,-21.510953399411,-1.57230264697389));
#65079=CARTESIAN_POINT('Ctrl Pts',(-18.9293330517837,-21.5045369730683,
-1.57647377080464));
#65080=CARTESIAN_POINT('Ctrl Pts',(-19.0131523042948,-21.4981226995185,
-1.58064349517013));
#65081=CARTESIAN_POINT('Ctrl Pts',(-19.0966871298398,-21.4875730181186,
-1.58481321953563));
#65082=CARTESIAN_POINT('Ctrl Pts',(-19.179501972955,-21.4729379191272,-1.58898294390113));
#65083=CARTESIAN_POINT('Ctrl Pts',(-19.2623138727389,-21.4583033402833,
-1.59315252007));
#65084=CARTESIAN_POINT('Ctrl Pts',(-19.3444053881076,-21.4395837134394,
-1.59732209623888));
#65085=CARTESIAN_POINT('Ctrl Pts',(-19.4253499807632,-21.4168803630397,
-1.60149167240775));
#65086=CARTESIAN_POINT('Ctrl Pts',(-19.5091400560411,-21.3933789112856,
-1.60580782361199));
#65087=CARTESIAN_POINT('Ctrl Pts',(-19.5917005611986,-21.3656085745896,
-1.61012397481624));
#65088=CARTESIAN_POINT('Ctrl Pts',(-19.6725761234496,-21.3337377816398,
-1.61444012602048));
#65089=CARTESIAN_POINT('Ctrl Pts',(-19.7508175799528,-21.3029050159575,
-1.61861570078383));
#65090=CARTESIAN_POINT('Ctrl Pts',(-19.8274817556368,-21.2682350333859,
-1.62279127554719));
#65091=CARTESIAN_POINT('Ctrl Pts',(-19.9021790201189,-21.2299283959234,
-1.62696685031055));
#65092=CARTESIAN_POINT('Ctrl Pts',(-19.9806484631081,-21.1896872903713,
-1.63135328973523));
#65093=CARTESIAN_POINT('Ctrl Pts',(-20.0569466040008,-21.1454328549357,
-1.63573972915991));
#65094=CARTESIAN_POINT('Ctrl Pts',(-20.1306554964563,-21.0974494690434,
-1.6401261685846));
#65095=CARTESIAN_POINT('Ctrl Pts',(-20.2043643889117,-21.049466083151,-1.64451260800928));
#65096=CARTESIAN_POINT('Ctrl Pts',(-20.2754836084046,-20.9977541495255,
-1.64889904743396));
#65097=CARTESIAN_POINT('Ctrl Pts',(-20.34363649293,-20.9426457144927,-1.65328548685865));
#65098=CARTESIAN_POINT('Ctrl Pts',(-20.4078056269716,-20.8907585408379,
-1.65741552510087));
#65099=CARTESIAN_POINT('Ctrl Pts',(-20.469597781961,-20.8356563927705,-1.6615455633431));
#65100=CARTESIAN_POINT('Ctrl Pts',(-20.5286666481821,-20.7775880208587,
-1.66567560158532));
#65101=CARTESIAN_POINT('Ctrl Pts',(-20.5888757444006,-20.7183987318922,
-1.66988536361091));
#65102=CARTESIAN_POINT('Ctrl Pts',(-20.6462548721938,-20.6561277358796,
-1.67409512563649));
#65103=CARTESIAN_POINT('Ctrl Pts',(-20.70047016696,-20.5910836105752,-1.67830488766208));
#65104=CARTESIAN_POINT('Ctrl Pts',(-20.7535207637169,-20.5274368172154,
-1.68242421208196));
#65105=CARTESIAN_POINT('Ctrl Pts',(-20.8035417749399,-20.4611352293305,
-1.68654353650185));
#65106=CARTESIAN_POINT('Ctrl Pts',(-20.8502568537434,-20.3925057892921,
-1.69066286092173));
#65107=CARTESIAN_POINT('Ctrl Pts',(-20.8969436352055,-20.3239179210705,
-1.69477969008884));
#65108=CARTESIAN_POINT('Ctrl Pts',(-20.940328192166,-20.2530053887166,-1.69889651925596));
#65109=CARTESIAN_POINT('Ctrl Pts',(-20.9801755792367,-20.1801267309364,
-1.70301334842307));
#65110=CARTESIAN_POINT('Ctrl Pts',(-21.0200115219931,-20.1072690041715,
-1.70712899522189));
#65111=CARTESIAN_POINT('Ctrl Pts',(-21.0563120854056,-20.0324466882332,
-1.71124464202071));
#65112=CARTESIAN_POINT('Ctrl Pts',(-21.0888874490411,-19.9560443726991,
-1.71536028881953));
#65113=CARTESIAN_POINT('Ctrl Pts',(-21.122756810271,-19.8766071129166,-1.71963942226786));
#65114=CARTESIAN_POINT('Ctrl Pts',(-21.1525985823987,-19.7954621912662,
-1.72391855571618));
#65115=CARTESIAN_POINT('Ctrl Pts',(-21.1782545829907,-19.7130647367531,
-1.7281976891645));
#65116=CARTESIAN_POINT('Ctrl Pts',(-21.2029529666689,-19.6337427887209,
-1.73231710284076));
#65117=CARTESIAN_POINT('Ctrl Pts',(-21.2237724306601,-19.5532606399815,
-1.73643651651702));
#65118=CARTESIAN_POINT('Ctrl Pts',(-21.2406233757609,-19.4720377410235,
-1.74055593019328));
#65119=CARTESIAN_POINT('Ctrl Pts',(-21.257483616485,-19.3907700364207,-1.74467761629503));
#65120=CARTESIAN_POINT('Ctrl Pts',(-21.2703709111432,-19.3087612356736,
-1.74879930239678));
#65121=CARTESIAN_POINT('Ctrl Pts',(-21.2792473404998,-19.2264375624415,
-1.75292098849853));
#65122=CARTESIAN_POINT('Ctrl Pts',(-21.2881358445687,-19.1440019033387,
-1.75704828137884));
#65123=CARTESIAN_POINT('Ctrl Pts',(-21.2930025792327,-19.061250988371,-1.76117557425916));
#65124=CARTESIAN_POINT('Ctrl Pts',(-21.2938616786583,-18.9786117668865,
-1.76530286713947));
#65125=CARTESIAN_POINT('Ctrl Pts',(-21.293959302996,-18.969221003687,-1.76577187482611));
#65126=CARTESIAN_POINT('Ctrl Pts',(-21.2940052315708,-18.95983167724,-1.76624088251274));
#65127=CARTESIAN_POINT('Ctrl Pts',(-21.2939995273704,-18.9504444089713,
-1.76670989019937));
#65128=CARTESIAN_POINT('Origin',(-18.734,-18.952,1.76670989022851));
#65129=CARTESIAN_POINT('',(-17.1769962711794,-16.9251779373085,-0.450077505597091));
#65130=CARTESIAN_POINT('',(-17.1722616763361,-16.9190322283098,-0.516748667021866));
#65131=CARTESIAN_POINT('',(-17.1744641548914,-16.9218650419685,1.76670989022851));
#65132=CARTESIAN_POINT('',(-21.2914666238416,-18.9551442278135,-0.166709890228505));
#65133=CARTESIAN_POINT('Ctrl Pts',(-21.2914666238416,-18.9551442278135,
-0.166709890228505));
#65134=CARTESIAN_POINT('Ctrl Pts',(-21.2869488473544,-18.3666789556461,
-0.195923797939959));
#65135=CARTESIAN_POINT('Ctrl Pts',(-20.7940986851072,-16.9152596074165,
-0.267529641211892));
#65136=CARTESIAN_POINT('Ctrl Pts',(-18.7954429923518,-16.112385634392,-0.361985513001419));
#65137=CARTESIAN_POINT('Ctrl Pts',(-17.5432453230646,-16.6451528738997,
-0.427227477079495));
#65138=CARTESIAN_POINT('Ctrl Pts',(-17.1769962711794,-16.9251779373085,
-0.450077505597091));
#65139=CARTESIAN_POINT('',(-19.3957372685685,-21.4249949024184,0.));
#65140=CARTESIAN_POINT('Ctrl Pts',(-19.3957372685684,-21.4249949024184,
8.32667268468867E-16));
#65141=CARTESIAN_POINT('Ctrl Pts',(-20.2191097516036,-21.2046724677036,
-0.0423919355604773));
#65142=CARTESIAN_POINT('Ctrl Pts',(-21.1334435320312,-20.3367930039316,
-0.0979618989699793));
#65143=CARTESIAN_POINT('Ctrl Pts',(-21.2935045362274,-19.2205935412502,
-0.153531862379481));
#65144=CARTESIAN_POINT('Ctrl Pts',(-21.2914666238416,-18.9551442278135,
-0.166709890228505));
#65145=CARTESIAN_POINT('',(-18.0722323438033,-21.4249867709335,-1.75387482315159E-11));
#65146=CARTESIAN_POINT('Origin',(-18.734,-18.952,0.));
#65147=CARTESIAN_POINT('',(-21.2939992553243,-18.9500473764188,-0.233290109771496));
#65148=CARTESIAN_POINT('Ctrl Pts',(-18.0722323438033,-21.4249867709335,
-1.75386372092134E-11));
#65149=CARTESIAN_POINT('Ctrl Pts',(-18.1529469590682,-21.4465858843588,
-0.0041815927697939));
#65150=CARTESIAN_POINT('Ctrl Pts',(-18.2348713083479,-21.4642696834585,
-0.00836318552204911));
#65151=CARTESIAN_POINT('Ctrl Pts',(-18.3175904330397,-21.4779063863382,
-0.0125447782743044));
#65152=CARTESIAN_POINT('Ctrl Pts',(-18.400191764092,-21.4915236702881,-0.0167204163572945));
#65153=CARTESIAN_POINT('Ctrl Pts',(-18.4835851718185,-21.5011052307698,
-0.0208960544402849));
#65154=CARTESIAN_POINT('Ctrl Pts',(-18.5673419980692,-21.5065694569521,
-0.025071692523275));
#65155=CARTESIAN_POINT('Ctrl Pts',(-18.6514951828607,-21.5120595412382,
-0.0292670907845262));
#65156=CARTESIAN_POINT('Ctrl Pts',(-18.7360147805747,-21.5133930942776,
-0.0334624890457766));
#65157=CARTESIAN_POINT('Ctrl Pts',(-18.8204570723937,-21.5105396566466,
-0.0376578873070279));
#65158=CARTESIAN_POINT('Ctrl Pts',(-18.9043499961556,-21.5077047830247,
-0.0418259909775909));
#65159=CARTESIAN_POINT('Ctrl Pts',(-18.9881661507819,-21.5007372505448,
-0.0459940946481546));
#65160=CARTESIAN_POINT('Ctrl Pts',(-19.0714685200795,-21.4896593541993,
-0.0501621983187175));
#65161=CARTESIAN_POINT('Ctrl Pts',(-19.1547428065988,-21.4785851924188,
-0.0543288968439942));
#65162=CARTESIAN_POINT('Ctrl Pts',(-19.2375031954147,-21.4634034794687,
-0.0584955953692703));
#65163=CARTESIAN_POINT('Ctrl Pts',(-19.3193181247986,-21.4441883341317,
-0.0626622938945471));
#65164=CARTESIAN_POINT('Ctrl Pts',(-19.4011301114166,-21.424973879936,-0.0668288425496348));
#65165=CARTESIAN_POINT('Ctrl Pts',(-19.4819962578844,-21.4017263881227,
-0.0709953912047227));
#65166=CARTESIAN_POINT('Ctrl Pts',(-19.5614968770271,-21.3745707251823,
-0.0751619398598105));
#65167=CARTESIAN_POINT('Ctrl Pts',(-19.6419526867073,-21.347088790163,-0.0793785491042684));
#65168=CARTESIAN_POINT('Ctrl Pts',(-19.72100947348,-21.3156042817862,-0.0835951583487267));
#65169=CARTESIAN_POINT('Ctrl Pts',(-19.7982514704289,-21.280297405335,-0.0878117675931847));
#65170=CARTESIAN_POINT('Ctrl Pts',(-19.8746836538425,-21.2453606900341,
-0.0919841694456243));
#65171=CARTESIAN_POINT('Ctrl Pts',(-19.9493385364599,-21.2066816487831,
-0.096156571298064));
#65172=CARTESIAN_POINT('Ctrl Pts',(-20.0218382563896,-21.1644811017,-0.100328973150504));
#65173=CARTESIAN_POINT('Ctrl Pts',(-20.0954901988232,-21.1216098703703,
-0.104567686090971));
#65174=CARTESIAN_POINT('Ctrl Pts',(-20.1669174627926,-21.0751044941558,
-0.108806399031438));
#65175=CARTESIAN_POINT('Ctrl Pts',(-20.2357562486613,-21.0252409820392,
-0.113045111971905));
#65176=CARTESIAN_POINT('Ctrl Pts',(-20.3045950345299,-20.9753774699226,
-0.117283824912372));
#65177=CARTESIAN_POINT('Ctrl Pts',(-20.3708449996543,-20.922156180229,-0.121522537852839));
#65178=CARTESIAN_POINT('Ctrl Pts',(-20.4341804646243,-20.8658929927532,
-0.125761250793306));
#65179=CARTESIAN_POINT('Ctrl Pts',(-20.4958618762422,-20.8110991607781,
-0.129889266554068));
#65180=CARTESIAN_POINT('Ctrl Pts',(-20.5550187782048,-20.7532072778741,
-0.13401728231483));
#65181=CARTESIAN_POINT('Ctrl Pts',(-20.6113174681947,-20.6924824399031,
-0.138145298075592));
#65182=CARTESIAN_POINT('Ctrl Pts',(-20.6675250873049,-20.6318558327154,
-0.142266636202703));
#65183=CARTESIAN_POINT('Ctrl Pts',(-20.7208833621661,-20.5684057202645,
-0.146387974329814));
#65184=CARTESIAN_POINT('Ctrl Pts',(-20.7710928145058,-20.5024363466744,
-0.150509312456925));
#65185=CARTESIAN_POINT('Ctrl Pts',(-20.8212566402015,-20.4365269211813,
-0.154626905416173));
#65186=CARTESIAN_POINT('Ctrl Pts',(-20.8682770342032,-20.36810315048,-0.158744498375422));
#65187=CARTESIAN_POINT('Ctrl Pts',(-20.9118931740675,-20.2975041145794,
-0.16286209133467));
#65188=CARTESIAN_POINT('Ctrl Pts',(-20.9554836015079,-20.2269466979588,
-0.166977256905893));
#65189=CARTESIAN_POINT('Ctrl Pts',(-20.9956735091388,-20.1542169629417,
-0.171092422477116));
#65190=CARTESIAN_POINT('Ctrl Pts',(-21.0322449112854,-20.0796836115466,
-0.17520758804834));
#65191=CARTESIAN_POINT('Ctrl Pts',(-21.0688064249755,-20.0051704130511,
-0.179321640929509));
#65192=CARTESIAN_POINT('Ctrl Pts',(-21.1017511684254,-19.9288549919469,
-0.183435693810678));
#65193=CARTESIAN_POINT('Ctrl Pts',(-21.1309074516109,-19.8511299507926,
-0.187549746691848));
#65194=CARTESIAN_POINT('Ctrl Pts',(-21.1600799699193,-19.7733616299242,
-0.19166609040528));
#65195=CARTESIAN_POINT('Ctrl Pts',(-21.1854596434762,-19.6941825637462,
-0.195782434118713));
#65196=CARTESIAN_POINT('Ctrl Pts',(-21.2069235785594,-19.6140037572439,
-0.199898777832145));
#65197=CARTESIAN_POINT('Ctrl Pts',(-21.2283934303839,-19.5338028486778,
-0.204016256255548));
#65198=CARTESIAN_POINT('Ctrl Pts',(-21.245945290129,-19.452602113539,-0.20813373467895));
#65199=CARTESIAN_POINT('Ctrl Pts',(-21.25950720014,-19.3708238078727,-0.212251213102353));
#65200=CARTESIAN_POINT('Ctrl Pts',(-21.2730871839159,-19.28893651742,-0.216374178830769));
#65201=CARTESIAN_POINT('Ctrl Pts',(-21.2826665420701,-19.2064705900184,
-0.220497144559185));
#65202=CARTESIAN_POINT('Ctrl Pts',(-21.2882251767647,-19.1238538518088,
-0.224620110287602));
#65203=CARTESIAN_POINT('Ctrl Pts',(-21.2921215111921,-19.0659435088809,
-0.227510110115567));
#65204=CARTESIAN_POINT('Ctrl Pts',(-21.2940434271759,-19.0079591563185,
-0.230400109943531));
#65205=CARTESIAN_POINT('Ctrl Pts',(-21.2939992553243,-18.9500473764188,
-0.233290109771496));
#65206=CARTESIAN_POINT('Ctrl Pts',(-21.2960080607363,-18.9500458442149,
-0.233290109771496));
#65207=CARTESIAN_POINT('Ctrl Pts',(-21.2971423972504,-18.8187089636245,
-0.239839092339242));
#65208=CARTESIAN_POINT('Ctrl Pts',(-21.2281784586555,-17.8383740905167,
-0.288780010467466));
#65209=CARTESIAN_POINT('Ctrl Pts',(-19.9618261937418,-16.1848209595297,
-0.380112864156168));
#65210=CARTESIAN_POINT('Ctrl Pts',(-17.9636855639766,-16.3488644542006,
-0.468050067338545));
#65211=CARTESIAN_POINT('Ctrl Pts',(-17.2221126135063,-16.8802618020223,
-0.513595334960445));
#65212=CARTESIAN_POINT('Ctrl Pts',(-17.1722616763361,-16.9190322283098,
-0.516748667021866));
#65213=CARTESIAN_POINT('Origin',(23.734,10.1295,-7.));
#65214=CARTESIAN_POINT('',(22.1191569089489,8.64088535679774,-10.9946458471364));
#65215=CARTESIAN_POINT('',(22.5286570306555,8.64088535511415,-10.994645846509));
#65216=CARTESIAN_POINT('',(23.734,8.64088535679774,-10.9946458471364));
#65217=CARTESIAN_POINT('',(23.534,7.33966741897454,-3.77664721604215));
#65218=CARTESIAN_POINT('Ctrl Pts',(23.534,7.33966741897454,-3.77664721604215));
#65219=CARTESIAN_POINT('Ctrl Pts',(23.51017627993,7.66133406205805,-3.49824266610593));
#65220=CARTESIAN_POINT('Ctrl Pts',(23.486909633093,8.02286895090474,-3.26954919204704));
#65221=CARTESIAN_POINT('Ctrl Pts',(23.4492315066612,8.63411569299029,-3.0005309807086));
#65222=CARTESIAN_POINT('Ctrl Pts',(23.4354446806246,8.8639010841975,-2.92198759519112));
#65223=CARTESIAN_POINT('Ctrl Pts',(23.399949158547,9.47603266342949,-2.76951143292666));
#65224=CARTESIAN_POINT('Ctrl Pts',(23.3787721949749,9.86402116292083,-2.72757919192478));
#65225=CARTESIAN_POINT('Ctrl Pts',(23.3407214533443,10.5425275171154,-2.747133164482));
#65226=CARTESIAN_POINT('Ctrl Pts',(23.3242429944554,10.8311360244973,-2.78512529399453));
#65227=CARTESIAN_POINT('Ctrl Pts',(23.2929661635979,11.3716051953523,-2.91335793594839));
#65228=CARTESIAN_POINT('Ctrl Pts',(23.2783733783153,11.6233081664386,-2.99849923355931));
#65229=CARTESIAN_POINT('Ctrl Pts',(23.2328152819286,12.3725180640175,-3.33254296279843));
#65230=CARTESIAN_POINT('Ctrl Pts',(23.2012866427256,12.8305461368956,-3.65549380921278));
#65231=CARTESIAN_POINT('Ctrl Pts',(23.1549367702088,13.4067359697088,-4.25937645462649));
#65232=CARTESIAN_POINT('Ctrl Pts',(23.1395239514397,13.5793277462794,-4.48008348661314));
#65233=CARTESIAN_POINT('Ctrl Pts',(23.1099688138179,13.8617277895674,-4.92516171922708));
#65234=CARTESIAN_POINT('Ctrl Pts',(23.0959457347052,13.9759147216023,-5.14539286840817));
#65235=CARTESIAN_POINT('Ctrl Pts',(23.0504578182471,14.2830486657584,-5.88990281436943));
#65236=CARTESIAN_POINT('Ctrl Pts',(23.0202677929568,14.3925081775317,-6.44228728766363));
#65237=CARTESIAN_POINT('Ctrl Pts',(22.9756095483293,14.39249658211,-7.23314652577812));
#65238=CARTESIAN_POINT('Ctrl Pts',(22.9623778488159,14.3733770772517,-7.46584216670397));
#65239=CARTESIAN_POINT('Ctrl Pts',(22.9358798283986,14.2959926399339,-7.93359342777265));
#65240=CARTESIAN_POINT('Ctrl Pts',(22.9226192672182,14.2365591328009,-8.16761560319146));
#65241=CARTESIAN_POINT('Ctrl Pts',(22.8884454080608,14.0354961954562,-8.7480497067035));
#65242=CARTESIAN_POINT('Ctrl Pts',(22.867361205658,13.8675338973621,-9.08316268713324));
#65243=CARTESIAN_POINT('Ctrl Pts',(22.83129324382,13.5087614903736,-9.61239330323816));
#65244=CARTESIAN_POINT('Ctrl Pts',(22.816606886244,13.3391139157858,-9.81822440975084));
#65245=CARTESIAN_POINT('Ctrl Pts',(22.7763959093789,12.8279581857622,-10.3319271922136));
#65246=CARTESIAN_POINT('Ctrl Pts',(22.7505181760814,12.4542070728383,-10.6026540019325));
#65247=CARTESIAN_POINT('Ctrl Pts',(22.6994595055266,11.6432335511213,-11.0104357195506));
#65248=CARTESIAN_POINT('Ctrl Pts',(22.6750357731946,11.2124938682904,-11.1475429363853));
#65249=CARTESIAN_POINT('Ctrl Pts',(22.6356443648331,10.5204537580763,-11.2524316658375));
#65250=CARTESIAN_POINT('Ctrl Pts',(22.6214072895926,10.2697555020984,-11.2680612232353));
#65251=CARTESIAN_POINT('Ctrl Pts',(22.5828683772762,9.58434848171878,-11.2503118781594));
#65252=CARTESIAN_POINT('Ctrl Pts',(22.5592032550112,9.15383198149799,-11.1725793563088));
#65253=CARTESIAN_POINT('Ctrl Pts',(22.5327132940792,8.70849794314267,-11.0193555381541));
#65254=CARTESIAN_POINT('Ctrl Pts',(22.5306859582416,8.67460721925019,-11.007212382501));
#65255=CARTESIAN_POINT('Ctrl Pts',(22.5286570306555,8.64088535511415,-10.994645846509));
#65256=CARTESIAN_POINT('',(23.533999981869,7.33961491412,-10.2235360410646));
#65257=CARTESIAN_POINT('Origin',(23.534,10.1295,-7.));
#65258=CARTESIAN_POINT('',(22.2043183294109,10.1294634651143,-11.262893868652));
#65259=CARTESIAN_POINT('Ctrl Pts',(23.533999981869,7.33961491412,-10.2235360410646));
#65260=CARTESIAN_POINT('Ctrl Pts',(23.5009788547464,6.89416391178422,-9.83730563779938));
#65261=CARTESIAN_POINT('Ctrl Pts',(23.4291758459878,6.10016038128925,-8.79502345374906));
#65262=CARTESIAN_POINT('Ctrl Pts',(23.3185909555934,5.6985094017683,-6.80076298606476));
#65263=CARTESIAN_POINT('Ctrl Pts',(23.2022453106851,6.3076790998453,-4.74899581907506));
#65264=CARTESIAN_POINT('Ctrl Pts',(23.085899665777,7.80672899094502,-3.22136567669558));
#65265=CARTESIAN_POINT('Ctrl Pts',(22.9695540208687,9.84662493401956,-2.57356512891912));
#65266=CARTESIAN_POINT('Ctrl Pts',(22.8532083759605,11.9523856169729,-2.95643327596383));
#65267=CARTESIAN_POINT('Ctrl Pts',(22.7368627310523,13.6336979697146,-4.28082124831138));
#65268=CARTESIAN_POINT('Ctrl Pts',(22.6205170861441,14.4990821903827,-6.2383517396752));
#65269=CARTESIAN_POINT('Ctrl Pts',(22.5041714412359,14.3470299002299,-8.3732307562808));
#65270=CARTESIAN_POINT('Ctrl Pts',(22.3878257963277,13.2129653049274,-10.1883541012585));
#65271=CARTESIAN_POINT('Ctrl Pts',(22.2878747590527,11.6218855899156,-11.109940009747));
#65272=CARTESIAN_POINT('Ctrl Pts',(22.2267056034138,10.5292997601409,-11.262549287517));
#65273=CARTESIAN_POINT('Ctrl Pts',(22.2043183294109,10.1294634667828,-11.26269919276));
#65274=CARTESIAN_POINT('Ctrl Pts',(22.2043183294109,10.1294634642048,-11.2629999998434));
#65275=CARTESIAN_POINT('Ctrl Pts',(22.1969189590874,9.99730152393924,-11.2629988671572));
#65276=CARTESIAN_POINT('Ctrl Pts',(22.189519588764,9.86515952805542,-11.2568474502169));
#65277=CARTESIAN_POINT('Ctrl Pts',(22.1821202184405,9.73360519517336,-11.2445772820755));
#65278=CARTESIAN_POINT('Ctrl Pts',(22.174718676944,9.60201226073271,-11.2323035135386));
#65279=CARTESIAN_POINT('Ctrl Pts',(22.1673171354475,9.47100764621991,-11.2139074381013));
#65280=CARTESIAN_POINT('Ctrl Pts',(22.1599155939509,9.34115385194522,-11.1894724430228));
#65281=CARTESIAN_POINT('Ctrl Pts',(22.1583218981377,9.31319380492507,-11.184211113424));
#65282=CARTESIAN_POINT('Ctrl Pts',(22.1567282023245,9.28528708178846,-11.1786699942205));
#65283=CARTESIAN_POINT('Ctrl Pts',(22.1551345065113,9.25743924154366,-11.1728502289874));
#65284=CARTESIAN_POINT('Ctrl Pts',(22.147885780794,9.1307768295063,-11.1463797560378));
#65285=CARTESIAN_POINT('Ctrl Pts',(22.1406370550766,9.00529749216246,-11.1141331631283));
#65286=CARTESIAN_POINT('Ctrl Pts',(22.1333883293593,8.8815309348635,-11.0762411867384));
#65287=CARTESIAN_POINT('Ctrl Pts',(22.1286445225558,8.80053399009637,-11.0514434191851));
#65288=CARTESIAN_POINT('Ctrl Pts',(22.1239007157524,8.7202703940275,-11.0242288773707));
#65289=CARTESIAN_POINT('Ctrl Pts',(22.1191569089489,8.64088535679774,-10.9946458471364));
#65290=CARTESIAN_POINT('Origin',(23.734,10.1295,-7.));
#65291=CARTESIAN_POINT('',(20.6190482080202,8.64088535679775,-10.9946458471364));
#65292=CARTESIAN_POINT('',(21.0285562485163,8.64088535679775,-10.9946458471364));
#65293=CARTESIAN_POINT('',(23.734,8.64088535679774,-10.9946458471364));
#65294=CARTESIAN_POINT('',(21.113681670589,10.1298201264287,-11.2629999879802));
#65295=CARTESIAN_POINT('Ctrl Pts',(21.0285562485163,8.64088535679774,-10.9946458471364));
#65296=CARTESIAN_POINT('Ctrl Pts',(21.0355842654606,8.75858542230884,-11.0385070673122));
#65297=CARTESIAN_POINT('Ctrl Pts',(21.042612282405,8.878246078405,-11.0771699233389));
#65298=CARTESIAN_POINT('Ctrl Pts',(21.0496402993493,8.99937754862533,-11.1104734818387));
#65299=CARTESIAN_POINT('Ctrl Pts',(21.0566702577254,9.12054248041531,-11.1437862401718));
#65300=CARTESIAN_POINT('Ctrl Pts',(21.0637002161014,9.24317866806857,-11.1717366365414));
#65301=CARTESIAN_POINT('Ctrl Pts',(21.0707301744775,9.36678222315231,-11.1942139421923));
#65302=CARTESIAN_POINT('Ctrl Pts',(21.0774006019609,9.48406436150666,-11.215541698254));
#65303=CARTESIAN_POINT('Ctrl Pts',(21.0840710294444,9.60221707186205,-11.2319422034653));
#65304=CARTESIAN_POINT('Ctrl Pts',(21.0907414569279,9.7208031090756,-11.2433637425218));
#65305=CARTESIAN_POINT('Ctrl Pts',(21.0983881948149,9.8567458722469,-11.2564569836444));
#65306=CARTESIAN_POINT('Ctrl Pts',(21.106034932702,9.99328288766813,-11.2630102411303));
#65307=CARTESIAN_POINT('Ctrl Pts',(21.113681670589,10.1298201264287,-11.2629999879802));
#65308=CARTESIAN_POINT('Ctrl Pts',(22.5286570306555,8.64088535511415,-10.994645846509));
#65309=CARTESIAN_POINT('Ctrl Pts',(22.5118636558758,8.36177046378126,-10.8906329926018));
#65310=CARTESIAN_POINT('Ctrl Pts',(22.4949371726258,8.09422513235076,-10.7576155574016));
#65311=CARTESIAN_POINT('Ctrl Pts',(22.4658689060726,7.65365862514857,-10.4775761889738));
#65312=CARTESIAN_POINT('Ctrl Pts',(22.4535279654699,7.47441140277351,-10.3427282621983));
#65313=CARTESIAN_POINT('Ctrl Pts',(22.4257237608203,7.10029198315386,-10.0121190423));
#65314=CARTESIAN_POINT('Ctrl Pts',(22.4102377872913,6.9121452084373,-9.81026367361129));
#65315=CARTESIAN_POINT('Ctrl Pts',(22.3707645547773,6.48795081170686,-9.25627062175758));
#65316=CARTESIAN_POINT('Ctrl Pts',(22.3475332522488,6.28239420355209,-8.88452324880333));
#65317=CARTESIAN_POINT('Ctrl Pts',(22.2991968287437,5.97938706676746,-8.07143465124029));
#65318=CARTESIAN_POINT('Ctrl Pts',(22.273851585444,5.89022879368264,-7.63244016957764));
#65319=CARTESIAN_POINT('Ctrl Pts',(22.2344146536939,5.85912002685203,-6.9263610284236));
#65320=CARTESIAN_POINT('Ctrl Pts',(22.2200353762392,5.87167646499845,-6.66457609220379));
#65321=CARTESIAN_POINT('Ctrl Pts',(22.1818223710797,5.96723863349493,-5.98591179105523));
#65322=CARTESIAN_POINT('Ctrl Pts',(22.1576958095408,6.08858787963603,-5.57739186590976));
#65323=CARTESIAN_POINT('Ctrl Pts',(22.1205062536004,6.37074684053622,-4.97428398518268));
#65324=CARTESIAN_POINT('Ctrl Pts',(22.1071894019662,6.49179727944132,-4.76418413843906));
#65325=CARTESIAN_POINT('Ctrl Pts',(22.0671850918357,6.90229670185062,-4.17411268177498));
#65326=CARTESIAN_POINT('Ctrl Pts',(22.0400473276349,7.23830147516879,-3.83117576454053));
#65327=CARTESIAN_POINT('Ctrl Pts',(21.9977748536775,7.85232129043855,-3.38513612330148));
#65328=CARTESIAN_POINT('Ctrl Pts',(21.9822603591102,8.0965069728334,-3.24237784686094));
#65329=CARTESIAN_POINT('Ctrl Pts',(21.9508581575842,8.6070684025483,-3.0083229022697));
#65330=CARTESIAN_POINT('Ctrl Pts',(21.9350483246724,8.87196946541536,-2.91712190086957));
#65331=CARTESIAN_POINT('Ctrl Pts',(21.8879430145404,9.68327455895831,-2.72432043907536));
#65332=CARTESIAN_POINT('Ctrl Pts',(21.8579319608022,10.2425282684304,-2.70258470449789));
#65333=CARTESIAN_POINT('Ctrl Pts',(21.8116740680761,11.0520540128713,-2.82959340678504));
#65334=CARTESIAN_POINT('Ctrl Pts',(21.7966310224467,11.3094654254284,-2.89499238840428));
#65335=CARTESIAN_POINT('Ctrl Pts',(21.7656906411665,11.8324564954503,-3.08116396146755));
#65336=CARTESIAN_POINT('Ctrl Pts',(21.7497498339434,12.0951273402525,-3.20610388733662));
#65337=CARTESIAN_POINT('Ctrl Pts',(21.7178985270123,12.5819652847213,-3.50189737230709));
#65338=CARTESIAN_POINT('Ctrl Pts',(21.7020850761519,12.8060015909147,-3.67018921888465));
#65339=CARTESIAN_POINT('Ctrl Pts',(21.6554218096547,13.414664248813,-4.22878178565749));
#65340=CARTESIAN_POINT('Ctrl Pts',(21.6258177033332,13.7425641809248,-4.672399799817));
#65341=CARTESIAN_POINT('Ctrl Pts',(21.5800184528173,14.091699551123,-5.40491681528636));
#65342=CARTESIAN_POINT('Ctrl Pts',(21.5649766711582,14.1831276533754,-5.65410747919475));
#65343=CARTESIAN_POINT('Ctrl Pts',(21.5244527242273,14.3689368074488,-6.35677233692095));
#65344=CARTESIAN_POINT('Ctrl Pts',(21.4991530720328,14.4136600195989,-6.81960777591371));
#65345=CARTESIAN_POINT('Ctrl Pts',(21.4579890825941,14.3657168863367,-7.54651079827598));
#65346=CARTESIAN_POINT('Ctrl Pts',(21.4429061062594,14.3232719350075,-7.81024381229356));
#65347=CARTESIAN_POINT('Ctrl Pts',(21.4159048305994,14.2016669275244,-8.28002389107006));
#65348=CARTESIAN_POINT('Ctrl Pts',(21.4038280841489,14.1306451549211,-8.48722632324378));
#65349=CARTESIAN_POINT('Ctrl Pts',(21.3837784855311,13.9883604529451,-8.81717803075001));
#65350=CARTESIAN_POINT('Ctrl Pts',(21.3758969361811,13.9263289765945,-8.94345786773658));
#65351=CARTESIAN_POINT('Ctrl Pts',(21.3539492458001,13.7375378316432,-9.28411162819851));
#65352=CARTESIAN_POINT('Ctrl Pts',(21.3398129173365,13.5980747677776,-9.49080140356762));
#65353=CARTESIAN_POINT('Ctrl Pts',(21.3135714918117,13.3034777608084,-9.85429566101133));
#65354=CARTESIAN_POINT('Ctrl Pts',(21.3015202725534,13.1526673276748,-10.0135693682859));
#65355=CARTESIAN_POINT('Ctrl Pts',(21.2602281400547,12.5999537871976,-10.5138599540741));
#65356=CARTESIAN_POINT('Ctrl Pts',(21.2303768190197,12.1475356841319,-10.7918148242534));
#65357=CARTESIAN_POINT('Ctrl Pts',(21.1865848300647,11.4157097369092,-11.0724755597816));
#65358=CARTESIAN_POINT('Ctrl Pts',(21.1723949368264,11.167582150591,-11.1426779064966));
#65359=CARTESIAN_POINT('Ctrl Pts',(21.1433266163339,10.6558371681204,-11.2385692421312));
#65360=CARTESIAN_POINT('Ctrl Pts',(21.1284972322154,10.3931077210865,-11.2629799952814));
#65361=CARTESIAN_POINT('Ctrl Pts',(21.1136182667127,10.1298237102038,-11.2629999877096));
#65362=CARTESIAN_POINT('',(20.7043183293681,10.1330470781642,-11.2629985243062));
#65363=CARTESIAN_POINT('Ctrl Pts',(22.1191569089489,8.64088535679774,-10.9946458471364));
#65364=CARTESIAN_POINT('Ctrl Pts',(22.1119092550574,8.5195997948344,-10.9494484828501));
#65365=CARTESIAN_POINT('Ctrl Pts',(22.1046616011658,8.40036603378345,-10.8987202994482));
#65366=CARTESIAN_POINT('Ctrl Pts',(22.0974139472743,8.28368678979871,-10.8426738858569));
#65367=CARTESIAN_POINT('Ctrl Pts',(22.0901668484829,8.16701648231366,-10.7866317648778));
#65368=CARTESIAN_POINT('Ctrl Pts',(22.0829197496915,8.05290061237157,-10.7252723788802));
#65369=CARTESIAN_POINT('Ctrl Pts',(22.0756726509,7.94181920681921,-10.6588552509149));
#65370=CARTESIAN_POINT('Ctrl Pts',(22.0684237902754,7.83071079640412,-10.5924219763641));
#65371=CARTESIAN_POINT('Ctrl Pts',(22.0611749296508,7.72263862195278,-10.5209286802897));
#65372=CARTESIAN_POINT('Ctrl Pts',(22.0539260690261,7.61805591081906,-10.4446796058441));
#65373=CARTESIAN_POINT('Ctrl Pts',(22.0488803332185,7.54525871443813,-10.3916046875702));
#65374=CARTESIAN_POINT('Ctrl Pts',(22.0438345974108,7.47415165964849,-10.3362264444816));
#65375=CARTESIAN_POINT('Ctrl Pts',(22.0387888616031,7.40487871978231,-10.2786594637725));
#65376=CARTESIAN_POINT('Ctrl Pts',(22.0315394209714,7.30535110199038,-10.1959503357274));
#65377=CARTESIAN_POINT('Ctrl Pts',(22.0242899803397,7.20957401612299,-10.1086907026288));
#65378=CARTESIAN_POINT('Ctrl Pts',(22.017040539708,7.11795438636582,-10.0172441096141));
#65379=CARTESIAN_POINT('Ctrl Pts',(22.0097925532381,7.02635313454589,-9.9258158598272));
#65380=CARTESIAN_POINT('Ctrl Pts',(22.0025445667682,6.93890792009219,-9.83020256976117));
#65381=CARTESIAN_POINT('Ctrl Pts',(21.9952965802982,6.85598915380836,-9.73080496188683));
#65382=CARTESIAN_POINT('Ctrl Pts',(21.9880483796479,6.77306793724778,-9.63140441678055));
#65383=CARTESIAN_POINT('Ctrl Pts',(21.9808001789976,6.6946736606481,-9.52821959371692));
#65384=CARTESIAN_POINT('Ctrl Pts',(21.9735519783473,6.62113693951177,-9.4216848754125));
#65385=CARTESIAN_POINT('Ctrl Pts',(21.9663041219354,6.54760371085093,-9.31515521675567));
#65386=CARTESIAN_POINT('Ctrl Pts',(21.9590562655235,6.47892777135004,-9.2052762668258));
#65387=CARTESIAN_POINT('Ctrl Pts',(21.9518084091116,6.41539671901929,-9.09251184422175));
#65388=CARTESIAN_POINT('Ctrl Pts',(21.9445590323088,6.35185233970911,-8.97972376689949));
#65389=CARTESIAN_POINT('Ctrl Pts',(21.937309655506,6.29345517258953,-8.86404930972801));
#65390=CARTESIAN_POINT('Ctrl Pts',(21.9300602787033,6.24044729171331,-8.74597767229939));
#65391=CARTESIAN_POINT('Ctrl Pts',(21.9275212580338,6.22188181928044,-8.70462427930291));
#65392=CARTESIAN_POINT('Ctrl Pts',(21.9249822373644,6.20397701830355,-8.66297703249341));
#65393=CARTESIAN_POINT('Ctrl Pts',(21.922443216695,6.18674190960378,-8.62105756856911));
#65394=CARTESIAN_POINT('Ctrl Pts',(21.9151754459718,6.13740760526893,-8.50106600792267));
#65395=CARTESIAN_POINT('Ctrl Pts',(21.9079076752487,6.09354713243275,-8.37880167535367));
#65396=CARTESIAN_POINT('Ctrl Pts',(21.9006399045255,6.05534999136786,-8.25477914676757));
#65397=CARTESIAN_POINT('Ctrl Pts',(21.8933734613687,6.01715982757829,-8.13077927273893));
#65398=CARTESIAN_POINT('Ctrl Pts',(21.8861070182118,5.98463103242785,-8.00502217048947));
#65399=CARTESIAN_POINT('Ctrl Pts',(21.878840575055,5.95790341045558,-7.87803809376438));
#65400=CARTESIAN_POINT('Ctrl Pts',(21.871573922425,5.93117501799356,-7.75105035640947));
#65401=CARTESIAN_POINT('Ctrl Pts',(21.8643072697949,5.91024820677359,-7.6228359082289));
#65402=CARTESIAN_POINT('Ctrl Pts',(21.8570406171649,5.89521184619667,-7.49393605918256));
#65403=CARTESIAN_POINT('Ctrl Pts',(21.8497743641547,5.8801763125242,-7.36504329881022));
#65404=CARTESIAN_POINT('Ctrl Pts',(21.8425081111445,5.8710306198732,-7.23546555319564));
#65405=CARTESIAN_POINT('Ctrl Pts',(21.8352418581342,5.86781184389181,-7.10574998859196));
#65406=CARTESIAN_POINT('Ctrl Pts',(21.8279743223649,5.8645924996789,-6.9760115244532));
#65407=CARTESIAN_POINT('Ctrl Pts',(21.8207067865956,5.86730217015556,-6.84613553506541));
#65408=CARTESIAN_POINT('Ctrl Pts',(21.8134392508263,5.87592582273696,-6.7166703006725));
#65409=CARTESIAN_POINT('Ctrl Pts',(21.8109920244798,5.878829699714,-6.67307495520454));
#65410=CARTESIAN_POINT('Ctrl Pts',(21.8085447981333,5.88240372517832,-6.62952616917805));
#65411=CARTESIAN_POINT('Ctrl Pts',(21.8060975717868,5.88664599746917,-6.58604479323473));
#65412=CARTESIAN_POINT('Ctrl Pts',(21.7989003324876,5.89912242773205,-6.45816701512477));
#65413=CARTESIAN_POINT('Ctrl Pts',(21.7917030931884,5.9173874845122,-6.33082262933598));
#65414=CARTESIAN_POINT('Ctrl Pts',(21.7845058538891,5.94137144353383,-6.20454529072198));
#65415=CARTESIAN_POINT('Ctrl Pts',(21.777310240048,5.96534998590645,-6.07829647117027));
#65416=CARTESIAN_POINT('Ctrl Pts',(21.7701146262068,5.9950447885472,-5.95311456770553));
#65417=CARTESIAN_POINT('Ctrl Pts',(21.7629190123656,6.03033483538351,-5.82952404843386));
#65418=CARTESIAN_POINT('Ctrl Pts',(21.7557229447161,6.06562710786945,-5.705925734636));
#65419=CARTESIAN_POINT('Ctrl Pts',(21.7485268770667,6.10651523595494,-5.58391934900157));
#65420=CARTESIAN_POINT('Ctrl Pts',(21.7413308094172,6.15282797750728,-5.46401542145645));
#65421=CARTESIAN_POINT('Ctrl Pts',(21.7341348236115,6.199140192326,-5.34411285762736));
#65422=CARTESIAN_POINT('Ctrl Pts',(21.7269388378059,6.25087676563492,-5.22631303483247));
#65423=CARTESIAN_POINT('Ctrl Pts',(21.7197428520002,6.3078179577087,-5.11110737001062));
#65424=CARTESIAN_POINT('Ctrl Pts',(21.7125445442252,6.36477752331817,-4.99586453112694));
#65425=CARTESIAN_POINT('Ctrl Pts',(21.7053462364502,6.42694490292231,-4.88321784067244));
#65426=CARTESIAN_POINT('Ctrl Pts',(21.6981479286752,6.49405382499079,-4.77363522561758));
#65427=CARTESIAN_POINT('Ctrl Pts',(21.6953492614097,6.52014544947959,-4.73103003461787));
#65428=CARTESIAN_POINT('Ctrl Pts',(21.6925505941441,6.54698356415018,-4.68888773294117));
#65429=CARTESIAN_POINT('Ctrl Pts',(21.6897519268785,6.57455071884714,-4.64723468904552));
#65430=CARTESIAN_POINT('Ctrl Pts',(21.6823654767811,6.64730799692895,-4.53730088807892));
#65431=CARTESIAN_POINT('Ctrl Pts',(21.6749790266836,6.72517120219222,-4.43074005094906));
#65432=CARTESIAN_POINT('Ctrl Pts',(21.6675925765861,6.8078078071312,-4.32801010933154));
#65433=CARTESIAN_POINT('Ctrl Pts',(21.6602070407686,6.89043418347741,-4.22529288341958));
#65434=CARTESIAN_POINT('Ctrl Pts',(21.652821504951,6.97783258068516,-4.12640585384117));
#65435=CARTESIAN_POINT('Ctrl Pts',(21.6454359691335,7.06962978046818,-4.03177439543045));
#65436=CARTESIAN_POINT('Ctrl Pts',(21.6380510733541,7.16141902501109,-3.93715113787961));
#65437=CARTESIAN_POINT('Ctrl Pts',(21.6306661775747,7.2576060910435,-3.84678294446063));
#65438=CARTESIAN_POINT('Ctrl Pts',(21.6232812817953,7.3577801678109,-3.76105909719711));
#65439=CARTESIAN_POINT('Ctrl Pts',(21.6158977417591,7.45793585429648,-3.67535098739542));
#65440=CARTESIAN_POINT('Ctrl Pts',(21.6085142017228,7.56207684856391,-3.59428572780241));
#65441=CARTESIAN_POINT('Ctrl Pts',(21.6011306616865,7.66975832511667,-3.51821311783129));
#65442=CARTESIAN_POINT('Ctrl Pts',(21.5937483307954,7.77742216750874,-3.4421529656818));
#65443=CARTESIAN_POINT('Ctrl Pts',(21.5863659999042,7.88862507567842,-3.3710840148624));
#65444=CARTESIAN_POINT('Ctrl Pts',(21.5789836690131,8.0028919322252,-3.30531366337072));
#65445=CARTESIAN_POINT('Ctrl Pts',(21.5771245399989,8.03166832162039,-3.28875038944878));
#65446=CARTESIAN_POINT('Ctrl Pts',(21.5752654109847,8.06063888910807,-3.27252294045707));
#65447=CARTESIAN_POINT('Ctrl Pts',(21.5734062819705,8.08979577177236,-3.25663578296871));
#65448=CARTESIAN_POINT('Ctrl Pts',(21.5663766750943,8.20004171021903,-3.19656438896128));
#65449=CARTESIAN_POINT('Ctrl Pts',(21.5593470682181,8.31298831198066,-3.14134266250149));
#65450=CARTESIAN_POINT('Ctrl Pts',(21.5523174613419,8.42817722338396,-3.0912060926972));
#65451=CARTESIAN_POINT('Ctrl Pts',(21.5452896275042,8.54333708133278,-3.04108216855934));
#65452=CARTESIAN_POINT('Ctrl Pts',(21.5382617936664,8.6607377697407,-2.99604099920424));
#65453=CARTESIAN_POINT('Ctrl Pts',(21.5312339598286,8.7798993723283,-2.95627063890421));
#65454=CARTESIAN_POINT('Ctrl Pts',(21.5242047012697,8.89908513201198,-2.9164922161378));
#65455=CARTESIAN_POINT('Ctrl Pts',(21.5171754427108,9.02003215567398,-2.88198686387374));
#65456=CARTESIAN_POINT('Ctrl Pts',(21.5101461841518,9.14224366034339,-2.85289330739999));
#65457=CARTESIAN_POINT('Ctrl Pts',(21.5031162567188,9.26446679413621,-2.82379698250799));
#65458=CARTESIAN_POINT('Ctrl Pts',(21.4960863292857,9.38795427288864,-2.80011356232756));
#65459=CARTESIAN_POINT('Ctrl Pts',(21.4890564018526,9.5121981594764,-2.78193084010158));
#65460=CARTESIAN_POINT('Ctrl Pts',(21.4820218975376,9.63652293588892,-2.76373627989101));
#65461=CARTESIAN_POINT('Ctrl Pts',(21.4749873932226,9.76160472207926,-2.75104962078328));
#65462=CARTESIAN_POINT('Ctrl Pts',(21.4679528889076,9.88692926940032,-2.74390690413657));
#65463=CARTESIAN_POINT('Ctrl Pts',(21.4643221382925,9.95161359638359,-2.74022030139992));
#65464=CARTESIAN_POINT('Ctrl Pts',(21.4606913876774,10.0163625427089,-2.73800972683479));
#65465=CARTESIAN_POINT('Ctrl Pts',(21.4570606370622,10.0811053611285,-2.737274702854));
#65466=CARTESIAN_POINT('Ctrl Pts',(21.4494491623812,10.216831654508,-2.73573380483792));
#65467=CARTESIAN_POINT('Ctrl Pts',(21.4418376877003,10.3526182676046,-2.74067973952619));
#65468=CARTESIAN_POINT('Ctrl Pts',(21.4342262130193,10.4878649307102,-2.75208950465796));
#65469=CARTESIAN_POINT('Ctrl Pts',(21.4264336112805,10.6263300017054,-2.76377078316592));
#65470=CARTESIAN_POINT('Ctrl Pts',(21.4186410095417,10.764228814435,-2.78222738393882));
#65471=CARTESIAN_POINT('Ctrl Pts',(21.410848407803,10.9009217006177,-2.80737819976378));
#65472=CARTESIAN_POINT('Ctrl Pts',(21.4032429171247,11.0343324030374,-2.83192510998959));
#65473=CARTESIAN_POINT('Ctrl Pts',(21.3956374264465,11.1665941568544,-2.86284837110384));
#65474=CARTESIAN_POINT('Ctrl Pts',(21.3880319357682,11.2971204731094,-2.90002055727401));
#65475=CARTESIAN_POINT('Ctrl Pts',(21.3801457784992,11.4324636220633,-2.93856451434043));
#65476=CARTESIAN_POINT('Ctrl Pts',(21.3722596212301,11.5659405054026,-2.98382740162559));
#65477=CARTESIAN_POINT('Ctrl Pts',(21.3643734639611,11.6969110187463,-3.03560954265189));
#65478=CARTESIAN_POINT('Ctrl Pts',(21.3564873066921,11.8278815320899,-3.08739168367819));
#65479=CARTESIAN_POINT('Ctrl Pts',(21.3486011494231,11.956345363596,-3.14569299962129));
#65480=CARTESIAN_POINT('Ctrl Pts',(21.340714992154,12.0816810369674,-3.21025618294525));
#65481=CARTESIAN_POINT('Ctrl Pts',(21.3336759604758,12.1935532384943,-3.26788403351437));
#65482=CARTESIAN_POINT('Ctrl Pts',(21.3266369287976,12.3028932792345,-3.33048051016728));
#65483=CARTESIAN_POINT('Ctrl Pts',(21.3195978971194,12.40925055225,-3.39779145252306));
#65484=CARTESIAN_POINT('Ctrl Pts',(21.3125590744663,12.5156046669697,-3.46510039606998));
#65485=CARTESIAN_POINT('Ctrl Pts',(21.3055202518132,12.6189758680056,-3.53712332086819));
#65486=CARTESIAN_POINT('Ctrl Pts',(21.2984814291601,12.7189414344944,-3.61356203994173));
#65487=CARTESIAN_POINT('Ctrl Pts',(21.2914389136867,12.8189594465259,-3.69004086152499));
#65488=CARTESIAN_POINT('Ctrl Pts',(21.2843963982133,12.9155679496317,-3.77093987410838));
#65489=CARTESIAN_POINT('Ctrl Pts',(21.2773538827399,13.0083761165701,-3.85591964074671));
#65490=CARTESIAN_POINT('Ctrl Pts',(21.2703094098651,13.1012100786724,-3.94092302671816));
#65491=CARTESIAN_POINT('Ctrl Pts',(21.2632649369902,13.1902413235328,-4.03000916216276));
#65492=CARTESIAN_POINT('Ctrl Pts',(21.2562204641154,13.2751155328051,-4.12280137637754));
#65493=CARTESIAN_POINT('Ctrl Pts',(21.2491695588495,13.3600672417159,-4.21567832025411));
#65494=CARTESIAN_POINT('Ctrl Pts',(21.2421186535837,13.4408540813723,-4.31226781405213));
#65495=CARTESIAN_POINT('Ctrl Pts',(21.2350677483178,13.5171614727389,-4.41215944345081));
#65496=CARTESIAN_POINT('Ctrl Pts',(21.2315016146271,13.5557554332217,-4.46268159508693));
#65497=CARTESIAN_POINT('Ctrl Pts',(21.2279354809365,13.5932042061302,-4.51404795176234));
#65498=CARTESIAN_POINT('Ctrl Pts',(21.2243693472458,13.6294713302574,-4.56620261990112));
#65499=CARTESIAN_POINT('Ctrl Pts',(21.2173459273525,13.7008986134619,-4.66892006279847));
#65500=CARTESIAN_POINT('Ctrl Pts',(21.2103225074592,13.7678679518273,-4.77488136034603));
#65501=CARTESIAN_POINT('Ctrl Pts',(21.2032990875659,13.8300824556287,-4.88366862493296));
#65502=CARTESIAN_POINT('Ctrl Pts',(21.1962814937663,13.8922453510204,-4.99236564789809));
#65503=CARTESIAN_POINT('Ctrl Pts',(21.1892638999668,13.9496610740247,-5.10388363594717));
#65504=CARTESIAN_POINT('Ctrl Pts',(21.1822463061672,14.0020763560252,-5.21777628599693));
#65505=CARTESIAN_POINT('Ctrl Pts',(21.1752329695233,14.0544598407996,-5.33159984416752));
#65506=CARTESIAN_POINT('Ctrl Pts',(21.1682196328795,14.1018487643949,-5.44779484503741));
#65507=CARTESIAN_POINT('Ctrl Pts',(21.1612062962356,14.1440362326073,-5.5658912743158));
#65508=CARTESIAN_POINT('Ctrl Pts',(21.1541426196187,14.1865265118952,-5.68483537017137));
#65509=CARTESIAN_POINT('Ctrl Pts',(21.1470789430017,14.223740187332,-5.80570794539113));
#65510=CARTESIAN_POINT('Ctrl Pts',(21.1400152663848,14.2555155490246,-5.92800900693764));
#65511=CARTESIAN_POINT('Ctrl Pts',(21.1330043158592,14.2870537267815,-6.04939716472518));
#65512=CARTESIAN_POINT('Ctrl Pts',(21.1259933653335,14.3132344332075,-6.17219216889758));
#65513=CARTESIAN_POINT('Ctrl Pts',(21.1189824148079,14.3339500177816,-6.29589130954337));
#65514=CARTESIAN_POINT('Ctrl Pts',(21.1119707905225,14.3546675931453,-6.41960233780791));
#65515=CARTESIAN_POINT('Ctrl Pts',(21.104959166237,14.3699189367607,-6.54421729408242));
#65516=CARTESIAN_POINT('Ctrl Pts',(21.0979475419516,14.3796478851492,-6.66922522109208));
#65517=CARTESIAN_POINT('Ctrl Pts',(21.0909338264986,14.3893797351281,-6.79427043083558));
#65518=CARTESIAN_POINT('Ctrl Pts',(21.0839201110456,14.3935858804475,-6.91970845912758));
#65519=CARTESIAN_POINT('Ctrl Pts',(21.0769063955927,14.3922622147059,-7.04502555802502));
#65520=CARTESIAN_POINT('Ctrl Pts',(21.069804034079,14.3909218192076,-7.17192653457186));
#65521=CARTESIAN_POINT('Ctrl Pts',(21.0627016725654,14.3839108701113,-7.29870309586766));
#65522=CARTESIAN_POINT('Ctrl Pts',(21.0555993110518,14.37127938786,-7.42482540499111));
#65523=CARTESIAN_POINT('Ctrl Pts',(21.0485733953341,14.358783863728,-7.54959020502676));
#65524=CARTESIAN_POINT('Ctrl Pts',(21.0415474796164,14.3407883237577,-7.67371439178308));
#65525=CARTESIAN_POINT('Ctrl Pts',(21.0345215638987,14.3173929110686,-7.79669439901484));
#65526=CARTESIAN_POINT('Ctrl Pts',(21.0273809794871,14.2936156660999,-7.92168154059925));
#65527=CARTESIAN_POINT('Ctrl Pts',(21.0202403950756,14.264260841247,-8.04548642037499));
#65528=CARTESIAN_POINT('Ctrl Pts',(21.013099810664,14.2294863484673,-8.16759622403539));
#65529=CARTESIAN_POINT('Ctrl Pts',(21.0059592262525,14.1947118556876,-8.28970602769578));
#65530=CARTESIAN_POINT('Ctrl Pts',(20.9988186418409,14.1545178775712,-8.41012037987649));
#65531=CARTESIAN_POINT('Ctrl Pts',(20.9916780574294,14.1091131539846,-8.52834817519842));
#65532=CARTESIAN_POINT('Ctrl Pts',(20.9848875792511,14.0659346454851,-8.64077920575989));
#65533=CARTESIAN_POINT('Ctrl Pts',(20.9780971010728,14.0179001275206,-8.75160660314064));
#65534=CARTESIAN_POINT('Ctrl Pts',(20.9713066228945,13.9651477064359,-8.86036976757665));
#65535=CARTESIAN_POINT('Ctrl Pts',(20.9645253559579,13.9124668436842,-8.96898539545253));
#65536=CARTESIAN_POINT('Ctrl Pts',(20.9577440890213,13.8550809778343,-9.07554198259683));
#65537=CARTESIAN_POINT('Ctrl Pts',(20.9509628220846,13.793177528671,-9.17959536747338));
#65538=CARTESIAN_POINT('Ctrl Pts',(20.9441888767195,13.7313409151793,-9.28353640840212));
#65539=CARTESIAN_POINT('Ctrl Pts',(20.9374149313544,13.6649966269885,-9.38497926183249));
#65540=CARTESIAN_POINT('Ctrl Pts',(20.9306409859893,13.5943792727532,-9.48350168617723));
#65541=CARTESIAN_POINT('Ctrl Pts',(20.9238724821202,13.5238186452894,-9.58194496766671));
#65542=CARTESIAN_POINT('Ctrl Pts',(20.9171039782511,13.4489920202032,-9.67747214528359));
#65543=CARTESIAN_POINT('Ctrl Pts',(20.910335474382,13.370178451617,-9.76968810035086));
#65544=CARTESIAN_POINT('Ctrl Pts',(20.903569799622,13.2913978256411,-9.8618655108588));
#65545=CARTESIAN_POINT('Ctrl Pts',(20.896804124862,13.2086338378673,-9.95073412927473));
#65546=CARTESIAN_POINT('Ctrl Pts',(20.890038450102,13.1222067694605,-10.0359306961828));
#65547=CARTESIAN_POINT('Ctrl Pts',(20.8832740089491,13.035795459577,-10.1211117289289));
#65548=CARTESIAN_POINT('Ctrl Pts',(20.8765095677961,12.9457226947661,-10.2026217459866));
#65549=CARTESIAN_POINT('Ctrl Pts',(20.8697451266432,12.8523461041995,-10.2801338528855));
#65550=CARTESIAN_POINT('Ctrl Pts',(20.8629802282965,12.7589632025141,-10.3576511986577));
#65551=CARTESIAN_POINT('Ctrl Pts',(20.8562153299499,12.6622763543278,-10.4311698294127));
#65552=CARTESIAN_POINT('Ctrl Pts',(20.8494504316032,12.5626761707932,-10.5004032227565));
#65553=CARTESIAN_POINT('Ctrl Pts',(20.8426833849945,12.4630443582094,-10.5696586018671));
#65554=CARTESIAN_POINT('Ctrl Pts',(20.8359163383857,12.3604977161624,-10.6346258000381));
#65555=CARTESIAN_POINT('Ctrl Pts',(20.8291492917769,12.2554550341066,-10.6950621365488));
#65556=CARTESIAN_POINT('Ctrl Pts',(20.8223742557459,12.1502883348272,-10.7555698264038));
#65557=CARTESIAN_POINT('Ctrl Pts',(20.815599219715,12.0426200781834,-10.8115357695555));
#65558=CARTESIAN_POINT('Ctrl Pts',(20.808824183684,11.9328928762342,-10.8627636652982));
#65559=CARTESIAN_POINT('Ctrl Pts',(20.8020445915196,11.8230918840095,-10.9140260112088));
#65560=CARTESIAN_POINT('Ctrl Pts',(20.7952649993552,11.7112295779413,-10.9605438102634));
#65561=CARTESIAN_POINT('Ctrl Pts',(20.7884854071908,11.5977659401151,-11.002169927564));
#65562=CARTESIAN_POINT('Ctrl Pts',(20.7816949968921,11.4841212493811,-11.0438624672861));
#65563=CARTESIAN_POINT('Ctrl Pts',(20.7749045865934,11.3688705257193,-11.0806476224473));
#65564=CARTESIAN_POINT('Ctrl Pts',(20.7681141762946,11.2524863546908,-11.1124288014722));
#65565=CARTESIAN_POINT('Ctrl Pts',(20.7650717067341,11.2003399773581,-11.1266684814808));
#65566=CARTESIAN_POINT('Ctrl Pts',(20.7620292371736,11.1479661589978,-11.1399042936374));
#65567=CARTESIAN_POINT('Ctrl Pts',(20.7589867676131,11.0954077443162,-11.1521309263401));
#65568=CARTESIAN_POINT('Ctrl Pts',(20.7486384526106,10.9166414426865,-11.193717224612));
#65569=CARTESIAN_POINT('Ctrl Pts',(20.7382901376082,10.7352286283145,-11.223745455636));
#65570=CARTESIAN_POINT('Ctrl Pts',(20.7279418226057,10.5523855434177,-11.2419732221183));
#65571=CARTESIAN_POINT('Ctrl Pts',(20.7200673248741,10.4132520268103,-11.2558435484257));
#65572=CARTESIAN_POINT('Ctrl Pts',(20.7121928271425,10.2732902767665,-11.2628818332749));
#65573=CARTESIAN_POINT('Ctrl Pts',(20.7043183294109,10.1330470789259,-11.2629985243055));
#65574=CARTESIAN_POINT('Ctrl Pts',(20.7043183293681,10.1330470781642,-11.2629985243062));
#65575=CARTESIAN_POINT('Ctrl Pts',(20.6972124859225,10.0064934563144,-11.2631038247387));
#65576=CARTESIAN_POINT('Ctrl Pts',(20.6901066424768,9.87976518847473,-11.2575689158587));
#65577=CARTESIAN_POINT('Ctrl Pts',(20.6830007990312,9.75340734194371,-11.2463776695622));
#65578=CARTESIAN_POINT('Ctrl Pts',(20.6761360072116,9.63133593439973,-11.2355660640696));
#65579=CARTESIAN_POINT('Ctrl Pts',(20.6692712153921,9.50961067676056,-11.2194756600415));
#65580=CARTESIAN_POINT('Ctrl Pts',(20.6624064235726,9.38872389838046,-11.1981448006553));
#65581=CARTESIAN_POINT('Ctrl Pts',(20.6555457687443,9.26790997108627,-11.1768267960766));
#65582=CARTESIAN_POINT('Ctrl Pts',(20.6486851139159,9.14793391910229,-11.1502746878193));
#65583=CARTESIAN_POINT('Ctrl Pts',(20.6418244590876,9.0292818698926,-11.1185785249504));
#65584=CARTESIAN_POINT('Ctrl Pts',(20.6349664011617,8.9106747329837,-11.0868943597471));
#65585=CARTESIAN_POINT('Ctrl Pts',(20.6281083432358,8.79339099550801,-11.0500701203385));
#65586=CARTESIAN_POINT('Ctrl Pts',(20.6212502853099,8.67790488099607,-11.0082465755594));
#65587=CARTESIAN_POINT('Ctrl Pts',(20.6205162595467,8.66554427041757,-11.003770153851));
#65588=CARTESIAN_POINT('Ctrl Pts',(20.6197822337835,8.65320423875188,-10.9992365089288));
#65589=CARTESIAN_POINT('Ctrl Pts',(20.6190482080202,8.64088535679775,-10.9946458471364));
#65590=CARTESIAN_POINT('Origin',(23.734,10.1295,-7.));
#65591=CARTESIAN_POINT('',(19.1191572628085,8.64088535679774,-10.9946458471364));
#65592=CARTESIAN_POINT('',(19.5287462306467,8.64088535560039,-10.9946458466902));
#65593=CARTESIAN_POINT('',(23.734,8.64088535679774,-10.9946458471364));
#65594=CARTESIAN_POINT('',(19.613681670589,10.1293184243372,-11.262999996133));
#65595=CARTESIAN_POINT('Ctrl Pts',(19.5287462306467,8.64088535560039,-10.9946458466902));
#65596=CARTESIAN_POINT('Ctrl Pts',(19.5427562929707,8.87611781401766,-11.0823058035117));
#65597=CARTESIAN_POINT('Ctrl Pts',(19.5565690978808,9.11863897266564,-11.1490184691121));
#65598=CARTESIAN_POINT('Ctrl Pts',(19.5847929390305,9.61761196897248,-11.2398990512266));
#65599=CARTESIAN_POINT('Ctrl Pts',(19.5992904570035,9.873209923916,-11.2629888770781));
#65600=CARTESIAN_POINT('Ctrl Pts',(19.6137437552536,10.1293149200936,-11.2629999959823));
#65601=CARTESIAN_POINT('Ctrl Pts',(19.613681670589,10.1293184243372,-11.262999996133));
#65602=CARTESIAN_POINT('Ctrl Pts',(19.6210623037642,10.2610687195736,-11.263005607826));
#65603=CARTESIAN_POINT('Ctrl Pts',(19.6284429369393,10.3928267771473,-11.2568991564636));
#65604=CARTESIAN_POINT('Ctrl Pts',(19.6358235701145,10.5240278125494,-11.2447045604052));
#65605=CARTESIAN_POINT('Ctrl Pts',(19.6432028342893,10.6552045120622,-11.2325122262675));
#65606=CARTESIAN_POINT('Ctrl Pts',(19.650582098464,10.7858240783452,-11.2142340323102));
#65607=CARTESIAN_POINT('Ctrl Pts',(19.6579613626388,10.9153264213143,-11.1899458034161));
#65608=CARTESIAN_POINT('Ctrl Pts',(19.6653396985726,11.044812474126,-11.1656606297492));
#65609=CARTESIAN_POINT('Ctrl Pts',(19.6727180345064,11.1731812706445,-11.1353669878975));
#65610=CARTESIAN_POINT('Ctrl Pts',(19.6800963704403,11.2998820511657,-11.0991919757812));
#65611=CARTESIAN_POINT('Ctrl Pts',(19.6849288196367,11.382864866059,-11.0754991119973));
#65612=CARTESIAN_POINT('Ctrl Pts',(19.6897612688331,11.4651323638681,-11.0492844183613));
#65613=CARTESIAN_POINT('Ctrl Pts',(19.6945937180296,11.5465329042847,-11.0205953226076));
#65614=CARTESIAN_POINT('Ctrl Pts',(19.7016231773756,11.6649411412557,-10.9788631027588));
#65615=CARTESIAN_POINT('Ctrl Pts',(19.7086526367216,11.7815525661295,-10.9318790465684));
#65616=CARTESIAN_POINT('Ctrl Pts',(19.7156820960676,11.8958854944383,-10.8798261926326));
#65617=CARTESIAN_POINT('Ctrl Pts',(19.722709782053,12.0101895793458,-10.8277864703587));
#65618=CARTESIAN_POINT('Ctrl Pts',(19.7297374680383,12.1222159630139,-10.7706806571767));
#65619=CARTESIAN_POINT('Ctrl Pts',(19.7367651540237,12.2315037832726,-10.7087395561171));
#65620=CARTESIAN_POINT('Ctrl Pts',(19.7437942650805,12.3408137648732,-10.6467858946649));
#65621=CARTESIAN_POINT('Ctrl Pts',(19.7508233761373,12.4473837362772,-10.5799951717423));
#65622=CARTESIAN_POINT('Ctrl Pts',(19.7578524871941,12.5507782076321,-10.5086437324479));
#65623=CARTESIAN_POINT('Ctrl Pts',(19.7648822673835,12.6541825215712,-10.4372855008895));
#65624=CARTESIAN_POINT('Ctrl Pts',(19.771912047573,12.7544104201016,-10.3613659117439));
#65625=CARTESIAN_POINT('Ctrl Pts',(19.7789418277624,12.8510567997471,-10.2812036794065));
#65626=CARTESIAN_POINT('Ctrl Pts',(19.7859761861195,12.947766120667,-10.20098924115));
#65627=CARTESIAN_POINT('Ctrl Pts',(19.7930105444766,13.0408889712832,-10.116526891086));
#65628=CARTESIAN_POINT('Ctrl Pts',(19.8000449028336,13.1300544842105,-10.0281746626118));
#65629=CARTESIAN_POINT('Ctrl Pts',(19.803676389535,13.176086170113,-9.9825628347157));
#65630=CARTESIAN_POINT('Ctrl Pts',(19.8073078762364,13.2210637677684,-9.93591490652767));
#65631=CARTESIAN_POINT('Ctrl Pts',(19.8109393629378,13.2649402640227,-9.88828380716734));
#65632=CARTESIAN_POINT('Ctrl Pts',(19.8185510511639,13.3569065129464,-9.788447814911));
#65633=CARTESIAN_POINT('Ctrl Pts',(19.82616273939,13.4440921851538,-9.68422623732347));
#65634=CARTESIAN_POINT('Ctrl Pts',(19.8337744276161,13.5261126987745,-9.57608058385672));
#65635=CARTESIAN_POINT('Ctrl Pts',(19.8415669759686,13.6100820889147,-9.46536529853304));
#65636=CARTESIAN_POINT('Ctrl Pts',(19.8493595243211,13.6886375971267,-9.350537337596));
#65637=CARTESIAN_POINT('Ctrl Pts',(19.8571520726736,13.7614114960694,-9.23212631468719));
#65638=CARTESIAN_POINT('Ctrl Pts',(19.8647577752929,13.8324404597364,-9.11655449063818));
#65639=CARTESIAN_POINT('Ctrl Pts',(19.8723634779121,13.8979617722854,-8.99756971412403));
#65640=CARTESIAN_POINT('Ctrl Pts',(19.8799691805314,13.9576776738065,-8.87569312462606));
#65641=CARTESIAN_POINT('Ctrl Pts',(19.8878551517505,14.0195940941942,-8.74932540750959));
#65642=CARTESIAN_POINT('Ctrl Pts',(19.8957411229696,14.0752688994055,-8.61984891580091));
#65643=CARTESIAN_POINT('Ctrl Pts',(19.9036270941887,14.1244221857155,-8.48787288774221));
#65644=CARTESIAN_POINT('Ctrl Pts',(19.9115130654078,14.1735754720254,-8.35589685968352));
#65645=CARTESIAN_POINT('Ctrl Pts',(19.9193990366269,14.2162070893851,-8.22142157961869));
#65646=CARTESIAN_POINT('Ctrl Pts',(19.9272850078459,14.2520924147731,-8.08508100234748));
#65647=CARTESIAN_POINT('Ctrl Pts',(19.9343239536661,14.2841233281666,-7.9633846494403));
#65648=CARTESIAN_POINT('Ctrl Pts',(19.9413628994862,14.3107676181272,-7.8402454199408));
#65649=CARTESIAN_POINT('Ctrl Pts',(19.9484018453063,14.3319126474473,-7.71616823482706));
#65650=CARTESIAN_POINT('Ctrl Pts',(19.9554405817332,14.3530570477492,-7.59209474073655));
#65651=CARTESIAN_POINT('Ctrl Pts',(19.9624793181602,14.3687024503286,-7.4670837237731));
#65652=CARTESIAN_POINT('Ctrl Pts',(19.9695180545871,14.3787875954937,-7.34164884133137));
#65653=CARTESIAN_POINT('Ctrl Pts',(19.976560483799,14.3888780317039,-7.21614815104951));
#65654=CARTESIAN_POINT('Ctrl Pts',(19.9836029130109,14.3934023507515,-7.09022353254098));
#65655=CARTESIAN_POINT('Ctrl Pts',(19.9906453422228,14.3923512886368,-6.96439254336727));
#65656=CARTESIAN_POINT('Ctrl Pts',(19.9976897288499,14.3912999343835,-6.83852657996872));
#65657=CARTESIAN_POINT('Ctrl Pts',(20.0047341154771,14.384670122848,-6.71275468020004));
#65658=CARTESIAN_POINT('Ctrl Pts',(20.0117785021043,14.3725046893258,-6.58759218441076));
#65659=CARTESIAN_POINT('Ctrl Pts',(20.0188293217025,14.3603281462655,-6.46231538956881));
#65660=CARTESIAN_POINT('Ctrl Pts',(20.0258801413008,14.3426059296771,-6.33764949029167));
#65661=CARTESIAN_POINT('Ctrl Pts',(20.032930960899,14.3194325420246,-6.21410287360031));
#65662=CARTESIAN_POINT('Ctrl Pts',(20.0364975248507,14.3077105900036,-6.15160844961165));
#65663=CARTESIAN_POINT('Ctrl Pts',(20.0400640888024,14.2945946542908,-6.08940024916908));
#65664=CARTESIAN_POINT('Ctrl Pts',(20.043630652754,14.2801018815878,-6.02754279242752));
#65665=CARTESIAN_POINT('Ctrl Pts',(20.0506540757907,14.2515621231407,-5.9057305685185));
#65666=CARTESIAN_POINT('Ctrl Pts',(20.0576774988273,14.2176287610004,-5.78506067889005));
#65667=CARTESIAN_POINT('Ctrl Pts',(20.064700921864,14.178413687597,-5.66603337733305));
#65668=CARTESIAN_POINT('Ctrl Pts',(20.0717185186296,14.1392311450044,-5.54710481471211));
#65669=CARTESIAN_POINT('Ctrl Pts',(20.0787361153952,14.0947757355895,-5.42981649293811));
#65670=CARTESIAN_POINT('Ctrl Pts',(20.0857537121608,14.0452096568303,-5.31465526274116));
#65671=CARTESIAN_POINT('Ctrl Pts',(20.0927670515899,13.9956736481201,-5.19956389693379));
#65672=CARTESIAN_POINT('Ctrl Pts',(20.0997803910189,13.9410332971071,-5.08659740716836));
#65673=CARTESIAN_POINT('Ctrl Pts',(20.106793730448,13.8814994526977,-4.97622404724333));
#65674=CARTESIAN_POINT('Ctrl Pts',(20.1138574059531,13.821538322521,-4.86505851664211));
#65675=CARTESIAN_POINT('Ctrl Pts',(20.1209210814582,13.7566133174844,-4.75652385852162));
#65676=CARTESIAN_POINT('Ctrl Pts',(20.1279847569633,13.6869877988477,-4.65107480726828));
#65677=CARTESIAN_POINT('Ctrl Pts',(20.1349957098057,13.6178819590572,-4.54641281860872));
#65678=CARTESIAN_POINT('Ctrl Pts',(20.1420066626481,13.5441457768754,-4.4447908421696));
#65679=CARTESIAN_POINT('Ctrl Pts',(20.1490176154904,13.4660808058284,-4.34662525711552));
#65680=CARTESIAN_POINT('Ctrl Pts',(20.1560292419106,13.3880083346838,-4.24845024079589));
#65681=CARTESIAN_POINT('Ctrl Pts',(20.1630408683308,13.3056064871499,-4.15373257998509));
#65682=CARTESIAN_POINT('Ctrl Pts',(20.1700524947509,13.2192173973556,-4.06285591016064));
#65683=CARTESIAN_POINT('Ctrl Pts',(20.1770662121528,13.1328025449214,-3.97195213942652));
#65684=CARTESIAN_POINT('Ctrl Pts',(20.1840799295547,13.0423983490892,-3.8848919206958));
#65685=CARTESIAN_POINT('Ctrl Pts',(20.1910936469566,12.9483838509154,-3.80202207089415));
#65686=CARTESIAN_POINT('Ctrl Pts',(20.1981960049244,12.8531811813556,-3.71810489768801));
#65687=CARTESIAN_POINT('Ctrl Pts',(20.2052983628922,12.7542766304511,-3.63848501133126));
#65688=CARTESIAN_POINT('Ctrl Pts',(20.2124007208601,12.6520974127302,-3.56347976969624));
#65689=CARTESIAN_POINT('Ctrl Pts',(20.2194266380452,12.5510179226514,-3.48928178945322));
#65690=CARTESIAN_POINT('Ctrl Pts',(20.2264525552303,12.4467342673697,-3.41959977243168));
#65691=CARTESIAN_POINT('Ctrl Pts',(20.2334784724154,12.3396876781542,-3.35469625033312));
#65692=CARTESIAN_POINT('Ctrl Pts',(20.2406190507746,12.2308941159415,-3.28873351932974));
#65693=CARTESIAN_POINT('Ctrl Pts',(20.2477596291338,12.1192470170137,-3.22770681705742));
#65694=CARTESIAN_POINT('Ctrl Pts',(20.254900207493,12.0052331387805,-3.17184193219762));
#65695=CARTESIAN_POINT('Ctrl Pts',(20.2620407858522,11.8912192605474,-3.11597704733782));
#65696=CARTESIAN_POINT('Ctrl Pts',(20.2691813642114,11.7748390041325,-3.06527409536859));
#65697=CARTESIAN_POINT('Ctrl Pts',(20.2763219425706,11.6565970046819,-3.01990656663797));
#65698=CARTESIAN_POINT('Ctrl Pts',(20.2831124368812,11.5441521039813,-2.97676329024846));
#65699=CARTESIAN_POINT('Ctrl Pts',(20.2899029311918,11.4296496272437,-2.93830180029273));
#65700=CARTESIAN_POINT('Ctrl Pts',(20.2966934255024,11.3135242806343,-2.90472766438319));
#65701=CARTESIAN_POINT('Ctrl Pts',(20.3034747086535,11.1975564555602,-2.87119907106695));
#65702=CARTESIAN_POINT('Ctrl Pts',(20.3102559918046,11.0799705337984,-2.84254477101641));
#65703=CARTESIAN_POINT('Ctrl Pts',(20.3170372749558,10.9612220024664,-2.81892268540592));
#65704=CARTESIAN_POINT('Ctrl Pts',(20.3238112366047,10.8426016795597,-2.79532610369315));
#65705=CARTESIAN_POINT('Ctrl Pts',(20.3305851982536,10.7228216505048,-2.77675101741854));
#65706=CARTESIAN_POINT('Ctrl Pts',(20.3373591599025,10.602352688061,-2.76330561222627));
#65707=CARTESIAN_POINT('Ctrl Pts',(20.3441276801126,10.48198049683,-2.74987100756003));
#65708=CARTESIAN_POINT('Ctrl Pts',(20.3508962003228,10.3609208876254,-2.74155793704571));
#65709=CARTESIAN_POINT('Ctrl Pts',(20.3576647205329,10.2396542166227,-2.73842340810819));
#65710=CARTESIAN_POINT('Ctrl Pts',(20.3644304116747,10.1184382319863,-2.73529018932358));
#65711=CARTESIAN_POINT('Ctrl Pts',(20.3711961028166,9.99701577598613,-2.73733122414958));
#65712=CARTESIAN_POINT('Ctrl Pts',(20.3779617939584,9.8758711148973,-2.74455156433055));
#65713=CARTESIAN_POINT('Ctrl Pts',(20.3847262515225,9.7547485419237,-2.75177058803827));
#65714=CARTESIAN_POINT('Ctrl Pts',(20.3914907090865,9.63390408190446,-2.76416701590755));
#65715=CARTESIAN_POINT('Ctrl Pts',(20.3982551666505,9.51381996728511,-2.78169381181069));
#65716=CARTESIAN_POINT('Ctrl Pts',(20.4050200814275,9.39372773612192,-2.79922179235852));
#65717=CARTESIAN_POINT('Ctrl Pts',(20.4117849962045,9.27439636769387,-2.82188076925702));
#65718=CARTESIAN_POINT('Ctrl Pts',(20.4185499109815,9.15630016132667,-2.8495721818099));
#65719=CARTESIAN_POINT('Ctrl Pts',(20.4253169740298,9.03816645224213,-2.87727238806794));
#65720=CARTESIAN_POINT('Ctrl Pts',(20.4320840370781,8.92126909293508,-2.91000810994903));
#65721=CARTESIAN_POINT('Ctrl Pts',(20.4388511001264,8.8060686569394,-2.94763051040446));
#65722=CARTESIAN_POINT('Ctrl Pts',(20.4456261525318,8.69073221254255,-2.98529732876934));
#65723=CARTESIAN_POINT('Ctrl Pts',(20.4524012049372,8.57709708877692,-3.02786220934678));
#65724=CARTESIAN_POINT('Ctrl Pts',(20.4591762573426,8.46560533251585,-3.07512757716664));
#65725=CARTESIAN_POINT('Ctrl Pts',(20.465955865875,8.3540385996251,-3.12242473027806));
#65726=CARTESIAN_POINT('Ctrl Pts',(20.4727354744074,8.24461847941592,-3.17442847978152));
#65727=CARTESIAN_POINT('Ctrl Pts',(20.4795150829397,8.13776210427539,-3.23089544391052));
#65728=CARTESIAN_POINT('Ctrl Pts',(20.4863055094517,8.03073522222619,-3.28745251036128));
#65729=CARTESIAN_POINT('Ctrl Pts',(20.4930959359638,7.92628060892515,-3.34848679214083));
#65730=CARTESIAN_POINT('Ctrl Pts',(20.4998863624758,7.82478626913523,-3.41371172118535));
#65731=CARTESIAN_POINT('Ctrl Pts',(20.5029286524462,7.77931413105292,-3.44293420774036));
#65732=CARTESIAN_POINT('Ctrl Pts',(20.5059709424165,7.73443575525086,-3.4729973349816));
#65733=CARTESIAN_POINT('Ctrl Pts',(20.5090132323869,7.69018375192213,-3.50387282241288));
#65734=CARTESIAN_POINT('Ctrl Pts',(20.5160528480572,7.58778815547792,-3.57531623091908));
#65735=CARTESIAN_POINT('Ctrl Pts',(20.5230924637274,7.48839576824068,-3.65135791091549));
#65736=CARTESIAN_POINT('Ctrl Pts',(20.5301320793977,7.39243615095284,-3.73172056178803));
#65737=CARTESIAN_POINT('Ctrl Pts',(20.5371627089137,7.29659902727188,-3.81198062876912));
#65738=CARTESIAN_POINT('Ctrl Pts',(20.5441933384298,7.20418624476916,-3.89655044007299));
#65739=CARTESIAN_POINT('Ctrl Pts',(20.5512239679459,7.11559764941311,-3.98511001508732));
#65740=CARTESIAN_POINT('Ctrl Pts',(20.5582471924636,7.0271023598425,-4.07357631488181));
#65741=CARTESIAN_POINT('Ctrl Pts',(20.5652704169812,6.94242351009667,-4.16602373977542));
#65742=CARTESIAN_POINT('Ctrl Pts',(20.5722936414989,6.86192690158119,-4.26209294414699));
#65743=CARTESIAN_POINT('Ctrl Pts',(20.5793524281949,6.78102269755993,-4.3586485960431));
#65744=CARTESIAN_POINT('Ctrl Pts',(20.5864112148909,6.70434351288937,-4.45886255685475));
#65745=CARTESIAN_POINT('Ctrl Pts',(20.5934700015869,6.63222286897191,-4.56233274034623));
#65746=CARTESIAN_POINT('Ctrl Pts',(20.6004830794517,6.56056923879038,-4.66513290767694));
#65747=CARTESIAN_POINT('Ctrl Pts',(20.6074961573164,6.49341550627245,-4.77114692695205));
#65748=CARTESIAN_POINT('Ctrl Pts',(20.6145092351811,6.4310476922353,-4.87994822535157));
#65749=CARTESIAN_POINT('Ctrl Pts',(20.6215200654578,6.36869986616283,-4.9887146545394));
#65750=CARTESIAN_POINT('Ctrl Pts',(20.6285308957345,6.31113509680343,-5.10026624921301));
#65751=CARTESIAN_POINT('Ctrl Pts',(20.6355417260111,6.25859484105923,-5.21414943220723));
#65752=CARTESIAN_POINT('Ctrl Pts',(20.6425517265455,6.20606080353314,-5.32801913695587));
#65753=CARTESIAN_POINT('Ctrl Pts',(20.6495617270799,6.15855025661158,-5.44421952922821));
#65754=CARTESIAN_POINT('Ctrl Pts',(20.6565717276143,6.11625749444774,-5.56227485532575));
#65755=CARTESIAN_POINT('Ctrl Pts',(20.6636661271634,6.07345553582416,-5.68175154411103));
#65756=CARTESIAN_POINT('Ctrl Pts',(20.6707605267125,6.0359979916284,-5.80312775504321));
#65757=CARTESIAN_POINT('Ctrl Pts',(20.6778549262616,6.00403488298935,-5.92589266442861));
#65758=CARTESIAN_POINT('Ctrl Pts',(20.6848699695753,5.97242930594331,-6.04728435526654));
#65759=CARTESIAN_POINT('Ctrl Pts',(20.691885012889,5.94619591700699,-6.17003344375839));
#65760=CARTESIAN_POINT('Ctrl Pts',(20.6989000562027,5.92542852701159,-6.29363462004067));
#65761=CARTESIAN_POINT('Ctrl Pts',(20.7060341338695,5.90430874677111,-6.41933311566898));
#65762=CARTESIAN_POINT('Ctrl Pts',(20.7131682115363,5.88884222559255,-6.54591246948119));
#65763=CARTESIAN_POINT('Ctrl Pts',(20.720302289203,5.87907269796409,-6.67283528596788));
#65764=CARTESIAN_POINT('Ctrl Pts',(20.7274363668698,5.86930317033562,-6.79975810245456));
#65765=CARTESIAN_POINT('Ctrl Pts',(20.7345704445365,5.86523062067719,-6.92702396271638));
#65766=CARTESIAN_POINT('Ctrl Pts',(20.7417045222033,5.86684324052786,-7.05409575700999));
#65767=CARTESIAN_POINT('Ctrl Pts',(20.7487555408127,5.86843708532577,-7.17968810799774));
#65768=CARTESIAN_POINT('Ctrl Pts',(20.7558065594222,5.87558719238043,-7.30531726205016));
#65769=CARTESIAN_POINT('Ctrl Pts',(20.7628575780316,5.88828942330491,-7.43046700701646));
#65770=CARTESIAN_POINT('Ctrl Pts',(20.7699032665315,5.90098205217249,-7.55552214695005));
#65771=CARTESIAN_POINT('Ctrl Pts',(20.7769489550314,5.91921840902034,-7.68009822009394));
#65772=CARTESIAN_POINT('Ctrl Pts',(20.7839946435314,5.94294234854903,-7.80368154829967));
#65773=CARTESIAN_POINT('Ctrl Pts',(20.7910363483395,5.96665287436202,-7.92719500144824));
#65774=CARTESIAN_POINT('Ctrl Pts',(20.7980780531477,5.99584473055009,-8.04971645279611));
#65775=CARTESIAN_POINT('Ctrl Pts',(20.8051197579558,6.03041028946687,-8.17074016972232));
#65776=CARTESIAN_POINT('Ctrl Pts',(20.8121590390629,6.06496395118215,-8.29172223120907));
#65777=CARTESIAN_POINT('Ctrl Pts',(20.81919832017,6.10488752575289,-8.41120721791972));
#65778=CARTESIAN_POINT('Ctrl Pts',(20.8262376012772,6.15002298728712,-8.528702621601));
#65779=CARTESIAN_POINT('Ctrl Pts',(20.8332767281295,6.19515745974894,-8.64619545055594));
#65780=CARTESIAN_POINT('Ctrl Pts',(20.8403158549819,6.24550345864841,-8.76169842478665));
#65781=CARTESIAN_POINT('Ctrl Pts',(20.8473549818343,6.30085412572507,-8.87473725342982));
#65782=CARTESIAN_POINT('Ctrl Pts',(20.8509200435934,6.32888722566361,-8.93198730925843));
#65783=CARTESIAN_POINT('Ctrl Pts',(20.8544851053524,6.35820328570989,-8.98860562121714));
#65784=CARTESIAN_POINT('Ctrl Pts',(20.8580501671115,6.38877083910759,-9.04453279378179));
#65785=CARTESIAN_POINT('Ctrl Pts',(20.8656419313286,6.45386414569605,-9.16362916184931));
#65786=CARTESIAN_POINT('Ctrl Pts',(20.8732336955456,6.52461037034494,-9.27954435589301));
#65787=CARTESIAN_POINT('Ctrl Pts',(20.8808254597627,6.60067979658225,-9.39177694862015));
#65788=CARTESIAN_POINT('Ctrl Pts',(20.8886229891175,6.67881098811066,-9.50705146338692));
#65789=CARTESIAN_POINT('Ctrl Pts',(20.8964205184722,6.7625578532525,-9.61844067454016));
#65790=CARTESIAN_POINT('Ctrl Pts',(20.904218047827,6.85151803388108,-9.72543633750618));
#65791=CARTESIAN_POINT('Ctrl Pts',(20.9118262952094,6.93831874095385,-9.82983472264376));
#65792=CARTESIAN_POINT('Ctrl Pts',(20.9194345425919,7.03008237539708,-9.93005022576152));
#65793=CARTESIAN_POINT('Ctrl Pts',(20.9270427899744,7.12639604911989,-10.0256463210706));
#65794=CARTESIAN_POINT('Ctrl Pts',(20.9349349603153,7.22630393604349,-10.1248098511419));
#65795=CARTESIAN_POINT('Ctrl Pts',(20.9428271306562,7.3311078117208,-10.219002308715));
#65796=CARTESIAN_POINT('Ctrl Pts',(20.950719300997,7.4403062336633,-10.3077796007437));
#65797=CARTESIAN_POINT('Ctrl Pts',(20.9586114713379,7.5495046556058,-10.3965568927723));
#65798=CARTESIAN_POINT('Ctrl Pts',(20.9665036416788,7.66309737480791,-10.4799188219024));
#65799=CARTESIAN_POINT('Ctrl Pts',(20.9743958120197,7.78054523318155,-10.5574682716));
#65800=CARTESIAN_POINT('Ctrl Pts',(20.9814303456134,7.88523011320223,-10.6265904756971));
#65801=CARTESIAN_POINT('Ctrl Pts',(20.9884648792071,7.99304022283171,-10.6911356375115));
#65802=CARTESIAN_POINT('Ctrl Pts',(20.9954994128008,8.10354413328733,-10.75082281988));
#65803=CARTESIAN_POINT('Ctrl Pts',(21.0025299902701,8.213985897873,-10.8104764350032));
#65804=CARTESIAN_POINT('Ctrl Pts',(21.0095605677395,8.32711810832358,-10.8652773293347));
#65805=CARTESIAN_POINT('Ctrl Pts',(21.0165911452088,8.4424828530154,-10.9149894183484));
#65806=CARTESIAN_POINT('Ctrl Pts',(21.020579512978,8.50792797917055,-10.9431905290571));
#65807=CARTESIAN_POINT('Ctrl Pts',(21.0245678807472,8.5740911029662,-10.9697548034393));
#65808=CARTESIAN_POINT('Ctrl Pts',(21.0285562485163,8.64088535679774,-10.9946458471364));
#65809=CARTESIAN_POINT('',(19.2043183294647,10.1295728822702,-11.262999999377));
#65810=CARTESIAN_POINT('Ctrl Pts',(20.6190482080202,8.64088535679775,-10.9946458471364));
#65811=CARTESIAN_POINT('Ctrl Pts',(20.6121906086773,8.52579681219007,-10.9517578166766));
#65812=CARTESIAN_POINT('Ctrl Pts',(20.6053330093343,8.412555906166,-10.9038893145581));
#65813=CARTESIAN_POINT('Ctrl Pts',(20.5984754099914,8.30161734079923,-10.8512353841583));
#65814=CARTESIAN_POINT('Ctrl Pts',(20.5916140006898,8.19061713996373,-10.7985522001832));
#65815=CARTESIAN_POINT('Ctrl Pts',(20.5847525913881,8.0819222045518,-10.7410784518095));
#65816=CARTESIAN_POINT('Ctrl Pts',(20.5778911820865,7.97596448314815,-10.6790560987375));
#65817=CARTESIAN_POINT('Ctrl Pts',(20.5710276626094,7.869974175234,-10.6170146711514));
#65818=CARTESIAN_POINT('Ctrl Pts',(20.5641641431323,7.76672310363603,-10.5504220702988));
#65819=CARTESIAN_POINT('Ctrl Pts',(20.5573006236552,7.66661480714346,-10.4795639851579));
#65820=CARTESIAN_POINT('Ctrl Pts',(20.5504298984386,7.56640141088351,-10.4086315088973));
#65821=CARTESIAN_POINT('Ctrl Pts',(20.5435591732221,7.46933770314235,-10.333424853554));
#65822=CARTESIAN_POINT('Ctrl Pts',(20.5366884480055,7.37579474398677,-10.2542704809227));
#65823=CARTESIAN_POINT('Ctrl Pts',(20.5332241246026,7.32862897147049,-10.2143596510014));
#65824=CARTESIAN_POINT('Ctrl Pts',(20.5297598011996,7.28235772638468,-10.1734457866596));
#65825=CARTESIAN_POINT('Ctrl Pts',(20.5262954777966,7.23702496054344,-10.1315742281033));
#65826=CARTESIAN_POINT('Ctrl Pts',(20.5192443736102,7.14475700001478,-10.0463510293761));
#65827=CARTESIAN_POINT('Ctrl Pts',(20.5121932694238,7.05617966494,-9.95697401157821));
#65828=CARTESIAN_POINT('Ctrl Pts',(20.5051421652374,6.97167381122514,-9.86379167564396));
#65829=CARTESIAN_POINT('Ctrl Pts',(20.4980963907359,6.88723183255123,-9.77067977300234));
#65830=CARTESIAN_POINT('Ctrl Pts',(20.4910506162344,6.80685546329167,-9.67376856212323));
#65831=CARTESIAN_POINT('Ctrl Pts',(20.4840048417328,6.73088887631933,-9.57344349656137));
#65832=CARTESIAN_POINT('Ctrl Pts',(20.4769630507529,6.65496523913739,-9.47317515252287));
#65833=CARTESIAN_POINT('Ctrl Pts',(20.4699212597729,6.58344664850125,-9.36949710276488));
#65834=CARTESIAN_POINT('Ctrl Pts',(20.462879468793,6.51663692385959,-9.26282774268419));
#65835=CARTESIAN_POINT('Ctrl Pts',(20.4558401014794,6.4498501940051,-9.15619509640896));
#65836=CARTESIAN_POINT('Ctrl Pts',(20.4488007341658,6.38776930400394,-9.04657351481714));
#65837=CARTESIAN_POINT('Ctrl Pts',(20.4417613668523,6.33065452248795,-8.93440999738582));
#65838=CARTESIAN_POINT('Ctrl Pts',(20.434722154203,6.27354099585986,-8.82224894433653));
#65839=CARTESIAN_POINT('Ctrl Pts',(20.4276829415537,6.22139353779856,-8.70754640545444));
#65840=CARTESIAN_POINT('Ctrl Pts',(20.4206437289045,6.17442620344216,-8.59077347972034));
#65841=CARTESIAN_POINT('Ctrl Pts',(20.4170790968991,6.15064211400004,-8.53164008950059));
#65842=CARTESIAN_POINT('Ctrl Pts',(20.4135144648938,6.12818565038781,-8.47197612678181));
#65843=CARTESIAN_POINT('Ctrl Pts',(20.4099498328884,6.10707988819629,-8.41184469548072));
#65844=CARTESIAN_POINT('Ctrl Pts',(20.4023582696467,6.06213114504391,-8.28378335202333));
#65845=CARTESIAN_POINT('Ctrl Pts',(20.3947667064051,6.02332867012886,-8.15364975670661));
#65846=CARTESIAN_POINT('Ctrl Pts',(20.3871751431634,5.99082447735158,-8.02202442154324));
#65847=CARTESIAN_POINT('Ctrl Pts',(20.3793775635648,5.95743820071792,-7.88682709848179));
#65848=CARTESIAN_POINT('Ctrl Pts',(20.3715799839662,5.93069696443189,-7.75005621879711));
#65849=CARTESIAN_POINT('Ctrl Pts',(20.3637824043676,5.91070925233697,-7.61235090220622));
#65850=CARTESIAN_POINT('Ctrl Pts',(20.3561743707007,5.89120740761466,-7.47799296824972));
#65851=CARTESIAN_POINT('Ctrl Pts',(20.3485663370339,5.8781345404609,-7.34274577259572));
#65852=CARTESIAN_POINT('Ctrl Pts',(20.340958303367,5.87153877916962,-7.20720820906679));
#65853=CARTESIAN_POINT('Ctrl Pts',(20.3330659508026,5.86469652848814,-7.06660548779349));
#65854=CARTESIAN_POINT('Ctrl Pts',(20.3251735982381,5.86482489394197,-6.92569058452576));
#65855=CARTESIAN_POINT('Ctrl Pts',(20.3172812456736,5.87191837083124,-6.78513336470115));
#65856=CARTESIAN_POINT('Ctrl Pts',(20.3093888931092,5.8790118477205,-6.64457614487654));
#65857=CARTESIAN_POINT('Ctrl Pts',(20.3014965405447,5.89307041607502,-6.50437692574409));
#65858=CARTESIAN_POINT('Ctrl Pts',(20.2936041879802,5.91402841188901,-6.36520216617491));
#65859=CARTESIAN_POINT('Ctrl Pts',(20.2865695905002,5.93270865498951,-6.24115317001707));
#65860=CARTESIAN_POINT('Ctrl Pts',(20.2795349930202,5.95688158865839,-6.11784437235239));
#65861=CARTESIAN_POINT('Ctrl Pts',(20.2725003955402,5.98646729786239,-5.99578437125368));
#65862=CARTESIAN_POINT('Ctrl Pts',(20.2654696839918,6.01603666383682,-5.87379179644538));
#65863=CARTESIAN_POINT('Ctrl Pts',(20.2584389724434,6.05101276049188,-5.75304701753563));
#65864=CARTESIAN_POINT('Ctrl Pts',(20.2514082608949,6.09126461877634,-5.63404831497107));
#65865=CARTESIAN_POINT('Ctrl Pts',(20.2443792951667,6.13150648198313,-5.5150791613845));
#65866=CARTESIAN_POINT('Ctrl Pts',(20.2373503294385,6.17702137841485,-5.39785558600509));
#65867=CARTESIAN_POINT('Ctrl Pts',(20.2303213637103,6.22762857144207,-5.28286041481675));
#65868=CARTESIAN_POINT('Ctrl Pts',(20.2232935368354,6.27822756494623,-5.167883875477));
#65869=CARTESIAN_POINT('Ctrl Pts',(20.2162657099604,6.33391705385406,-5.05513537191307));
#65870=CARTESIAN_POINT('Ctrl Pts',(20.2092378830855,6.39446848337008,-4.94507699176315));
#65871=CARTESIAN_POINT('Ctrl Pts',(20.202208203391,6.45503587669273,-4.83498959577145));
#65872=CARTESIAN_POINT('Ctrl Pts',(20.1951785236966,6.52046758537476,-4.72759407695164));
#65873=CARTESIAN_POINT('Ctrl Pts',(20.1881488440021,6.59048948921103,-4.62332719868191));
#65874=CARTESIAN_POINT('Ctrl Pts',(20.1845187436921,6.626648538538,-4.56948417260053));
#65875=CARTESIAN_POINT('Ctrl Pts',(20.1808886433821,6.66403091020618,-4.51647499565652));
#65876=CARTESIAN_POINT('Ctrl Pts',(20.177258543072,6.70259439411009,-4.46435669536894));
#65877=CARTESIAN_POINT('Ctrl Pts',(20.1698761111912,6.78101985585918,-4.35836518858973));
#65878=CARTESIAN_POINT('Ctrl Pts',(20.1624936793103,6.86435866190934,-4.25602485199227));
#65879=CARTESIAN_POINT('Ctrl Pts',(20.1551112474295,6.95225090147646,-4.15777249926552));
#65880=CARTESIAN_POINT('Ctrl Pts',(20.1477279447581,7.04015350832238,-4.05950855723876));
#65881=CARTESIAN_POINT('Ctrl Pts',(20.1403446420867,7.13261040743368,-3.96533379717853));
#65882=CARTESIAN_POINT('Ctrl Pts',(20.1329613394153,7.22922309246197,-3.87565001006583));
#65883=CARTESIAN_POINT('Ctrl Pts',(20.125576061468,7.32586162455663,-3.78594222959454));
#65884=CARTESIAN_POINT('Ctrl Pts',(20.1181907835206,7.42665793153525,-3.7007280395822));
#65885=CARTESIAN_POINT('Ctrl Pts',(20.1108055055733,7.53117808025158,-3.62037099649164));
#65886=CARTESIAN_POINT('Ctrl Pts',(20.1034200529725,7.63570070075121,-3.54001205304791));
#65887=CARTESIAN_POINT('Ctrl Pts',(20.0960346003717,7.74394708454327,-3.46451067662804));
#65888=CARTESIAN_POINT('Ctrl Pts',(20.0886491477709,7.855451839869,-3.39418886165612));
#65889=CARTESIAN_POINT('Ctrl Pts',(20.0812627355946,7.96697108276045,-3.32385790992663));
#65890=CARTESIAN_POINT('Ctrl Pts',(20.0738763234183,8.08174927371947,-3.25870803300175));
#65891=CARTESIAN_POINT('Ctrl Pts',(20.066489911242,8.19929334163063,-3.19901706712769));
#65892=CARTESIAN_POINT('Ctrl Pts',(20.0646309068826,8.22887670760733,-3.1839941083316));
#65893=CARTESIAN_POINT('Ctrl Pts',(20.0627719025232,8.25863514608028,-3.16931670369317));
#65894=CARTESIAN_POINT('Ctrl Pts',(20.0609128981638,8.28856055418469,-3.15498882227357));
#65895=CARTESIAN_POINT('Ctrl Pts',(20.0537145950365,8.40443556957037,-3.09950942917227));
#65896=CARTESIAN_POINT('Ctrl Pts',(20.0465162919091,8.52285398389169,-3.04925596260064));
#65897=CARTESIAN_POINT('Ctrl Pts',(20.0393179887818,8.6433237577775,-3.00444632409307));
#65898=CARTESIAN_POINT('Ctrl Pts',(20.032121772119,8.76375861289033,-2.95964967388574));
#65899=CARTESIAN_POINT('Ctrl Pts',(20.0249255554562,8.88624330867259,-2.92029382958354));
#65900=CARTESIAN_POINT('Ctrl Pts',(20.0177293387934,9.01026695320274,-2.88654811782648));
#65901=CARTESIAN_POINT('Ctrl Pts',(20.0105333517354,9.13428664059432,-2.85280348277102));
#65902=CARTESIAN_POINT('Ctrl Pts',(20.0033373646774,9.25984483663122,-2.82466872119205));
#65903=CARTESIAN_POINT('Ctrl Pts',(19.9961413776194,9.38641645673583,-2.80226300874746));
#65904=CARTESIAN_POINT('Ctrl Pts',(19.9889458669186,9.51297969810196,-2.77985877950743));
#65905=CARTESIAN_POINT('Ctrl Pts',(19.9817503562177,9.64055587871207,-2.76318290195909));
#65906=CARTESIAN_POINT('Ctrl Pts',(19.9745548455169,9.76861097645808,-2.75230319906341));
#65907=CARTESIAN_POINT('Ctrl Pts',(19.9673575905949,9.89669711528098,-2.74142085888347));
#65908=CARTESIAN_POINT('Ctrl Pts',(19.960160335673,10.0252620483062,-2.73633752911708));
#65909=CARTESIAN_POINT('Ctrl Pts',(19.9529630807511,10.1537676164009,-2.73706907365435));
#65910=CARTESIAN_POINT('Ctrl Pts',(19.9501644715859,10.2037362314554,-2.73735353033525));
#65911=CARTESIAN_POINT('Ctrl Pts',(19.9473658624208,10.2536958590512,-2.73851663601357));
#65912=CARTESIAN_POINT('Ctrl Pts',(19.9445672532556,10.3036148840483,-2.74055719522461));
#65913=CARTESIAN_POINT('Ctrl Pts',(19.9372997188826,10.4332465005499,-2.74585619673975));
#65914=CARTESIAN_POINT('Ctrl Pts',(19.9300321845096,10.5626553456609,-2.75707812798666));
#65915=CARTESIAN_POINT('Ctrl Pts',(19.9227646501365,10.6912947465663,-2.77417988282387));
#65916=CARTESIAN_POINT('Ctrl Pts',(19.91549833993,10.8199124790436,-2.79127875698733));
#65917=CARTESIAN_POINT('Ctrl Pts',(19.9082320297235,10.9477606866541,-2.81425543359745));
#65918=CARTESIAN_POINT('Ctrl Pts',(19.9009657195169,11.0742992481297,-2.84301510939317));
#65919=CARTESIAN_POINT('Ctrl Pts',(19.8936990472744,11.2008441142512,-2.87177621810837));
#65920=CARTESIAN_POINT('Ctrl Pts',(19.8864323750319,11.3260788692529,-2.90632082903432));
#65921=CARTESIAN_POINT('Ctrl Pts',(19.8791657027894,11.4494746488613,-2.94650324702691));
#65922=CARTESIAN_POINT('Ctrl Pts',(19.8718993416436,11.572865145719,-2.98668394475241));
#65923=CARTESIAN_POINT('Ctrl Pts',(19.8646329804978,11.6944164996854,-3.03250185894799));
#65924=CARTESIAN_POINT('Ctrl Pts',(19.857366619352,11.8136161997892,-3.08376180172764));
#65925=CARTESIAN_POINT('Ctrl Pts',(19.8500988473739,11.9328390436335,-3.13503169710623));
#65926=CARTESIAN_POINT('Ctrl Pts',(19.8428310753959,12.0497090072423,-3.19174559577496));
#65927=CARTESIAN_POINT('Ctrl Pts',(19.8355633034179,12.1637343634684,-3.25366051264916));
#65928=CARTESIAN_POINT('Ctrl Pts',(19.8331160717277,12.2021294130214,-3.27450873781707));
#65929=CARTESIAN_POINT('Ctrl Pts',(19.8306688400376,12.2402021300839,-3.29594627973528));
#65930=CARTESIAN_POINT('Ctrl Pts',(19.8282216083474,12.2779343732715,-3.31796269115241));
#65931=CARTESIAN_POINT('Ctrl Pts',(19.8209722370613,12.3897076236044,-3.3831813385709));
#65932=CARTESIAN_POINT('Ctrl Pts',(19.8137228657752,12.4985292694164,-3.45350511738675));
#65933=CARTESIAN_POINT('Ctrl Pts',(19.8064734944891,12.6039381989666,-3.52864225417559));
#65934=CARTESIAN_POINT('Ctrl Pts',(19.7992255471016,12.7093264244276,-3.60376463276527));
#65935=CARTESIAN_POINT('Ctrl Pts',(19.7919775997141,12.8113029891484,-3.68369828266069));
#65936=CARTESIAN_POINT('Ctrl Pts',(19.7847296523266,12.9094366941866,-3.76810876168227));
#65937=CARTESIAN_POINT('Ctrl Pts',(19.7774814460529,13.007573904419,-3.85252225572431));
#65938=CARTESIAN_POINT('Ctrl Pts',(19.7702332397791,13.1018677159777,-3.94141267555906));
#65939=CARTESIAN_POINT('Ctrl Pts',(19.7629850335054,13.1919206551921,-4.03440583851178));
#65940=CARTESIAN_POINT('Ctrl Pts',(19.7557371455646,13.2819696393849,-4.12739491731172));
#65941=CARTESIAN_POINT('Ctrl Pts',(19.7484892576238,13.3677778844239,-4.22448612893644));
#65942=CARTESIAN_POINT('Ctrl Pts',(19.7412413696829,13.4489855172323,-4.32526919094931));
#65943=CARTESIAN_POINT('Ctrl Pts',(19.7339919237521,13.5302106062536,-4.42607391706597));
#65944=CARTESIAN_POINT('Ctrl Pts',(19.7267424778214,13.6068328911244,-4.53057180878018));
#65945=CARTESIAN_POINT('Ctrl Pts',(19.7194930318906,13.6785332358806,-4.63832007024348));
#65946=CARTESIAN_POINT('Ctrl Pts',(19.7169540090735,13.7036453359045,-4.67605747762233));
#65947=CARTESIAN_POINT('Ctrl Pts',(19.7144149862564,13.7281540642729,-4.71419332453206));
#65948=CARTESIAN_POINT('Ctrl Pts',(19.7118759634392,13.7520469693732,-4.75270775049499));
#65949=CARTESIAN_POINT('Ctrl Pts',(19.7046273193903,13.820258709417,-4.86266240024108));
#65950=CARTESIAN_POINT('Ctrl Pts',(19.6973786753414,13.8834733182431,-4.97574546948885));
#65951=CARTESIAN_POINT('Ctrl Pts',(19.6901300312925,13.9414199126782,-5.09148340868428));
#65952=CARTESIAN_POINT('Ctrl Pts',(19.6828828572101,13.9993547560108,-5.20719787715811));
#65953=CARTESIAN_POINT('Ctrl Pts',(19.6756356831278,14.0520235610632,-5.3255658322583));
#65954=CARTESIAN_POINT('Ctrl Pts',(19.6683885090455,14.0992018473551,-5.44609001447772));
#65955=CARTESIAN_POINT('Ctrl Pts',(19.6611411361963,14.1463814275969,-5.56661750229129));
#65956=CARTESIAN_POINT('Ctrl Pts',(19.6538937633471,14.1880700584847,-5.68930101442326));
#65957=CARTESIAN_POINT('Ctrl Pts',(19.6466463904979,14.2240916631679,-5.81362395847015));
#65958=CARTESIAN_POINT('Ctrl Pts',(19.6393993687001,14.2601115230209,-5.93794088050801));
#65959=CARTESIAN_POINT('Ctrl Pts',(19.6321523469024,14.2904648110072,-6.06389674266133));
#65960=CARTESIAN_POINT('Ctrl Pts',(19.6249053251046,14.3150255733708,-6.19096064702689));
#65961=CARTESIAN_POINT('Ctrl Pts',(19.617656786201,14.3395914773327,-6.31805115120036));
#65962=CARTESIAN_POINT('Ctrl Pts',(19.6104082472974,14.3583623684871,-6.44624982084262));
#65963=CARTESIAN_POINT('Ctrl Pts',(19.6031597083938,14.3712635105564,-6.57501609381955));
#65964=CARTESIAN_POINT('Ctrl Pts',(19.6006165784395,14.3757898407971,-6.62019338682416));
#65965=CARTESIAN_POINT('Ctrl Pts',(19.5980734484853,14.379594106723,-6.66544048851997));
#65966=CARTESIAN_POINT('Ctrl Pts',(19.5955303185311,14.3826745937204,-6.71073390220859));
#65967=CARTESIAN_POINT('Ctrl Pts',(19.5882769321214,14.3914606026636,-6.83991748197387));
#65968=CARTESIAN_POINT('Ctrl Pts',(19.5810235457117,14.3943581882403,-6.96952423534298));
#65969=CARTESIAN_POINT('Ctrl Pts',(19.5737701593021,14.3913501125846,-7.09900817068766));
#65970=CARTESIAN_POINT('Ctrl Pts',(19.5665181595134,14.388342611979,-7.22846735274605));
#65971=CARTESIAN_POINT('Ctrl Pts',(19.5592661597248,14.3794317103126,-7.3578034186612));
#65972=CARTESIAN_POINT('Ctrl Pts',(19.5520141599362,14.364652272981,-7.4864711961294));
#65973=CARTESIAN_POINT('Ctrl Pts',(19.5447618877024,14.3498722804115,-7.6151438074243));
#65974=CARTESIAN_POINT('Ctrl Pts',(19.5375096154687,14.3292233474636,-7.74314773673032));
#65975=CARTESIAN_POINT('Ctrl Pts',(19.5302573432349,14.3027921585418,-7.86994342313364));
#65976=CARTESIAN_POINT('Ctrl Pts',(19.5230053926805,14.2763621419927,-7.99673348543143));
#65977=CARTESIAN_POINT('Ctrl Pts',(19.515753442126,14.2441504547407,-8.12231507444478));
#65978=CARTESIAN_POINT('Ctrl Pts',(19.5085014915715,14.2062947632617,-8.24615948347003));
#65979=CARTESIAN_POINT('Ctrl Pts',(19.5012480222094,14.1684311435003,-8.370029829769));
#65980=CARTESIAN_POINT('Ctrl Pts',(19.4939945528474,14.1249212600331,-8.49216193935917));
#65981=CARTESIAN_POINT('Ctrl Pts',(19.4867410834853,14.0759525550909,-8.6120425647037));
#65982=CARTESIAN_POINT('Ctrl Pts',(19.4842222801979,14.0589479289135,-8.65367170769003));
#65983=CARTESIAN_POINT('Ctrl Pts',(19.4817034769104,14.0412854766061,-8.69502951553451));
#65984=CARTESIAN_POINT('Ctrl Pts',(19.4791846736229,14.0229744084962,-8.73609505223213));
#65985=CARTESIAN_POINT('Ctrl Pts',(19.4719351256642,13.9702720132359,-8.8542887115877));
#65986=CARTESIAN_POINT('Ctrl Pts',(19.4646855777054,13.9121739978676,-8.97010247114962));
#65987=CARTESIAN_POINT('Ctrl Pts',(19.4574360297467,13.8489203073898,-9.08304622535753));
#65988=CARTESIAN_POINT('Ctrl Pts',(19.4501879283525,13.7856792384645,-9.19596744292739));
#65989=CARTESIAN_POINT('Ctrl Pts',(19.4429398269584,13.7172847155392,-9.30601949578961));
#65990=CARTESIAN_POINT('Ctrl Pts',(19.4356917255643,13.6440223508725,-9.41273737593164));
#65991=CARTESIAN_POINT('Ctrl Pts',(19.428443400293,13.5707577233001,-9.5194585523432));
#65992=CARTESIAN_POINT('Ctrl Pts',(19.4211950750217,13.492625146295,-9.62284506291008));
#65993=CARTESIAN_POINT('Ctrl Pts',(19.4139467497504,13.4099534015183,-9.72246110724593));
#65994=CARTESIAN_POINT('Ctrl Pts',(19.4066987635179,13.3272855236945,-9.82207249206305));
#65995=CARTESIAN_POINT('Ctrl Pts',(19.3994507772854,13.2400791250862,-9.91791349828917));
#65996=CARTESIAN_POINT('Ctrl Pts',(19.3922027910529,13.1487029610089,-10.0095817782933));
#65997=CARTESIAN_POINT('Ctrl Pts',(19.384953278128,13.0573075497507,-10.1012693670086));
#65998=CARTESIAN_POINT('Ctrl Pts',(19.3777037652031,12.961740863451,-10.1887822292906));
#65999=CARTESIAN_POINT('Ctrl Pts',(19.3704542522781,12.8624084057092,-10.2717549795185));
#66000=CARTESIAN_POINT('Ctrl Pts',(19.3679158444237,12.8276272702665,-10.3008077839022));
#66001=CARTESIAN_POINT('Ctrl Pts',(19.3653774365692,12.792384745242,-10.3293043021381));
#66002=CARTESIAN_POINT('Ctrl Pts',(19.3628390287147,12.7566992070898,-10.3572300079481));
#66003=CARTESIAN_POINT('Ctrl Pts',(19.355587325406,12.6547530463751,-10.4370079415306));
#66004=CARTESIAN_POINT('Ctrl Pts',(19.3483356220973,12.5491521538965,-10.5121531526707));
#66005=CARTESIAN_POINT('Ctrl Pts',(19.3410839187886,12.4403383965228,-10.582344889197));
#66006=CARTESIAN_POINT('Ctrl Pts',(19.3338336305964,12.3315458733526,-10.6525229283228));
#66007=CARTESIAN_POINT('Ctrl Pts',(19.3265833424042,12.2195420262118,-10.7177492338765));
#66008=CARTESIAN_POINT('Ctrl Pts',(19.319333054212,12.1047973069638,-10.7777466232003));
#66009=CARTESIAN_POINT('Ctrl Pts',(19.3120825180557,11.9900486633794,-10.8377460644699));
#66010=CARTESIAN_POINT('Ctrl Pts',(19.3048319818994,11.8725592649077,-10.8925160688187));
#66011=CARTESIAN_POINT('Ctrl Pts',(19.2975814457431,11.7528240201902,-10.9418254813568));
#66012=CARTESIAN_POINT('Ctrl Pts',(19.2903312406935,11.6330942433642,-10.9911326421057));
#66013=CARTESIAN_POINT('Ctrl Pts',(19.283081035644,11.5111191456424,-11.0349795799072));
#66014=CARTESIAN_POINT('Ctrl Pts',(19.2758308305944,11.3874132828957,-11.0731834199695));
#66015=CARTESIAN_POINT('Ctrl Pts',(19.2685791058577,11.2636814906467,-11.1113952677894));
#66016=CARTESIAN_POINT('Ctrl Pts',(19.2613273811211,11.1382185391783,-11.1439615539113));
#66017=CARTESIAN_POINT('Ctrl Pts',(19.2540756563844,11.0115541411716,-11.1707492722582));
#66018=CARTESIAN_POINT('Ctrl Pts',(19.2515482321917,10.9674081379115,-11.1800855239602));
#66019=CARTESIAN_POINT('Ctrl Pts',(19.2490208079991,10.9231163019457,-11.1887202965382));
#66020=CARTESIAN_POINT('Ctrl Pts',(19.2464933838065,10.8787013672108,-11.1966494148749));
#66021=CARTESIAN_POINT('Ctrl Pts',(19.2390336219372,10.7476094683813,-11.2200524252586));
#66022=CARTESIAN_POINT('Ctrl Pts',(19.231573860068,10.6154089528811,-11.2373107444924));
#66023=CARTESIAN_POINT('Ctrl Pts',(19.2241140981988,10.4826720229851,-11.2483453864041));
#66024=CARTESIAN_POINT('Ctrl Pts',(19.2175155086208,10.3652585535498,-11.2581061635431));
#66025=CARTESIAN_POINT('Ctrl Pts',(19.2109169190427,10.2474256436952,-11.2629979845103));
#66026=CARTESIAN_POINT('Ctrl Pts',(19.2043183294647,10.1295728822702,-11.262999999377));
#66027=CARTESIAN_POINT('Ctrl Pts',(19.2043183294109,10.1295728813087,-11.262999999377));
#66028=CARTESIAN_POINT('Ctrl Pts',(19.1970583189289,9.99990694692026,-11.2630022161781));
#66029=CARTESIAN_POINT('Ctrl Pts',(19.1897983084469,9.87023735638593,-11.2570840955062));
#66030=CARTESIAN_POINT('Ctrl Pts',(19.1825382979649,9.7411112248888,-11.2452706815193));
#66031=CARTESIAN_POINT('Ctrl Pts',(19.1752785223053,9.61198926992911,-11.233457649633));
#66032=CARTESIAN_POINT('Ctrl Pts',(19.1680187466457,9.48341108082839,-11.215749739548));
#66033=CARTESIAN_POINT('Ctrl Pts',(19.1607589709861,9.35591875974781,-11.1922238805591));
#66034=CARTESIAN_POINT('Ctrl Pts',(19.1534975256724,9.22839711708991,-11.1686926109282));
#66035=CARTESIAN_POINT('Ctrl Pts',(19.1462360803587,9.1019621791951,-11.1393407825559));
#66036=CARTESIAN_POINT('Ctrl Pts',(19.138974635045,8.97714636126784,-11.1042965403709));
#66037=CARTESIAN_POINT('Ctrl Pts',(19.1360323363295,8.92657166092885,-11.090096801295));
#66038=CARTESIAN_POINT('Ctrl Pts',(19.1330900376139,8.87626264874846,-11.0749630455192));
#66039=CARTESIAN_POINT('Ctrl Pts',(19.1301477388984,8.82625408154575,-11.0589061427966));
#66040=CARTESIAN_POINT('Ctrl Pts',(19.1264842468684,8.76398780436326,-11.0389134973053));
#66041=CARTESIAN_POINT('Ctrl Pts',(19.1228207548385,8.70217597612885,-11.0174859478408));
#66042=CARTESIAN_POINT('Ctrl Pts',(19.1191572628085,8.64088535679774,-10.9946458471364));
#66043=CARTESIAN_POINT('Origin',(23.734,10.1295,-7.));
#66044=CARTESIAN_POINT('',(17.734,8.64088535679774,-10.9946458471364));
#66045=CARTESIAN_POINT('',(18.0286142064722,8.64088528410776,-10.9946458200483));
#66046=CARTESIAN_POINT('',(23.734,8.64088535679774,-10.9946458471364));
#66047=CARTESIAN_POINT('',(17.7339050262067,5.86731958600617,-6.91641101407839));
#66048=CARTESIAN_POINT('Origin',(17.734,10.1295,-7.));
#66049=CARTESIAN_POINT('Ctrl Pts',(17.7339050262067,5.86731958600617,-6.91641101407839));
#66050=CARTESIAN_POINT('Ctrl Pts',(17.7472545315539,5.86268934162998,-7.15250595738485));
#66051=CARTESIAN_POINT('Ctrl Pts',(17.7606088204071,5.87768407296756,-7.38858354784552));
#66052=CARTESIAN_POINT('Ctrl Pts',(17.7867512045192,5.94579532231527,-7.8502465191533));
#66053=CARTESIAN_POINT('Ctrl Pts',(17.7995044918489,5.99788017560926,-8.07518560832005));
#66054=CARTESIAN_POINT('Ctrl Pts',(17.8350441223152,6.19253199136132,-8.68577563313481));
#66055=CARTESIAN_POINT('Ctrl Pts',(17.8582714071464,6.37296588560031,-9.05669361479852));
#66056=CARTESIAN_POINT('Ctrl Pts',(17.8967465912778,6.75751592584523,-9.62257240524602));
#66057=CARTESIAN_POINT('Ctrl Pts',(17.9119120419527,6.93290530427956,-9.8337166577424));
#66058=CARTESIAN_POINT('Ctrl Pts',(17.9585433380038,7.53005115412866,-10.4260456333765));
#66059=CARTESIAN_POINT('Ctrl Pts',(17.9907102178401,8.00846843554533,-10.7411421365182));
#66060=CARTESIAN_POINT('Ctrl Pts',(18.0243885125157,8.5697845022952,-10.9676068626257));
#66061=CARTESIAN_POINT('Ctrl Pts',(18.0265024679027,8.60524950852272,-10.9813660595043));
#66062=CARTESIAN_POINT('Ctrl Pts',(18.0286142064722,8.64088528410776,-10.9946458200483));
#66063=CARTESIAN_POINT('Origin',(-23.734,10.1295,-7.));
#66064=CARTESIAN_POINT('',(-18.0286142198359,11.618114722277,-10.994645817669));
#66065=CARTESIAN_POINT('',(-17.734,11.6181146495903,-10.9946458447559));
#66066=CARTESIAN_POINT('',(-23.734,11.6181146495903,-10.9946458447559));
#66067=CARTESIAN_POINT('',(-17.7339050342228,14.3916804139849,-6.91641101362462));
#66068=CARTESIAN_POINT('Origin',(-17.734,10.1295,-7.));
#66069=CARTESIAN_POINT('Ctrl Pts',(-17.7339050342228,14.3916804139849,-6.91641101362462));
#66070=CARTESIAN_POINT('Ctrl Pts',(-17.7472546703102,14.3963107039188,-7.15250827862387));
#66071=CARTESIAN_POINT('Ctrl Pts',(-17.7606090905621,14.3813156320825,-7.38858818646879));
#66072=CARTESIAN_POINT('Ctrl Pts',(-17.7867517208388,14.3132029843049,-7.85025542053381));
#66073=CARTESIAN_POINT('Ctrl Pts',(-17.799505122171,14.261117122435,-8.07519644101184));
#66074=CARTESIAN_POINT('Ctrl Pts',(-17.8350446877022,14.0664638141747,-8.68578459435684));
#66075=CARTESIAN_POINT('Ctrl Pts',(-17.8582717904186,13.8860307362702,-9.05669910101929));
#66076=CARTESIAN_POINT('Ctrl Pts',(-17.8967467678593,13.5014823080873,-9.62257466023843));
#66077=CARTESIAN_POINT('Ctrl Pts',(-17.9119122070986,13.3260928888101,-9.83371868146643));
#66078=CARTESIAN_POINT('Ctrl Pts',(-17.9585434935157,12.7289467612535,-10.4260472219077));
#66079=CARTESIAN_POINT('Ctrl Pts',(-17.990710378402,12.2505292507666,-10.7411434545049));
#66080=CARTESIAN_POINT('Ctrl Pts',(-18.024388625212,11.6892138344056,-10.9676075078961));
#66081=CARTESIAN_POINT('Ctrl Pts',(-18.0265025308825,11.6537496589754,-10.9813663696733));
#66082=CARTESIAN_POINT('Ctrl Pts',(-18.0286142198359,11.618114722277,-10.994645817669));
#66083=CARTESIAN_POINT('Origin',(-23.734,10.1295,-7.));
#66084=CARTESIAN_POINT('',(-19.5287463281039,11.618114650837,-10.9946458442913));
#66085=CARTESIAN_POINT('',(-19.1191572624809,11.6181146495903,-10.9946458447559));
#66086=CARTESIAN_POINT('',(-23.734,11.6181146495903,-10.9946458447559));
#66087=CARTESIAN_POINT('',(-17.734,9.60084442449481,-11.2300936493755));
#66088=CARTESIAN_POINT('Ctrl Pts',(-19.1191572624809,11.6181146495903,-10.9946458447559));
#66089=CARTESIAN_POINT('Ctrl Pts',(-19.1119070028363,11.7394122804076,-10.9494439827604));
#66090=CARTESIAN_POINT('Ctrl Pts',(-19.1046567431916,11.8586672520018,-10.898706644448));
#66091=CARTESIAN_POINT('Ctrl Pts',(-19.097406483547,11.9753756588468,-10.8426438882723));
#66092=CARTESIAN_POINT('Ctrl Pts',(-19.0901561762952,12.0920848320306,-10.7865807639736));
#66093=CARTESIAN_POINT('Ctrl Pts',(-19.0829058690433,12.2062470931261,-10.7251922967873));
#66094=CARTESIAN_POINT('Ctrl Pts',(-19.0756555617915,12.3173806376937,-10.658735753673));
#66095=CARTESIAN_POINT('Ctrl Pts',(-19.0684059351248,12.4285037501756,-10.5922854488224));
#66096=CARTESIAN_POINT('Ctrl Pts',(-19.061156308458,12.5365984180107,-10.5207681969686));
#66097=CARTESIAN_POINT('Ctrl Pts',(-19.0539066817912,12.6412096611553,-10.444485967174));
#66098=CARTESIAN_POINT('Ctrl Pts',(-19.0466552548783,12.7458468816354,-10.3681847947783));
#66099=CARTESIAN_POINT('Ctrl Pts',(-19.0394038279654,12.8469986686003,-10.2871164827276));
#66100=CARTESIAN_POINT('Ctrl Pts',(-19.0321524010525,12.9442407270079,-10.2016251560298));
#66101=CARTESIAN_POINT('Ctrl Pts',(-19.0260356320317,13.0262669568152,-10.1295109769896));
#66102=CARTESIAN_POINT('Ctrl Pts',(-19.0199188630109,13.1055117254018,-10.054250454771));
#66103=CARTESIAN_POINT('Ctrl Pts',(-19.0138020939901,13.1817396470563,-9.97607159472646));
#66104=CARTESIAN_POINT('Ctrl Pts',(-19.006551083536,13.2721026238059,-9.88339591422544));
#66105=CARTESIAN_POINT('Ctrl Pts',(-18.999300073082,13.3582578890542,-9.7865849347629));
#66106=CARTESIAN_POINT('Ctrl Pts',(-18.9920490626279,13.4398386609267,-9.68604299108816));
#66107=CARTESIAN_POINT('Ctrl Pts',(-18.9847994767659,13.5214034047821,-9.58552080069554));
#66108=CARTESIAN_POINT('Ctrl Pts',(-18.9775498909039,13.598395230372,-9.48126937662048));
#66109=CARTESIAN_POINT('Ctrl Pts',(-18.9703003050419,13.670487562286,-9.37372620235276));
#66110=CARTESIAN_POINT('Ctrl Pts',(-18.9630504780159,13.7425822924159,-9.26617945056504));
#66111=CARTESIAN_POINT('Ctrl Pts',(-18.9558006509899,13.8097770076549,-9.15534101487568));
#66112=CARTESIAN_POINT('Ctrl Pts',(-18.9485508239639,13.871788232083,-9.04167768955162));
#66113=CARTESIAN_POINT('Ctrl Pts',(-18.9413013300434,13.9337966073018,-8.92801958667901));
#66114=CARTESIAN_POINT('Ctrl Pts',(-18.9340518361228,13.9906218040944,-8.81153715811386));
#66115=CARTESIAN_POINT('Ctrl Pts',(-18.9268023422023,14.0420262078369,-8.69272197155634));
#66116=CARTESIAN_POINT('Ctrl Pts',(-18.9195513255415,14.0934414089613,-8.57388182813012));
#66117=CARTESIAN_POINT('Ctrl Pts',(-18.9123003088806,14.1394334060361,-8.45270826559124));
#66118=CARTESIAN_POINT('Ctrl Pts',(-18.9050492922198,14.179812512944,-8.32971333282391));
#66119=CARTESIAN_POINT('Ctrl Pts',(-18.9025183445072,14.1939067307684,-8.28678228490142));
#66120=CARTESIAN_POINT('Ctrl Pts',(-18.8999873967946,14.2073175453242,-8.24362948941841));
#66121=CARTESIAN_POINT('Ctrl Pts',(-18.8974564490819,14.2200383107599,-8.20027718807187));
#66122=CARTESIAN_POINT('Ctrl Pts',(-18.8902054209966,14.2564826145993,-8.07607519327786));
#66123=CARTESIAN_POINT('Ctrl Pts',(-18.8829543929113,14.2872725593705,-7.95018973113526));
#66124=CARTESIAN_POINT('Ctrl Pts',(-18.8757033648259,14.3122734063533,-7.8231498229993));
#66125=CARTESIAN_POINT('Ctrl Pts',(-18.8684537617915,14.3372693398978,-7.69613488212714));
#66126=CARTESIAN_POINT('Ctrl Pts',(-18.861204158757,14.3564783785018,-7.56796628686594));
#66127=CARTESIAN_POINT('Ctrl Pts',(-18.8539545557225,14.369816831984,-7.43918352017531));
#66128=CARTESIAN_POINT('Ctrl Pts',(-18.8467047123714,14.3831557276218,-7.31039648447218));
#66129=CARTESIAN_POINT('Ctrl Pts',(-18.8394548690202,14.3906236100164,-7.18099558012911));
#66130=CARTESIAN_POINT('Ctrl Pts',(-18.8322050256691,14.3921885964997,-7.05152600577627));
#66131=CARTESIAN_POINT('Ctrl Pts',(-18.8249555159603,14.3937535109613,-6.92206238969404));
#66132=CARTESIAN_POINT('Ctrl Pts',(-18.8177060062514,14.3894160704854,-6.79253045561143));
#66133=CARTESIAN_POINT('Ctrl Pts',(-18.8104564965426,14.379196515432,-6.66347581554241));
#66134=CARTESIAN_POINT('Ctrl Pts',(-18.8032054650126,14.3689748150839,-6.53439408425104));
#66135=CARTESIAN_POINT('Ctrl Pts',(-18.7959544334827,14.3528685617423,-6.40579019172858));
#66136=CARTESIAN_POINT('Ctrl Pts',(-18.7887034019527,14.3309499353665,-6.27820540275729));
#66137=CARTESIAN_POINT('Ctrl Pts',(-18.7861725360264,14.3232995611519,-6.23367380835046));
#66138=CARTESIAN_POINT('Ctrl Pts',(-18.7836416701,14.3149415512132,-6.1892663009137));
#66139=CARTESIAN_POINT('Ctrl Pts',(-18.7811108041737,14.3058804482948,-6.14500564264953));
#66140=CARTESIAN_POINT('Ctrl Pts',(-18.7738598726569,14.2799203861494,-6.01819884556579));
#66141=CARTESIAN_POINT('Ctrl Pts',(-18.76660894114,14.2481760638575,-5.89255238081223));
#66142=CARTESIAN_POINT('Ctrl Pts',(-18.7593580096232,14.2107761567794,-5.76859676299603));
#66143=CARTESIAN_POINT('Ctrl Pts',(-18.7521085029907,14.1733835991768,-5.64466550376387));
#66144=CARTESIAN_POINT('Ctrl Pts',(-18.7448589963582,14.1303377735899,-5.52242475946198));
#66145=CARTESIAN_POINT('Ctrl Pts',(-18.7376094897257,14.0818173597769,-5.40239038322671));
#66146=CARTESIAN_POINT('Ctrl Pts',(-18.7303597415627,14.0332953294174,-5.2823520078264));
#66147=CARTESIAN_POINT('Ctrl Pts',(-18.7231099933996,13.9792984725236,-5.16452046926666));
#66148=CARTESIAN_POINT('Ctrl Pts',(-18.7158602452366,13.9200539214188,-5.04939241034578));
#66149=CARTESIAN_POINT('Ctrl Pts',(-18.7086108297512,13.860812088938,-4.93426963444092));
#66150=CARTESIAN_POINT('Ctrl Pts',(-18.7013614142658,13.7963232036895,-4.82185039661095));
#66151=CARTESIAN_POINT('Ctrl Pts',(-18.6941119987804,13.7268606462205,-4.71260729628162));
#66152=CARTESIAN_POINT('Ctrl Pts',(-18.6868610592732,13.6573834858556,-4.60334123011747));
#66153=CARTESIAN_POINT('Ctrl Pts',(-18.6796101197659,13.5829307508601,-4.4972529265802));
#66154=CARTESIAN_POINT('Ctrl Pts',(-18.6723591802586,13.5038196785847,-4.39478682125318));
#66155=CARTESIAN_POINT('Ctrl Pts',(-18.6698278399276,13.4762015957584,-4.35901537608866));
#66156=CARTESIAN_POINT('Ctrl Pts',(-18.6672964995966,13.448016156806,-4.32368511023057));
#66157=CARTESIAN_POINT('Ctrl Pts',(-18.6647651592655,13.4192780434162,-4.28881401872603));
#66158=CARTESIAN_POINT('Ctrl Pts',(-18.6575139795992,13.3369559546373,-4.18892363790238));
#66159=CARTESIAN_POINT('Ctrl Pts',(-18.650262799933,13.2500660974698,-4.09276745063653));
#66160=CARTESIAN_POINT('Ctrl Pts',(-18.6430116202667,13.1589706262765,-4.00075397399144));
#66161=CARTESIAN_POINT('Ctrl Pts',(-18.6357618651641,13.0678930516613,-3.9087585742755));
#66162=CARTESIAN_POINT('Ctrl Pts',(-18.6285121100615,12.9726117542656,-3.82090450717327));
#66163=CARTESIAN_POINT('Ctrl Pts',(-18.621262354959,12.8735262051464,-3.73756391856177));
#66164=CARTESIAN_POINT('Ctrl Pts',(-18.6140123603528,12.7744373826274,-3.65422057670254));
#66165=CARTESIAN_POINT('Ctrl Pts',(-18.6067623657466,12.671544319424,-3.57539123658429));
#66166=CARTESIAN_POINT('Ctrl Pts',(-18.5995123711404,12.565280302068,-3.50140838049687));
#66167=CARTESIAN_POINT('Ctrl Pts',(-18.5922627110611,12.4590211879107,-3.42742893810165));
#66168=CARTESIAN_POINT('Ctrl Pts',(-18.5850130509817,12.3493917154141,-3.35829572848366));
#66169=CARTESIAN_POINT('Ctrl Pts',(-18.5777633909024,12.2368547762457,-3.29429833269943));
#66170=CARTESIAN_POINT('Ctrl Pts',(-18.5705122115537,12.1242942533625,-3.23028752535143));
#66171=CARTESIAN_POINT('Ctrl Pts',(-18.5632610322051,12.0088253476332,-3.17141485196072));
#66172=CARTESIAN_POINT('Ctrl Pts',(-18.5560098528564,11.8909365133965,-3.11792447146199));
#66173=CARTESIAN_POINT('Ctrl Pts',(-18.5534797400234,11.8498022319187,-3.0992603767491));
#66174=CARTESIAN_POINT('Ctrl Pts',(-18.5509496271904,11.8083735322816,-3.08125114867534));
#66175=CARTESIAN_POINT('Ctrl Pts',(-18.5484195143573,11.7666717816433,-3.06390579922293));
#66176=CARTESIAN_POINT('Ctrl Pts',(-18.5411687398128,11.6471632806606,-3.01419765315347));
#66177=CARTESIAN_POINT('Ctrl Pts',(-18.5339179652682,11.5253676687474,-2.96992735828438));
#66178=CARTESIAN_POINT('Ctrl Pts',(-18.5266671907236,11.4017961818643,-2.93128626890347));
#66179=CARTESIAN_POINT('Ctrl Pts',(-18.5194178411145,11.2782489794753,-2.89265277333995));
#66180=CARTESIAN_POINT('Ctrl Pts',(-18.5121684915053,11.1529269281156,-2.85964637962311));
#66181=CARTESIAN_POINT('Ctrl Pts',(-18.5049191418962,11.0263572046861,-2.83240883070295));
#66182=CARTESIAN_POINT('Ctrl Pts',(-18.4976695492601,10.8997832381373,-2.80517036867211));
#66183=CARTESIAN_POINT('Ctrl Pts',(-18.490419956624,10.7719618531677,-2.78370121420388));
#66184=CARTESIAN_POINT('Ctrl Pts',(-18.4831703639879,10.6434315319627,-2.76809222921216));
#66185=CARTESIAN_POINT('Ctrl Pts',(-18.4759211027388,10.5149070860224,-2.75248395772461));
#66186=CARTESIAN_POINT('Ctrl Pts',(-18.4686718414897,10.3856741121022,-2.74273535980208));
#66187=CARTESIAN_POINT('Ctrl Pts',(-18.4614225802406,10.2562771601344,-2.73888552704011));
#66188=CARTESIAN_POINT('Ctrl Pts',(-18.4541717917954,10.1268529482137,-2.73503488323693));
#66189=CARTESIAN_POINT('Ctrl Pts',(-18.4469210033502,9.99726503491748,-2.73708549638287));
#66190=CARTESIAN_POINT('Ctrl Pts',(-18.439670214905,9.86805928547783,-2.74502435344336));
#66191=CARTESIAN_POINT('Ctrl Pts',(-18.4371380997531,9.82293814612162,-2.74779675542476));
#66192=CARTESIAN_POINT('Ctrl Pts',(-18.4346059846011,9.77786359757213,-2.75128678775841));
#66193=CARTESIAN_POINT('Ctrl Pts',(-18.4320738694491,9.73285879557307,-2.75549240135552));
#66194=CARTESIAN_POINT('Ctrl Pts',(-18.4248227518998,9.60398033231389,-2.76753584990727));
#66195=CARTESIAN_POINT('Ctrl Pts',(-18.4175716343504,9.47562755644352,-2.78545561278176));
#66196=CARTESIAN_POINT('Ctrl Pts',(-18.410320516801,9.34834184038334,-2.80918135328379));
#66197=CARTESIAN_POINT('Ctrl Pts',(-18.4030708252718,9.22108115660127,-2.83290242783151));
#66198=CARTESIAN_POINT('Ctrl Pts',(-18.3958211337425,9.09488745366868,-2.86242713899534));
#66199=CARTESIAN_POINT('Ctrl Pts',(-18.3885714422132,8.97029295673026,-2.89763384973576));
#66200=CARTESIAN_POINT('Ctrl Pts',(-18.3813215126581,8.84569436903645,-2.93284171640238));
#66201=CARTESIAN_POINT('Ctrl Pts',(-18.3740715831029,8.72269542589954,-2.97373186495665));
#66202=CARTESIAN_POINT('Ctrl Pts',(-18.3668216535478,8.60181451476024,-3.02013240695274));
#66203=CARTESIAN_POINT('Ctrl Pts',(-18.3595720591937,8.48093919255952,-3.06653080361607));
#66204=CARTESIAN_POINT('Ctrl Pts',(-18.3523224648397,8.36218202856164,-3.11843895858724));
#66205=CARTESIAN_POINT('Ctrl Pts',(-18.3450728704856,8.24604252945651,-3.17563639847701));
#66206=CARTESIAN_POINT('Ctrl Pts',(-18.3378217572843,8.1298786982106,-3.23284582168142));
#66207=CARTESIAN_POINT('Ctrl Pts',(-18.3305706440831,8.01633393716156,-3.29534658989738));
#66208=CARTESIAN_POINT('Ctrl Pts',(-18.3233195308819,7.90588451646996,-3.36287157479895));
#66209=CARTESIAN_POINT('Ctrl Pts',(-18.3207890954349,7.8673407616755,-3.38643590355911));
#66210=CARTESIAN_POINT('Ctrl Pts',(-18.3182586599879,7.82917373057229,-3.41061168551164));
#66211=CARTESIAN_POINT('Ctrl Pts',(-18.3157282245409,7.79140288446141,-3.43538629325559));
#66212=CARTESIAN_POINT('Ctrl Pts',(-18.3084765678271,7.68316016674423,-3.50638472587502));
#66213=CARTESIAN_POINT('Ctrl Pts',(-18.3012249111132,7.57813431895171,-3.58232985338498));
#66214=CARTESIAN_POINT('Ctrl Pts',(-18.2939732543993,7.47677079571313,-3.66290593948514));
#66215=CARTESIAN_POINT('Ctrl Pts',(-18.2867230174911,7.37542711849153,-3.74346624955146));
#66216=CARTESIAN_POINT('Ctrl Pts',(-18.2794727805829,7.27774460581844,-3.82865549458475));
#66217=CARTESIAN_POINT('Ctrl Pts',(-18.2722225436747,7.18413660431221,-3.91811689589912));
#66218=CARTESIAN_POINT('Ctrl Pts',(-18.2649720651783,7.09052548365482,-4.00758127819406));
#66219=CARTESIAN_POINT('Ctrl Pts',(-18.2577215866819,7.00098939780611,-4.10131786511218));
#66220=CARTESIAN_POINT('Ctrl Pts',(-18.2504711081855,6.91590593318733,-4.19893195838688));
#66221=CARTESIAN_POINT('Ctrl Pts',(-18.2432209643435,6.8308263956953,-4.296541546169));
#66222=CARTESIAN_POINT('Ctrl Pts',(-18.2359708205014,6.75019929407812,-4.39802802065957));
#66223=CARTESIAN_POINT('Ctrl Pts',(-18.2287206766593,6.67436277978478,-4.5029625975001));
#66224=CARTESIAN_POINT('Ctrl Pts',(-18.2214690178202,6.5985104186205,-4.6079191015707));
#66225=CARTESIAN_POINT('Ctrl Pts',(-18.2142173589811,6.52745084621281,-4.71632486665446));
#66226=CARTESIAN_POINT('Ctrl Pts',(-18.206965700142,6.46147983464391,-4.82772076690378));
#66227=CARTESIAN_POINT('Ctrl Pts',(-18.2044379933056,6.43848435448568,-4.86654997617272));
#66228=CARTESIAN_POINT('Ctrl Pts',(-18.2019102864692,6.41610674542311,-4.90574224142944));
#66229=CARTESIAN_POINT('Ctrl Pts',(-18.1993825796327,6.39435825302684,-4.94527735934548));
#66230=CARTESIAN_POINT('Ctrl Pts',(-18.1921344615983,6.33199515075258,-5.05864303808309));
#66231=CARTESIAN_POINT('Ctrl Pts',(-18.1848863435638,6.27478555423617,-5.17487082656046));
#66232=CARTESIAN_POINT('Ctrl Pts',(-18.1776382255294,6.22297508950893,-5.29347366744233));
#66233=CARTESIAN_POINT('Ctrl Pts',(-18.1703915452606,6.17117490211235,-5.41205298179112));
#66234=CARTESIAN_POINT('Ctrl Pts',(-18.1631448649917,6.12477184866148,-5.53300609161682));
#66235=CARTESIAN_POINT('Ctrl Pts',(-18.1558981847229,6.08396397100318,-5.65582469964344));
#66236=CARTESIAN_POINT('Ctrl Pts',(-18.1486512534106,6.04315467965562,-5.77864756242078));
#66237=CARTESIAN_POINT('Ctrl Pts',(-18.1414043220982,6.00794106410452,-5.90333572510643));
#66238=CARTESIAN_POINT('Ctrl Pts',(-18.1341573907859,5.97847181466648,-6.02936412359387));
#66239=CARTESIAN_POINT('Ctrl Pts',(-18.126910778967,5.94900386443136,-6.15538696590101));
#66240=CARTESIAN_POINT('Ctrl Pts',(-18.1196641671482,5.92527985076615,-6.28274958823024));
#66241=CARTESIAN_POINT('Ctrl Pts',(-18.1124175553294,5.90739765777448,-6.4109152762346));
#66242=CARTESIAN_POINT('Ctrl Pts',(-18.1051693767042,5.88951159843356,-6.53910867523119));
#66243=CARTESIAN_POINT('Ctrl Pts',(-18.0979211980791,5.87746992980869,-6.66810514361617));
#66244=CARTESIAN_POINT('Ctrl Pts',(-18.090673019454,5.87131888145374,-6.79736100657538));
#66245=CARTESIAN_POINT('Ctrl Pts',(-18.0881276578775,5.86915880194306,-6.8427521212444));
#66246=CARTESIAN_POINT('Ctrl Pts',(-18.085582296301,5.8677246979414,-6.88817518983173));
#66247=CARTESIAN_POINT('Ctrl Pts',(-18.0830369347245,5.86701704802671,-6.93360659568108));
#66248=CARTESIAN_POINT('Ctrl Pts',(-18.075778159349,5.86499899612295,-7.06316633017908));
#66249=CARTESIAN_POINT('Ctrl Pts',(-18.0685193839736,5.86889196438214,-7.19284036543872));
#66250=CARTESIAN_POINT('Ctrl Pts',(-18.0612606085981,5.87868451109096,-7.32208178969175));
#66251=CARTESIAN_POINT('Ctrl Pts',(-18.0540032283321,5.8884751757089,-7.45129837422593));
#66252=CARTESIAN_POINT('Ctrl Pts',(-18.0467458480661,5.90416313081031,-7.58008217059496));
#66253=CARTESIAN_POINT('Ctrl Pts',(-18.0394884678001,5.92568494599538,-7.70788981609017));
#66254=CARTESIAN_POINT('Ctrl Pts',(-18.0322308822655,5.94720736990625,-7.83570107651326));
#66255=CARTESIAN_POINT('Ctrl Pts',(-18.0249732967308,5.97456393001379,-7.96253579089963));
#66256=CARTESIAN_POINT('Ctrl Pts',(-18.0177157111962,6.00763974228285,-8.08785891357838));
#66257=CARTESIAN_POINT('Ctrl Pts',(-18.0104585011979,6.04071384307759,-8.21317555153937));
#66258=CARTESIAN_POINT('Ctrl Pts',(-18.0032012911997,6.07950651480405,-8.33698042184617));
#66259=CARTESIAN_POINT('Ctrl Pts',(-17.9959440812014,6.12385252539537,-8.45875196973082));
#66260=CARTESIAN_POINT('Ctrl Pts',(-17.9886854754884,6.16820706466122,-8.58054693685623));
#66261=CARTESIAN_POINT('Ctrl Pts',(-17.9814268697753,6.21811695780158,-8.70030747718995));
#66262=CARTESIAN_POINT('Ctrl Pts',(-17.9741682640623,6.27336806870438,-8.81753006259657));
#66263=CARTESIAN_POINT('Ctrl Pts',(-17.9716759393136,6.29233916543256,-8.85777976925658));
#66264=CARTESIAN_POINT('Ctrl Pts',(-17.969183614565,6.31193956155937,-8.89773043939557));
#66265=CARTESIAN_POINT('Ctrl Pts',(-17.9666912898163,6.33215930540418,-8.93736229166527));
#66266=CARTESIAN_POINT('Ctrl Pts',(-17.9594570419305,6.39084934539216,-9.05239812062335));
#66267=CARTESIAN_POINT('Ctrl Pts',(-17.9522227940446,6.45478200713309,-9.1647874961122));
#66268=CARTESIAN_POINT('Ctrl Pts',(-17.9449885461588,6.52369336922076,-9.27405530746912));
#66269=CARTESIAN_POINT('Ctrl Pts',(-17.9377557403836,6.59259099417794,-9.38330133684209));
#66270=CARTESIAN_POINT('Ctrl Pts',(-17.9305229346084,6.66646515380628,-9.48942674829286));
#66271=CARTESIAN_POINT('Ctrl Pts',(-17.9232901288331,6.74500762221501,-9.59198386274208));
#66272=CARTESIAN_POINT('Ctrl Pts',(-17.9160569412351,6.82355423691301,-9.69454639122362));
#66273=CARTESIAN_POINT('Ctrl Pts',(-17.9088237536371,6.90676944361806,-9.79353996699944));
#66274=CARTESIAN_POINT('Ctrl Pts',(-17.9015905660391,6.99430342483591,-9.88854832659579));
#66275=CARTESIAN_POINT('Ctrl Pts',(-17.8943575860858,7.08183489319576,-9.98355395876547));
#66276=CARTESIAN_POINT('Ctrl Pts',(-17.8871246061326,7.17368464971698,-10.0745743487264));
#66277=CARTESIAN_POINT('Ctrl Pts',(-17.8798916261793,7.26946473159495,-10.1612287584861));
#66278=CARTESIAN_POINT('Ctrl Pts',(-17.8726568022711,7.36526923137027,-10.2479052596705));
#66279=CARTESIAN_POINT('Ctrl Pts',(-17.8654219783628,7.46500579836938,-10.3302133240362));
#66280=CARTESIAN_POINT('Ctrl Pts',(-17.8581871544545,7.56825173400053,-10.4078110745631));
#66281=CARTESIAN_POINT('Ctrl Pts',(-17.8555733179391,7.60555298694718,-10.4358460117526));
#66282=CARTESIAN_POINT('Ctrl Pts',(-17.8529594814236,7.64331200171484,-10.4632665119052));
#66283=CARTESIAN_POINT('Ctrl Pts',(-17.8503456449081,7.68150784529143,-10.4900577947199));
#66284=CARTESIAN_POINT('Ctrl Pts',(-17.8430549103876,7.7880469320545,-10.5647863132449));
#66285=CARTESIAN_POINT('Ctrl Pts',(-17.835764175867,7.89802714309815,-10.6346446939616));
#66286=CARTESIAN_POINT('Ctrl Pts',(-17.8284734413464,8.01098544471159,-10.6993330586784));
#66287=CARTESIAN_POINT('Ctrl Pts',(-17.8211842251912,8.12392022167701,-10.7640079514238));
#66288=CARTESIAN_POINT('Ctrl Pts',(-17.8138950090359,8.23983155880657,-10.8235148084672));
#66289=CARTESIAN_POINT('Ctrl Pts',(-17.8066057928806,8.35823017917576,-10.8775987700944));
#66290=CARTESIAN_POINT('Ctrl Pts',(-17.7993168960918,8.47662361207955,-10.9316803621104));
#66291=CARTESIAN_POINT('Ctrl Pts',(-17.7920279993031,8.59750380479902,-10.9803393896484));
#66292=CARTESIAN_POINT('Ctrl Pts',(-17.7847391025143,8.72035948000763,-11.0233682400342));
#66293=CARTESIAN_POINT('Ctrl Pts',(-17.777450984006,8.84320203715903,-11.0663924959646));
#66294=CARTESIAN_POINT('Ctrl Pts',(-17.7701628654976,8.96801933638021,-11.1037876646716));
#66295=CARTESIAN_POINT('Ctrl Pts',(-17.7628747469893,9.09428288699931,-11.1353953292219));
#66296=CARTESIAN_POINT('Ctrl Pts',(-17.7555860914211,9.22055574195172,-11.1670053229341));
#66297=CARTESIAN_POINT('Ctrl Pts',(-17.7482974358529,9.34827473355606,-11.1928268781538));
#66298=CARTESIAN_POINT('Ctrl Pts',(-17.7410087802847,9.47689872479612,-11.2127521379263));
#66299=CARTESIAN_POINT('Ctrl Pts',(-17.7386725201898,9.51812705492797,-11.2191388561422));
#66300=CARTESIAN_POINT('Ctrl Pts',(-17.7363362600949,9.55944829064432,-11.2249201712499));
#66301=CARTESIAN_POINT('Ctrl Pts',(-17.734,9.6008444244948,-11.2300936493755));
#66302=CARTESIAN_POINT('Origin',(-17.734,10.1295,-7.));
#66303=CARTESIAN_POINT('Ctrl Pts',(-18.0286142198359,11.618114722277,-10.994645817669));
#66304=CARTESIAN_POINT('Ctrl Pts',(-18.0397899417923,11.4295234319622,-11.0649248321473));
#66305=CARTESIAN_POINT('Ctrl Pts',(-18.0508912348905,11.2361487040778,-11.1217763475609));
#66306=CARTESIAN_POINT('Ctrl Pts',(-18.0855390992679,10.6302068195219,-11.2541656503512));
#66307=CARTESIAN_POINT('Ctrl Pts',(-18.1093855857369,10.2100253826391,-11.2827745919004));
#66308=CARTESIAN_POINT('Ctrl Pts',(-18.1471820760258,9.53442686787758,-11.2291898906281));
#66309=CARTESIAN_POINT('Ctrl Pts',(-18.1614172796559,9.27881522463706,-11.1852708984346));
#66310=CARTESIAN_POINT('Ctrl Pts',(-18.190622001046,8.77281474633276,-11.0500330431345));
#66311=CARTESIAN_POINT('Ctrl Pts',(-18.2056655138667,8.52380028392084,-10.9579139355769));
#66312=CARTESIAN_POINT('Ctrl Pts',(-18.2520857621324,7.78229449195763,-10.6020365091));
#66313=CARTESIAN_POINT('Ctrl Pts',(-18.2822658968775,7.33181572759219,-10.2645063028337));
#66314=CARTESIAN_POINT('Ctrl Pts',(-18.3295643900168,6.77226297682638,-9.6420119018166));
#66315=CARTESIAN_POINT('Ctrl Pts',(-18.3453631324316,6.60632476873529,-9.41630116393842));
#66316=CARTESIAN_POINT('Ctrl Pts',(-18.3745510922519,6.33970460921812,-8.96713091919617));
#66317=CARTESIAN_POINT('Ctrl Pts',(-18.3879438485495,6.23381129189303,-8.74807419247257));
#66318=CARTESIAN_POINT('Ctrl Pts',(-18.4231083478773,6.00795504093371,-8.15680262527249));
#66319=CARTESIAN_POINT('Ctrl Pts',(-18.4452893358322,5.91943710373188,-7.77503571946316));
#66320=CARTESIAN_POINT('Ctrl Pts',(-18.4823846590503,5.85951254984844,-7.1169598782444));
#66321=CARTESIAN_POINT('Ctrl Pts',(-18.4973479370614,5.86070190714408,-6.84560128227382));
#66322=CARTESIAN_POINT('Ctrl Pts',(-18.5347901270604,5.92780682615062,-6.17395386811052));
#66323=CARTESIAN_POINT('Ctrl Pts',(-18.5577037975171,6.02500291571947,-5.77948263353823));
#66324=CARTESIAN_POINT('Ctrl Pts',(-18.611839791862,6.38541099251693,-4.88640861831262));
#66325=CARTESIAN_POINT('Ctrl Pts',(-18.6422260281472,6.69442287471882,-4.41432819085399));
#66326=CARTESIAN_POINT('Ctrl Pts',(-18.7055320907897,7.4779313868878,-3.61529311894462));
#66327=CARTESIAN_POINT('Ctrl Pts',(-18.735995631186,7.94522306179521,-3.29648992480263));
#66328=CARTESIAN_POINT('Ctrl Pts',(-18.7812358479547,8.68608970371472,-2.98133201949152));
#66329=CARTESIAN_POINT('Ctrl Pts',(-18.7951410857659,8.91925017279069,-2.9050736050566));
#66330=CARTESIAN_POINT('Ctrl Pts',(-18.8352496726883,9.6127897355547,-2.74269183357329));
#66331=CARTESIAN_POINT('Ctrl Pts',(-18.8606371003608,10.0823473599482,-2.71170941554586));
#66332=CARTESIAN_POINT('Ctrl Pts',(-18.9017618534194,10.8091993674334,-2.78332875356657));
#66333=CARTESIAN_POINT('Ctrl Pts',(-18.9166851645012,11.0679300498758,-2.8332674363393));
#66334=CARTESIAN_POINT('Ctrl Pts',(-18.9543381615285,11.7116484510719,-3.02055286889724));
#66335=CARTESIAN_POINT('Ctrl Pts',(-18.9765376750217,12.0845440079559,-3.18988324934561));
#66336=CARTESIAN_POINT('Ctrl Pts',(-19.0125999013546,12.6253538391597,-3.53605033808907));
#66337=CARTESIAN_POINT('Ctrl Pts',(-19.0259253745705,12.8122090384483,-3.67865896236762));
#66338=CARTESIAN_POINT('Ctrl Pts',(-19.0711062246202,13.4071505539574,-4.21583690391118));
#66339=CARTESIAN_POINT('Ctrl Pts',(-19.1018264230492,13.7479366700916,-4.67589507881516));
#66340=CARTESIAN_POINT('Ctrl Pts',(-19.1493255902435,14.1047108978616,-5.43622809776405));
#66341=CARTESIAN_POINT('Ctrl Pts',(-19.1647081333843,14.1966683223724,-5.69392415695462));
#66342=CARTESIAN_POINT('Ctrl Pts',(-19.2024932025121,14.3622053978055,-6.35105363367153));
#66343=CARTESIAN_POINT('Ctrl Pts',(-19.2246636397218,14.4046789399255,-6.75553616149174));
#66344=CARTESIAN_POINT('Ctrl Pts',(-19.2628448806025,14.3793616086868,-7.42998982348097));
#66345=CARTESIAN_POINT('Ctrl Pts',(-19.278113450657,14.3435617867383,-7.69850243303745));
#66346=CARTESIAN_POINT('Ctrl Pts',(-19.3145998245686,14.196207970448,-8.33476912891735));
#66347=CARTESIAN_POINT('Ctrl Pts',(-19.335512893636,14.0599945188133,-8.69438243891843));
#66348=CARTESIAN_POINT('Ctrl Pts',(-19.3695475245382,13.772450891264,-9.22503986555262));
#66349=CARTESIAN_POINT('Ctrl Pts',(-19.3820444339168,13.6523714961616,-9.41065803948714));
#66350=CARTESIAN_POINT('Ctrl Pts',(-19.4101330724861,13.3490093207116,-9.80819322705906));
#66351=CARTESIAN_POINT('Ctrl Pts',(-19.4255790255469,13.1581441494962,-10.0130563185497));
#66352=CARTESIAN_POINT('Ctrl Pts',(-19.4697727609324,12.5604719313637,-10.5399554439652));
#66353=CARTESIAN_POINT('Ctrl Pts',(-19.4992177593519,12.1132641842266,-10.8086187469988));
#66354=CARTESIAN_POINT('Ctrl Pts',(-19.5283177970268,11.6253074398653,-10.991959899824));
#66355=CARTESIAN_POINT('Ctrl Pts',(-19.5285320816716,11.6217118974251,-10.9933053214558));
#66356=CARTESIAN_POINT('Ctrl Pts',(-19.5287463281039,11.618114650837,-10.9946458442913));
#66357=CARTESIAN_POINT('Origin',(-23.734,10.1295,-7.));
#66358=CARTESIAN_POINT('',(-21.0285562874006,11.6181146495903,-10.9946458447559));
#66359=CARTESIAN_POINT('',(-20.6190482780298,11.6181146495903,-10.9946458447559));
#66360=CARTESIAN_POINT('',(-23.734,11.6181146495903,-10.9946458447559));
#66361=CARTESIAN_POINT('',(-19.2043183294647,10.1294271144268,-11.2629999993769));
#66362=CARTESIAN_POINT('Ctrl Pts',(-20.6190482780298,11.6181146495903,-10.9946458447559));
#66363=CARTESIAN_POINT('Ctrl Pts',(-20.6121906290549,11.7332039726838,-10.9517575239819));
#66364=CARTESIAN_POINT('Ctrl Pts',(-20.60533298008,11.8464456215055,-10.9038886682126));
#66365=CARTESIAN_POINT('Ctrl Pts',(-20.5984753311051,11.9573848895994,-10.8512343255603));
#66366=CARTESIAN_POINT('Ctrl Pts',(-20.5916138715458,12.06838580323,-10.7985507245105));
#66367=CARTESIAN_POINT('Ctrl Pts',(-20.5847524119864,12.1770814109274,-10.7410764995601));
#66368=CARTESIAN_POINT('Ctrl Pts',(-20.5778909524271,12.2830397599629,-10.6790536150291));
#66369=CARTESIAN_POINT('Ctrl Pts',(-20.5710273823149,12.3890307012904,-10.6170116525494));
#66370=CARTESIAN_POINT('Ctrl Pts',(-20.5641638122027,12.4922823613388,-10.5504184614062));
#66371=CARTESIAN_POINT('Ctrl Pts',(-20.5573002420905,12.5923911973628,-10.4795597350747));
#66372=CARTESIAN_POINT('Ctrl Pts',(-20.5504294658789,12.6926051381959,-10.4086266137826));
#66373=CARTESIAN_POINT('Ctrl Pts',(-20.5435586896673,12.7896693412134,-10.3334192620168));
#66374=CARTESIAN_POINT('Ctrl Pts',(-20.5366879134557,12.8832127424892,-10.2542641459864));
#66375=CARTESIAN_POINT('Ctrl Pts',(-20.533223768236,12.9303759619541,-10.2143552902232));
#66376=CARTESIAN_POINT('Ctrl Pts',(-20.5297596230163,12.9766447457956,-10.1734435061821));
#66377=CARTESIAN_POINT('Ctrl Pts',(-20.5262954777966,13.0219751493983,-10.1315741265557));
#66378=CARTESIAN_POINT('Ctrl Pts',(-20.5192445844224,13.1142402890342,-10.0463535273403));
#66379=CARTESIAN_POINT('Ctrl Pts',(-20.5121936910481,13.202815074995,-9.95697931960131));
#66380=CARTESIAN_POINT('Ctrl Pts',(-20.5051427976739,13.2873186628024,-9.86379997430979));
#66381=CARTESIAN_POINT('Ctrl Pts',(-20.4980972350301,13.3717583628408,-9.77069107597379));
#66382=CARTESIAN_POINT('Ctrl Pts',(-20.4910516723863,13.4521327375992,-9.67378305102304));
#66383=CARTESIAN_POINT('Ctrl Pts',(-20.4840061097425,13.5280976244367,-9.57346132420387));
#66384=CARTESIAN_POINT('Ctrl Pts',(-20.4769645310387,13.6040195566425,-9.47319632468334));
#66385=CARTESIAN_POINT('Ctrl Pts',(-20.4699229523349,13.6755367369793,-9.36952177262488));
#66386=CARTESIAN_POINT('Ctrl Pts',(-20.462881373631,13.7423453554112,-9.26285603560717));
#66387=CARTESIAN_POINT('Ctrl Pts',(-20.4558422186787,13.8091309779363,-9.15622701354339));
#66388=CARTESIAN_POINT('Ctrl Pts',(-20.4488030637263,13.8712110646756,-9.04660918159906));
#66389=CARTESIAN_POINT('Ctrl Pts',(-20.4417639087739,13.9283253559476,-8.93444951213759));
#66390=CARTESIAN_POINT('Ctrl Pts',(-20.4347249074765,13.9854384004943,-8.82229229096549));
#66391=CARTESIAN_POINT('Ctrl Pts',(-20.4276859061791,14.0375856880425,-8.7075936815819));
#66392=CARTESIAN_POINT('Ctrl Pts',(-20.4206469048817,14.0845531721528,-8.59082475635887));
#66393=CARTESIAN_POINT('Ctrl Pts',(-20.4170812142173,14.1083451154338,-8.53167405458023));
#66394=CARTESIAN_POINT('Ctrl Pts',(-20.4135155235529,14.1308086464159,-8.47199245138789));
#66395=CARTESIAN_POINT('Ctrl Pts',(-20.4099498328884,14.1519206685263,-8.41184310934763));
#66396=CARTESIAN_POINT('Ctrl Pts',(-20.4023577742973,14.1968723269634,-8.28377329848487));
#66397=CARTESIAN_POINT('Ctrl Pts',(-20.3947657157062,14.235676866179,-8.15363107788822));
#66398=CARTESIAN_POINT('Ctrl Pts',(-20.387173657115,14.2681822825818,-8.02199704688589));
#66399=CARTESIAN_POINT('Ctrl Pts',(-20.3793762013538,14.301567107443,-7.88680176077315));
#66400=CARTESIAN_POINT('Ctrl Pts',(-20.3715787455926,14.3283070841755,-7.75003309890807));
#66401=CARTESIAN_POINT('Ctrl Pts',(-20.3637812898313,14.3482937650472,-7.61233011358183));
#66402=CARTESIAN_POINT('Ctrl Pts',(-20.356172729412,14.3677962635095,-7.47796301797296));
#66403=CARTESIAN_POINT('Ctrl Pts',(-20.3485641689927,14.3808689065492,-7.34270661697724));
#66404=CARTESIAN_POINT('Ctrl Pts',(-20.3409556085734,14.3874635719564,-7.20715988967947));
#66405=CARTESIAN_POINT('Ctrl Pts',(-20.3330637051412,14.3943038228966,-7.06656539828703));
#66406=CARTESIAN_POINT('Ctrl Pts',(-20.325171801709,14.3941742794439,-6.92565884820072));
#66407=CARTESIAN_POINT('Ctrl Pts',(-20.3172798982768,14.3870804471944,-6.78510994516341));
#66408=CARTESIAN_POINT('Ctrl Pts',(-20.3093879948446,14.379986614945,-6.6445610421261));
#66409=CARTESIAN_POINT('Ctrl Pts',(-20.3014960914124,14.3659285138308,-6.50437010302651));
#66410=CARTESIAN_POINT('Ctrl Pts',(-20.2936041879802,14.3449717784631,-6.36520343023823));
#66411=CARTESIAN_POINT('Ctrl Pts',(-20.2865699500337,14.3262925505144,-6.24116092274532));
#66412=CARTESIAN_POINT('Ctrl Pts',(-20.2795357120872,14.3021211905467,-6.11785842915652));
#66413=CARTESIAN_POINT('Ctrl Pts',(-20.2725014741406,14.2725375817417,-5.99580450295988));
#66414=CARTESIAN_POINT('Ctrl Pts',(-20.265471124558,14.2429703260709,-5.87381804534861));
#66415=CARTESIAN_POINT('Ctrl Pts',(-20.2584407749754,14.2079968698656,-5.75307915384293));
#66416=CARTESIAN_POINT('Ctrl Pts',(-20.2514104253928,14.1677481508453,-5.63408606706174));
#66417=CARTESIAN_POINT('Ctrl Pts',(-20.2443818233126,14.1275094362681,-5.51512255785725));
#66418=CARTESIAN_POINT('Ctrl Pts',(-20.2373532212324,14.081998189689,-5.39790435455489));
#66419=CARTESIAN_POINT('Ctrl Pts',(-20.2303246191521,14.0313951170116,-5.2829142433062));
#66420=CARTESIAN_POINT('Ctrl Pts',(-20.2232971566901,13.9808002491211,-5.16794277656471));
#66421=CARTESIAN_POINT('Ctrl Pts',(-20.2162696942281,13.9251153573761,-5.05519903309845));
#66422=CARTESIAN_POINT('Ctrl Pts',(-20.2092422317661,13.864568966409,-4.94514506201334));
#66423=CARTESIAN_POINT('Ctrl Pts',(-20.2022129155991,13.8040066045073,-4.83506206087784));
#66424=CARTESIAN_POINT('Ctrl Pts',(-20.1951835994321,13.7385803675296,-4.72767058650132));
#66425=CARTESIAN_POINT('Ctrl Pts',(-20.1881542832652,13.668564345964,-4.62340736449718));
#66426=CARTESIAN_POINT('Ctrl Pts',(-20.1845223698675,13.6323884049852,-4.5695365492016));
#66427=CARTESIAN_POINT('Ctrl Pts',(-20.1808904564697,13.5949879020393,-4.51650039912015));
#66428=CARTESIAN_POINT('Ctrl Pts',(-20.177258543072,13.556405113779,-4.4643560302843));
#66429=CARTESIAN_POINT('Ctrl Pts',(-20.1698758048977,13.4779763098484,-4.35836004959168));
#66430=CARTESIAN_POINT('Ctrl Pts',(-20.1624930667234,13.3946337929648,-4.25601561199655));
#66431=CARTESIAN_POINT('Ctrl Pts',(-20.1551103285491,13.3067375194271,-4.15775955536042));
#66432=CARTESIAN_POINT('Ctrl Pts',(-20.1477267136224,13.2188308075853,-4.05949183012278));
#66433=CARTESIAN_POINT('Ctrl Pts',(-20.1403430986957,13.1263694729261,-3.96531369053039));
#66434=CARTESIAN_POINT('Ctrl Pts',(-20.132959483769,13.0297520661519,-3.87562695044562));
#66435=CARTESIAN_POINT('Ctrl Pts',(-20.1255738893439,12.9331087568887,-3.78591616593788));
#66436=CARTESIAN_POINT('Ctrl Pts',(-20.1181882949188,12.8323073816896,-3.70069940365669));
#66437=CARTESIAN_POINT('Ctrl Pts',(-20.1108027004937,12.7277819172479,-3.62034024219851));
#66438=CARTESIAN_POINT('Ctrl Pts',(-20.103416930456,12.62325396743,-3.5399791699835));
#66439=CARTESIAN_POINT('Ctrl Pts',(-20.0960311604184,12.5150020057933,-3.46447611991925));
#66440=CARTESIAN_POINT('Ctrl Pts',(-20.0886453903808,12.4034914669734,-3.39415310805738));
#66441=CARTESIAN_POINT('Ctrl Pts',(-20.0812586628136,12.2919664713494,-3.32382097915588));
#66442=CARTESIAN_POINT('Ctrl Pts',(-20.0738719352465,12.1771823237382,-3.25867039897299));
#66443=CARTESIAN_POINT('Ctrl Pts',(-20.0664852076794,12.0596321377066,-3.19897922513017));
#66444=CARTESIAN_POINT('Ctrl Pts',(-20.0646277711742,12.030073445479,-3.18396952505323));
#66445=CARTESIAN_POINT('Ctrl Pts',(-20.062770334669,12.000339980668,-3.16930479834316));
#66446=CARTESIAN_POINT('Ctrl Pts',(-20.0609128981638,11.9704398252603,-3.15498900394674));
#66447=CARTESIAN_POINT('Ctrl Pts',(-20.0537147341779,11.8545671043196,-3.09951069533852));
#66448=CARTESIAN_POINT('Ctrl Pts',(-20.0465165701919,11.7361510511272,-3.04925809080175));
#66449=CARTESIAN_POINT('Ctrl Pts',(-20.039318406206,11.6156836829833,-3.00444909174791));
#66450=CARTESIAN_POINT('Ctrl Pts',(-20.0321223301932,11.495251258838,-2.95965309045125));
#66451=CARTESIAN_POINT('Ctrl Pts',(-20.0249262541804,11.3727690395134,-2.92029767028471));
#66452=CARTESIAN_POINT('Ctrl Pts',(-20.0177301781676,11.2487478957301,-2.88655215811556));
#66453=CARTESIAN_POINT('Ctrl Pts',(-20.0105343327563,11.1247307262596,-2.85280772733637));
#66454=CARTESIAN_POINT('Ctrl Pts',(-20.003338487345,10.9991750728829,-2.82467294395313));
#66455=CARTESIAN_POINT('Ctrl Pts',(-19.9961426419336,10.8726059996031,-2.80226698403128));
#66456=CARTESIAN_POINT('Ctrl Pts',(-19.9889472731621,10.746045310029,-2.77986250823955));
#66457=CARTESIAN_POINT('Ctrl Pts',(-19.9817519043905,10.6184716854824,-2.76318615803964));
#66458=CARTESIAN_POINT('Ctrl Pts',(-19.9745565356189,10.4904191279099,-2.75230575687129));
#66459=CARTESIAN_POINT('Ctrl Pts',(-19.9673594219651,10.3623355174989,-2.74142271719775));
#66460=CARTESIAN_POINT('Ctrl Pts',(-19.9601623083114,10.2337730969215,-2.73633846333066));
#66461=CARTESIAN_POINT('Ctrl Pts',(-19.9529651946576,10.1052700053776,-2.73706885965061));
#66462=CARTESIAN_POINT('Ctrl Pts',(-19.950165880857,10.0552887913946,-2.73735294693847));
#66463=CARTESIAN_POINT('Ctrl Pts',(-19.9473665670563,10.0053165643208,-2.73851612639266));
#66464=CARTESIAN_POINT('Ctrl Pts',(-19.9445672532556,9.95538496385429,-2.74055720144196));
#66465=CARTESIAN_POINT('Ctrl Pts',(-19.9372996658139,9.82575238303743,-2.74585624701248));
#66466=CARTESIAN_POINT('Ctrl Pts',(-19.9300320783721,9.69634259000923,-2.75707830985315));
#66467=CARTESIAN_POINT('Ctrl Pts',(-19.9227644909304,9.56770226521737,-2.77418028008848));
#66468=CARTESIAN_POINT('Ctrl Pts',(-19.9154981270172,9.4390835975591,-2.791279371136));
#66469=CARTESIAN_POINT('Ctrl Pts',(-19.908231763104,9.31123447891631,-2.81425634945049));
#66470=CARTESIAN_POINT('Ctrl Pts',(-19.9009653991908,9.18469503787924,-2.8430164080728));
#66471=CARTESIAN_POINT('Ctrl Pts',(-19.8936986728736,9.05814928578943,-2.87177790107988));
#66472=CARTESIAN_POINT('Ctrl Pts',(-19.8864319465564,8.93291367641405,-2.90632297800972));
#66473=CARTESIAN_POINT('Ctrl Pts',(-19.8791652202392,8.80951708114262,-2.94650594006544));
#66474=CARTESIAN_POINT('Ctrl Pts',(-19.8718988049651,8.68612576770948,-2.98668718213929));
#66475=CARTESIAN_POINT('Ctrl Pts',(-19.8646323896911,8.56457363589267,-3.03250571882476));
#66476=CARTESIAN_POINT('Ctrl Pts',(-19.8573659744171,8.44537320366214,-3.08376635862251));
#66477=CARTESIAN_POINT('Ctrl Pts',(-19.8500981487013,8.32614963412624,-3.1350369483261));
#66478=CARTESIAN_POINT('Ctrl Pts',(-19.8428303229855,8.20927899029798,-3.19175161528081));
#66479=CARTESIAN_POINT('Ctrl Pts',(-19.8355624972697,8.09525300626815,-3.25366737081543));
#66480=CARTESIAN_POINT('Ctrl Pts',(-19.8331155342956,8.05686224513593,-3.27451343499348));
#66481=CARTESIAN_POINT('Ctrl Pts',(-19.8306685713215,8.01879374688149,-3.29594868576314));
#66482=CARTESIAN_POINT('Ctrl Pts',(-19.8282216083474,7.98106564680016,-3.3179626794408));
#66483=CARTESIAN_POINT('Ctrl Pts',(-19.8209722445845,7.8692925123192,-3.38318125844403));
#66484=CARTESIAN_POINT('Ctrl Pts',(-19.8137228808216,7.76047097522316,-3.45350495882227));
#66485=CARTESIAN_POINT('Ctrl Pts',(-19.8064735170587,7.65506214645853,-3.5286420079512));
#66486=CARTESIAN_POINT('Ctrl Pts',(-19.7992255772224,7.54967402219211,-3.60376429859246));
#66487=CARTESIAN_POINT('Ctrl Pts',(-19.7919776373861,7.44769755071203,-3.68369785128094));
#66488=CARTESIAN_POINT('Ctrl Pts',(-19.7847296975498,7.34956393018538,-3.76810822462391));
#66489=CARTESIAN_POINT('Ctrl Pts',(-19.777481498792,7.25142680398565,-3.85252161339799));
#66490=CARTESIAN_POINT('Ctrl Pts',(-19.7702333000342,7.15713306776873,-3.94141191953554));
#66491=CARTESIAN_POINT('Ctrl Pts',(-19.7629851012764,7.06708019444085,-4.03440496113865));
#66492=CARTESIAN_POINT('Ctrl Pts',(-19.7557372208103,6.97703127562475,-4.12739391911772));
#66493=CARTESIAN_POINT('Ctrl Pts',(-19.7484893403443,6.89122308655681,-4.22448500231484));
#66494=CARTESIAN_POINT('Ctrl Pts',(-19.7412414598782,6.81001549954522,-4.32526792907393));
#66495=CARTESIAN_POINT('Ctrl Pts',(-19.7339920212989,6.72879045493104,-4.42607252164463));
#66496=CARTESIAN_POINT('Ctrl Pts',(-19.7267425827196,6.65216820444815,-4.53057027310971));
#66497=CARTESIAN_POINT('Ctrl Pts',(-19.7194931441403,6.58046788328555,-4.63831838840851));
#66498=CARTESIAN_POINT('Ctrl Pts',(-19.7169540839066,6.55535539599213,-4.6760563389847));
#66499=CARTESIAN_POINT('Ctrl Pts',(-19.7144150236729,6.53084629803888,-4.71419274091907));
#66500=CARTESIAN_POINT('Ctrl Pts',(-19.7118759634392,6.50695304158714,-4.7527077328274));
#66501=CARTESIAN_POINT('Ctrl Pts',(-19.7046273272713,6.43874137784321,-4.86266225838396));
#66502=CARTESIAN_POINT('Ctrl Pts',(-19.6973786911033,6.37552683267345,-4.97574519864636));
#66503=CARTESIAN_POINT('Ctrl Pts',(-19.6901300549354,6.31758028923035,-5.09148300540817));
#66504=CARTESIAN_POINT('Ctrl Pts',(-19.6828828888796,6.25964549805596,-5.20719733912528));
#66505=CARTESIAN_POINT('Ctrl Pts',(-19.6756357228238,6.20697673229024,-5.3255651559131));
#66506=CARTESIAN_POINT('Ctrl Pts',(-19.6683885567681,6.15979847242466,-5.44608919755154));
#66507=CARTESIAN_POINT('Ctrl Pts',(-19.6611411920792,6.1126189194791,-5.5666165425595));
#66508=CARTESIAN_POINT('Ctrl Pts',(-19.6538938273903,6.07093030282521,-5.68929990953642));
#66509=CARTESIAN_POINT('Ctrl Pts',(-19.6466464627014,6.03490869934269,-5.81362270732221));
#66510=CARTESIAN_POINT('Ctrl Pts',(-19.6393994491196,5.99888884096896,-5.9379394821444));
#66511=CARTESIAN_POINT('Ctrl Pts',(-19.6321524355377,5.96853554134302,-6.06389519594937));
#66512=CARTESIAN_POINT('Ctrl Pts',(-19.6249054219559,5.94397475426181,-6.19095895203749));
#66513=CARTESIAN_POINT('Ctrl Pts',(-19.6176568912815,5.91940882561603,-6.31804930770098));
#66514=CARTESIAN_POINT('Ctrl Pts',(-19.6104083606071,5.90063789667634,-6.44624782889921));
#66515=CARTESIAN_POINT('Ctrl Pts',(-19.6031598299327,5.88773670376587,-6.575013954675));
#66516=CARTESIAN_POINT('Ctrl Pts',(-19.6006166594655,5.88321027844253,-6.62019196701424));
#66517=CARTESIAN_POINT('Ctrl Pts',(-19.5980734889982,5.87940594047427,-6.66543979058032));
#66518=CARTESIAN_POINT('Ctrl Pts',(-19.595530318531,5.87632540455801,-6.71073392752201));
#66519=CARTESIAN_POINT('Ctrl Pts',(-19.5882769227069,5.86753938465133,-6.8399176798439));
#66520=CARTESIAN_POINT('Ctrl Pts',(-19.5810235268829,5.8646418040146,-6.969524604123));
#66521=CARTESIAN_POINT('Ctrl Pts',(-19.5737701310588,5.86764989988178,-7.09900870730542));
#66522=CARTESIAN_POINT('Ctrl Pts',(-19.56651812171,5.8706574207561,-7.22846805980276));
#66523=CARTESIAN_POINT('Ctrl Pts',(-19.5592661123613,5.87956835819632,-7.35780429308268));
#66524=CARTESIAN_POINT('Ctrl Pts',(-19.5520141030125,5.89434784617514,-7.48647223348577));
#66525=CARTESIAN_POINT('Ctrl Pts',(-19.5447618211018,5.90912788963121,-7.61514500978809));
#66526=CARTESIAN_POINT('Ctrl Pts',(-19.5375095391911,5.9297768885282,-7.74314909965177));
#66527=CARTESIAN_POINT('Ctrl Pts',(-19.5302572572804,5.95620815783502,-7.869944940855));
#66528=CARTESIAN_POINT('Ctrl Pts',(-19.5230052970079,5.98263825491685,-7.99673515867135));
#66529=CARTESIAN_POINT('Ctrl Pts',(-19.5157533367354,6.01485003720225,-8.12231689743408));
#66530=CARTESIAN_POINT('Ctrl Pts',(-19.5085013764629,6.05270583759639,-8.24616144916773));
#66531=CARTESIAN_POINT('Ctrl Pts',(-19.5012478974044,6.09056956617225,-8.37003193780146));
#66532=CARTESIAN_POINT('Ctrl Pts',(-19.4939944183459,6.13407957230502,-8.49216418269563));
#66533=CARTESIAN_POINT('Ctrl Pts',(-19.4867409392874,6.18304841315165,-8.61204493506296));
#66534=CARTESIAN_POINT('Ctrl Pts',(-19.4842221840659,6.20005273929354,-8.65367327210638));
#66535=CARTESIAN_POINT('Ctrl Pts',(-19.4817034288444,6.21771486629463,-8.69503028409148));
#66536=CARTESIAN_POINT('Ctrl Pts',(-19.4791846736229,6.23602558437293,-8.73609503624007));
#66537=CARTESIAN_POINT('Ctrl Pts',(-19.4719351321326,6.28872793086994,-8.8542885875413));
#66538=CARTESIAN_POINT('Ctrl Pts',(-19.4646855906423,6.34682588834277,-8.97010224507851));
#66539=CARTESIAN_POINT('Ctrl Pts',(-19.4574360491521,6.41007951261352,-9.08304590396125));
#66540=CARTESIAN_POINT('Ctrl Pts',(-19.4501879543185,6.4733205145299,-9.19596702476964));
#66541=CARTESIAN_POINT('Ctrl Pts',(-19.442939859485,6.54171496200513,-9.30601898763982));
#66542=CARTESIAN_POINT('Ctrl Pts',(-19.4356917646515,6.61497724357959,-9.41273678518878));
#66543=CARTESIAN_POINT('Ctrl Pts',(-19.4284434460103,6.6882417873569,-9.51945787798464));
#66544=CARTESIAN_POINT('Ctrl Pts',(-19.421195127369,6.76637427283083,-9.62284431239772));
#66545=CARTESIAN_POINT('Ctrl Pts',(-19.4139468087278,6.84904591912196,-9.7224602886453));
#66546=CARTESIAN_POINT('Ctrl Pts',(-19.4066988291477,6.93171369820757,-9.82207160506727));
#66547=CARTESIAN_POINT('Ctrl Pts',(-19.3994508495676,7.01891999109499,-9.91791255098534));
#66548=CARTESIAN_POINT('Ctrl Pts',(-19.3922028699875,7.11029604323606,-10.0095807793547));
#66549=CARTESIAN_POINT('Ctrl Pts',(-19.384953363692,7.20169134284058,-10.1012683167315));
#66550=CARTESIAN_POINT('Ctrl Pts',(-19.3777038573965,7.29725791129566,-10.1887811363229));
#66551=CARTESIAN_POINT('Ctrl Pts',(-19.370454351101,7.39659024575933,-10.2717538530849));
#66552=CARTESIAN_POINT('Ctrl Pts',(-19.3679159103056,7.43137182119772,-10.3008070493374));
#66553=CARTESIAN_POINT('Ctrl Pts',(-19.3653774695102,7.46661479837169,-10.3293039451163));
#66554=CARTESIAN_POINT('Ctrl Pts',(-19.3628390287147,7.50230080009072,-10.3572300135671));
#66555=CARTESIAN_POINT('Ctrl Pts',(-19.3555873220309,7.60424700961119,-10.4370079849911));
#66556=CARTESIAN_POINT('Ctrl Pts',(-19.348335615347,7.70984795365347,-10.5121532289869));
#66557=CARTESIAN_POINT('Ctrl Pts',(-19.3410839086632,7.81866176481192,-10.5823449932681));
#66558=CARTESIAN_POINT('Ctrl Pts',(-19.3338336170501,7.92745434245319,-10.6525230605928));
#66559=CARTESIAN_POINT('Ctrl Pts',(-19.3265833254369,8.03945824632693,-10.7177493891838));
#66560=CARTESIAN_POINT('Ctrl Pts',(-19.3193330338238,8.15420302405171,-10.7777467962808));
#66561=CARTESIAN_POINT('Ctrl Pts',(-19.312082494214,8.26895172662819,-10.8377462555925));
#66562=CARTESIAN_POINT('Ctrl Pts',(-19.3048319546043,8.38644118586107,-10.8925162726726));
#66563=CARTESIAN_POINT('Ctrl Pts',(-19.2975814149945,8.5061764926047,-10.9418256925361));
#66564=CARTESIAN_POINT('Ctrl Pts',(-19.290331206482,8.62590633161308,-10.9911328606757));
#66565=CARTESIAN_POINT('Ctrl Pts',(-19.2830809979695,8.74788149278864,-11.0349798004483));
#66566=CARTESIAN_POINT('Ctrl Pts',(-19.2758307894569,8.87158741976644,-11.0731836369712));
#66567=CARTESIAN_POINT('Ctrl Pts',(-19.2685790612726,8.99531927598627,-11.1113954811665));
#66568=CARTESIAN_POINT('Ctrl Pts',(-19.2613273330882,9.12078229219613,-11.143961758176));
#66569=CARTESIAN_POINT('Ctrl Pts',(-19.2540756049039,9.24744675522654,-11.1707494618335));
#66570=CARTESIAN_POINT('Ctrl Pts',(-19.2515481978714,9.29159246042793,-11.180085640588));
#66571=CARTESIAN_POINT('Ctrl Pts',(-19.249020790839,9.33588399625009,-11.1887203497344));
#66572=CARTESIAN_POINT('Ctrl Pts',(-19.2464933838065,9.38029862923168,-11.1966494142398));
#66573=CARTESIAN_POINT('Ctrl Pts',(-19.239033624303,9.51139048591435,-11.220052417214));
#66574=CARTESIAN_POINT('Ctrl Pts',(-19.2315738647995,9.64359095899357,-11.2373107330629));
#66575=CARTESIAN_POINT('Ctrl Pts',(-19.224114105296,9.77632784658091,-11.2483453755609));
#66576=CARTESIAN_POINT('Ctrl Pts',(-19.2175155133523,9.8937413579231,-11.2581061598134));
#66577=CARTESIAN_POINT('Ctrl Pts',(-19.2109169214085,10.0115743103388,-11.2629979844182));
#66578=CARTESIAN_POINT('Ctrl Pts',(-19.2043183294647,10.1294271144268,-11.2629999993769));
#66579=CARTESIAN_POINT('Ctrl Pts',(-19.2043183294109,10.1294271153884,-11.2629999993769));
#66580=CARTESIAN_POINT('Ctrl Pts',(-19.1970583198552,10.2590930336831,-11.2630022162782));
#66581=CARTESIAN_POINT('Ctrl Pts',(-19.1897983102996,10.3887626081957,-11.257084097175));
#66582=CARTESIAN_POINT('Ctrl Pts',(-19.182538300744,10.5178887238751,-11.2452706862068));
#66583=CARTESIAN_POINT('Ctrl Pts',(-19.175278526011,10.6470106630119,-11.2334576573395));
#66584=CARTESIAN_POINT('Ctrl Pts',(-19.168018751278,10.7755888364936,-11.2157497517238));
#66585=CARTESIAN_POINT('Ctrl Pts',(-19.160758976545,10.9030811422902,-11.1922238986358));
#66586=CARTESIAN_POINT('Ctrl Pts',(-19.1534975321505,11.0306027697949,-11.1686926348825));
#66587=CARTESIAN_POINT('Ctrl Pts',(-19.1462360877561,11.1570376928693,-11.1393408138078));
#66588=CARTESIAN_POINT('Ctrl Pts',(-19.1389746433616,11.2818534964405,-11.1042965803218));
#66589=CARTESIAN_POINT('Ctrl Pts',(-19.1360323418738,11.3324282450154,-11.0900968295944));
#66590=CARTESIAN_POINT('Ctrl Pts',(-19.1330900403861,11.3827373049399,-11.0749630604004));
#66591=CARTESIAN_POINT('Ctrl Pts',(-19.1301477388984,11.4327459192928,-11.0589061425274));
#66592=CARTESIAN_POINT('Ctrl Pts',(-19.1264842467592,11.4950121983722,-11.0389134964128));
#66593=CARTESIAN_POINT('Ctrl Pts',(-19.1228207546201,11.5568240284571,-11.0174859462435));
#66594=CARTESIAN_POINT('Ctrl Pts',(-19.1191572624809,11.6181146495903,-10.9946458447559));
#66595=CARTESIAN_POINT('',(-19.613681670589,10.1296816520865,-11.2629999961298));
#66596=CARTESIAN_POINT('Ctrl Pts',(-19.5287463281039,11.618114650837,-10.9946458442913));
#66597=CARTESIAN_POINT('Ctrl Pts',(-19.5427543530944,11.3829167082039,-11.0822929391522));
#66598=CARTESIAN_POINT('Ctrl Pts',(-19.5565651777506,11.1404319869351,-11.1489989699717));
#66599=CARTESIAN_POINT('Ctrl Pts',(-19.584788886185,10.641461197615,-11.2398924321116));
#66600=CARTESIAN_POINT('Ctrl Pts',(-19.5992884130183,10.3858268071179,-11.2629888708551));
#66601=CARTESIAN_POINT('Ctrl Pts',(-19.6137437660346,10.1296851569352,-11.262999995979));
#66602=CARTESIAN_POINT('Ctrl Pts',(-19.613681670589,10.1296816520865,-11.2629999961298));
#66603=CARTESIAN_POINT('Ctrl Pts',(-19.6210625559268,9.99792696780947,-11.2630056103717));
#66604=CARTESIAN_POINT('Ctrl Pts',(-19.6284434412646,9.86616452721088,-11.2568987546168));
#66605=CARTESIAN_POINT('Ctrl Pts',(-19.6358243266025,9.73495915245449,-11.2447033488358));
#66606=CARTESIAN_POINT('Ctrl Pts',(-19.6432038414137,9.60377814069074,-11.2325102075702));
#66607=CARTESIAN_POINT('Ctrl Pts',(-19.6505833562249,9.47315430553389,-11.2142308037361));
#66608=CARTESIAN_POINT('Ctrl Pts',(-19.6579628710361,9.34364777489142,-11.1899409638194));
#66609=CARTESIAN_POINT('Ctrl Pts',(-19.665341452104,9.21415763094539,-11.1656541973403));
#66610=CARTESIAN_POINT('Ctrl Pts',(-19.6727200331718,9.0857848227637,-11.1353585705236));
#66611=CARTESIAN_POINT('Ctrl Pts',(-19.6800986142396,8.95908014795422,-11.0991811828629));
#66612=CARTESIAN_POINT('Ctrl Pts',(-19.6849303155029,8.87611038293851,-11.0754912175352));
#66613=CARTESIAN_POINT('Ctrl Pts',(-19.6897620167663,8.79385571635695,-11.049280203234));
#66614=CARTESIAN_POINT('Ctrl Pts',(-19.6945937180296,8.71246771439215,-11.0205955406563));
#66615=CARTESIAN_POINT('Ctrl Pts',(-19.7016228891401,8.59406424510147,-10.9788650216284));
#66616=CARTESIAN_POINT('Ctrl Pts',(-19.7086520602506,8.47745739883753,-10.9318830738138));
#66617=CARTESIAN_POINT('Ctrl Pts',(-19.7156812313611,8.36312882780601,-10.8798327131517));
#66618=CARTESIAN_POINT('Ctrl Pts',(-19.7227086284805,8.24882911051486,-10.82779548873));
#66619=CARTESIAN_POINT('Ctrl Pts',(-19.7297360255998,8.13680687283187,-10.7706925591275));
#66620=CARTESIAN_POINT('Ctrl Pts',(-19.7367634227191,8.02752294555477,-10.7087547050979));
#66621=CARTESIAN_POINT('Ctrl Pts',(-19.7437922455919,7.91821684620777,-10.6468042848066));
#66622=CARTESIAN_POINT('Ctrl Pts',(-19.7508210684647,7.8116505045704,-10.5800171656424));
#66623=CARTESIAN_POINT('Ctrl Pts',(-19.7578498913375,7.70825937959702,-10.5086696707029));
#66624=CARTESIAN_POINT('Ctrl Pts',(-19.7648793838462,7.60485840455196,-10.4373153784882));
#66625=CARTESIAN_POINT('Ctrl Pts',(-19.7719088763549,7.50463356199163,-10.3614000686881));
#66626=CARTESIAN_POINT('Ctrl Pts',(-19.7789383688636,7.40798992434636,-10.2812424336089));
#66627=CARTESIAN_POINT('Ctrl Pts',(-19.7859724420486,7.31128331014651,-10.2010325648618));
#66628=CARTESIAN_POINT('Ctrl Pts',(-19.7930065152336,7.21816285464981,-10.1165750994141));
#66629=CARTESIAN_POINT('Ctrl Pts',(-19.8000405884186,7.12899939384763,-10.0282280482948));
#66630=CARTESIAN_POINT('Ctrl Pts',(-19.8036735132583,7.08294867145319,-9.98259898131086));
#66631=CARTESIAN_POINT('Ctrl Pts',(-19.807306438098,7.03795286658765,-9.93593298706528));
#66632=CARTESIAN_POINT('Ctrl Pts',(-19.8109393629378,6.99405904894667,-9.88828306134593));
#66633=CARTESIAN_POINT('Ctrl Pts',(-19.8185514682813,6.90208787460305,-9.78844167453286));
#66634=CARTESIAN_POINT('Ctrl Pts',(-19.8261635736248,6.81489782850554,-9.68421427120516));
#66635=CARTESIAN_POINT('Ctrl Pts',(-19.8337756789683,6.73287352582023,-9.57606242061428));
#66636=CARTESIAN_POINT('Ctrl Pts',(-19.8415681230414,6.64890598169537,-9.46534833967273));
#66637=CARTESIAN_POINT('Ctrl Pts',(-19.8493605671145,6.5703521935622,-9.35052175498863));
#66638=CARTESIAN_POINT('Ctrl Pts',(-19.8571530111877,6.49757984993105,-9.23211223363054));
#66639=CARTESIAN_POINT('Ctrl Pts',(-19.8647591278018,6.42654758755655,-9.11653403772446));
#66640=CARTESIAN_POINT('Ctrl Pts',(-19.872365244416,6.36102356679838,-8.99754254531327));
#66641=CARTESIAN_POINT('Ctrl Pts',(-19.8799713610301,6.30130558280906,-8.8756589519921));
#66642=CARTESIAN_POINT('Ctrl Pts',(-19.8878569688327,6.23939322668899,-8.74929667498954));
#66643=CARTESIAN_POINT('Ctrl Pts',(-19.8957425766354,6.18372190273754,-8.61982593912762));
#66644=CARTESIAN_POINT('Ctrl Pts',(-19.903628184438,6.13457147332775,-8.48785586223272));
#66645=CARTESIAN_POINT('Ctrl Pts',(-19.9115137922407,6.08542104391795,-8.35588578533781));
#66646=CARTESIAN_POINT('Ctrl Pts',(-19.9193994000433,6.04279165902778,-8.22141665147341));
#66647=CARTESIAN_POINT('Ctrl Pts',(-19.927285007846,6.00690792403289,-8.085082289586));
#66648=CARTESIAN_POINT('Ctrl Pts',(-19.9343237861388,5.97487771643589,-7.96338877260736));
#66649=CARTESIAN_POINT('Ctrl Pts',(-19.9413625644316,5.94823387545845,-7.8402524200153));
#66650=CARTESIAN_POINT('Ctrl Pts',(-19.9484013427244,5.92708903886797,-7.71617812990721));
#66651=CARTESIAN_POINT('Ctrl Pts',(-19.9554399109056,5.90594483346336,-7.59210754349001));
#66652=CARTESIAN_POINT('Ctrl Pts',(-19.9624784790867,5.89029936842274,-7.46709945251523));
#66653=CARTESIAN_POINT('Ctrl Pts',(-19.9695170472678,5.8802139040895,-7.3416674920177));
#66654=CARTESIAN_POINT('Ctrl Pts',(-19.9765593081639,5.87012314851751,-7.21616972488726));
#66655=CARTESIAN_POINT('Ctrl Pts',(-19.9836015690599,5.86559825316507,-7.0902480255059));
#66656=CARTESIAN_POINT('Ctrl Pts',(-19.990643829956,5.86664848269717,-6.96441992932841));
#66657=CARTESIAN_POINT('Ctrl Pts',(-19.9976880482936,5.86769900414732,-6.83855685842447));
#66658=CARTESIAN_POINT('Ctrl Pts',(-20.0047322666312,5.87432772657293,-6.71278782503369));
#66659=CARTESIAN_POINT('Ctrl Pts',(-20.0117764849689,5.88649181534104,-6.58762814727832));
#66660=CARTESIAN_POINT('Ctrl Pts',(-20.0188271374083,5.89866701463715,-6.46235415022382));
#66661=CARTESIAN_POINT('Ctrl Pts',(-20.0258777898477,5.91638763336263,-6.33769100055036));
#66662=CARTESIAN_POINT('Ctrl Pts',(-20.0329284422871,5.93955916974701,-6.21414706275352));
#66663=CARTESIAN_POINT('Ctrl Pts',(-20.0364958457761,5.95128322230163,-6.15163780158474));
#66664=CARTESIAN_POINT('Ctrl Pts',(-20.0400632492651,5.96440191628728,-6.08941489423676));
#66665=CARTESIAN_POINT('Ctrl Pts',(-20.0436306527542,5.97889809135828,-6.02754290789789));
#66666=CARTESIAN_POINT('Ctrl Pts',(-20.0506540818166,6.00743785637264,-5.90573064070087));
#66667=CARTESIAN_POINT('Ctrl Pts',(-20.0576775108791,6.04137122992328,-5.78506070393765));
#66668=CARTESIAN_POINT('Ctrl Pts',(-20.0647009399416,6.08058632073389,-5.6660333520467));
#66669=CARTESIAN_POINT('Ctrl Pts',(-20.0717185423857,6.11976887880798,-5.54710474493479));
#66670=CARTESIAN_POINT('Ctrl Pts',(-20.0787361448298,6.16422430917893,-5.42981637531585));
#66671=CARTESIAN_POINT('Ctrl Pts',(-20.085753747274,6.21379041548669,-5.3146550947208));
#66672=CARTESIAN_POINT('Ctrl Pts',(-20.0927670920274,6.2633264492517,-5.19956368430097));
#66673=CARTESIAN_POINT('Ctrl Pts',(-20.0997804367809,6.31796683139565,-5.08659714716067));
#66674=CARTESIAN_POINT('Ctrl Pts',(-20.1067937815343,6.37750071407498,-4.97622373805349));
#66675=CARTESIAN_POINT('Ctrl Pts',(-20.1138574549108,6.43746181920613,-4.86505827581068));
#66676=CARTESIAN_POINT('Ctrl Pts',(-20.1209211282873,6.5023867959048,-4.75652367863071));
#66677=CARTESIAN_POINT('Ctrl Pts',(-20.1279848016638,6.57201228474143,-4.65107468067111));
#66678=CARTESIAN_POINT('Ctrl Pts',(-20.1349957589147,6.64111815923273,-4.54641264755664));
#66679=CARTESIAN_POINT('Ctrl Pts',(-20.1420067161656,6.71485438329882,-4.44479062478944));
#66680=CARTESIAN_POINT('Ctrl Pts',(-20.1490176734164,6.79291940437145,-4.34662499279219));
#66681=CARTESIAN_POINT('Ctrl Pts',(-20.1560293038896,6.87099192158304,-4.2484499345089));
#66682=CARTESIAN_POINT('Ctrl Pts',(-20.1630409343627,6.95339382288946,-4.15373223076921));
#66683=CARTESIAN_POINT('Ctrl Pts',(-20.1700525648358,7.03978297499938,-4.06285551846333));
#66684=CARTESIAN_POINT('Ctrl Pts',(-20.1770662859279,7.12619788528295,-3.97195170995291));
#66685=CARTESIAN_POINT('Ctrl Pts',(-20.1840800070199,7.21660214710082,-3.88489145349599));
#66686=CARTESIAN_POINT('Ctrl Pts',(-20.191093728112,7.3106167200912,-3.80202156757576));
#66687=CARTESIAN_POINT('Ctrl Pts',(-20.1981960793168,7.4058193246704,-3.71810448185337));
#66688=CARTESIAN_POINT('Ctrl Pts',(-20.2052984305217,7.50472380869981,-3.63848467191371));
#66689=CARTESIAN_POINT('Ctrl Pts',(-20.2124007817266,7.6069029600472,-3.5634794960569));
#66690=CARTESIAN_POINT('Ctrl Pts',(-20.2194267016631,7.70798252029948,-3.4892814811754));
#66691=CARTESIAN_POINT('Ctrl Pts',(-20.2264526215996,7.81226625486711,-3.41959943125368));
#66692=CARTESIAN_POINT('Ctrl Pts',(-20.2334785415361,7.91931293289363,-3.3546958798482));
#66693=CARTESIAN_POINT('Ctrl Pts',(-20.2406191083752,8.02810636724196,-3.28873325131098));
#66694=CARTESIAN_POINT('Ctrl Pts',(-20.2477596752143,8.13975333669771,-3.22770663540868));
#66695=CARTESIAN_POINT('Ctrl Pts',(-20.2549002420533,8.25376708692567,-3.17184182160537));
#66696=CARTESIAN_POINT('Ctrl Pts',(-20.2620408088924,8.36778083715362,-3.11597700780207));
#66697=CARTESIAN_POINT('Ctrl Pts',(-20.2691813757315,8.48416096703565,-3.06527411157802));
#66698=CARTESIAN_POINT('Ctrl Pts',(-20.2763219425705,8.60240284429547,-3.0199066245829));
#66699=CARTESIAN_POINT('Ctrl Pts',(-20.2831124685135,8.71484833401245,-2.97676311730259));
#66700=CARTESIAN_POINT('Ctrl Pts',(-20.2899029944564,8.82935140599041,-2.93830145149597));
#66701=CARTESIAN_POINT('Ctrl Pts',(-20.2966935203994,8.94547734886698,-2.90472719326246));
#66702=CARTESIAN_POINT('Ctrl Pts',(-20.3034748353439,9.06144577288687,-2.87119847677993));
#66703=CARTESIAN_POINT('Ctrl Pts',(-20.3102561502883,9.17903229471747,-2.842544107233));
#66704=CARTESIAN_POINT('Ctrl Pts',(-20.3170374652328,9.29778142242843,-2.81892200410919));
#66705=CARTESIAN_POINT('Ctrl Pts',(-20.3238114588109,9.41640234404969,-2.79532540430932));
#66706=CARTESIAN_POINT('Ctrl Pts',(-20.330585452389,9.53618296819803,-2.77675035206636));
#66707=CARTESIAN_POINT('Ctrl Pts',(-20.3373594459671,9.65665251765119,-2.76330503122583));
#66708=CARTESIAN_POINT('Ctrl Pts',(-20.3441279982186,9.77702529787156,-2.74987051056998));
#66709=CARTESIAN_POINT('Ctrl Pts',(-20.3508965504701,9.89808548802565,-2.74155757451038));
#66710=CARTESIAN_POINT('Ctrl Pts',(-20.3576651027216,10.0193527277818,-2.73842322861328));
#66711=CARTESIAN_POINT('Ctrl Pts',(-20.3644308259848,10.1405692826068,-2.73529019274934));
#66712=CARTESIAN_POINT('Ctrl Pts',(-20.371196549248,10.2619922966189,-2.73733145918129));
#66713=CARTESIAN_POINT('Ctrl Pts',(-20.3779622725112,10.383137499644,-2.74455207777438));
#66714=CARTESIAN_POINT('Ctrl Pts',(-20.384726762254,10.5042606155877,-2.75177137991097));
#66715=CARTESIAN_POINT('Ctrl Pts',(-20.3914912519967,10.6251056025061,-2.7641681330934));
#66716=CARTESIAN_POINT('Ctrl Pts',(-20.3982557417395,10.7451902242561,-2.78169529932278));
#66717=CARTESIAN_POINT('Ctrl Pts',(-20.405020688733,10.8652829632157,-2.79922365031404));
#66718=CARTESIAN_POINT('Ctrl Pts',(-20.4117856357265,10.9846148196652,-2.82188304272845));
#66719=CARTESIAN_POINT('Ctrl Pts',(-20.41855058272,11.1027114907248,-2.84957491402132));
#66720=CARTESIAN_POINT('Ctrl Pts',(-20.4253176780028,11.2208456647849,-2.87727557919678));
#66721=CARTESIAN_POINT('Ctrl Pts',(-20.4320847732856,11.3377434657248,-2.91001180325871));
#66722=CARTESIAN_POINT('Ctrl Pts',(-20.4388518685683,11.4529443165418,-2.9476347473342));
#66723=CARTESIAN_POINT('Ctrl Pts',(-20.4456269530807,11.5682811734314,-2.98530210904052));
#66724=CARTESIAN_POINT('Ctrl Pts',(-20.4524020375931,11.6819166829018,-3.0278675742583));
#66725=CARTESIAN_POINT('Ctrl Pts',(-20.4591771221056,11.7934087946616,-3.07513356621555));
#66726=CARTESIAN_POINT('Ctrl Pts',(-20.4659567627322,11.9049758827261,-3.12243134364499));
#66727=CARTESIAN_POINT('Ctrl Pts',(-20.4727364033589,12.0143963278875,-3.1744357569713));
#66728=CARTESIAN_POINT('Ctrl Pts',(-20.4795160439856,12.1212529943158,-3.23090342261781));
#66729=CARTESIAN_POINT('Ctrl Pts',(-20.4863065022887,12.2282801625317,-3.28746118875372));
#66730=CARTESIAN_POINT('Ctrl Pts',(-20.4930969605919,12.3327350284989,-3.34849620756881));
#66731=CARTESIAN_POINT('Ctrl Pts',(-20.499887418895,12.434229583985,-3.41372190917881));
#66732=CARTESIAN_POINT('Ctrl Pts',(-20.5029293567257,12.479696342509,-3.44294122257403));
#66733=CARTESIAN_POINT('Ctrl Pts',(-20.5059712945563,12.5245694743666,-3.47300098129164));
#66734=CARTESIAN_POINT('Ctrl Pts',(-20.5090132323869,12.5688163807365,-3.50387291497142));
#66735=CARTESIAN_POINT('Ctrl Pts',(-20.5160528500654,12.6712120645548,-3.57531639021697));
#66736=CARTESIAN_POINT('Ctrl Pts',(-20.5230924677439,12.7706045269319,-3.65135814019731));
#66737=CARTESIAN_POINT('Ctrl Pts',(-20.5301320854224,12.8665642076717,-3.73172086212295));
#66738=CARTESIAN_POINT('Ctrl Pts',(-20.5371627173815,12.9624014006857,-3.81198100505939));
#66739=CARTESIAN_POINT('Ctrl Pts',(-20.5441933493406,13.0548142404394,-3.89655089391907));
#66740=CARTESIAN_POINT('Ctrl Pts',(-20.5512239812998,13.1434028817285,-3.98511054605499));
#66741=CARTESIAN_POINT('Ctrl Pts',(-20.5582472086855,13.2318982225716,-4.07357692827592));
#66742=CARTESIAN_POINT('Ctrl Pts',(-20.5652704360712,13.3165771118334,-4.16602443564554));
#66743=CARTESIAN_POINT('Ctrl Pts',(-20.5722936634569,13.3970737490667,-4.26209372066711));
#66744=CARTESIAN_POINT('Ctrl Pts',(-20.579352449238,13.477977938426,-4.35864940167621));
#66745=CARTESIAN_POINT('Ctrl Pts',(-20.5864112350191,13.5546571020791,-4.45886338581479));
#66746=CARTESIAN_POINT('Ctrl Pts',(-20.5934700208002,13.6267777203579,-4.56233358584726));
#66747=CARTESIAN_POINT('Ctrl Pts',(-20.6004831025417,13.6984313739637,-4.6651338397634));
#66748=CARTESIAN_POINT('Ctrl Pts',(-20.6074961842832,13.7655851192017,-4.77114794331499));
#66749=CARTESIAN_POINT('Ctrl Pts',(-20.6145092660247,13.8279529364795,-4.87994932215142));
#66750=CARTESIAN_POINT('Ctrl Pts',(-20.6215201005457,13.8903007690717,-4.98871583747262));
#66751=CARTESIAN_POINT('Ctrl Pts',(-20.6285309350668,13.947865534977,-5.10026751473464));
#66752=CARTESIAN_POINT('Ctrl Pts',(-20.6355417695879,14.000405778642,-5.214150775436));
#66753=CARTESIAN_POINT('Ctrl Pts',(-20.6425517747268,14.0529398067936,-5.32802056374194));
#66754=CARTESIAN_POINT('Ctrl Pts',(-20.6495617798658,14.1004503352034,-5.44422103493076));
#66755=CARTESIAN_POINT('Ctrl Pts',(-20.6565717850048,14.1427430711648,-5.56227643416836));
#66756=CARTESIAN_POINT('Ctrl Pts',(-20.6636661797713,14.1855449463016,-5.68175303795214));
#66757=CARTESIAN_POINT('Ctrl Pts',(-20.6707605745379,14.2230024133749,-5.80312915290586));
#66758=CARTESIAN_POINT('Ctrl Pts',(-20.6778549693044,14.2549654534142,-5.92589395649855));
#66759=CARTESIAN_POINT('Ctrl Pts',(-20.6848700180614,14.2865710084581,-6.04728571875378));
#66760=CARTESIAN_POINT('Ctrl Pts',(-20.6918850668184,14.3128043681359,-6.17003487300886));
#66761=CARTESIAN_POINT('Ctrl Pts',(-20.6989001155754,14.3335717231044,-6.29363610865666));
#66762=CARTESIAN_POINT('Ctrl Pts',(-20.7060341833467,14.3546914220416,-6.41933439277077));
#66763=CARTESIAN_POINT('Ctrl Pts',(-20.713168251118,14.37015788043,-6.5459135246403));
#66764=CARTESIAN_POINT('Ctrl Pts',(-20.7203023188893,14.3799273655978,-6.6728361117461));
#66765=CARTESIAN_POINT('Ctrl Pts',(-20.7274363866606,14.3896968507655,-6.79975869885191));
#66766=CARTESIAN_POINT('Ctrl Pts',(-20.7345704544319,14.3937693782952,-6.92702432229997));
#66767=CARTESIAN_POINT('Ctrl Pts',(-20.7417045222032,14.3921567579672,-7.05409587559758));
#66768=CARTESIAN_POINT('Ctrl Pts',(-20.7487553738306,14.3905629482322,-7.17968518832687));
#66769=CARTESIAN_POINT('Ctrl Pts',(-20.755806225458,14.3834131442202,-7.30531135250305));
#66770=CARTESIAN_POINT('Ctrl Pts',(-20.7628570770854,14.3707114727388,-7.43045817858265));
#66771=CARTESIAN_POINT('Ctrl Pts',(-20.7699025977755,14.35801940461,-7.55551038490363));
#66772=CARTESIAN_POINT('Ctrl Pts',(-20.7769481184657,14.339783866004,-7.68008359541989));
#66773=CARTESIAN_POINT('Ctrl Pts',(-20.7839936391558,14.316060990687,-7.80366415327441));
#66774=CARTESIAN_POINT('Ctrl Pts',(-20.7910351758234,14.2923515299169,-7.92717483017315));
#66775=CARTESIAN_POINT('Ctrl Pts',(-20.7980767124911,14.2631609851212,-8.0496935975355));
#66776=CARTESIAN_POINT('Ctrl Pts',(-20.8051182491587,14.2285969725616,-8.17071474302503));
#66777=CARTESIAN_POINT('Ctrl Pts',(-20.8121573620581,14.1940448572855,-8.29169423180984));
#66778=CARTESIAN_POINT('Ctrl Pts',(-20.8191964749575,14.1541230641496,-8.41117675831594));
#66779=CARTESIAN_POINT('Ctrl Pts',(-20.8262355878569,14.108989607831,-8.52866983392907));
#66780=CARTESIAN_POINT('Ctrl Pts',(-20.8332745473014,14.0638571354359,-8.64616034815655));
#66781=CARTESIAN_POINT('Ctrl Pts',(-20.8403135067459,14.0135133592023,-8.76166113931436));
#66782=CARTESIAN_POINT('Ctrl Pts',(-20.8473524661904,13.9581651263394,-8.87469793576249));
#66783=CARTESIAN_POINT('Ctrl Pts',(-20.8509183664974,13.9301259989493,-8.93196178993535));
#66784=CARTESIAN_POINT('Ctrl Pts',(-20.8544842668044,13.9008033009508,-8.98859361159937));
#66785=CARTESIAN_POINT('Ctrl Pts',(-20.8580501671115,13.8702285225073,-9.04453396178702));
#66786=CARTESIAN_POINT('Ctrl Pts',(-20.8656423239006,13.8051317750523,-9.16363653698444));
#66787=CARTESIAN_POINT('Ctrl Pts',(-20.8732344806897,13.7343815652685,-9.27955752070515));
#66788=CARTESIAN_POINT('Ctrl Pts',(-20.8808266374789,13.6583076665164,-9.39179544542065));
#66789=CARTESIAN_POINT('Ctrl Pts',(-20.8886240686906,13.580176904863,-9.50706802495553));
#66790=CARTESIAN_POINT('Ctrl Pts',(-20.8964214999023,13.4964306780399,-9.61845531819866));
#66791=CARTESIAN_POINT('Ctrl Pts',(-20.9042189311141,13.4074713236086,-9.72544913759181));
#66792=CARTESIAN_POINT('Ctrl Pts',(-20.9118275959575,13.3206655674336,-9.82985276616849));
#66793=CARTESIAN_POINT('Ctrl Pts',(-20.9194362608009,13.2288963926098,-9.93007301888365));
#66794=CARTESIAN_POINT('Ctrl Pts',(-20.9270449256444,13.1325767406687,-10.0256733283113));
#66795=CARTESIAN_POINT('Ctrl Pts',(-20.9349367400403,13.032672640352,-10.1248313164362));
#66796=CARTESIAN_POINT('Ctrl Pts',(-20.9428285544361,12.9278730596352,-10.2190186506558));
#66797=CARTESIAN_POINT('Ctrl Pts',(-20.950720368832,12.818679347433,-10.3077913231248));
#66798=CARTESIAN_POINT('Ctrl Pts',(-20.9586121832279,12.7094856352308,-10.3965639955938));
#66799=CARTESIAN_POINT('Ctrl Pts',(-20.9665039976238,12.5958980403164,-10.4799218091269));
#66800=CARTESIAN_POINT('Ctrl Pts',(-20.9743958120197,12.4784556130269,-10.5574677128583));
#66801=CARTESIAN_POINT('Ctrl Pts',(-20.9814300607243,12.3737750920986,-10.6265870744537));
#66802=CARTESIAN_POINT('Ctrl Pts',(-20.9884643094289,12.2659695289948,-10.6911298205444));
#66803=CARTESIAN_POINT('Ctrl Pts',(-20.9954985581336,12.1554703093618,-10.7508150188439));
#66804=CARTESIAN_POINT('Ctrl Pts',(-21.0025288485313,12.045033269762,-10.8104666311358));
#66805=CARTESIAN_POINT('Ctrl Pts',(-21.0095591389291,11.9319059302526,-10.8652659569974));
#66806=CARTESIAN_POINT('Ctrl Pts',(-21.0165894293269,11.8165461611719,-10.9149769156504));
#66807=CARTESIAN_POINT('Ctrl Pts',(-21.0205783820181,11.7510915874208,-10.9431826726081));
#66808=CARTESIAN_POINT('Ctrl Pts',(-21.0245673347093,11.684918780429,-10.969751120246));
#66809=CARTESIAN_POINT('Ctrl Pts',(-21.0285562874006,11.6181146495903,-10.9946458447559));
#66810=CARTESIAN_POINT('Origin',(-23.734,10.1295,-7.));
#66811=CARTESIAN_POINT('',(-22.5286570444943,11.618114651272,-10.9946458441291));
#66812=CARTESIAN_POINT('',(-22.1191569086782,11.6181146495903,-10.9946458447559));
#66813=CARTESIAN_POINT('',(-23.734,11.6181146495903,-10.9946458447559));
#66814=CARTESIAN_POINT('',(-23.534,12.9193325810254,-3.77664721604209));
#66815=CARTESIAN_POINT('Ctrl Pts',(-23.534,12.9193325810254,-3.7766472160421));
#66816=CARTESIAN_POINT('Ctrl Pts',(-23.5090016758881,12.5818064945809,-3.4845162158006));
#66817=CARTESIAN_POINT('Ctrl Pts',(-23.484592830165,12.2004820816042,-3.24720404572943));
#66818=CARTESIAN_POINT('Ctrl Pts',(-23.4464839655589,11.5791039345357,-2.98454272618526));
#66819=CARTESIAN_POINT('Ctrl Pts',(-23.4335068125947,11.3621073396055,-2.91271141912405));
#66820=CARTESIAN_POINT('Ctrl Pts',(-23.3973171935771,10.7367537118015,-2.76006416037631));
#66821=CARTESIAN_POINT('Ctrl Pts',(-23.3746868396262,10.3208579053535,-2.72107458050878));
#66822=CARTESIAN_POINT('Ctrl Pts',(-23.3367605198731,9.64691836463789,-2.75646976697985));
#66823=CARTESIAN_POINT('Ctrl Pts',(-23.3220373816232,9.3897063732441,-2.79367902397596));
#66824=CARTESIAN_POINT('Ctrl Pts',(-23.2925172001717,8.87968350748323,-2.91571422403364));
#66825=CARTESIAN_POINT('Ctrl Pts',(-23.2779320658428,8.62820751784597,-3.00130584031873));
#66826=CARTESIAN_POINT('Ctrl Pts',(-23.2322650016507,7.87791905695821,-3.33750035182252));
#66827=CARTESIAN_POINT('Ctrl Pts',(-23.2006283778644,7.41908692516015,-3.66275820743672));
#66828=CARTESIAN_POINT('Ctrl Pts',(-23.1541830548561,6.84351004176925,-4.26987945763089));
#66829=CARTESIAN_POINT('Ctrl Pts',(-23.138764797502,6.67163085484486,-4.49113043515536));
#66830=CARTESIAN_POINT('Ctrl Pts',(-23.1094026333514,6.39258651629209,-4.93404287435651));
#66831=CARTESIAN_POINT('Ctrl Pts',(-23.0955826074097,6.28049087961493,-5.15126367730691));
#66832=CARTESIAN_POINT('Ctrl Pts',(-23.0502851047814,5.97511370653541,-5.89289766113601));
#66833=CARTESIAN_POINT('Ctrl Pts',(-23.0200794903383,5.8660154708496,-6.44565312269876));
#66834=CARTESIAN_POINT('Ctrl Pts',(-22.9755292798195,5.86670271206618,-7.23455531700981));
#66835=CARTESIAN_POINT('Ctrl Pts',(-22.9624255642123,5.88565354052962,-7.46500360398424));
#66836=CARTESIAN_POINT('Ctrl Pts',(-22.9360178923028,5.96242869756211,-7.93115308143177));
#66837=CARTESIAN_POINT('Ctrl Pts',(-22.9227269527656,6.02187927087701,-8.16575496768535));
#66838=CARTESIAN_POINT('Ctrl Pts',(-22.8885016510635,6.2230623764673,-8.74714389776903));
#66839=CARTESIAN_POINT('Ctrl Pts',(-22.8673967100352,6.39113240840198,-9.08263163558883));
#66840=CARTESIAN_POINT('Ctrl Pts',(-22.8313068463502,6.75008956149188,-9.61220121735023));
#66841=CARTESIAN_POINT('Ctrl Pts',(-22.8166199946301,6.91972932205428,-9.81804642132396));
#66842=CARTESIAN_POINT('Ctrl Pts',(-22.7764052945812,7.43090592911632,-10.3318258316762));
#66843=CARTESIAN_POINT('Ctrl Pts',(-22.7505241782358,7.80470051667608,-10.6026024093102));
#66844=CARTESIAN_POINT('Ctrl Pts',(-22.6994601906312,8.61575317480828,-11.0104340665967));
#66845=CARTESIAN_POINT('Ctrl Pts',(-22.6750348689543,9.0465220160346,-11.1475503300876));
#66846=CARTESIAN_POINT('Ctrl Pts',(-22.6356423579933,9.73858190014085,-11.2524342877029));
#66847=CARTESIAN_POINT('Ctrl Pts',(-22.6214059145636,9.98926909238338,-11.26806137762));
#66848=CARTESIAN_POINT('Ctrl Pts',(-22.5828682290083,10.6746545951026,-11.2503104255814));
#66849=CARTESIAN_POINT('Ctrl Pts',(-22.5592036554187,11.1051607797456,-11.1725799713837));
#66850=CARTESIAN_POINT('Ctrl Pts',(-22.532713960555,11.5504911528519,-11.0193594451106));
#66851=CARTESIAN_POINT('Ctrl Pts',(-22.5306862986621,11.5843873590537,-11.0072144029709));
#66852=CARTESIAN_POINT('Ctrl Pts',(-22.5286570444943,11.618114651272,-10.9946458441291));
#66853=CARTESIAN_POINT('',(-23.533999981871,12.9193850840203,-10.2235360174615));
#66854=CARTESIAN_POINT('Origin',(-23.534,10.1295,-7.));
#66855=CARTESIAN_POINT('',(-22.2043183294109,10.1295365072714,-11.2628938598663));
#66856=CARTESIAN_POINT('Ctrl Pts',(-23.533999981871,12.9193850840203,-10.2235360174615));
#66857=CARTESIAN_POINT('Ctrl Pts',(-23.5009788547478,13.3648360859832,-9.83730561563166));
#66858=CARTESIAN_POINT('Ctrl Pts',(-23.4291758459887,14.1588395586771,-8.79502344007021));
#66859=CARTESIAN_POINT('Ctrl Pts',(-23.3185909555933,14.5604905826756,-6.80076298861617));
#66860=CARTESIAN_POINT('Ctrl Pts',(-23.2022453106852,13.9513208636606,-4.74899583476332));
#66861=CARTESIAN_POINT('Ctrl Pts',(-23.0858996657769,12.452270995998,-3.22136570469558));
#66862=CARTESIAN_POINT('Ctrl Pts',(-22.9695540208687,10.4123750626855,-2.57356516157568));
#66863=CARTESIAN_POINT('Ctrl Pts',(-22.8532083759605,8.30661439543301,-2.9564333045403));
#66864=CARTESIAN_POINT('Ctrl Pts',(-22.7368627310523,6.62530205950465,-4.28082127060911));
#66865=CARTESIAN_POINT('Ctrl Pts',(-22.6205170861441,5.75991783379543,-6.23835174036327));
#66866=CARTESIAN_POINT('Ctrl Pts',(-22.5041714412359,5.9119701463398,-8.37323075593554));
#66867=CARTESIAN_POINT('Ctrl Pts',(-22.3878257963277,7.04603468702391,-10.1883540588533));
#66868=CARTESIAN_POINT('Ctrl Pts',(-22.2878747590527,8.63711446750853,-11.1099400088585));
#66869=CARTESIAN_POINT('Ctrl Pts',(-22.2267056034138,9.72970022779226,-11.2625492465514));
#66870=CARTESIAN_POINT('Ctrl Pts',(-22.2043183294109,10.1295365056039,-11.2626991438894));
#66871=CARTESIAN_POINT('Ctrl Pts',(-22.2043183294109,10.1295365081804,-11.2629999998437));
#66872=CARTESIAN_POINT('Ctrl Pts',(-22.1969189537551,10.2616985400649,-11.2629988680127));
#66873=CARTESIAN_POINT('Ctrl Pts',(-22.1895195780993,10.3938406290833,-11.2568474434062));
#66874=CARTESIAN_POINT('Ctrl Pts',(-22.1821202024435,10.5253950557853,-11.2445772586684));
#66875=CARTESIAN_POINT('Ctrl Pts',(-22.1747186558373,10.6569880800863,-11.2323034739021));
#66876=CARTESIAN_POINT('Ctrl Pts',(-22.1673171092312,10.787992785182,-11.2139073736702));
#66877=CARTESIAN_POINT('Ctrl Pts',(-22.159915562625,10.9178466698904,-11.1894723448273));
#66878=CARTESIAN_POINT('Ctrl Pts',(-22.1583218772538,10.9458065338847,-11.1842110460631));
#66879=CARTESIAN_POINT('Ctrl Pts',(-22.1567281918825,10.9737130747606,-11.1786699613312));
#66880=CARTESIAN_POINT('Ctrl Pts',(-22.1551345065113,11.0015607336212,-11.1728502341776));
#66881=CARTESIAN_POINT('Ctrl Pts',(-22.1478857890208,11.1282230068014,-11.1463797910337));
#66882=CARTESIAN_POINT('Ctrl Pts',(-22.1406370715302,11.2537022086528,-11.1141332404387));
#66883=CARTESIAN_POINT('Ctrl Pts',(-22.1333883540397,11.3774686349185,-11.0762413184525));
#66884=CARTESIAN_POINT('Ctrl Pts',(-22.1286445389192,11.4584657278658,-11.0514435148828));
#66885=CARTESIAN_POINT('Ctrl Pts',(-22.1239007237987,11.5387294697866,-11.0242289282653));
#66886=CARTESIAN_POINT('Ctrl Pts',(-22.1191569086782,11.6181146495903,-10.9946458447559));
#66887=CARTESIAN_POINT('Origin',(-18.734,-18.952,0.));
#66888=CARTESIAN_POINT('',(-20.7225805821494,-19.6781103692267,-21.2464098430158));
#66889=CARTESIAN_POINT('',(-20.722580582091,-19.6781103693865,-21.465822579505));
#66890=CARTESIAN_POINT('',(-20.7225805821191,-19.6781103693095,0.));
#66891=CARTESIAN_POINT('',(-20.8509993841958,-18.953614718169,-21.5109437210328));
#66892=CARTESIAN_POINT('Ctrl Pts',(-20.722580582091,-19.6781103693865,-21.465822579505));
#66893=CARTESIAN_POINT('Ctrl Pts',(-20.7235155796043,-19.6755497147289,
-21.4659707954636));
#66894=CARTESIAN_POINT('Ctrl Pts',(-20.7244456404574,-19.6729872286501,
-21.4661190479908));
#66895=CARTESIAN_POINT('Ctrl Pts',(-20.7392637896057,-19.6319133320967,
-21.4684943566896));
#66896=CARTESIAN_POINT('Ctrl Pts',(-20.752036519493,-19.5930097144133,-21.4707296572491));
#66897=CARTESIAN_POINT('Ctrl Pts',(-20.7690503572088,-19.5356239558152,
-21.4740356753045));
#66898=CARTESIAN_POINT('Ctrl Pts',(-20.7741842861848,-19.5174157143311,
-21.4750859568108));
#66899=CARTESIAN_POINT('Ctrl Pts',(-20.7947015602454,-19.4407274461673,
-21.4795238028831));
#66900=CARTESIAN_POINT('Ctrl Pts',(-20.8078182966199,-19.3816762398259,
-21.4829755341861));
#66901=CARTESIAN_POINT('Ctrl Pts',(-20.8199726159277,-19.3132330043184,
-21.4870989280524));
#66902=CARTESIAN_POINT('Ctrl Pts',(-20.8214990062904,-19.3043051658438,
-21.4876391708838));
#66903=CARTESIAN_POINT('Ctrl Pts',(-20.8236943731102,-19.2909490836379,
-21.4884513018792));
#66904=CARTESIAN_POINT('Ctrl Pts',(-20.8244066869518,-19.2865279309743,
-21.4887207763421));
#66905=CARTESIAN_POINT('Ctrl Pts',(-20.8256596197291,-19.2785910105057,
-21.4892057453182));
#66906=CARTESIAN_POINT('Ctrl Pts',(-20.8262054097228,-19.2750761148281,
-21.4894209425139));
#66907=CARTESIAN_POINT('Ctrl Pts',(-20.8272520454122,-19.2682218781208,
-21.4898414207746));
#66908=CARTESIAN_POINT('Ctrl Pts',(-20.8277537589423,-19.2648827230304,
-21.4900466455382));
#66909=CARTESIAN_POINT('Ctrl Pts',(-20.8288495023066,-19.257469335688,-21.4905030984026));
#66910=CARTESIAN_POINT('Ctrl Pts',(-20.8294396375628,-19.2533945537653,
-21.4907545413552));
#66911=CARTESIAN_POINT('Ctrl Pts',(-20.8308795084341,-19.2432438265539,
-21.4913822453917));
#66912=CARTESIAN_POINT('Ctrl Pts',(-20.8317147195046,-19.2371659041556,
-21.4917592813314));
#66913=CARTESIAN_POINT('Ctrl Pts',(-20.835602193926,-19.2079347725518,-21.4935780223869));
#66914=CARTESIAN_POINT('Ctrl Pts',(-20.8382974849493,-19.1847367233153,
-21.4950377275373));
#66915=CARTESIAN_POINT('Ctrl Pts',(-20.8474812907066,-19.0923897727793,
-21.5009009877621));
#66916=CARTESIAN_POINT('Ctrl Pts',(-20.8509485267258,-19.0229896553394,
-21.5054226551349));
#66917=CARTESIAN_POINT('Ctrl Pts',(-20.8509994311328,-18.953551961105,-21.509989519712));
#66918=CARTESIAN_POINT('',(-17.1140743056113,-20.3149122292574,-22.));
#66919=CARTESIAN_POINT('Ctrl Pts',(-20.8509993841958,-18.953614718169,-21.5109437210328));
#66920=CARTESIAN_POINT('Ctrl Pts',(-20.8510560133107,-18.8793703058911,
-21.5154240901546));
#66921=CARTESIAN_POINT('Ctrl Pts',(-20.8472020782088,-18.804981409641,-21.5199044592764));
#66922=CARTESIAN_POINT('Ctrl Pts',(-20.8394225349145,-18.7309005891588,
-21.5243848283982));
#66923=CARTESIAN_POINT('Ctrl Pts',(-20.8319236702397,-18.6594925351418,
-21.5287035500076));
#66924=CARTESIAN_POINT('Ctrl Pts',(-20.820777658289,-18.5883712544674,-21.5330222716171));
#66925=CARTESIAN_POINT('Ctrl Pts',(-20.8060239432422,-18.5179426551354,
-21.5373409932266));
#66926=CARTESIAN_POINT('Ctrl Pts',(-20.791280056931,-18.4475609744317,-21.5416568377592));
#66927=CARTESIAN_POINT('Ctrl Pts',(-20.7729333337529,-18.3778715449745,
-21.5459726822918));
#66928=CARTESIAN_POINT('Ctrl Pts',(-20.7510747171251,-18.3092725417919,
-21.5502885268244));
#66929=CARTESIAN_POINT('Ctrl Pts',(-20.7292229915306,-18.2406951647726,
-21.5546030107664));
#66930=CARTESIAN_POINT('Ctrl Pts',(-20.7038617199401,-18.1732080048576,
-21.5589174947085));
#66931=CARTESIAN_POINT('Ctrl Pts',(-20.6751318662711,-18.1071946509717,
-21.5632319786505));
#66932=CARTESIAN_POINT('Ctrl Pts',(-20.646400988223,-18.0411789433423,-21.5675466164279));
#66933=CARTESIAN_POINT('Ctrl Pts',(-20.6143014909514,-17.9766376000802,
-21.5718612542053));
#66934=CARTESIAN_POINT('Ctrl Pts',(-20.5790219474228,-17.9139330399593,
-21.5761758919827));
#66935=CARTESIAN_POINT('Ctrl Pts',(-20.5437075154313,-17.8511664703707,
-21.5804947965692));
#66936=CARTESIAN_POINT('Ctrl Pts',(-20.5052070087195,-17.7902407402828,
-21.5848137011558));
#66937=CARTESIAN_POINT('Ctrl Pts',(-20.4637537458688,-17.7314915081602,
-21.5891326057424));
#66938=CARTESIAN_POINT('Ctrl Pts',(-20.4222758278492,-17.6727073337405,
-21.593454079085));
#66939=CARTESIAN_POINT('Ctrl Pts',(-20.3778419690816,-17.6161026206995,
-21.5977755524276));
#66940=CARTESIAN_POINT('Ctrl Pts',(-20.3307256571012,-17.561979792969,-21.6020970257703));
#66941=CARTESIAN_POINT('Ctrl Pts',(-20.2835347568318,-17.507771285164,-21.6064253402958));
#66942=CARTESIAN_POINT('Ctrl Pts',(-20.2336532809969,-17.4560528519306,
-21.6107536548212));
#66943=CARTESIAN_POINT('Ctrl Pts',(-20.1813905809776,-17.4070891591754,
-21.6150819693466));
#66944=CARTESIAN_POINT('Ctrl Pts',(-20.1677438166228,-17.3943038270605,
-21.616212172883));
#66945=CARTESIAN_POINT('Ctrl Pts',(-20.1539348588654,-17.3817060999665,
-21.6173423764194));
#66946=CARTESIAN_POINT('Ctrl Pts',(-20.1399695509607,-17.369300211104,-21.6184725799558));
#66947=CARTESIAN_POINT('Ctrl Pts',(-20.0856805133166,-17.3210732925096,
-21.6228661574372));
#66948=CARTESIAN_POINT('Ctrl Pts',(-20.0288041823845,-17.2755513561322,
-21.6272597349186));
#66949=CARTESIAN_POINT('Ctrl Pts',(-19.969640873017,-17.2330233762701,-21.6316533124001));
#66950=CARTESIAN_POINT('Ctrl Pts',(-19.9105638618643,-17.1905574295968,
-21.6360404812154));
#66951=CARTESIAN_POINT('Ctrl Pts',(-19.849206882515,-17.1510770477242,-21.6404276500308));
#66952=CARTESIAN_POINT('Ctrl Pts',(-19.7859046048043,-17.1148321518186,
-21.6448148188462));
#66953=CARTESIAN_POINT('Ctrl Pts',(-19.7226747936877,-17.0786287480086,
-21.6491969653592));
#66954=CARTESIAN_POINT('Ctrl Pts',(-19.6575045236034,-17.0456537097674,
-21.6535791118721));
#66955=CARTESIAN_POINT('Ctrl Pts',(-19.5907574447862,-17.0161137221408,
-21.6579612583851));
#66956=CARTESIAN_POINT('Ctrl Pts',(-19.524051506928,-16.9865919421039,-21.6623407038703));
#66957=CARTESIAN_POINT('Ctrl Pts',(-19.4557711276412,-16.960501205489,-21.6667201493556));
#66958=CARTESIAN_POINT('Ctrl Pts',(-19.3863033026644,-16.9380016382,-21.6710995948408));
#66959=CARTESIAN_POINT('Ctrl Pts',(-19.3168555527303,-16.9155085729106,
-21.6754777747394));
#66960=CARTESIAN_POINT('Ctrl Pts',(-19.2462214956912,-16.8966047644762,
-21.6798559546379));
#66961=CARTESIAN_POINT('Ctrl Pts',(-19.1748052243022,-16.8814011121833,
-21.6842341345365));
#66962=CARTESIAN_POINT('Ctrl Pts',(-19.10338621101,-16.8661968761726,-21.6886124825276));
#66963=CARTESIAN_POINT('Ctrl Pts',(-19.0311853945028,-16.8546931765608,
-21.6929908305188));
#66964=CARTESIAN_POINT('Ctrl Pts',(-18.958617414822,-16.8469498778037,-21.6973691785099));
#66965=CARTESIAN_POINT('Ctrl Pts',(-18.8859734847581,-16.8391984748317,
-21.7017521089244));
#66966=CARTESIAN_POINT('Ctrl Pts',(-18.8129621034892,-16.835215381558,-21.7061350393389));
#66967=CARTESIAN_POINT('Ctrl Pts',(-18.7400025813939,-16.8350085099329,
-21.7105179697534));
#66968=CARTESIAN_POINT('Ctrl Pts',(-18.6670027054265,-16.8348015238872,
-21.7149033243644));
#66969=CARTESIAN_POINT('Ctrl Pts',(-18.5940552263849,-16.8383748946447,
-21.7192886789753));
#66970=CARTESIAN_POINT('Ctrl Pts',(-18.5215762918332,-16.8456844566379,
-21.7236740335863));
#66971=CARTESIAN_POINT('Ctrl Pts',(-18.4489692699444,-16.8530069363477,
-21.728067138151));
#66972=CARTESIAN_POINT('Ctrl Pts',(-18.3768329218414,-16.8640787198162,
-21.7324602427158));
#66973=CARTESIAN_POINT('Ctrl Pts',(-18.3055745682925,-16.8788042423673,
-21.7368533472805));
#66974=CARTESIAN_POINT('Ctrl Pts',(-18.2580212556926,-16.8886311235987,
-21.739785027066));
#66975=CARTESIAN_POINT('Ctrl Pts',(-18.2108587080193,-16.900084095337,-21.7427167068516));
#66976=CARTESIAN_POINT('Ctrl Pts',(-18.1642037039559,-16.913122568418,-21.7456483866372));
#66977=CARTESIAN_POINT('Ctrl Pts',(-18.0951065059757,-16.932432864793,-21.7499902758433));
#66978=CARTESIAN_POINT('Ctrl Pts',(-18.0268409185985,-16.9553020920462,
-21.7543321650495));
#66979=CARTESIAN_POINT('Ctrl Pts',(-17.9598056269363,-16.9816416385042,
-21.7586740542557));
#66980=CARTESIAN_POINT('Ctrl Pts',(-17.8928712802768,-17.007941521592,-21.7630094052339));
#66981=CARTESIAN_POINT('Ctrl Pts',(-17.8271640088704,-17.0377011783514,
-21.7673447562122));
#66982=CARTESIAN_POINT('Ctrl Pts',(-17.7630690182321,-17.0707817700641,
-21.7716801071904));
#66983=CARTESIAN_POINT('Ctrl Pts',(-17.6990476945068,-17.1038243409416,
-21.7760104753779));
#66984=CARTESIAN_POINT('Ctrl Pts',(-17.6366354094004,-17.140180045608,-21.7803408435655));
#66985=CARTESIAN_POINT('Ctrl Pts',(-17.576197298269,-17.1796620232404,-21.784671211753));
#66986=CARTESIAN_POINT('Ctrl Pts',(-17.5157963311547,-17.2191197360633,
-21.7889989185855));
#66987=CARTESIAN_POINT('Ctrl Pts',(-17.4573675446825,-17.2616996436244,
-21.793326625418));
#66988=CARTESIAN_POINT('Ctrl Pts',(-17.4012499559382,-17.3071698202996,
-21.7976543322506));
#66989=CARTESIAN_POINT('Ctrl Pts',(-17.3451474140536,-17.3526278050152,
-21.8019808786911));
#66990=CARTESIAN_POINT('Ctrl Pts',(-17.2913552237362,-17.4009742110386,
-21.8063074251317));
#66991=CARTESIAN_POINT('Ctrl Pts',(-17.2401804886106,-17.4519359122383,
-21.8106339715723));
#66992=CARTESIAN_POINT('Ctrl Pts',(-17.1890017454992,-17.502901604739,-21.8149608568663));
#66993=CARTESIAN_POINT('Ctrl Pts',(-17.1404412125279,-17.5564826492106,
-21.8192877421603));
#66994=CARTESIAN_POINT('Ctrl Pts',(-17.0947688687351,-17.6123693425829,
-21.8236146274544));
#66995=CARTESIAN_POINT('Ctrl Pts',(-17.0490417134499,-17.6683231057134,
-21.8279467054541));
#66996=CARTESIAN_POINT('Ctrl Pts',(-17.0062099790967,-17.7265876580954,
-21.8322787834538));
#66997=CARTESIAN_POINT('Ctrl Pts',(-16.9665025074284,-17.7868212095334,
-21.8366108614535));
#66998=CARTESIAN_POINT('Ctrl Pts',(-16.9267705288898,-17.8470919362378,
-21.8409456131484));
#66999=CARTESIAN_POINT('Ctrl Pts',(-16.8901668972173,-17.9093336530359,
-21.8452803648433));
#67000=CARTESIAN_POINT('Ctrl Pts',(-16.8568748225048,-17.9731792462286,
-21.8496151165381));
#67001=CARTESIAN_POINT('Ctrl Pts',(-16.8235156981184,-18.0371534233633,
-21.8539585983494));
#67002=CARTESIAN_POINT('Ctrl Pts',(-16.7934816509746,-18.1027374769631,
-21.8583020801606));
#67003=CARTESIAN_POINT('Ctrl Pts',(-16.7669077870852,-18.1695441061056,
-21.8626455619719));
#67004=CARTESIAN_POINT('Ctrl Pts',(-16.7461498194961,-18.221729586104,-21.8660384390875));
#67005=CARTESIAN_POINT('Ctrl Pts',(-16.7275022238381,-18.2746606281223,
-21.869431316203));
#67006=CARTESIAN_POINT('Ctrl Pts',(-16.7110077838934,-18.328147859207,-21.8728241933186));
#67007=CARTESIAN_POINT('Ctrl Pts',(-16.6890805388882,-18.3992522813377,
-21.8773345888236));
#67008=CARTESIAN_POINT('Ctrl Pts',(-16.6708712302021,-18.471627433023,-21.8818449843287));
#67009=CARTESIAN_POINT('Ctrl Pts',(-16.65651913225,-18.5448609032129,-21.8863553798337));
#67010=CARTESIAN_POINT('Ctrl Pts',(-16.6414517292682,-18.6217443115328,
-21.8910905723407));
#67011=CARTESIAN_POINT('Ctrl Pts',(-16.6306362647773,-18.699573380232,-21.8958257648476));
#67012=CARTESIAN_POINT('Ctrl Pts',(-16.6241750600365,-18.7778514349529,
-21.9005609573545));
#67013=CARTESIAN_POINT('Ctrl Pts',(-16.6180410539461,-18.8521654497015,
-21.9050563573367));
#67014=CARTESIAN_POINT('Ctrl Pts',(-16.6158311159158,-18.9268835670766,
-21.9095517573189));
#67015=CARTESIAN_POINT('Ctrl Pts',(-16.6175804464527,-19.001570892293,-21.9140471573011));
#67016=CARTESIAN_POINT('Ctrl Pts',(-16.6193281321099,-19.0761879896894,
-21.9185383302991));
#67017=CARTESIAN_POINT('Ctrl Pts',(-16.6250276759246,-19.1507739043837,
-21.9230295032971));
#67018=CARTESIAN_POINT('Ctrl Pts',(-16.6346622676094,-19.2248920763987,
-21.9275206762951));
#67019=CARTESIAN_POINT('Ctrl Pts',(-16.6442903170874,-19.2989599197204,
-21.932008799638));
#67020=CARTESIAN_POINT('Ctrl Pts',(-16.6578480436051,-19.3725602066461,
-21.9364969229808));
#67021=CARTESIAN_POINT('Ctrl Pts',(-16.6752667781491,-19.4452611085899,
-21.9409850463236));
#67022=CARTESIAN_POINT('Ctrl Pts',(-16.6926782312815,-19.5179316199686,
-21.9454712935328));
#67023=CARTESIAN_POINT('Ctrl Pts',(-16.7139473766674,-19.5897030572418,
-21.949957540742));
#67024=CARTESIAN_POINT('Ctrl Pts',(-16.7389546395216,-19.6601546509298,
-21.9544437879513));
#67025=CARTESIAN_POINT('Ctrl Pts',(-16.7639650091895,-19.7306149972742,
-21.9589305925159));
#67026=CARTESIAN_POINT('Ctrl Pts',(-16.792714280612,-19.7997547457854,-21.9634173970806));
#67027=CARTESIAN_POINT('Ctrl Pts',(-16.8250335623977,-19.8671700061235,
-21.9679042016453));
#67028=CARTESIAN_POINT('Ctrl Pts',(-16.8573543979593,-19.9345885075052,
-21.9723912219168));
#67029=CARTESIAN_POINT('Ctrl Pts',(-16.8932453841005,-20.0002819530908,
-21.9768782421882));
#67030=CARTESIAN_POINT('Ctrl Pts',(-16.9324909433493,-20.0638696500964,
-21.9813652624597));
#67031=CARTESIAN_POINT('Ctrl Pts',(-16.971763585854,-20.1275012288023,-21.9858553792119));
#67032=CARTESIAN_POINT('Ctrl Pts',(-17.0143951804746,-20.1890237784353,
-21.9903454959641));
#67033=CARTESIAN_POINT('Ctrl Pts',(-17.0601263939598,-20.2480849320172,
-21.9948356127163));
#67034=CARTESIAN_POINT('Ctrl Pts',(-17.0776592489258,-20.2707283425231,
-21.9965570751442));
#67035=CARTESIAN_POINT('Ctrl Pts',(-17.0956472766607,-20.2930102923405,
-21.9982785375721));
#67036=CARTESIAN_POINT('Ctrl Pts',(-17.1140743056112,-20.3149122292573,
-22.));
#67037=CARTESIAN_POINT('',(-20.3539401105369,-20.3148950943758,-21.9999997808643));
#67038=CARTESIAN_POINT('Origin',(-18.734,-18.952,-22.));
#67039=CARTESIAN_POINT('',(-20.8509997094769,-18.9531090873175,-21.2890562790225));
#67040=CARTESIAN_POINT('Ctrl Pts',(-20.3539401105369,-20.3148950943758,
-21.9999997808643));
#67041=CARTESIAN_POINT('Ctrl Pts',(-20.3072932296543,-20.3703396797185,
-21.9956147616661));
#67042=CARTESIAN_POINT('Ctrl Pts',(-20.2577049138449,-20.4234955896159,
-21.9912297424679));
#67043=CARTESIAN_POINT('Ctrl Pts',(-20.2054285432655,-20.4740338504986,
-21.9868447232696));
#67044=CARTESIAN_POINT('Ctrl Pts',(-20.1532297926735,-20.5244970721403,
-21.9824662149506));
#67045=CARTESIAN_POINT('Ctrl Pts',(-20.0983512546661,-20.5723500270703,
-21.9780877066316));
#67046=CARTESIAN_POINT('Ctrl Pts',(-20.0410860694924,-20.6172972728431,
-21.9737091983125));
#67047=CARTESIAN_POINT('Ctrl Pts',(-19.983888278367,-20.6621916212607,-21.9693358429569));
#67048=CARTESIAN_POINT('Ctrl Pts',(-19.9243097978752,-20.7041867567888,
-21.9649624876012));
#67049=CARTESIAN_POINT('Ctrl Pts',(-19.8626788010172,-20.7430257296126,
-21.9605891322455));
#67050=CARTESIAN_POINT('Ctrl Pts',(-19.8010868010387,-20.7818401271607,
-21.956218544121));
#67051=CARTESIAN_POINT('Ctrl Pts',(-19.7374452692593,-20.8175020674031,
-21.9518479559964));
#67052=CARTESIAN_POINT('Ctrl Pts',(-19.6721123140465,-20.8497972194717,
-21.9474773678718));
#67053=CARTESIAN_POINT('Ctrl Pts',(-19.6067990615792,-20.8820826321498,
-21.9431080978047));
#67054=CARTESIAN_POINT('Ctrl Pts',(-19.5397958312689,-20.911003058507,-21.9387388277375));
#67055=CARTESIAN_POINT('Ctrl Pts',(-19.4714848515874,-20.9363903581904,
-21.9343695576704));
#67056=CARTESIAN_POINT('Ctrl Pts',(-19.4031718505269,-20.9617784091052,
-21.9300001583129));
#67057=CARTESIAN_POINT('Ctrl Pts',(-19.3335514769124,-20.9836329595348,
-21.9256307589554));
#67058=CARTESIAN_POINT('Ctrl Pts',(-19.2630238363122,-21.001834817885,-21.9212613595979));
#67059=CARTESIAN_POINT('Ctrl Pts',(-19.192424400798,-21.0200552051529,-21.9168875123296));
#67060=CARTESIAN_POINT('Ctrl Pts',(-19.1209163233831,-21.0346153567022,
-21.9125136650614));
#67061=CARTESIAN_POINT('Ctrl Pts',(-19.0489118445282,-21.0454468061491,
-21.9081398177931));
#67062=CARTESIAN_POINT('Ctrl Pts',(-18.9768675429743,-21.0562842460226,
-21.9037635515308));
#67063=CARTESIAN_POINT('Ctrl Pts',(-18.904326774497,-21.0633888314031,-21.8993872852686));
#67064=CARTESIAN_POINT('Ctrl Pts',(-18.8317061863209,-21.0667440746234,
-21.8950110190063));
#67065=CARTESIAN_POINT('Ctrl Pts',(-18.7589614597164,-21.0701050533332,
-21.8906272719066));
#67066=CARTESIAN_POINT('Ctrl Pts',(-18.6861371242322,-21.0697038968461,
-21.8862435248068));
#67067=CARTESIAN_POINT('Ctrl Pts',(-18.6136484217024,-21.0655762341589,
-21.8818597777071));
#67068=CARTESIAN_POINT('Ctrl Pts',(-18.5716418570464,-21.063184289987,-21.8793194348736));
#67069=CARTESIAN_POINT('Ctrl Pts',(-18.5297478967642,-21.0595419177169,
-21.8767790920401));
#67070=CARTESIAN_POINT('Ctrl Pts',(-18.4880458377735,-21.0546639175302,
-21.8742387492067));
#67071=CARTESIAN_POINT('Ctrl Pts',(-18.4158851680032,-21.0462230930451,
-21.8698429748793));
#67072=CARTESIAN_POINT('Ctrl Pts',(-18.3440241776343,-21.0340474650401,
-21.8654472005519));
#67073=CARTESIAN_POINT('Ctrl Pts',(-18.2728787135213,-21.0181694410566,
-21.8610514262245));
#67074=CARTESIAN_POINT('Ctrl Pts',(-18.2018360755882,-21.0023143655011,
-21.8566620050875));
#67075=CARTESIAN_POINT('Ctrl Pts',(-18.1315073759669,-20.9827676217893,
-21.8522725839506));
#67076=CARTESIAN_POINT('Ctrl Pts',(-18.0623020985936,-20.9596132419483,
-21.8478831628136));
#67077=CARTESIAN_POINT('Ctrl Pts',(-17.9931748381961,-20.9364849646642,
-21.8434986899895));
#67078=CARTESIAN_POINT('Ctrl Pts',(-17.9251689375377,-20.9097572825852,
-21.8391142171653));
#67079=CARTESIAN_POINT('Ctrl Pts',(-17.8586808325707,-20.8795646176279,
-21.8347297443412));
#67080=CARTESIAN_POINT('Ctrl Pts',(-17.7922330111159,-20.8493902456658,
-21.8303479279616));
#67081=CARTESIAN_POINT('Ctrl Pts',(-17.7273015969599,-20.8157552549639,
-21.8259661115821));
#67082=CARTESIAN_POINT('Ctrl Pts',(-17.6642637491768,-20.7788424545304,
-21.8215842952025));
#67083=CARTESIAN_POINT('Ctrl Pts',(-17.6012435076605,-20.7419399637226,
-21.8172037026501));
#67084=CARTESIAN_POINT('Ctrl Pts',(-17.5401161967491,-20.7017617236165,
-21.8128231100976));
#67085=CARTESIAN_POINT('Ctrl Pts',(-17.4812335587017,-20.6585360364073,
-21.8084425175452));
#67086=CARTESIAN_POINT('Ctrl Pts',(-17.4223481372602,-20.6153083059113,
-21.8040617179213));
#67087=CARTESIAN_POINT('Ctrl Pts',(-17.3657079854645,-20.5690331281733,
-21.7996809182973));
#67088=CARTESIAN_POINT('Ctrl Pts',(-17.3116337298584,-20.5199806100726,
-21.7953001186734));
#67089=CARTESIAN_POINT('Ctrl Pts',(-17.2575023549029,-20.47087627715,-21.790914691553));
#67090=CARTESIAN_POINT('Ctrl Pts',(-17.2059426440142,-20.4189890701121,
-21.7865292644327));
#67091=CARTESIAN_POINT('Ctrl Pts',(-17.1572395226006,-20.3646271259293,
-21.7821438373123));
#67092=CARTESIAN_POINT('Ctrl Pts',(-17.1085091560373,-20.3102347709788,
-21.7777559569279));
#67093=CARTESIAN_POINT('Ctrl Pts',(-17.0626388625667,-20.253365296582,-21.7733680765434));
#67094=CARTESIAN_POINT('Ctrl Pts',(-17.0198725666879,-20.1943591036278,
-21.768980196159));
#67095=CARTESIAN_POINT('Ctrl Pts',(-16.9770305343292,-20.1352484143348,
-21.7645845451083));
#67096=CARTESIAN_POINT('Ctrl Pts',(-16.9373037385248,-20.0739938533524,
-21.7601888940575));
#67097=CARTESIAN_POINT('Ctrl Pts',(-16.9008918467625,-20.010963407552,-21.7557932430068));
#67098=CARTESIAN_POINT('Ctrl Pts',(-16.8767856902822,-19.9692346833373,
-21.7528831428463));
#67099=CARTESIAN_POINT('Ctrl Pts',(-16.8541315013796,-19.9267281135982,
-21.7499730426858));
#67100=CARTESIAN_POINT('Ctrl Pts',(-16.8329755935997,-19.8835552620593,
-21.7470629425253));
#67101=CARTESIAN_POINT('Ctrl Pts',(-16.8011149796973,-19.8185373215268,
-21.7426803568856));
#67102=CARTESIAN_POINT('Ctrl Pts',(-16.7725300723094,-19.7517529070192,
-21.7382977712459));
#67103=CARTESIAN_POINT('Ctrl Pts',(-16.7474199334088,-19.6835658815327,
-21.7339151856062));
#67104=CARTESIAN_POINT('Ctrl Pts',(-16.722347574114,-19.6154814472323,-21.7295391938112));
#67105=CARTESIAN_POINT('Ctrl Pts',(-16.7007397717712,-19.5459990409051,
-21.7251632020162));
#67106=CARTESIAN_POINT('Ctrl Pts',(-16.6827489097976,-19.4755054583704,
-21.7207872102213));
#67107=CARTESIAN_POINT('Ctrl Pts',(-16.6647796017072,-19.4050963304016,
-21.7164164610665));
#67108=CARTESIAN_POINT('Ctrl Pts',(-16.6504187455061,-19.3336788989525,
-21.7120457119117));
#67109=CARTESIAN_POINT('Ctrl Pts',(-16.6397693978102,-19.2616565595166,
-21.7076749627569));
#67110=CARTESIAN_POINT('Ctrl Pts',(-16.6291269464843,-19.1896808607495,
-21.7033070440387));
#67111=CARTESIAN_POINT('Ctrl Pts',(-16.6221913058276,-19.117101508527,-21.6989391253204));
#67112=CARTESIAN_POINT('Ctrl Pts',(-16.6190144751312,-19.0443321698839,
-21.6945712066022));
#67113=CARTESIAN_POINT('Ctrl Pts',(-16.6158386463066,-18.9715857803861,
-21.6902046653873));
#67114=CARTESIAN_POINT('Ctrl Pts',(-16.6164192953802,-18.8986500064394,
-21.6858381241723));
#67115=CARTESIAN_POINT('Ctrl Pts',(-16.6207564302585,-18.8259420175236,
-21.6814715829573));
#67116=CARTESIAN_POINT('Ctrl Pts',(-16.6250936381862,-18.7532328040023,
-21.6771049681976));
#67117=CARTESIAN_POINT('Ctrl Pts',(-16.6331874267156,-18.6807518659564,
-21.6727383534379));
#67118=CARTESIAN_POINT('Ctrl Pts',(-16.64498579739,-18.6089130412075,-21.6683717386782));
#67119=CARTESIAN_POINT('Ctrl Pts',(-16.6567963801275,-18.5369998587107,
-21.6640006041948));
#67120=CARTESIAN_POINT('Ctrl Pts',(-16.672319122297,-18.465730594939,-21.6596294697114));
#67121=CARTESIAN_POINT('Ctrl Pts',(-16.6914506939752,-18.3955098091991,
-21.655258335228));
#67122=CARTESIAN_POINT('Ctrl Pts',(-16.7105926424343,-18.325250936379,-21.6508848298832));
#67123=CARTESIAN_POINT('Ctrl Pts',(-16.7333471660201,-18.2560421336627,
-21.6465113245384));
#67124=CARTESIAN_POINT('Ctrl Pts',(-16.7595615727462,-18.1882710579117,
-21.6421378191936));
#67125=CARTESIAN_POINT('Ctrl Pts',(-16.7858227154186,-18.1203791575545,
-21.6377565166129));
#67126=CARTESIAN_POINT('Ctrl Pts',(-16.8155558613104,-18.0539305447508,
-21.6333752140323));
#67127=CARTESIAN_POINT('Ctrl Pts',(-16.8485611226492,-17.9892906774244,
-21.6289939114516));
#67128=CARTESIAN_POINT('Ctrl Pts',(-16.8714288660015,-17.9445048512745,
-21.6259583195824));
#67129=CARTESIAN_POINT('Ctrl Pts',(-16.8958663903147,-17.9005867928719,
-21.6229227277131));
#67130=CARTESIAN_POINT('Ctrl Pts',(-16.9217951734766,-17.8576496599694,
-21.6198871358438));
#67131=CARTESIAN_POINT('Ctrl Pts',(-16.9592871125939,-17.7955643564438,
-21.6154977965973));
#67132=CARTESIAN_POINT('Ctrl Pts',(-17.0000461986468,-17.7352871847913,
-21.6111084573508));
#67133=CARTESIAN_POINT('Ctrl Pts',(-17.0438726443021,-17.6771829458619,
-21.6067191181042));
#67134=CARTESIAN_POINT('Ctrl Pts',(-17.0876341035589,-17.6191648646202,
-21.6023362874245));
#67135=CARTESIAN_POINT('Ctrl Pts',(-17.134453605312,-17.5633137014982,-21.5979534567447));
#67136=CARTESIAN_POINT('Ctrl Pts',(-17.1840868960386,-17.5099672783988,
-21.593570626065));
#67137=CARTESIAN_POINT('Ctrl Pts',(-17.2336618872153,-17.4566835163159,
-21.5891929434835));
#67138=CARTESIAN_POINT('Ctrl Pts',(-17.2860437748972,-17.4058990008948,
-21.5848152609019));
#67139=CARTESIAN_POINT('Ctrl Pts',(-17.3409477315906,-17.3579189551721,
-21.5804375783204));
#67140=CARTESIAN_POINT('Ctrl Pts',(-17.3958168761313,-17.3099693314588,
-21.5760626714324));
#67141=CARTESIAN_POINT('Ctrl Pts',(-17.4532045546155,-17.2648209656694,
-21.5716877645444));
#67142=CARTESIAN_POINT('Ctrl Pts',(-17.5127897524411,-17.2227416239159,
-21.5673128576563));
#67143=CARTESIAN_POINT('Ctrl Pts',(-17.5723567979443,-17.1806751014162,
-21.5629392835611));
#67144=CARTESIAN_POINT('Ctrl Pts',(-17.6341196401156,-17.14167602466,-21.5585657094658));
#67145=CARTESIAN_POINT('Ctrl Pts',(-17.6977262557446,-17.1059702800424,
-21.5541921353705));
#67146=CARTESIAN_POINT('Ctrl Pts',(-17.761334446059,-17.0702636514709,-21.5498184530003));
#67147=CARTESIAN_POINT('Ctrl Pts',(-17.8267860790938,-17.0378507511553,
-21.5454447706301));
#67148=CARTESIAN_POINT('Ctrl Pts',(-17.8937038483149,-17.0089118966287,
-21.5410710882598));
#67149=CARTESIAN_POINT('Ctrl Pts',(-17.9606908447099,-16.9799431045363,
-21.5366928812667));
#67150=CARTESIAN_POINT('Ctrl Pts',(-18.0291465621343,-16.9544557255711,
-21.5323146742736));
#67151=CARTESIAN_POINT('Ctrl Pts',(-18.0986737635119,-16.9325818726103,
-21.5279364672805));
#67152=CARTESIAN_POINT('Ctrl Pts',(-18.168238835056,-16.9106961053709,-21.5235558755599));
#67153=CARTESIAN_POINT('Ctrl Pts',(-18.2388760855,-16.8924279037581,-21.5191752838393));
#67154=CARTESIAN_POINT('Ctrl Pts',(-18.3101757995837,-16.8778587205445,
-21.5147946921187));
#67155=CARTESIAN_POINT('Ctrl Pts',(-18.38160150593,-16.8632637924259,-21.5104063595443));
#67156=CARTESIAN_POINT('Ctrl Pts',(-18.453691536507,-16.8523810078683,-21.5060180269699));
#67157=CARTESIAN_POINT('Ctrl Pts',(-18.5260293173379,-16.8452401192464,
-21.5016296943955));
#67158=CARTESIAN_POINT('Ctrl Pts',(-18.5750331047421,-16.8404026666194,
-21.4986569059845));
#67159=CARTESIAN_POINT('Ctrl Pts',(-18.6241504958208,-16.8372813242577,
-21.4956841175734));
#67160=CARTESIAN_POINT('Ctrl Pts',(-18.6732524736177,-16.8358717576578,
-21.4927113291624));
#67161=CARTESIAN_POINT('Ctrl Pts',(-18.7457477453063,-16.833790641617,-21.4883222370484));
#67162=CARTESIAN_POINT('Ctrl Pts',(-18.8184909189991,-16.8354351540471,
-21.4839331449344));
#67163=CARTESIAN_POINT('Ctrl Pts',(-18.8910671368434,-16.8408347022263,
-21.4795440528204));
#67164=CARTESIAN_POINT('Ctrl Pts',(-18.9635359887558,-16.8462262625614,
-21.4751614537282));
#67165=CARTESIAN_POINT('Ctrl Pts',(-19.0358378982521,-16.8553617955042,
-21.470778854636));
#67166=CARTESIAN_POINT('Ctrl Pts',(-19.1075566334651,-16.8682187155092,
-21.4663962555438));
#67167=CARTESIAN_POINT('Ctrl Pts',(-19.1791915242117,-16.8810606048308,
-21.4620187800316));
#67168=CARTESIAN_POINT('Ctrl Pts',(-19.2502441227826,-16.8976151540491,
-21.4576413045195));
#67169=CARTESIAN_POINT('Ctrl Pts',(-19.3203036537857,-16.9178080165438,
-21.4532638290073));
#67170=CARTESIAN_POINT('Ctrl Pts',(-19.3903190046979,-16.9379881452606,
-21.4488891139657));
#67171=CARTESIAN_POINT('Ctrl Pts',(-19.4593420684319,-16.9618019016887,
-21.444514398924));
#67172=CARTESIAN_POINT('Ctrl Pts',(-19.5269739887336,-16.989124238982,-21.4401396838823));
#67173=CARTESIAN_POINT('Ctrl Pts',(-19.5945855447919,-17.0164383494096,
-21.435766286085));
#67174=CARTESIAN_POINT('Ctrl Pts',(-19.6608063422521,-17.0472587627945,
-21.4313928882876));
#67175=CARTESIAN_POINT('Ctrl Pts',(-19.7252559661585,-17.0814116942643,
-21.4270194904902));
#67176=CARTESIAN_POINT('Ctrl Pts',(-19.7897074198449,-17.115565595365,-21.4226459685284));
#67177=CARTESIAN_POINT('Ctrl Pts',(-19.852387175046,-17.1530519748722,-21.4182724465665));
#67178=CARTESIAN_POINT('Ctrl Pts',(-19.9129394590442,-17.1936511290678,
-21.4138989246046));
#67179=CARTESIAN_POINT('Ctrl Pts',(-19.9735547443612,-17.2342925244489,
-21.4095208522338));
#67180=CARTESIAN_POINT('Ctrl Pts',(-20.0320377377389,-17.2780528916324,
-21.4051427798631));
#67181=CARTESIAN_POINT('Ctrl Pts',(-20.0880624200393,-17.3246696823824,
-21.4007647074923));
#67182=CARTESIAN_POINT('Ctrl Pts',(-20.1441178009626,-17.3713120167183,
-21.3963842361647));
#67183=CARTESIAN_POINT('Ctrl Pts',(-20.1977118344489,-17.420813563513,-21.3920037648371));
#67184=CARTESIAN_POINT('Ctrl Pts',(-20.2485543554084,-17.4728738713303,
-21.3876232935095));
#67185=CARTESIAN_POINT('Ctrl Pts',(-20.2994870055889,-17.5250264671557,
-21.3832350568615));
#67186=CARTESIAN_POINT('Ctrl Pts',(-20.3476580839202,-17.5797465198983,
-21.3788468202134));
#67187=CARTESIAN_POINT('Ctrl Pts',(-20.3928171932228,-17.6366998367413,
-21.3744585835654));
#67188=CARTESIAN_POINT('Ctrl Pts',(-20.4234261084619,-17.6753028843823,
-21.3714842298706));
#67189=CARTESIAN_POINT('Ctrl Pts',(-20.4526521461855,-17.7149312605343,
-21.3685098761757));
#67190=CARTESIAN_POINT('Ctrl Pts',(-20.4804290453301,-17.7554739494572,
-21.3655355224809));
#67191=CARTESIAN_POINT('Ctrl Pts',(-20.5219871745244,-17.8161314870525,
-21.361085473018));
#67192=CARTESIAN_POINT('Ctrl Pts',(-20.5604589913813,-17.8790695530753,
-21.3566354235551));
#67193=CARTESIAN_POINT('Ctrl Pts',(-20.5955899131733,-17.9439464323899,
-21.3521853740922));
#67194=CARTESIAN_POINT('Ctrl Pts',(-20.6306645420735,-18.00871935465,-21.347742455275));
#67195=CARTESIAN_POINT('Ctrl Pts',(-20.6624086883073,-18.0754245154655,
-21.3432995364577));
#67196=CARTESIAN_POINT('Ctrl Pts',(-20.6906106838733,-18.1436908810653,
-21.3388566176404));
#67197=CARTESIAN_POINT('Ctrl Pts',(-20.7187693738979,-18.2118524203273,
-21.3344205211419));
#67198=CARTESIAN_POINT('Ctrl Pts',(-20.7433965530088,-18.2815699703269,
-21.3299844246434));
#67199=CARTESIAN_POINT('Ctrl Pts',(-20.764326992868,-18.3524490830367,-21.3255483281449));
#67200=CARTESIAN_POINT('Ctrl Pts',(-20.7852384436445,-18.423263890871,-21.3211162562824));
#67201=CARTESIAN_POINT('Ctrl Pts',(-20.8024596851649,-18.4952377246083,
-21.31668418442));
#67202=CARTESIAN_POINT('Ctrl Pts',(-20.8158744003031,-18.5679583598586,
-21.3122521125575));
#67203=CARTESIAN_POINT('Ctrl Pts',(-20.829281573186,-18.6406381088439,-21.3078225325719));
#67204=CARTESIAN_POINT('Ctrl Pts',(-20.8388863850559,-18.7140633695048,
-21.3033929525863));
#67205=CARTESIAN_POINT('Ctrl Pts',(-20.8446233129547,-18.787810381534,-21.2989633726007));
#67206=CARTESIAN_POINT('Ctrl Pts',(-20.8489003385967,-18.8427906544308,
-21.2956610080746));
#67207=CARTESIAN_POINT('Ctrl Pts',(-20.8510286073718,-18.8979494671394,
-21.2923586435486));
#67208=CARTESIAN_POINT('Ctrl Pts',(-20.8509997094769,-18.9531090873175,
-21.2890562790225));
#67209=CARTESIAN_POINT('Ctrl Pts',(-20.8509997572016,-18.9530139075719,
-21.2873808207992));
#67210=CARTESIAN_POINT('Ctrl Pts',(-20.8509644636734,-19.0267054279197,
-21.2831945047056));
#67211=CARTESIAN_POINT('Ctrl Pts',(-20.8470814811288,-19.1003499721809,
-21.2791138391139));
#67212=CARTESIAN_POINT('Ctrl Pts',(-20.8222221592446,-19.3364815089262,
-21.2661204831227));
#67213=CARTESIAN_POINT('Ctrl Pts',(-20.7862490061281,-19.496756327703,-21.2574710226349));
#67214=CARTESIAN_POINT('Ctrl Pts',(-20.7290394438667,-19.6602350880456,
-21.2475108436966));
#67215=CARTESIAN_POINT('Ctrl Pts',(-20.7258400125798,-19.6691838473955,
-21.2469617469771));
#67216=CARTESIAN_POINT('Ctrl Pts',(-20.7225805821494,-19.6781103692267,
-21.2464098430158));
#67217=CARTESIAN_POINT('Origin',(-18.734,-18.952,0.));
#67218=CARTESIAN_POINT('',(-20.722580711674,-19.6781100145006,-20.4442392611068));
#67219=CARTESIAN_POINT('',(-20.7225805821175,-19.6781103693139,-20.6683680078465));
#67220=CARTESIAN_POINT('',(-20.7225805821191,-19.6781103693095,0.));
#67221=CARTESIAN_POINT('Ctrl Pts',(-20.7225805821175,-19.6781103693139,
-20.6683680078465));
#67222=CARTESIAN_POINT('Ctrl Pts',(-20.723865209165,-19.6745921928633,-20.6685904485746));
#67223=CARTESIAN_POINT('Ctrl Pts',(-20.7251405065262,-19.6710705886775,
-20.6688125801961));
#67224=CARTESIAN_POINT('Ctrl Pts',(-20.7310458544951,-19.6546273968654,
-20.6698473346312));
#67225=CARTESIAN_POINT('Ctrl Pts',(-20.7355595809394,-19.6416641653527,
-20.6706561060802));
#67226=CARTESIAN_POINT('Ctrl Pts',(-20.768858785208,-19.5429489113029,-20.6767638662585));
#67227=CARTESIAN_POINT('Ctrl Pts',(-20.7922497624033,-19.4554696483961,
-20.6818795550824));
#67228=CARTESIAN_POINT('Ctrl Pts',(-20.8373639001823,-19.2296587432863,
-20.6946257986702));
#67229=CARTESIAN_POINT('Ctrl Pts',(-20.8511051846752,-19.0901947745664,
-20.7020608620861));
#67230=CARTESIAN_POINT('Ctrl Pts',(-20.8509840406084,-18.9301095183909,
-20.7109057851118));
#67231=CARTESIAN_POINT('Ctrl Pts',(-20.8506770340003,-18.9098227212298,
-20.7120328634699));
#67232=CARTESIAN_POINT('Ctrl Pts',(-20.8483264214982,-18.8301815006497,
-20.7164921316393));
#67233=CARTESIAN_POINT('Ctrl Pts',(-20.8440773295534,-18.7709246959545,
-20.7198853747503));
#67234=CARTESIAN_POINT('Ctrl Pts',(-20.8363297185987,-18.703044686032,-20.723937924618));
#67235=CARTESIAN_POINT('Ctrl Pts',(-20.8352591867053,-18.6941651343004,
-20.7244713321321));
#67236=CARTESIAN_POINT('Ctrl Pts',(-20.8335616364937,-18.6807981145446,
-20.7252796168894));
#67237=CARTESIAN_POINT('Ctrl Pts',(-20.8329764089932,-18.6763053106714,
-20.7255521954006));
#67238=CARTESIAN_POINT('Ctrl Pts',(-20.8319046584194,-18.6682787131095,
-20.726040842706));
#67239=CARTESIAN_POINT('Ctrl Pts',(-20.8314236225146,-18.6647442395577,
-20.7262565992299));
#67240=CARTESIAN_POINT('Ctrl Pts',(-20.8303644475976,-18.6571063331617,
-20.7267241180625));
#67241=CARTESIAN_POINT('Ctrl Pts',(-20.8297832008255,-18.6530034342164,
-20.7269760486134));
#67242=CARTESIAN_POINT('Ctrl Pts',(-20.8281309523601,-18.6415821188147,
-20.7276795047986));
#67243=CARTESIAN_POINT('Ctrl Pts',(-20.8270336495137,-18.6342676521319,
-20.7281324773477));
#67244=CARTESIAN_POINT('Ctrl Pts',(-20.820538960699,-18.5924691228918,-20.7307345037716));
#67245=CARTESIAN_POINT('Ctrl Pts',(-20.8143280497843,-18.5581190996876,
-20.732925459951));
#67246=CARTESIAN_POINT('Ctrl Pts',(-20.7918958200027,-18.449470363468,-20.7399904291395));
#67247=CARTESIAN_POINT('Ctrl Pts',(-20.7725200329496,-18.3758873924989,
-20.7449760667154));
#67248=CARTESIAN_POINT('Ctrl Pts',(-20.6904215811938,-18.1207597792959,
-20.7626582812333));
#67249=CARTESIAN_POINT('Ctrl Pts',(-20.607011625039,-17.9468115910366,-20.7753362062963));
#67250=CARTESIAN_POINT('Ctrl Pts',(-20.4894885235568,-17.7686120090818,
-20.7884544750299));
#67251=CARTESIAN_POINT('Ctrl Pts',(-20.4774343679079,-17.750923919569,-20.7897596960255));
#67252=CARTESIAN_POINT('Ctrl Pts',(-20.4603097930515,-17.7265967405172,
-20.791559750663));
#67253=CARTESIAN_POINT('Ctrl Pts',(-20.455465536487,-17.7198007223895,-20.7920631596211));
#67254=CARTESIAN_POINT('Ctrl Pts',(-20.4470413638233,-17.7081290786888,
-20.7929287332018));
#67255=CARTESIAN_POINT('Ctrl Pts',(-20.4434805340322,-17.7032398597014,
-20.7932916276391));
#67256=CARTESIAN_POINT('Ctrl Pts',(-20.4360698635491,-17.6931556940307,
-20.7940407786998));
#67257=CARTESIAN_POINT('Ctrl Pts',(-20.4322170744055,-17.6879629844414,
-20.7944269154879));
#67258=CARTESIAN_POINT('Ctrl Pts',(-20.4231495398308,-17.675858236915,-20.7953279585973));
#67259=CARTESIAN_POINT('Ctrl Pts',(-20.4179160356735,-17.6689603452745,
-20.7958421240079));
#67260=CARTESIAN_POINT('Ctrl Pts',(-20.4008332352383,-17.6467293514784,
-20.7975016805812));
#67261=CARTESIAN_POINT('Ctrl Pts',(-20.3888154824816,-17.6315265031748,
-20.7986404092484));
#67262=CARTESIAN_POINT('Ctrl Pts',(-20.3265596628857,-17.5549558727395,
-20.8043990523528));
#67263=CARTESIAN_POINT('Ctrl Pts',(-20.2731076957359,-17.4962774859446,
-20.8088863626349));
#67264=CARTESIAN_POINT('Ctrl Pts',(-20.1000686770742,-17.3265342060466,
-20.8223349060607));
#67265=CARTESIAN_POINT('Ctrl Pts',(-19.9708583089203,-17.2261788962322,
-20.8309359319349));
#67266=CARTESIAN_POINT('Ctrl Pts',(-19.7791771957653,-17.1099832231012,
-20.8434651877469));
#67267=CARTESIAN_POINT('Ctrl Pts',(-19.7255935311021,-17.0805935827379,
-20.8469516357444));
#67268=CARTESIAN_POINT('Ctrl Pts',(-19.6626469889472,-17.0495313841536,
-20.8511147944165));
#67269=CARTESIAN_POINT('Ctrl Pts',(-19.654448179116,-17.0455511527494,-20.8516583326422));
#67270=CARTESIAN_POINT('Ctrl Pts',(-19.642158524247,-17.0396827165673,-20.8524753631453));
#67271=CARTESIAN_POINT('Ctrl Pts',(-19.6380868132261,-17.0377543702632,
-20.8527464286688));
#67272=CARTESIAN_POINT('Ctrl Pts',(-19.6307806650308,-17.0343227173495,
-20.8532335425438));
#67273=CARTESIAN_POINT('Ctrl Pts',(-19.6275485583818,-17.032814575116,-20.853449287818));
#67274=CARTESIAN_POINT('Ctrl Pts',(-19.6205324220565,-17.0295623222176,
-20.8539181837594));
#67275=CARTESIAN_POINT('Ctrl Pts',(-19.6167470999229,-17.0278212356431,
-20.8541715103589));
#67276=CARTESIAN_POINT('Ctrl Pts',(-19.6061407962318,-17.0229806728741,
-20.8548822451461));
#67277=CARTESIAN_POINT('Ctrl Pts',(-19.5993085431071,-17.0199062511749,
-20.8553411458966));
#67278=CARTESIAN_POINT('Ctrl Pts',(-19.5591795513974,-17.0021042886336,
-20.8580420997529));
#67279=CARTESIAN_POINT('Ctrl Pts',(-19.5255257813601,-16.9882023662435,
-20.8603297434085));
#67280=CARTESIAN_POINT('Ctrl Pts',(-19.4153870013204,-16.9459964143811,
-20.867850708044));
#67281=CARTESIAN_POINT('Ctrl Pts',(-19.3376237011844,-16.9212426779879,
-20.8732108566154));
#67282=CARTESIAN_POINT('Ctrl Pts',(-19.0810906874427,-16.8556220082492,
-20.8906948988151));
#67283=CARTESIAN_POINT('Ctrl Pts',(-18.8983629531948,-16.8334429315667,
-20.9027594792982));
#67284=CARTESIAN_POINT('Ctrl Pts',(-18.6927250276458,-16.8352847743648,
-20.9154088693627));
#67285=CARTESIAN_POINT('Ctrl Pts',(-18.6704146050536,-16.8358374525744,
-20.9167705395927));
#67286=CARTESIAN_POINT('Ctrl Pts',(-18.6396301837634,-16.8370873605794,
-20.9186352418421));
#67287=CARTESIAN_POINT('Ctrl Pts',(-18.6311460223452,-16.8374829872602,
-20.9191476686827));
#67288=CARTESIAN_POINT('Ctrl Pts',(-18.6165842214634,-16.8382498715001,
-20.920024686603));
#67289=CARTESIAN_POINT('Ctrl Pts',(-18.6105054302373,-16.8385963085047,
-20.920390051414));
#67290=CARTESIAN_POINT('Ctrl Pts',(-18.5979928579742,-16.8393635839881,
-20.9211406155645));
#67291=CARTESIAN_POINT('Ctrl Pts',(-18.591559329758,-16.8397875992643,-20.9215257112028));
#67292=CARTESIAN_POINT('Ctrl Pts',(-18.5766198067645,-16.8408407875793,
-20.9224180998122));
#67293=CARTESIAN_POINT('Ctrl Pts',(-18.5681154392479,-16.8414919897895,
-20.9229246961162));
#67294=CARTESIAN_POINT('Ctrl Pts',(-18.5410187258285,-16.8437316543733,
-20.9245345206078));
#67295=CARTESIAN_POINT('Ctrl Pts',(-18.5224430221923,-16.8455145698367,
-20.9256316433706));
#67296=CARTESIAN_POINT('Ctrl Pts',(-18.3441739464121,-16.8650070012947,
-20.936104450901));
#67297=CARTESIAN_POINT('Ctrl Pts',(-18.1869591311987,-16.9005959487609,
-20.9448516755273));
#67298=CARTESIAN_POINT('Ctrl Pts',(-17.9084942866733,-16.9979616726981,
-20.9608714191344));
#67299=CARTESIAN_POINT('Ctrl Pts',(-17.7862430511598,-17.0542454535539,
-20.9681340845894));
#67300=CARTESIAN_POINT('Ctrl Pts',(-17.6566079943566,-17.1295946355659,
-20.9769255817016));
#67301=CARTESIAN_POINT('Ctrl Pts',(-17.6431404604304,-17.1376239974544,
-20.9778531014542));
#67302=CARTESIAN_POINT('Ctrl Pts',(-17.6248246786053,-17.1488215231846,
-20.9791358277245));
#67303=CARTESIAN_POINT('Ctrl Pts',(-17.6198980247693,-17.1518613109438,
-20.9794829963443));
#67304=CARTESIAN_POINT('Ctrl Pts',(-17.6120883509842,-17.156724286518,-20.9800368289494));
#67305=CARTESIAN_POINT('Ctrl Pts',(-17.6091971209646,-17.1585343274685,
-20.9802426318032));
#67306=CARTESIAN_POINT('Ctrl Pts',(-17.6032372336692,-17.1622855671119,
-20.9806684816565));
#67307=CARTESIAN_POINT('Ctrl Pts',(-17.600169203859,-17.1642276683136,-20.9808885916277));
#67308=CARTESIAN_POINT('Ctrl Pts',(-17.5928705750823,-17.1688741358451,
-20.981414321515));
#67309=CARTESIAN_POINT('Ctrl Pts',(-17.5886445864649,-17.1715856697601,
-20.9817204144978));
#67310=CARTESIAN_POINT('Ctrl Pts',(-17.5744205112017,-17.1807839067649,
-20.9827562835207));
#67311=CARTESIAN_POINT('Ctrl Pts',(-17.564467779022,-17.1873398602394,-20.9834904712269));
#67312=CARTESIAN_POINT('Ctrl Pts',(-17.5406895091441,-17.203292332644,-20.9852661703009));
#67313=CARTESIAN_POINT('Ctrl Pts',(-17.5269190639248,-17.2127691325323,
-20.9863123277161));
#67314=CARTESIAN_POINT('Ctrl Pts',(-17.4756950857485,-17.2489227495913,
-20.9902669456693));
#67315=CARTESIAN_POINT('Ctrl Pts',(-17.4390035992435,-17.2766531241249,
-20.9932277158313));
#67316=CARTESIAN_POINT('Ctrl Pts',(-17.3454265824065,-17.3522875177858,
-21.0010643322817));
#67317=CARTESIAN_POINT('Ctrl Pts',(-17.2901100640836,-17.4020330766274,
-21.0059879963955));
#67318=CARTESIAN_POINT('Ctrl Pts',(-17.1277255407977,-17.5643153714376,
-21.0211549223784));
#67319=CARTESIAN_POINT('Ctrl Pts',(-17.030308298842,-17.6858098785556,-21.0312706877406));
#67320=CARTESIAN_POINT('Ctrl Pts',(-16.9342096445632,-17.8370933919803,
-21.0423125955737));
#67321=CARTESIAN_POINT('Ctrl Pts',(-16.9217171620446,-17.8575169908679,
-21.0437748597252));
#67322=CARTESIAN_POINT('Ctrl Pts',(-16.9046537626209,-17.8865069658841,
-21.0458116978412));
#67323=CARTESIAN_POINT('Ctrl Pts',(-16.8997915892861,-17.8948989769513,
-21.0463968450537));
#67324=CARTESIAN_POINT('Ctrl Pts',(-16.8920196577054,-17.9085282434224,
-21.0473400426544));
#67325=CARTESIAN_POINT('Ctrl Pts',(-16.8890742006779,-17.9137448847618,
-21.047699380446));
#67326=CARTESIAN_POINT('Ctrl Pts',(-16.8829819480667,-17.9246425422203,
-21.0484465936299));
#67327=CARTESIAN_POINT('Ctrl Pts',(-16.8798390665344,-17.930325683547,-21.0488343254957));
#67328=CARTESIAN_POINT('Ctrl Pts',(-16.8724722135699,-17.943792813822,-21.0497485918363));
#67329=CARTESIAN_POINT('Ctrl Pts',(-16.8682708156304,-17.9515890623656,
-21.0502743159918));
#67330=CARTESIAN_POINT('Ctrl Pts',(-16.8544957143635,-17.9775392009793,
-21.0520126536078));
#67331=CARTESIAN_POINT('Ctrl Pts',(-16.8451368942052,-17.9958062853925,
-21.0532176622835));
#67332=CARTESIAN_POINT('Ctrl Pts',(-16.7969204161315,-18.0933893498731,
-21.0595611632357));
#67333=CARTESIAN_POINT('Ctrl Pts',(-16.7627868894722,-18.1749472340003,
-21.0645331899724));
#67334=CARTESIAN_POINT('Ctrl Pts',(-16.6909636103039,-18.3820681892771,
-21.0766335480794));
#67335=CARTESIAN_POINT('Ctrl Pts',(-16.6596436015191,-18.5094347336584,
-21.0836107002132));
#67336=CARTESIAN_POINT('Ctrl Pts',(-16.634706335176,-18.6761780249987,-21.0929106682711));
#67337=CARTESIAN_POINT('Ctrl Pts',(-16.6301256108669,-18.7136221971592,
-21.0950110809277));
#67338=CARTESIAN_POINT('Ctrl Pts',(-16.6221958036023,-18.7968341192315,
-21.0997427780473));
#67339=CARTESIAN_POINT('Ctrl Pts',(-16.6193297501016,-18.8426269120661,
-21.1023893118999));
#67340=CARTESIAN_POINT('Ctrl Pts',(-16.6177244973075,-18.8960967451019,
-21.1055661122373));
#67341=CARTESIAN_POINT('Ctrl Pts',(-16.617536821783,-18.9037217596845,-21.1060211891972));
#67342=CARTESIAN_POINT('Ctrl Pts',(-16.6173018883948,-18.9159537791142,
-21.1067547501936));
#67343=CARTESIAN_POINT('Ctrl Pts',(-16.6172284559638,-18.9205602933888,
-21.1070318079103));
#67344=CARTESIAN_POINT('Ctrl Pts',(-16.6171246682075,-18.9287479991062,
-21.1075257395748));
#67345=CARTESIAN_POINT('Ctrl Pts',(-16.6170883627061,-18.9323290672215,
-21.1077422775414));
#67346=CARTESIAN_POINT('Ctrl Pts',(-16.6170304189219,-18.9399527748725,
-21.1082043602753));
#67347=CARTESIAN_POINT('Ctrl Pts',(-16.6170112736669,-18.9439953270453,
-21.1084500359427));
#67348=CARTESIAN_POINT('Ctrl Pts',(-16.6169907237168,-18.9549753220759,
-21.1091190402344));
#67349=CARTESIAN_POINT('Ctrl Pts',(-16.6170118413194,-18.9619126857155,
-21.109543598171));
#67350=CARTESIAN_POINT('Ctrl Pts',(-16.6172932041723,-18.9972620389329,
-21.1117160260678));
#67351=CARTESIAN_POINT('Ctrl Pts',(-16.6180913198089,-19.0256653586692,
-21.1134914872741));
#67352=CARTESIAN_POINT('Ctrl Pts',(-16.6221156261413,-19.109057745881,-21.1187756317686));
#67353=CARTESIAN_POINT('Ctrl Pts',(-16.6269164156029,-19.1639449947982,
-21.1223445100066));
#67354=CARTESIAN_POINT('Ctrl Pts',(-16.6514713538496,-19.357392784989,-21.135115341163));
#67355=CARTESIAN_POINT('Ctrl Pts',(-16.6828132132105,-19.4941315393559,
-21.1444672079832));
#67356=CARTESIAN_POINT('Ctrl Pts',(-16.7562372029758,-19.7124716697801,
-21.1593415142229));
#67357=CARTESIAN_POINT('Ctrl Pts',(-16.7905170766199,-19.7962397232974,
-21.1650403125865));
#67358=CARTESIAN_POINT('Ctrl Pts',(-16.8360578917058,-19.8899196901911,
-21.1713959949041));
#67359=CARTESIAN_POINT('Ctrl Pts',(-16.8421821526842,-19.9022119964556,
-21.1722297439337));
#67360=CARTESIAN_POINT('Ctrl Pts',(-16.8521965011511,-19.9218316279638,
-21.1735603356539));
#67361=CARTESIAN_POINT('Ctrl Pts',(-16.8560107186651,-19.9291970410959,
-21.1740598207493));
#67362=CARTESIAN_POINT('Ctrl Pts',(-16.8628604740812,-19.9422359684906,
-21.1749440587411));
#67363=CARTESIAN_POINT('Ctrl Pts',(-16.8658787581825,-19.9479183832198,
-21.175329414469));
#67364=CARTESIAN_POINT('Ctrl Pts',(-16.8722219962547,-19.9597302656751,
-21.176130484694));
#67365=CARTESIAN_POINT('Ctrl Pts',(-16.8755514267536,-19.96585725128,-21.17654603432));
#67366=CARTESIAN_POINT('Ctrl Pts',(-16.8842776700188,-19.9817282994689,
-21.1776225832501));
#67367=CARTESIAN_POINT('Ctrl Pts',(-16.8897212647759,-19.9914464982501,
-21.1782819047145));
#67368=CARTESIAN_POINT('Ctrl Pts',(-16.913706544352,-20.0334846631622,-21.1811350176553));
#67369=CARTESIAN_POINT('Ctrl Pts',(-16.9330236523287,-20.0653560913092,
-21.1833007414704));
#67370=CARTESIAN_POINT('Ctrl Pts',(-16.9865970614789,-20.1487008703966,
-21.1889869142468));
#67371=CARTESIAN_POINT('Ctrl Pts',(-17.0222841596487,-20.199212789821,-21.1924562191714));
#67372=CARTESIAN_POINT('Ctrl Pts',(-17.1467978282404,-20.3600185623447,
-21.2037083688439));
#67373=CARTESIAN_POINT('Ctrl Pts',(-17.244465309878,-20.4629636279903,-21.211232481966));
#67374=CARTESIAN_POINT('Ctrl Pts',(-17.4090638204192,-20.6048687831921,
-21.2232630176597));
#67375=CARTESIAN_POINT('Ctrl Pts',(-17.4690650998353,-20.6512257663225,
-21.2275443446769));
#67376=CARTESIAN_POINT('Ctrl Pts',(-17.5392393551531,-20.6996631281265,
-21.2325977268907));
#67377=CARTESIAN_POINT('Ctrl Pts',(-17.5471006958358,-20.7050115350583,
-21.2331644703743));
#67378=CARTESIAN_POINT('Ctrl Pts',(-17.5588073131143,-20.7128612063167,
-21.2340097870987));
#67379=CARTESIAN_POINT('Ctrl Pts',(-17.5626252450527,-20.7154033066165,
-21.2342856862601));
#67380=CARTESIAN_POINT('Ctrl Pts',(-17.5694383459189,-20.7199077962093,
-21.2347784625273));
#67381=CARTESIAN_POINT('Ctrl Pts',(-17.5724302594645,-20.7218750124284,
-21.2349950118591));
#67382=CARTESIAN_POINT('Ctrl Pts',(-17.5788828540481,-20.7260942552716,
-21.2354623749235));
#67383=CARTESIAN_POINT('Ctrl Pts',(-17.5823450925328,-20.7283437226215,
-21.2357133476784));
#67384=CARTESIAN_POINT('Ctrl Pts',(-17.5919287779979,-20.7345305886333,
-21.2364085628659));
#67385=CARTESIAN_POINT('Ctrl Pts',(-17.5980639170006,-20.7384465251871,
-21.2368541848435));
#67386=CARTESIAN_POINT('Ctrl Pts',(-17.6319421156355,-20.7598252261794,
-21.2393174960063));
#67387=CARTESIAN_POINT('Ctrl Pts',(-17.6600661054577,-20.7766723941025,
-21.2413718829415));
#67388=CARTESIAN_POINT('Ctrl Pts',(-17.8308836100605,-20.8736804273696,
-21.2538542178134));
#67389=CARTESIAN_POINT('Ctrl Pts',(-17.9820874314102,-20.9377247233029,
-21.2648714402771));
#67390=CARTESIAN_POINT('Ctrl Pts',(-18.2489541487524,-21.0158575328392,
-21.2830116145616));
#67391=CARTESIAN_POINT('Ctrl Pts',(-18.3611878695894,-21.0390543424456,
-21.2902911434788));
#67392=CARTESIAN_POINT('Ctrl Pts',(-18.4889224800171,-21.0548146728704,
-21.2981492569332));
#67393=CARTESIAN_POINT('Ctrl Pts',(-18.5030993886727,-21.0564185568766,
-21.2990158239945));
#67394=CARTESIAN_POINT('Ctrl Pts',(-18.525705743568,-21.0587448940237,-21.3003889799335));
#67395=CARTESIAN_POINT('Ctrl Pts',(-18.5341249893068,-21.0595603263237,
-21.3008984733819));
#67396=CARTESIAN_POINT('Ctrl Pts',(-18.5489925275914,-21.0609104050816,
-21.3017948850917));
#67397=CARTESIAN_POINT('Ctrl Pts',(-18.5554387657245,-21.0614659865855,
-21.3021824555291));
#67398=CARTESIAN_POINT('Ctrl Pts',(-18.5687870401352,-21.0625548081514,
-21.3029827754518));
#67399=CARTESIAN_POINT('Ctrl Pts',(-18.5756893555835,-21.0630837647827,
-21.3033953861626));
#67400=CARTESIAN_POINT('Ctrl Pts',(-18.5934347757626,-21.0643561583935,
-21.3044530871225));
#67401=CARTESIAN_POINT('Ctrl Pts',(-18.6042813204718,-21.0650499740904,
-21.305096617988));
#67402=CARTESIAN_POINT('Ctrl Pts',(-18.6497597959553,-21.0676075730786,
-21.3077829067901));
#67403=CARTESIAN_POINT('Ctrl Pts',(-18.6844306700201,-21.0687037816909,
-21.3098016289608));
#67404=CARTESIAN_POINT('Ctrl Pts',(-18.7749976417425,-21.0693406171065,
-21.3150108688458));
#67405=CARTESIAN_POINT('Ctrl Pts',(-18.8308771138604,-21.0675206425202,
-21.3181607867753));
#67406=CARTESIAN_POINT('Ctrl Pts',(-19.0845521969156,-21.0491845589789,
-21.332294817397));
#67407=CARTESIAN_POINT('Ctrl Pts',(-19.2794561066504,-21.0071224258054,
-21.3426052650713));
#67408=CARTESIAN_POINT('Ctrl Pts',(-19.4955714179402,-20.9275293304824,
-21.3558293489102));
#67409=CARTESIAN_POINT('Ctrl Pts',(-19.525258987734,-20.9158269089208,-21.3576899172998));
#67410=CARTESIAN_POINT('Ctrl Pts',(-19.5609542872504,-20.9008155632122,
-21.3599938570517));
#67411=CARTESIAN_POINT('Ctrl Pts',(-19.5672267492959,-20.8981419973941,
-21.3604012509739));
#67412=CARTESIAN_POINT('Ctrl Pts',(-19.5775380098296,-20.8936879531629,
-21.3610753296728));
#67413=CARTESIAN_POINT('Ctrl Pts',(-19.5815844043926,-20.8919250393001,
-21.3613409679403));
#67414=CARTESIAN_POINT('Ctrl Pts',(-19.5888753552902,-20.8887213867386,
-21.3618216678));
#67415=CARTESIAN_POINT('Ctrl Pts',(-19.5921218304316,-20.887285128067,-21.3620364532172));
#67416=CARTESIAN_POINT('Ctrl Pts',(-19.5984334106447,-20.8844738455263,
-21.3624554896874));
#67417=CARTESIAN_POINT('Ctrl Pts',(-19.6014988122479,-20.8830997114248,
-21.3626596782347));
#67418=CARTESIAN_POINT('Ctrl Pts',(-19.6105424044381,-20.8790198424555,
-21.3632640343987));
#67419=CARTESIAN_POINT('Ctrl Pts',(-19.6165112337142,-20.8762936313696,
-21.3636654434041));
#67420=CARTESIAN_POINT('Ctrl Pts',(-19.6448669640108,-20.8631827205932,
-21.3655841187029));
#67421=CARTESIAN_POINT('Ctrl Pts',(-19.6670827966634,-20.8524353154302,
-21.3671222453472));
#67422=CARTESIAN_POINT('Ctrl Pts',(-19.7292807475042,-20.8209922084031,
-21.3715174049684));
#67423=CARTESIAN_POINT('Ctrl Pts',(-19.7687964036886,-20.7994067013962,
-21.374415197408));
#67424=CARTESIAN_POINT('Ctrl Pts',(-19.88952039456,-20.728372134586,-21.3835369426157));
#67425=CARTESIAN_POINT('Ctrl Pts',(-19.968107776952,-20.6747021716754,-21.3898620877258));
#67426=CARTESIAN_POINT('Ctrl Pts',(-20.160632426997,-20.5232656827976,-21.4060183990992));
#67427=CARTESIAN_POINT('Ctrl Pts',(-20.2682886293656,-20.4183322888617,
-21.4156928769252));
#67428=CARTESIAN_POINT('Ctrl Pts',(-20.3729857267611,-20.2920053876034,
-21.4257089935953));
#67429=CARTESIAN_POINT('Ctrl Pts',(-20.3818931560424,-20.2810360465027,
-21.4265671086272));
#67430=CARTESIAN_POINT('Ctrl Pts',(-20.3959063430243,-20.263421558129,-21.4279269323577));
#67431=CARTESIAN_POINT('Ctrl Pts',(-20.4010835075936,-20.2568340039992,
-21.4284315172946));
#67432=CARTESIAN_POINT('Ctrl Pts',(-20.4101513952445,-20.2451537298734,
-21.4293192798389));
#67433=CARTESIAN_POINT('Ctrl Pts',(-20.4140583306603,-20.2400737850971,
-21.4297031032954));
#67434=CARTESIAN_POINT('Ctrl Pts',(-20.4220971023071,-20.2295226717649,
-21.430495646683));
#67435=CARTESIAN_POINT('Ctrl Pts',(-20.4262255532588,-20.2240490093937,
-21.4309042295636));
#67436=CARTESIAN_POINT('Ctrl Pts',(-20.4367657948163,-20.2099322157558,
-21.4319514664971));
#67437=CARTESIAN_POINT('Ctrl Pts',(-20.4431384531545,-20.2012600073221,
-21.432588579356));
#67438=CARTESIAN_POINT('Ctrl Pts',(-20.4695463826491,-20.1647425511917,
-21.4352459081674));
#67439=CARTESIAN_POINT('Ctrl Pts',(-20.488970148204,-20.1364600957453,-21.437242430499));
#67440=CARTESIAN_POINT('Ctrl Pts',(-20.5378432110347,-20.0614537507977,
-21.442391173593));
#67441=CARTESIAN_POINT('Ctrl Pts',(-20.5661674189159,-20.0140269094543,
-21.4455035225487));
#67442=CARTESIAN_POINT('Ctrl Pts',(-20.6274484735311,-19.9016515664535,
-21.4526164833822));
#67443=CARTESIAN_POINT('Ctrl Pts',(-20.658973887806,-19.8360030591184,-21.4565792730157));
#67444=CARTESIAN_POINT('Ctrl Pts',(-20.6995927811212,-19.7388860102984,
-21.4622948261543));
#67445=CARTESIAN_POINT('Ctrl Pts',(-20.7114372793834,-19.7086282580148,
-21.4640561413387));
#67446=CARTESIAN_POINT('Ctrl Pts',(-20.722580582091,-19.6781103693865,-21.465822579505));
#67447=CARTESIAN_POINT('Ctrl Pts',(-20.7225805821494,-19.6781103692267,
-21.2464098430158));
#67448=CARTESIAN_POINT('Ctrl Pts',(-20.7151809012897,-19.698375692923,-21.2451568900026));
#67449=CARTESIAN_POINT('Ctrl Pts',(-20.7074719860344,-19.7185264049827,
-21.2438894700321));
#67450=CARTESIAN_POINT('Ctrl Pts',(-20.6968058209637,-19.7451791787207,
-21.2421798140781));
#67451=CARTESIAN_POINT('Ctrl Pts',(-20.6941216461761,-19.7517893655548,
-21.2417530485997));
#67452=CARTESIAN_POINT('Ctrl Pts',(-20.6898485633233,-19.7621617588142,
-21.2410788630868));
#67453=CARTESIAN_POINT('Ctrl Pts',(-20.6882820649243,-19.7659332209493,
-21.2408327803363));
#67454=CARTESIAN_POINT('Ctrl Pts',(-20.6853241227265,-19.7729969202685,
-21.2403700669868));
#67455=CARTESIAN_POINT('Ctrl Pts',(-20.6839352503089,-19.7762901758043,
-21.2401535926792));
#67456=CARTESIAN_POINT('Ctrl Pts',(-20.6807339855021,-19.783827558518,-21.239656439768));
#67457=CARTESIAN_POINT('Ctrl Pts',(-20.6789160539789,-19.7880692791049,
-21.2393754270876));
#67458=CARTESIAN_POINT('Ctrl Pts',(-20.6732460556527,-19.801180334003,-21.23850306994));
#67459=CARTESIAN_POINT('Ctrl Pts',(-20.6693471421221,-19.8100290993669,
-21.2379089766039));
#67460=CARTESIAN_POINT('Ctrl Pts',(-20.6276874059676,-19.9028491342297,
-21.2316233024324));
#67461=CARTESIAN_POINT('Ctrl Pts',(-20.5845514899138,-19.9842893332979,
-21.2256463578304));
#67462=CARTESIAN_POINT('Ctrl Pts',(-20.4721083710498,-20.1667509646173,
-21.2115516109801));
#67463=CARTESIAN_POINT('Ctrl Pts',(-20.3990542360701,-20.2651025885536,
-21.2034109595741));
#67464=CARTESIAN_POINT('Ctrl Pts',(-20.2756220774325,-20.4042926086402,
-21.1913749560756));
#67465=CARTESIAN_POINT('Ctrl Pts',(-20.2311926486573,-20.4500546900007,
-21.1873152381914));
#67466=CARTESIAN_POINT('Ctrl Pts',(-20.1664053107302,-20.511018717677,-21.1817683175493));
#67467=CARTESIAN_POINT('Ctrl Pts',(-20.1477410408678,-20.5279634166997,
-21.1802101097512));
#67468=CARTESIAN_POINT('Ctrl Pts',(-20.1189668361614,-20.553163937167,-21.1778667360507));
#67469=CARTESIAN_POINT('Ctrl Pts',(-20.1090763545244,-20.5616658417592,
-21.1770714691907));
#67470=CARTESIAN_POINT('Ctrl Pts',(-20.0907048659911,-20.5771651522004,
-21.1756127710069));
#67471=CARTESIAN_POINT('Ctrl Pts',(-20.0822467551121,-20.584188886067,-21.1749482736233));
#67472=CARTESIAN_POINT('Ctrl Pts',(-20.0684444358686,-20.5954700245966,
-21.1738751989208));
#67473=CARTESIAN_POINT('Ctrl Pts',(-20.0631337397865,-20.5997679380398,
-21.1734649829231));
#67474=CARTESIAN_POINT('Ctrl Pts',(-20.0530398016817,-20.6078563483877,
-21.1726902874773));
#67475=CARTESIAN_POINT('Ctrl Pts',(-20.0482608031583,-20.6116520079229,
-21.1723256027671));
#67476=CARTESIAN_POINT('Ctrl Pts',(-20.0371069785972,-20.6204324038952,
-21.1714792774759));
#67477=CARTESIAN_POINT('Ctrl Pts',(-20.0307198245265,-20.6254013814665,
-21.1709982678441));
#67478=CARTESIAN_POINT('Ctrl Pts',(-20.0141841566172,-20.6381140161988,
-21.1697621944453));
#67479=CARTESIAN_POINT('Ctrl Pts',(-20.0039937205729,-20.6458027957396,
-21.1690092928549));
#67480=CARTESIAN_POINT('Ctrl Pts',(-19.9390512959285,-20.693886866537,-21.1642655842235));
#67481=CARTESIAN_POINT('Ctrl Pts',(-19.8824450058645,-20.731717368187,-21.1603753219429));
#67482=CARTESIAN_POINT('Ctrl Pts',(-19.6842207853306,-20.8507889829137,
-21.1474096945091));
#67483=CARTESIAN_POINT('Ctrl Pts',(-19.5350931339249,-20.9183587656678,
-21.1387753113413));
#67484=CARTESIAN_POINT('Ctrl Pts',(-19.3268970384958,-20.9850358507186,
-21.126700253472));
#67485=CARTESIAN_POINT('Ctrl Pts',(-19.2734664663781,-20.9998615054935,
-21.123594526353));
#67486=CARTESIAN_POINT('Ctrl Pts',(-19.1917461770392,-21.0191167450673,
-21.1187518383991));
#67487=CARTESIAN_POINT('Ctrl Pts',(-19.1638446024887,-21.0250983182965,
-21.117082298086));
#67488=CARTESIAN_POINT('Ctrl Pts',(-19.129008203159,-21.0318331249412,-21.1149682959755));
#67489=CARTESIAN_POINT('Ctrl Pts',(-19.1221778031881,-21.0331187612011,
-21.1145523991981));
#67490=CARTESIAN_POINT('Ctrl Pts',(-19.1113601054842,-21.0350997893233,
-21.1138913254639));
#67491=CARTESIAN_POINT('Ctrl Pts',(-19.1073768621791,-21.0358174343373,
-21.113647395275));
#67492=CARTESIAN_POINT('Ctrl Pts',(-19.0998621341073,-21.0371490947439,
-21.1131861925066));
#67493=CARTESIAN_POINT('Ctrl Pts',(-19.0963311398356,-21.037765565178,-21.1129690612158));
#67494=CARTESIAN_POINT('Ctrl Pts',(-19.0882556979009,-21.0391543184373,
-21.1124715243904));
#67495=CARTESIAN_POINT('Ctrl Pts',(-19.0837102896108,-21.0399207266753,
-21.1121907899535));
#67496=CARTESIAN_POINT('Ctrl Pts',(-19.0716369458633,-21.0419159008968,
-21.1114433573562));
#67497=CARTESIAN_POINT('Ctrl Pts',(-19.0641048904745,-21.0431188242895,
-21.1109752549015));
#67498=CARTESIAN_POINT('Ctrl Pts',(-19.0113293099853,-21.051255227184,-21.1076834758471));
#67499=CARTESIAN_POINT('Ctrl Pts',(-18.9658812712963,-21.0567599492808,
-21.1047878632221));
#67500=CARTESIAN_POINT('Ctrl Pts',(-18.9096436732841,-21.0617280930136,
-21.1011583933981));
#67501=CARTESIAN_POINT('Ctrl Pts',(-18.8989859729359,-21.0625882944636,
-21.1004685066869));
#67502=CARTESIAN_POINT('Ctrl Pts',(-18.7360005561771,-21.0745010916135,
-21.0898909620382));
#67503=CARTESIAN_POINT('Ctrl Pts',(-18.5829201314274,-21.0691191483902,
-21.0796342248313));
#67504=CARTESIAN_POINT('Ctrl Pts',(-18.3398835153214,-21.0340603373794,
-21.0636972639725));
#67505=CARTESIAN_POINT('Ctrl Pts',(-18.2489842435714,-21.0147813028083,
-21.0578076430166));
#67506=CARTESIAN_POINT('Ctrl Pts',(-18.1393414552467,-20.9838746727492,
-21.0508125005824));
#67507=CARTESIAN_POINT('Ctrl Pts',(-18.1191357823133,-20.9778517998307,
-21.0495277076858));
#67508=CARTESIAN_POINT('Ctrl Pts',(-18.0904777832314,-20.9688411919096,
-21.0477110701582));
#67509=CARTESIAN_POINT('Ctrl Pts',(-18.0819497443941,-20.9661002221531,
-21.0471711860068));
#67510=CARTESIAN_POINT('Ctrl Pts',(-18.0672475774973,-20.9612716787602,
-21.0462415917969));
#67511=CARTESIAN_POINT('Ctrl Pts',(-18.061065269426,-20.9592095859284,-21.0458510489854));
#67512=CARTESIAN_POINT('Ctrl Pts',(-18.0492323639408,-20.9552019361616,
-21.0451041963304));
#67513=CARTESIAN_POINT('Ctrl Pts',(-18.0435802983861,-20.9532609398044,
-21.0447477402189));
#67514=CARTESIAN_POINT('Ctrl Pts',(-18.0288741174594,-20.9481409195988,
-21.043820969016));
#67515=CARTESIAN_POINT('Ctrl Pts',(-18.0198331983671,-20.9449241995567,
-21.0432519085));
#67516=CARTESIAN_POINT('Ctrl Pts',(-17.9889239525977,-20.9336894763137,
-21.0413085124323));
#67517=CARTESIAN_POINT('Ctrl Pts',(-17.9671657534014,-20.9253719361747,
-21.0399441529836));
#67518=CARTESIAN_POINT('Ctrl Pts',(-17.7867624565159,-20.8529743856351,
-21.0286518996669));
#67519=CARTESIAN_POINT('Ctrl Pts',(-17.6362869280282,-20.7702396597499,
-21.0194319214345));
#67520=CARTESIAN_POINT('Ctrl Pts',(-17.4242275491654,-20.6176266887034,
-21.0052256167648));
#67521=CARTESIAN_POINT('Ctrl Pts',(-17.3544997997982,-20.5603509426405,
-21.000300137549));
#67522=CARTESIAN_POINT('Ctrl Pts',(-17.2604303378236,-20.4724512888722,
-20.9929553840031));
#67523=CARTESIAN_POINT('Ctrl Pts',(-17.2329484304121,-20.445326298497,-20.9907140073888));
#67524=CARTESIAN_POINT('Ctrl Pts',(-17.2009536051128,-20.4119711469122,
-20.9879643324888));
#67525=CARTESIAN_POINT('Ctrl Pts',(-17.1957115255254,-20.4064468240535,
-20.9875091327688));
#67526=CARTESIAN_POINT('Ctrl Pts',(-17.1876306650577,-20.3978383207474,
-20.9867998873983));
#67527=CARTESIAN_POINT('Ctrl Pts',(-17.1847709836745,-20.3947737258723,
-20.9865474158765));
#67528=CARTESIAN_POINT('Ctrl Pts',(-17.1794976182552,-20.3890887368434,
-20.9860790539247));
#67529=CARTESIAN_POINT('Ctrl Pts',(-17.177081440136,-20.3864707350773,-20.9858633588662));
#67530=CARTESIAN_POINT('Ctrl Pts',(-17.1716505172992,-20.3805562813599,
-20.985376054872));
#67531=CARTESIAN_POINT('Ctrl Pts',(-17.1686396098713,-20.3772563991359,
-20.985104163261));
#67532=CARTESIAN_POINT('Ctrl Pts',(-17.1598311659693,-20.3675409753861,
-20.9843037118207));
#67533=CARTESIAN_POINT('Ctrl Pts',(-17.1540625473198,-20.3610995035121,
-20.9837730572173));
#67534=CARTESIAN_POINT('Ctrl Pts',(-17.1140943616616,-20.3159154402178,
-20.9800522807053));
#67535=CARTESIAN_POINT('Ctrl Pts',(-17.0812867997021,-20.2759704416452,
-20.9767710271767));
#67536=CARTESIAN_POINT('Ctrl Pts',(-17.0366100744695,-20.2173232628266,
-20.9720114015117));
#67537=CARTESIAN_POINT('Ctrl Pts',(-17.0235191220997,-20.1995698929873,
-20.9705777308999));
#67538=CARTESIAN_POINT('Ctrl Pts',(-16.9840342976884,-20.144232382046,-20.966137766717));
#67539=CARTESIAN_POINT('Ctrl Pts',(-16.9585843969024,-20.1059918777097,
-20.9631098909174));
#67540=CARTESIAN_POINT('Ctrl Pts',(-16.8768042599706,-19.9739940599948,
-20.9528524498352));
#67541=CARTESIAN_POINT('Ctrl Pts',(-16.8264948390657,-19.8767028731446,
-20.9456214661846));
#67542=CARTESIAN_POINT('Ctrl Pts',(-16.7624917060153,-19.725225034177,-20.9350516013849));
#67543=CARTESIAN_POINT('Ctrl Pts',(-16.7430436419927,-19.6736754860697,
-20.9315643118513));
#67544=CARTESIAN_POINT('Ctrl Pts',(-16.7147840953464,-19.5888923770621,
-20.9260094054404));
#67545=CARTESIAN_POINT('Ctrl Pts',(-16.7047327990432,-19.5561023197927,
-20.9239033881697));
#67546=CARTESIAN_POINT('Ctrl Pts',(-16.6925670008698,-19.5126755570457,
-20.9211678392338));
#67547=CARTESIAN_POINT('Ctrl Pts',(-16.6897316436486,-19.5022478207212,
-20.9205149824574));
#67548=CARTESIAN_POINT('Ctrl Pts',(-16.685217618378,-19.4851297404333,-20.9194496972804));
#67549=CARTESIAN_POINT('Ctrl Pts',(-16.6834916088089,-19.4784521885083,
-20.9190357400471));
#67550=CARTESIAN_POINT('Ctrl Pts',(-16.6802131660186,-19.4655078583839,
-20.9182363370981));
#67551=CARTESIAN_POINT('Ctrl Pts',(-16.6786567087105,-19.4592421871588,
-20.9178507651476));
#67552=CARTESIAN_POINT('Ctrl Pts',(-16.67512833542,-19.4447554572578,-20.9169624231352));
#67553=CARTESIAN_POINT('Ctrl Pts',(-16.6731769453728,-19.4365294754173,
-20.9164603192327));
#67554=CARTESIAN_POINT('Ctrl Pts',(-16.6680598806704,-19.4143684912192,
-20.9151137450957));
#67555=CARTESIAN_POINT('Ctrl Pts',(-16.6649859002001,-19.400412609178,-20.9142722168645));
#67556=CARTESIAN_POINT('Ctrl Pts',(-16.6380607690271,-19.271996305939,-20.9065856210845));
#67557=CARTESIAN_POINT('Ctrl Pts',(-16.6235870997623,-19.1557683937764,
-20.9000577587314));
#67558=CARTESIAN_POINT('Ctrl Pts',(-16.612097379801,-18.8761836513789,-20.8847397841375));
#67559=CARTESIAN_POINT('Ctrl Pts',(-16.6242138937639,-18.7132333547738,
-20.8761329405072));
#67560=CARTESIAN_POINT('Ctrl Pts',(-16.6609684104183,-18.5215660670561,
-20.8649248914188));
#67561=CARTESIAN_POINT('Ctrl Pts',(-16.6677801148839,-18.4899735165662,
-20.863039780627));
#67562=CARTESIAN_POINT('Ctrl Pts',(-16.6769960023837,-18.4515244600164,
-20.8606855787975));
#67563=CARTESIAN_POINT('Ctrl Pts',(-16.6787161943862,-18.4445064657664,
-20.8602534085993));
#67564=CARTESIAN_POINT('Ctrl Pts',(-16.6814702302107,-18.4335143144678,
-20.8595724420682));
#67565=CARTESIAN_POINT('Ctrl Pts',(-16.682479785303,-18.4295340489524,-20.859325025088));
#67566=CARTESIAN_POINT('Ctrl Pts',(-16.6843892282124,-18.4220967587648,
-20.8588611041058));
#67567=CARTESIAN_POINT('Ctrl Pts',(-16.6852862879052,-18.4186390658179,
-20.858644764284));
#67568=CARTESIAN_POINT('Ctrl Pts',(-16.6873549502471,-18.4107476831028,
-20.8581495268807));
#67569=CARTESIAN_POINT('Ctrl Pts',(-16.6885322068715,-18.4063155338617,
-20.8578703058359));
#67570=CARTESIAN_POINT('Ctrl Pts',(-16.6921982200937,-18.3926922466135,
-20.8570088212555));
#67571=CARTESIAN_POINT('Ctrl Pts',(-16.6947345554561,-18.3835141951356,
-20.8564239044982));
#67572=CARTESIAN_POINT('Ctrl Pts',(-16.7185357292232,-18.2995959243037,
-20.8510361990448));
#67573=CARTESIAN_POINT('Ctrl Pts',(-16.743836590417,-18.2260701042058,-20.8460290686741));
#67574=CARTESIAN_POINT('Ctrl Pts',(-16.788529564351,-18.1162333045789,-20.8382678938088));
#67575=CARTESIAN_POINT('Ctrl Pts',(-16.8050356844214,-18.0788117456707,
-20.8355711291447));
#67576=CARTESIAN_POINT('Ctrl Pts',(-16.8696063712948,-17.94320199509,-20.8256493319105));
#67577=CARTESIAN_POINT('Ctrl Pts',(-16.9241745769758,-17.8482915134168,
-20.8184220279744));
#67578=CARTESIAN_POINT('Ctrl Pts',(-17.0168587405443,-17.7125883932035,
-20.8078598389365));
#67579=CARTESIAN_POINT('Ctrl Pts',(-17.0496457258955,-17.668385286558,-20.8043765462533));
#67580=CARTESIAN_POINT('Ctrl Pts',(-17.1055891224957,-17.5988034141636,
-20.7988271578512));
#67581=CARTESIAN_POINT('Ctrl Pts',(-17.1277043407155,-17.5726242511841,
-20.7967227675539));
#67582=CARTESIAN_POINT('Ctrl Pts',(-17.1576169442291,-17.5389104083168,
-20.7939889082263));
#67583=CARTESIAN_POINT('Ctrl Pts',(-17.1648493857497,-17.5308835061051,
-20.7933361569086));
#67584=CARTESIAN_POINT('Ctrl Pts',(-17.1767991672402,-17.5178235323663,
-20.7922709472738));
#67585=CARTESIAN_POINT('Ctrl Pts',(-17.1814801501911,-17.5127575980527,
-20.7918569613977));
#67586=CARTESIAN_POINT('Ctrl Pts',(-17.190591411671,-17.5029932264992,-20.7910574359211));
#67587=CARTESIAN_POINT('Ctrl Pts',(-17.1950185883894,-17.4982920113303,
-20.7906717704168));
#67588=CARTESIAN_POINT('Ctrl Pts',(-17.2052937529954,-17.4874803708258,
-20.7897831160845));
#67589=CARTESIAN_POINT('Ctrl Pts',(-17.2111570117524,-17.4813845607437,
-20.7892807942162));
#67590=CARTESIAN_POINT('Ctrl Pts',(-17.2270312020111,-17.4650774993905,
-20.7879334180775));
#67591=CARTESIAN_POINT('Ctrl Pts',(-17.2371094313686,-17.4549321587139,
-20.7870913100847));
#67592=CARTESIAN_POINT('Ctrl Pts',(-17.3310036155552,-17.3623089324332,
-20.779364792049));
#67593=CARTESIAN_POINT('Ctrl Pts',(-17.4214570547904,-17.286841479805,-20.7728014692284));
#67594=CARTESIAN_POINT('Ctrl Pts',(-17.6516594578399,-17.1252524985302,
-20.7574079964102));
#67595=CARTESIAN_POINT('Ctrl Pts',(-17.7960292751888,-17.0470942151458,
-20.7487611914907));
#67596=CARTESIAN_POINT('Ctrl Pts',(-17.9767199868582,-16.9748361343166,
-20.7375685113015));
#67597=CARTESIAN_POINT('Ctrl Pts',(-18.0057509713667,-16.9639599868621,
-20.7357583226344));
#67598=CARTESIAN_POINT('Ctrl Pts',(-18.041742500261,-16.9513702367761,-20.7334874885538));
#67599=CARTESIAN_POINT('Ctrl Pts',(-18.0484882638105,-16.9490487894883,
-20.7330607358659));
#67600=CARTESIAN_POINT('Ctrl Pts',(-18.0591164680737,-16.9454512417125,
-20.7323863937624));
#67601=CARTESIAN_POINT('Ctrl Pts',(-18.062991161965,-16.9441521871218,-20.732140138974));
#67602=CARTESIAN_POINT('Ctrl Pts',(-18.0702630837045,-16.9417375565125,
-20.7316771606436));
#67603=CARTESIAN_POINT('Ctrl Pts',(-18.0736593846302,-16.9406193655189,
-20.7314605938004));
#67604=CARTESIAN_POINT('Ctrl Pts',(-18.0814483199326,-16.9380768066054,
-20.7309631694134));
#67605=CARTESIAN_POINT('Ctrl Pts',(-18.0858427797469,-16.9366582074118,
-20.7306819776656));
#67606=CARTESIAN_POINT('Ctrl Pts',(-18.0994689304275,-16.9323086530672,
-20.7298084506056));
#67607=CARTESIAN_POINT('Ctrl Pts',(-18.1087159687357,-16.9294267164841,
-20.729213355607));
#67608=CARTESIAN_POINT('Ctrl Pts',(-18.2199628802434,-16.8955912489628,
-20.7220292534648));
#67609=CARTESIAN_POINT('Ctrl Pts',(-18.324128948869,-16.8723241983385,-20.7150599223007));
#67610=CARTESIAN_POINT('Ctrl Pts',(-18.5378458842779,-16.8412703940283,
-20.700813451564));
#67611=CARTESIAN_POINT('Ctrl Pts',(-18.6471661833861,-16.8339540624244,
-20.6935567741784));
#67612=CARTESIAN_POINT('Ctrl Pts',(-18.8191791912484,-16.8357877355927,
-20.6824361753263));
#67613=CARTESIAN_POINT('Ctrl Pts',(-18.8817359967659,-16.8392328358894,
-20.6784511901261));
#67614=CARTESIAN_POINT('Ctrl Pts',(-18.9688258376729,-16.8479169160879,
-20.6729961074588));
#67615=CARTESIAN_POINT('Ctrl Pts',(-18.9935540026917,-16.8508239959902,
-20.6714575304749));
#67616=CARTESIAN_POINT('Ctrl Pts',(-19.036759637992,-16.8566777328146,-20.6687868523993));
#67617=CARTESIAN_POINT('Ctrl Pts',(-19.0552596515311,-16.8594343323808,
-20.6676489700601));
#67618=CARTESIAN_POINT('Ctrl Pts',(-19.0821456222421,-16.8638054513975,
-20.6660031193632));
#67619=CARTESIAN_POINT('Ctrl Pts',(-19.090561795757,-16.8652260457255,-20.6654890348276));
#67620=CARTESIAN_POINT('Ctrl Pts',(-19.1053189666751,-16.8678088429808,
-20.6645895244084));
#67621=CARTESIAN_POINT('Ctrl Pts',(-19.1116636326348,-16.8689491758432,
-20.6642034090808));
#67622=CARTESIAN_POINT('Ctrl Pts',(-19.1239854232061,-16.8712219301125,
-20.6634547123123));
#67623=CARTESIAN_POINT('Ctrl Pts',(-19.1299630637734,-16.8723511691265,
-20.6630920337509));
#67624=CARTESIAN_POINT('Ctrl Pts',(-19.1442606325555,-16.8751160100363,
-20.6622258044872));
#67625=CARTESIAN_POINT('Ctrl Pts',(-19.1525758062836,-16.8767758694626,
-20.6617230309353));
#67626=CARTESIAN_POINT('Ctrl Pts',(-19.1826603860175,-16.882969475897,-20.6599074474704));
#67627=CARTESIAN_POINT('Ctrl Pts',(-19.2043684754828,-16.8877962784277,
-20.6586039909661));
#67628=CARTESIAN_POINT('Ctrl Pts',(-19.4052514603699,-16.9357963450666,
-20.6465932891083));
#67629=CARTESIAN_POINT('Ctrl Pts',(-19.5781410126775,-17.001849293089,-20.6367286530683));
#67630=CARTESIAN_POINT('Ctrl Pts',(-19.8115637456355,-17.1279644304358,
-20.6222693001478));
#67631=CARTESIAN_POINT('Ctrl Pts',(-19.8805505657211,-17.1705205217267,
-20.6178176188594));
#67632=CARTESIAN_POINT('Ctrl Pts',(-19.9766422664143,-17.2376943237939,
-20.6111128236623));
#67633=CARTESIAN_POINT('Ctrl Pts',(-20.0058197364711,-17.2592277303693,
-20.609004110606));
#67634=CARTESIAN_POINT('Ctrl Pts',(-20.040330275753,-17.2860929914317,-20.6064014951247));
#67635=CARTESIAN_POINT('Ctrl Pts',(-20.0462081769648,-17.2907189740851,
-20.6059543080364));
#67636=CARTESIAN_POINT('Ctrl Pts',(-20.0553184657506,-17.2979674015733,
-20.6052548840553));
#67637=CARTESIAN_POINT('Ctrl Pts',(-20.0585679101481,-17.3005684466764,
-20.605004152083));
#67638=CARTESIAN_POINT('Ctrl Pts',(-20.064586644847,-17.3054153852174,-20.6045373436736));
#67639=CARTESIAN_POINT('Ctrl Pts',(-20.0673579396073,-17.3076586980289,
-20.6043214519178));
#67640=CARTESIAN_POINT('Ctrl Pts',(-20.0736189984585,-17.3127531466337,
-20.6038315428823));
#67641=CARTESIAN_POINT('Ctrl Pts',(-20.0771053160298,-17.3156084159083,
-20.6035572294908));
#67642=CARTESIAN_POINT('Ctrl Pts',(-20.087394471296,-17.3240901923961,-20.6027432103989));
#67643=CARTESIAN_POINT('Ctrl Pts',(-20.0941711619113,-17.3297480649717,
-20.6022013047546));
#67644=CARTESIAN_POINT('Ctrl Pts',(-20.1437896734811,-17.371704121525,-20.5981920727157));
#67645=CARTESIAN_POINT('Ctrl Pts',(-20.1852038922591,-17.4096485278185,
-20.5946172570416));
#67646=CARTESIAN_POINT('Ctrl Pts',(-20.2694067173499,-17.4931928310492,
-20.5869375741964));
#67647=CARTESIAN_POINT('Ctrl Pts',(-20.3117850996791,-17.5391356368496,
-20.5828223138073));
#67648=CARTESIAN_POINT('Ctrl Pts',(-20.4227519187064,-17.6706641931095,
-20.5714554048852));
#67649=CARTESIAN_POINT('Ctrl Pts',(-20.4868273101149,-17.7598152940171,
-20.564205795166));
#67650=CARTESIAN_POINT('Ctrl Pts',(-20.5724489149629,-17.90087597484,-20.5535967989467));
#67651=CARTESIAN_POINT('Ctrl Pts',(-20.599318236279,-17.9493311416735,-20.5500891540958));
#67652=CARTESIAN_POINT('Ctrl Pts',(-20.6397608396946,-18.029530453112,-20.5445055773609));
#67653=CARTESIAN_POINT('Ctrl Pts',(-20.6545119754037,-18.060647985304,-20.5423907557199));
#67654=CARTESIAN_POINT('Ctrl Pts',(-20.6728942822845,-18.1020028838744,
-20.5396455710918));
#67655=CARTESIAN_POINT('Ctrl Pts',(-20.6772145069152,-18.1119264780837,
-20.5389916811012));
#67656=CARTESIAN_POINT('Ctrl Pts',(-20.6841645653466,-18.1282313471316,
-20.537925111408));
#67657=CARTESIAN_POINT('Ctrl Pts',(-20.6868395931637,-18.1345930325052,
-20.5375108962547));
#67658=CARTESIAN_POINT('Ctrl Pts',(-20.6919565598858,-18.1469305737922,
-20.5367112718804));
#67659=CARTESIAN_POINT('Ctrl Pts',(-20.6944023640957,-18.1529047342856,
-20.536325734962));
#67660=CARTESIAN_POINT('Ctrl Pts',(-20.6999852466446,-18.1667214793585,
-20.5354378681961));
#67661=CARTESIAN_POINT('Ctrl Pts',(-20.7031028042766,-18.1745718719074,
-20.5349362018097));
#67662=CARTESIAN_POINT('Ctrl Pts',(-20.7113578715634,-18.1957273899532,
-20.5335916742474));
#67663=CARTESIAN_POINT('Ctrl Pts',(-20.7164081052022,-18.209066266619,-20.5327517402014));
#67664=CARTESIAN_POINT('Ctrl Pts',(-20.7714922872059,-18.3591188841948,
-20.5233872254654));
#67665=CARTESIAN_POINT('Ctrl Pts',(-20.8074336418282,-18.5005981030119,
-20.5153747188882));
#67666=CARTESIAN_POINT('Ctrl Pts',(-20.8435716231846,-18.7468873152343,
-20.5018390224732));
#67667=CARTESIAN_POINT('Ctrl Pts',(-20.8510665767245,-18.8500662004454,
-20.496275824337));
#67668=CARTESIAN_POINT('Ctrl Pts',(-20.8509605931098,-19.0134280306006,
-20.4871374269587));
#67669=CARTESIAN_POINT('Ctrl Pts',(-20.8483662197824,-19.0734481143259,
-20.4837076978117));
#67670=CARTESIAN_POINT('Ctrl Pts',(-20.8424571655091,-19.1422045950063,
-20.4796144560487));
#67671=CARTESIAN_POINT('Ctrl Pts',(-20.8416326176233,-19.151133496576,-20.4790796927553));
#67672=CARTESIAN_POINT('Ctrl Pts',(-20.8403055945935,-19.1645707348717,
-20.4782697314217));
#67673=CARTESIAN_POINT('Ctrl Pts',(-20.8398453005765,-19.1690832658228,
-20.477996845725));
#67674=CARTESIAN_POINT('Ctrl Pts',(-20.8389970512125,-19.1771424971639,
-20.4775078488365));
#67675=CARTESIAN_POINT('Ctrl Pts',(-20.8386146293109,-19.1806897275217,
-20.4772920515391));
#67676=CARTESIAN_POINT('Ctrl Pts',(-20.8377689774517,-19.1883519337853,
-20.4768246768379));
#67677=CARTESIAN_POINT('Ctrl Pts',(-20.8373026472245,-19.1924664645893,
-20.4765729324308));
#67678=CARTESIAN_POINT('Ctrl Pts',(-20.8359714184113,-19.2039119845512,
-20.4758705576885));
#67679=CARTESIAN_POINT('Ctrl Pts',(-20.8350802524445,-19.211239774869,-20.4754184877748));
#67680=CARTESIAN_POINT('Ctrl Pts',(-20.8297855240793,-19.2529550296279,
-20.4728319418377));
#67681=CARTESIAN_POINT('Ctrl Pts',(-20.8245763695238,-19.2872327764827,
-20.4706561388139));
#67682=CARTESIAN_POINT('Ctrl Pts',(-20.805407201064,-19.3954149280918,-20.4636610476318));
#67683=CARTESIAN_POINT('Ctrl Pts',(-20.788350364743,-19.4687084470379,-20.4587324323691));
#67684=CARTESIAN_POINT('Ctrl Pts',(-20.7540340641799,-19.5871935736654,
-20.4505956310275));
#67685=CARTESIAN_POINT('Ctrl Pts',(-20.7390724262502,-19.6329445370197,
-20.4474103621586));
#67686=CARTESIAN_POINT('Ctrl Pts',(-20.7225807116741,-19.6781100145004,
-20.4442392611068));
#67687=CARTESIAN_POINT('Origin',(-18.734,-18.952,0.));
#67688=CARTESIAN_POINT('',(-20.7225805821918,-19.6781103691105,-19.6425236185391));
#67689=CARTESIAN_POINT('',(-20.7227693935251,-19.6781792853784,-19.8664843272136));
#67690=CARTESIAN_POINT('',(-20.7225805821191,-19.6781103693095,0.));
#67691=CARTESIAN_POINT('',(-20.8479201338006,-18.951171742175,-19.9109991854362));
#67692=CARTESIAN_POINT('Ctrl Pts',(-20.7227693935251,-19.6781792853784,
-19.8664843272136));
#67693=CARTESIAN_POINT('Ctrl Pts',(-20.8048847772777,-19.4459845977201,
-19.8813041251349));
#67694=CARTESIAN_POINT('Ctrl Pts',(-20.846952464507,-19.1984404792794,-19.8961239230562));
#67695=CARTESIAN_POINT('Ctrl Pts',(-20.847823891442,-18.9511685861153,-19.9109437209775));
#67696=CARTESIAN_POINT('Ctrl Pts',(-20.8509998750795,-18.9512727356193,
-19.9127740399324));
#67697=CARTESIAN_POINT('Ctrl Pts',(-20.8509329970543,-18.7565969413839,
-19.9239834015842));
#67698=CARTESIAN_POINT('Ctrl Pts',(-20.8240164173847,-18.5628627648932,
-19.9342647202721));
#67699=CARTESIAN_POINT('Ctrl Pts',(-20.7539265921552,-18.3151986713921,
-19.9484106374171));
#67700=CARTESIAN_POINT('Ctrl Pts',(-20.7341848163476,-18.2556675204103,
-19.9519023759823));
#67701=CARTESIAN_POINT('Ctrl Pts',(-20.7008062966819,-18.1682154893869,
-19.9572865832378));
#67702=CARTESIAN_POINT('Ctrl Pts',(-20.689148933844,-18.1395730264876,-19.9590923501055));
#67703=CARTESIAN_POINT('Ctrl Pts',(-20.6740381863279,-18.1046561236404,
-19.9613582347434));
#67704=CARTESIAN_POINT('Ctrl Pts',(-20.6711741824253,-18.0981288195114,
-19.9617846298524));
#67705=CARTESIAN_POINT('Ctrl Pts',(-20.6666170550983,-18.0878836845935,
-19.9624585183398));
#67706=CARTESIAN_POINT('Ctrl Pts',(-20.6649460104447,-18.0841560092348,
-19.9627046797831));
#67707=CARTESIAN_POINT('Ctrl Pts',(-20.66179207534,-18.0771745887545,-19.9631675666607));
#67708=CARTESIAN_POINT('Ctrl Pts',(-20.6603117271982,-18.0739197560113,
-19.9633841359097));
#67709=CARTESIAN_POINT('Ctrl Pts',(-20.6568999800879,-18.0664685173876,
-19.9638816696385));
#67710=CARTESIAN_POINT('Ctrl Pts',(-20.6549630923311,-18.062274684474,-19.9641629690023));
#67711=CARTESIAN_POINT('Ctrl Pts',(-20.6489187126931,-18.0492988762204,
-19.9650371755357));
#67712=CARTESIAN_POINT('Ctrl Pts',(-20.6447646758537,-18.0405388980323,
-19.9656328485742));
#67713=CARTESIAN_POINT('Ctrl Pts',(-20.5974983407664,-17.9426075312916,
-19.9723513825971));
#67714=CARTESIAN_POINT('Ctrl Pts',(-20.5482438232996,-17.8565485333077,
-19.9788036086315));
#67715=CARTESIAN_POINT('Ctrl Pts',(-20.3994705247197,-17.6343296035303,
-19.9964201072025));
#67716=CARTESIAN_POINT('Ctrl Pts',(-20.2894060373859,-17.5060483292051,
-20.0076072383412));
#67717=CARTESIAN_POINT('Ctrl Pts',(-20.1424171177537,-17.3711730409822,
-20.0201341058102));
#67718=CARTESIAN_POINT('Ctrl Pts',(-20.1190845959435,-17.3506900764286,
-20.0220635731716));
#67719=CARTESIAN_POINT('Ctrl Pts',(-20.0837111244639,-17.3209885883243,
-20.0249032042272));
#67720=CARTESIAN_POINT('Ctrl Pts',(-20.0720088310794,-17.3113748962161,
-20.0258292017461));
#67721=CARTESIAN_POINT('Ctrl Pts',(-20.0531030042032,-17.2961801840757,
-20.0273041307332));
#67722=CARTESIAN_POINT('Ctrl Pts',(-20.0459650155932,-17.2905187932341,
-20.0278562767433));
#67723=CARTESIAN_POINT('Ctrl Pts',(-20.032281594028,-17.279809154674,-20.0289058492431));
#67724=CARTESIAN_POINT('Ctrl Pts',(-20.0257427224932,-17.2747528320202,
-20.0294035922447));
#67725=CARTESIAN_POINT('Ctrl Pts',(-20.01421400205,-17.2659454119496,-20.030274561818));
#67726=CARTESIAN_POINT('Ctrl Pts',(-20.0092368956509,-17.2621778714327,
-20.0306484353059));
#67727=CARTESIAN_POINT('Ctrl Pts',(-19.9993815351404,-17.2547859586397,
-20.0313845884839));
#67728=CARTESIAN_POINT('Ctrl Pts',(-19.9945041966061,-17.2511604710649,
-20.0317469096997));
#67729=CARTESIAN_POINT('Ctrl Pts',(-19.9828033277665,-17.2425408021907,
-20.0326114133704));
#67730=CARTESIAN_POINT('Ctrl Pts',(-19.9759653205673,-17.2375663774657,
-20.0331128257484));
#67731=CARTESIAN_POINT('Ctrl Pts',(-19.9511593222597,-17.2197471280602,
-20.0349182820432));
#67732=CARTESIAN_POINT('Ctrl Pts',(-19.9330199963934,-17.2071424326034,
-20.0362131104266));
#67733=CARTESIAN_POINT('Ctrl Pts',(-19.7605250822278,-17.091239235717,-20.0483000397543));
#67734=CARTESIAN_POINT('Ctrl Pts',(-19.5934087661266,-17.0083933158489,
-20.0582339598155));
#67735=CARTESIAN_POINT('Ctrl Pts',(-19.34184897396,-16.9225623314705,-20.0727242238513));
#67736=CARTESIAN_POINT('Ctrl Pts',(-19.2646841100287,-16.9010319360953,
-20.0771269185047));
#67737=CARTESIAN_POINT('Ctrl Pts',(-19.1513181956848,-16.8762276177192,
-20.0837651271762));
#67738=CARTESIAN_POINT('Ctrl Pts',(-19.1159556306609,-16.8694306715644,
-20.0858595222651));
#67739=CARTESIAN_POINT('Ctrl Pts',(-19.0730752307487,-16.8623175572817,
-20.0884462581942));
#67740=CARTESIAN_POINT('Ctrl Pts',(-19.0657047598637,-16.8611349464801,
-20.0888925479951));
#67741=CARTESIAN_POINT('Ctrl Pts',(-19.0542183933179,-16.8593541919355,
-20.0895908735595));
#67742=CARTESIAN_POINT('Ctrl Pts',(-19.0501066449248,-16.8587291418022,
-20.0898414120969));
#67743=CARTESIAN_POINT('Ctrl Pts',(-19.042466088925,-16.857590682762,-20.0903080542773));
#67744=CARTESIAN_POINT('Ctrl Pts',(-19.0389378164005,-16.857074072032,-20.0905239744579));
#67745=CARTESIAN_POINT('Ctrl Pts',(-19.0309431720641,-16.8559241182523,
-20.09101419882));
#67746=CARTESIAN_POINT('Ctrl Pts',(-19.0264760935226,-16.8552961383814,
-20.0912888006934));
#67747=CARTESIAN_POINT('Ctrl Pts',(-19.0149359627932,-16.8537114286811,
-20.09199990662));
#67748=CARTESIAN_POINT('Ctrl Pts',(-19.0078600843968,-16.8527761923558,
-20.0924375781615));
#67749=CARTESIAN_POINT('Ctrl Pts',(-18.9643547654437,-16.8472496894368,
-20.0951381493054));
#67750=CARTESIAN_POINT('Ctrl Pts',(-18.9278180434111,-16.843571348409,-20.0974473660306));
#67751=CARTESIAN_POINT('Ctrl Pts',(-18.7213427963177,-16.8281961996241,
-20.1106611846892));
#67752=CARTESIAN_POINT('Ctrl Pts',(-18.5505747211863,-16.8360933337509,
-20.1221541195018));
#67753=CARTESIAN_POINT('Ctrl Pts',(-18.2884304756434,-16.8802193876888,
-20.1394304840613));
#67754=CARTESIAN_POINT('Ctrl Pts',(-18.1954371985372,-16.9024240731352,
-20.1454976502872));
#67755=CARTESIAN_POINT('Ctrl Pts',(-18.0838147822577,-16.9372031578587,
-20.1526793179893));
#67756=CARTESIAN_POINT('Ctrl Pts',(-18.063476885015,-16.9438799992159,-20.1539839864423));
#67757=CARTESIAN_POINT('Ctrl Pts',(-18.0347244211766,-16.953804844348,-20.1558235435656));
#67758=CARTESIAN_POINT('Ctrl Pts',(-18.0262244632704,-16.9567997572317,
-20.1563667515203));
#67759=CARTESIAN_POINT('Ctrl Pts',(-18.0116019152073,-16.9620571349953,
-20.1573002549157));
#67760=CARTESIAN_POINT('Ctrl Pts',(-18.00547023807,-16.9642937877145,-20.1576914019878));
#67761=CARTESIAN_POINT('Ctrl Pts',(-17.993755266139,-16.9686285503661,-20.1584381771184));
#67762=CARTESIAN_POINT('Ctrl Pts',(-17.9881703117364,-16.9707219653826,
-20.1587939573603));
#67763=CARTESIAN_POINT('Ctrl Pts',(-17.9736826109668,-16.9762223474794,
-20.1597163031347));
#67764=CARTESIAN_POINT('Ctrl Pts',(-17.9647938323402,-16.9796659156173,
-20.1602816379677));
#67765=CARTESIAN_POINT('Ctrl Pts',(-17.9346252640623,-16.9915883753866,
-20.1621987222366));
#67766=CARTESIAN_POINT('Ctrl Pts',(-17.9134594912385,-17.0003527367573,
-20.1635408625983));
#67767=CARTESIAN_POINT('Ctrl Pts',(-17.7303956665289,-17.0796608672349,
-20.1751347597013));
#67768=CARTESIAN_POINT('Ctrl Pts',(-17.5777740492076,-17.169859802721,-20.1846244359568));
#67769=CARTESIAN_POINT('Ctrl Pts',(-17.3699313704298,-17.3307533985968,
-20.1989284464757));
#67770=CARTESIAN_POINT('Ctrl Pts',(-17.3050419795286,-17.387646972506,-20.2036512495653));
#67771=CARTESIAN_POINT('Ctrl Pts',(-17.217082933855,-17.474817791539,-20.2107230866526));
#67772=CARTESIAN_POINT('Ctrl Pts',(-17.1910710207122,-17.5020088158801,
-20.2129089615281));
#67773=CARTESIAN_POINT('Ctrl Pts',(-17.1607204334145,-17.535476945143,-20.2155971437152));
#67774=CARTESIAN_POINT('Ctrl Pts',(-17.1556717596129,-17.5411044966881,
-20.216049077638));
#67775=CARTESIAN_POINT('Ctrl Pts',(-17.1478789038328,-17.5498850477863,
-20.2167543284615));
#67776=CARTESIAN_POINT('Ctrl Pts',(-17.1451136752056,-17.5530194007364,
-20.2170060997183));
#67777=CARTESIAN_POINT('Ctrl Pts',(-17.1400078814819,-17.5588414203773,
-20.21747384555));
#67778=CARTESIAN_POINT('Ctrl Pts',(-17.137664814137,-17.5615268159126,-20.2176896291192));
#67779=CARTESIAN_POINT('Ctrl Pts',(-17.1323895818204,-17.5676036810643,
-20.2181780108206));
#67780=CARTESIAN_POINT('Ctrl Pts',(-17.1294614194031,-17.5709985365596,
-20.218450897087));
#67781=CARTESIAN_POINT('Ctrl Pts',(-17.1208693984005,-17.581024176285,-20.2192568622714));
#67782=CARTESIAN_POINT('Ctrl Pts',(-17.1152357822721,-17.5876805914954,
-20.2197920781554));
#67783=CARTESIAN_POINT('Ctrl Pts',(-17.0754246202606,-17.6353132956759,
-20.2236215820678));
#67784=CARTESIAN_POINT('Ctrl Pts',(-17.0427688019964,-17.6775306336755,
-20.2270129847817));
#67785=CARTESIAN_POINT('Ctrl Pts',(-17.0014775411127,-17.7352967883276,
-20.2316021017822));
#67786=CARTESIAN_POINT('Ctrl Pts',(-16.9913899387585,-17.7497891508251,
-20.2327493452099));
#67787=CARTESIAN_POINT('Ctrl Pts',(-16.9543067499844,-17.8045122534429,
-20.2370618079783));
#67788=CARTESIAN_POINT('Ctrl Pts',(-16.9285139369384,-17.8455389606142,
-20.2402556476629));
#67789=CARTESIAN_POINT('Ctrl Pts',(-16.8491461703863,-17.9819589767084,
-20.2506813367774));
#67790=CARTESIAN_POINT('Ctrl Pts',(-16.8015464442096,-18.0806331045793,
-20.2579141275912));
#67791=CARTESIAN_POINT('Ctrl Pts',(-16.7417568791854,-18.2338826545686,
-20.2684877683439));
#67792=CARTESIAN_POINT('Ctrl Pts',(-16.7237400994398,-18.285981135755,-20.2719769974339));
#67793=CARTESIAN_POINT('Ctrl Pts',(-16.6978381947743,-18.3715597840864,
-20.2775346885533));
#67794=CARTESIAN_POINT('Ctrl Pts',(-16.6886998489945,-18.4046306092406,
-20.2796415923459));
#67795=CARTESIAN_POINT('Ctrl Pts',(-16.6777441326697,-18.448395364119,-20.2823781553355));
#67796=CARTESIAN_POINT('Ctrl Pts',(-16.6751997356609,-18.4589003147906,
-20.2830311571577));
#67797=CARTESIAN_POINT('Ctrl Pts',(-16.6711634649893,-18.4761407653388,
-20.2840966490657));
#67798=CARTESIAN_POINT('Ctrl Pts',(-16.6696238863996,-18.4828647905609,
-20.2845106686239));
#67799=CARTESIAN_POINT('Ctrl Pts',(-16.6667069045328,-18.4958970013511,
-20.2853101715274));
#67800=CARTESIAN_POINT('Ctrl Pts',(-16.6653254436708,-18.5022041914769,
-20.2856957812267));
#67801=CARTESIAN_POINT('Ctrl Pts',(-16.6622017631382,-18.5167844867839,
-20.286584181432));
#67802=CARTESIAN_POINT('Ctrl Pts',(-16.6604801968111,-18.5250619410805,
-20.2870863059102));
#67803=CARTESIAN_POINT('Ctrl Pts',(-16.6559824485151,-18.5473566521787,
-20.2884328726699));
#67804=CARTESIAN_POINT('Ctrl Pts',(-16.6532984925475,-18.5613922235672,
-20.2892743737397));
#67805=CARTESIAN_POINT('Ctrl Pts',(-16.6299804196924,-18.6903996668701,
-20.2969545228158));
#67806=CARTESIAN_POINT('Ctrl Pts',(-16.6187513229764,-18.806874455848,-20.3034766474817));
#67807=CARTESIAN_POINT('Ctrl Pts',(-16.615014097604,-19.086361850776,-20.3187785307505));
#67808=CARTESIAN_POINT('Ctrl Pts',(-16.6315963082219,-19.2487174594628,
-20.3273754006275));
#67809=CARTESIAN_POINT('Ctrl Pts',(-16.6736061947993,-19.439368188625,-20.3385839925853));
#67810=CARTESIAN_POINT('Ctrl Pts',(-16.6813498347196,-19.4710158185405,
-20.3404840399642));
#67811=CARTESIAN_POINT('Ctrl Pts',(-16.6917037687518,-19.5094653211933,
-20.342854886854));
#67812=CARTESIAN_POINT('Ctrl Pts',(-16.693623332179,-19.5164506448447,-20.3432881531509));
#67813=CARTESIAN_POINT('Ctrl Pts',(-16.6966882472585,-19.5273839760889,
-20.3439704835333));
#67814=CARTESIAN_POINT('Ctrl Pts',(-16.697809331024,-19.5313388099488,-20.3442181595012));
#67815=CARTESIAN_POINT('Ctrl Pts',(-16.6999260225975,-19.5387237950756,
-20.3446823072514));
#67816=CARTESIAN_POINT('Ctrl Pts',(-16.7009187949994,-19.5421547004578,
-20.3448986132719));
#67817=CARTESIAN_POINT('Ctrl Pts',(-16.7032043731675,-19.5499791775736,
-20.345393446038));
#67818=CARTESIAN_POINT('Ctrl Pts',(-16.7045027522856,-19.5543710612096,
-20.3456722941024));
#67819=CARTESIAN_POINT('Ctrl Pts',(-16.7085358505881,-19.567852316147,-20.3465315437817));
#67820=CARTESIAN_POINT('Ctrl Pts',(-16.711317413698,-19.5769273903545,-20.3471145792903));
#67821=CARTESIAN_POINT('Ctrl Pts',(-16.7367684491466,-19.6580131647515,
-20.3523635292386));
#67822=CARTESIAN_POINT('Ctrl Pts',(-16.7632115404834,-19.72877460799,-20.3572224496216));
#67823=CARTESIAN_POINT('Ctrl Pts',(-16.8474928283607,-19.9221143500789,
-20.3710143398489));
#67824=CARTESIAN_POINT('Ctrl Pts',(-16.9134063328808,-20.0407945341658,
-20.3800670204478));
#67825=CARTESIAN_POINT('Ctrl Pts',(-17.0412031255139,-20.2264476862477,
-20.394673558666));
#67826=CARTESIAN_POINT('Ctrl Pts',(-17.0968741233894,-20.2972139712001,
-20.400373149202));
#67827=CARTESIAN_POINT('Ctrl Pts',(-17.1707155237133,-20.3796765933551,
-20.4071678726449));
#67828=CARTESIAN_POINT('Ctrl Pts',(-17.1847720441322,-20.3949177376972,
-20.4084309937528));
#67829=CARTESIAN_POINT('Ctrl Pts',(-17.2051779457729,-20.4164013404719,
-20.4102225718888));
#67830=CARTESIAN_POINT('Ctrl Pts',(-17.2113459827121,-20.4228136887047,
-20.4107587695586));
#67831=CARTESIAN_POINT('Ctrl Pts',(-17.2220941535637,-20.43384750951,-20.4116840183791));
#67832=CARTESIAN_POINT('Ctrl Pts',(-17.2266554701769,-20.4384870668149,
-20.4120738816011));
#67833=CARTESIAN_POINT('Ctrl Pts',(-17.2354564878018,-20.4473568838949,
-20.4128208134854));
#67834=CARTESIAN_POINT('Ctrl Pts',(-17.2396928872848,-20.451590318116,-20.4131780218039));
#67835=CARTESIAN_POINT('Ctrl Pts',(-17.250814654177,-20.462610371447,-20.4141097738007));
#67836=CARTESIAN_POINT('Ctrl Pts',(-17.2577286957619,-20.4693679531944,
-20.4146830356762));
#67837=CARTESIAN_POINT('Ctrl Pts',(-17.2817679450944,-20.4925433654805,
-20.4166559486511));
#67838=CARTESIAN_POINT('Ctrl Pts',(-17.2991230571168,-20.508720921618,-20.4180452046877));
#67839=CARTESIAN_POINT('Ctrl Pts',(-17.4372537298969,-20.6332062567327,
-20.4288424935057));
#67840=CARTESIAN_POINT('Ctrl Pts',(-17.5698440812476,-20.7275994337756,
-20.4376243940364));
#67841=CARTESIAN_POINT('Ctrl Pts',(-17.8260924463474,-20.8688692918437,
-20.4535207488873));
#67842=CARTESIAN_POINT('Ctrl Pts',(-17.9458112407303,-20.9211197571371,
-20.4606106172316));
#67843=CARTESIAN_POINT('Ctrl Pts',(-18.0808438911388,-20.965757066104,-20.4690034223024));
#67844=CARTESIAN_POINT('Ctrl Pts',(-18.0921660941425,-20.9693942714539,
-20.469710147926));
#67845=CARTESIAN_POINT('Ctrl Pts',(-18.1083101749773,-20.9744308251401,
-20.4707229111744));
#67846=CARTESIAN_POINT('Ctrl Pts',(-18.1131075513589,-20.975908783926,-20.4710244962193));
#67847=CARTESIAN_POINT('Ctrl Pts',(-18.1213859719733,-20.9784269669529,
-20.4715460767364));
#67848=CARTESIAN_POINT('Ctrl Pts',(-18.1248645571478,-20.9794753295272,
-20.4717655975527));
#67849=CARTESIAN_POINT('Ctrl Pts',(-18.1316161515226,-20.9814911548301,
-20.4721923771178));
#67850=CARTESIAN_POINT('Ctrl Pts',(-18.1348888083142,-20.9824596593024,
-20.4723995676264));
#67851=CARTESIAN_POINT('Ctrl Pts',(-18.1437281282218,-20.9850523218094,
-20.4729600179989));
#67852=CARTESIAN_POINT('Ctrl Pts',(-18.1492990979716,-20.9866615146446,
-20.4733141354594));
#67853=CARTESIAN_POINT('Ctrl Pts',(-18.1700201228114,-20.9925547226728,
-20.4746343977901));
#67854=CARTESIAN_POINT('Ctrl Pts',(-18.1852107811283,-20.9966924555437,
-20.4756084985981));
#67855=CARTESIAN_POINT('Ctrl Pts',(-18.3278347717561,-21.0338375366539,
-20.4848031192346));
#67856=CARTESIAN_POINT('Ctrl Pts',(-18.4580291706067,-21.0550577051422,
-20.4935418434554));
#67857=CARTESIAN_POINT('Ctrl Pts',(-18.748286193705,-21.0749386024076,-20.5127600440346));
#67858=CARTESIAN_POINT('Ctrl Pts',(-18.9079848879175,-21.0678496762759,
-20.5231322867377));
#67859=CARTESIAN_POINT('Ctrl Pts',(-19.0864170712931,-21.0395689391876,
-20.5342281393122));
#67860=CARTESIAN_POINT('Ctrl Pts',(-19.1073845519363,-21.0359207989438,
-20.5355251823464));
#67861=CARTESIAN_POINT('Ctrl Pts',(-19.1371281121068,-21.0302823604703,
-20.5373559650473));
#67862=CARTESIAN_POINT('Ctrl Pts',(-19.1459514913827,-21.0285514241788,
-20.5378979157303));
#67863=CARTESIAN_POINT('Ctrl Pts',(-19.1611568397871,-21.0254677686635,
-20.5388299521332));
#67864=CARTESIAN_POINT('Ctrl Pts',(-19.167544024576,-21.024141677998,-20.5392208822398));
#67865=CARTESIAN_POINT('Ctrl Pts',(-19.179763757998,-21.0215456751046,-20.5399677152005));
#67866=CARTESIAN_POINT('Ctrl Pts',(-19.1855972553064,-21.0202805780194,
-20.5403237679751));
#67867=CARTESIAN_POINT('Ctrl Pts',(-19.2007565735772,-21.0169258186646,
-20.5412478413821));
#67868=CARTESIAN_POINT('Ctrl Pts',(-19.2100738002333,-21.0147976335184,
-20.5418146221666));
#67869=CARTESIAN_POINT('Ctrl Pts',(-19.2418171196734,-21.0073204857516,
-20.5437418553954));
#67870=CARTESIAN_POINT('Ctrl Pts',(-19.2641705933201,-21.0016681998754,
-20.5450925586066));
#67871=CARTESIAN_POINT('Ctrl Pts',(-19.4549978446067,-20.9500848969666,
-20.5565785128637));
#67872=CARTESIAN_POINT('Ctrl Pts',(-19.6172811142733,-20.8838391131288,
-20.5659714918151));
#67873=CARTESIAN_POINT('Ctrl Pts',(-19.8460095525323,-20.7555518136834,
-20.5802387771242));
#67874=CARTESIAN_POINT('Ctrl Pts',(-19.919680919093,-20.7079962178389,-20.5850331460968));
#67875=CARTESIAN_POINT('Ctrl Pts',(-20.0207562854745,-20.6334843026501,
-20.592201479975));
#67876=CARTESIAN_POINT('Ctrl Pts',(-20.0507102079952,-20.6101329930742,
-20.5944071623543));
#67877=CARTESIAN_POINT('Ctrl Pts',(-20.0858688111806,-20.5811707038233,
-20.5971173035553));
#67878=CARTESIAN_POINT('Ctrl Pts',(-20.0916937761353,-20.576319571742,-20.5975704278403));
#67879=CARTESIAN_POINT('Ctrl Pts',(-20.1006932791636,-20.5687424002123,
-20.598277141533));
#67880=CARTESIAN_POINT('Ctrl Pts',(-20.1038860686648,-20.5660380002148,
-20.5985291750483));
#67881=CARTESIAN_POINT('Ctrl Pts',(-20.1097830087991,-20.561012992622,-20.5989971462403));
#67882=CARTESIAN_POINT('Ctrl Pts',(-20.1124893257759,-20.5586950164464,
-20.5992128912466));
#67883=CARTESIAN_POINT('Ctrl Pts',(-20.1185827341293,-20.5534492488169,
-20.599700855679));
#67884=CARTESIAN_POINT('Ctrl Pts',(-20.1219663773731,-20.5505175565551,
-20.5999733611393));
#67885=CARTESIAN_POINT('Ctrl Pts',(-20.1318927170447,-20.5418617939693,
-20.600777268036));
#67886=CARTESIAN_POINT('Ctrl Pts',(-20.1384093920862,-20.5361082115079,
-20.601310790974));
#67887=CARTESIAN_POINT('Ctrl Pts',(-20.184271689178,-20.4951108945783,-20.6051053299702));
#67888=CARTESIAN_POINT('Ctrl Pts',(-20.2223182614543,-20.4584484552833,
-20.6084615483248));
#67889=CARTESIAN_POINT('Ctrl Pts',(-20.2724921822122,-20.4063424455187,
-20.6131349579266));
#67890=CARTESIAN_POINT('Ctrl Pts',(-20.285838299166,-20.392093053928,-20.6144037498945));
#67891=CARTESIAN_POINT('Ctrl Pts',(-20.3975957567918,-20.2694140259198,
-20.6252362741466));
#67892=CARTESIAN_POINT('Ctrl Pts',(-20.4847189654111,-20.1512159401151,
-20.6350415699039));
#67893=CARTESIAN_POINT('Ctrl Pts',(-20.5902290846866,-19.9717611426943,
-20.648490670156));
#67894=CARTESIAN_POINT('Ctrl Pts',(-20.6191743324805,-19.9172036395424,
-20.6524167790985));
#67895=CARTESIAN_POINT('Ctrl Pts',(-20.6616864867386,-19.8278420644759,
-20.6585827761446));
#67896=CARTESIAN_POINT('Ctrl Pts',(-20.6767885703725,-19.7938119504006,
-20.6608724366706));
#67897=CARTESIAN_POINT('Ctrl Pts',(-20.6952311444707,-19.7491105817123,
-20.663807008012));
#67898=CARTESIAN_POINT('Ctrl Pts',(-20.6993949321712,-19.7387881859354,
-20.6644796971704));
#67899=CARTESIAN_POINT('Ctrl Pts',(-20.7060328946612,-19.7219505308917,
-20.6655690589631));
#67900=CARTESIAN_POINT('Ctrl Pts',(-20.7085566075863,-19.7154551479231,
-20.6659873958385));
#67901=CARTESIAN_POINT('Ctrl Pts',(-20.7133473731806,-19.7029422902167,
-20.6667896842573));
#67902=CARTESIAN_POINT('Ctrl Pts',(-20.7156191670391,-19.6969267247085,
-20.6671737914042));
#67903=CARTESIAN_POINT('Ctrl Pts',(-20.7194496029756,-19.6866424461285,
-20.6678277834673));
#67904=CARTESIAN_POINT('Ctrl Pts',(-20.7210219595117,-19.6823789306509,
-20.6680981231762));
#67905=CARTESIAN_POINT('Ctrl Pts',(-20.7225805821175,-19.6781103693139,
-20.6683680078465));
#67906=CARTESIAN_POINT('',(-20.8509992561137,-18.9502252848438,-19.6896814721675));
#67907=CARTESIAN_POINT('Ctrl Pts',(-20.7225807116741,-19.6781100145004,
-20.4442392611068));
#67908=CARTESIAN_POINT('Ctrl Pts',(-20.6728905732413,-19.8141952479699,
-20.4346846178026));
#67909=CARTESIAN_POINT('Ctrl Pts',(-20.6093080329127,-19.9449670995714,
-20.4252946123284));
#67910=CARTESIAN_POINT('Ctrl Pts',(-20.5215596583061,-20.0863590344177,
-20.4150699495229));
#67911=CARTESIAN_POINT('Ctrl Pts',(-20.5100907474605,-20.1042333354495,
-20.4137750968991));
#67912=CARTESIAN_POINT('Ctrl Pts',(-20.4937578065146,-20.1288647531108,
-20.4119869716777));
#67913=CARTESIAN_POINT('Ctrl Pts',(-20.4891202532205,-20.1357698613022,
-20.4114852708096));
#67914=CARTESIAN_POINT('Ctrl Pts',(-20.4810444557183,-20.1476425736561,
-20.4106218506718));
#67915=CARTESIAN_POINT('Ctrl Pts',(-20.4776254479406,-20.1526230851792,
-20.4102594099103));
#67916=CARTESIAN_POINT('Ctrl Pts',(-20.4705005740399,-20.1629073531736,
-20.4095104707037));
#67917=CARTESIAN_POINT('Ctrl Pts',(-20.4667916145951,-20.1682088979423,
-20.4091240952779));
#67918=CARTESIAN_POINT('Ctrl Pts',(-20.4580471986295,-20.1805868654808,
-20.4082212470825));
#67919=CARTESIAN_POINT('Ctrl Pts',(-20.452992360912,-20.187649503576,-20.4077055242836));
#67920=CARTESIAN_POINT('Ctrl Pts',(-20.4364321378702,-20.2104892116244,
-20.4060356905465));
#67921=CARTESIAN_POINT('Ctrl Pts',(-20.424751694462,-20.2261385424026,-20.4048883601294));
#67922=CARTESIAN_POINT('Ctrl Pts',(-20.3638543915206,-20.3054157388934,
-20.3990559106396));
#67923=CARTESIAN_POINT('Ctrl Pts',(-20.3112537829685,-20.3663663031307,
-20.3945074155572));
#67924=CARTESIAN_POINT('Ctrl Pts',(-20.1384828639412,-20.5449025565689,
-20.3807325628625));
#67925=CARTESIAN_POINT('Ctrl Pts',(-20.0077162827823,-20.6512792951468,
-20.371890691937));
#67926=CARTESIAN_POINT('Ctrl Pts',(-19.8645508543518,-20.7418451960285,
-20.3623780550102));
#67927=CARTESIAN_POINT('Ctrl Pts',(-19.8633371225165,-20.7426112709669,
-20.3622974162171));
#67928=CARTESIAN_POINT('Ctrl Pts',(-19.8165508761117,-20.7720750013025,
-20.3591892579398));
#67929=CARTESIAN_POINT('Ctrl Pts',(-19.769904612416,-20.7990219267759,-20.3561000848259));
#67930=CARTESIAN_POINT('Ctrl Pts',(-19.7145581433667,-20.8282385500187,
-20.3523862632687));
#67931=CARTESIAN_POINT('Ctrl Pts',(-19.7068048655429,-20.8322702084328,
-20.3518649282507));
#67932=CARTESIAN_POINT('Ctrl Pts',(-19.6950330482054,-20.8382991851899,
-20.3510714194898));
#67933=CARTESIAN_POINT('Ctrl Pts',(-19.6910326447661,-20.8403319760547,
-20.3508014210781));
#67934=CARTESIAN_POINT('Ctrl Pts',(-19.6838431722597,-20.8439565671958,
-20.3503155183131));
#67935=CARTESIAN_POINT('Ctrl Pts',(-19.6806565215616,-20.8455530449225,
-20.350099911411));
#67936=CARTESIAN_POINT('Ctrl Pts',(-19.6737267196445,-20.8490029357433,
-20.3496305209935));
#67937=CARTESIAN_POINT('Ctrl Pts',(-19.6699821599284,-20.8508532964483,
-20.3493765573496));
#67938=CARTESIAN_POINT('Ctrl Pts',(-19.659456669546,-20.8560157310239,-20.3486618363524));
#67939=CARTESIAN_POINT('Ctrl Pts',(-19.6526635481287,-20.859302606456,-20.3481995577124));
#67940=CARTESIAN_POINT('Ctrl Pts',(-19.6121125286872,-20.8786564651601,
-20.3454347298672));
#67941=CARTESIAN_POINT('Ctrl Pts',(-19.5779535986707,-20.8938621666274,
-20.3430840466224));
#67942=CARTESIAN_POINT('Ctrl Pts',(-19.4646015911746,-20.94076467045,-20.3352549237691));
#67943=CARTESIAN_POINT('Ctrl Pts',(-19.383896804573,-20.9685802419175,-20.3296386863144));
#67944=CARTESIAN_POINT('Ctrl Pts',(-19.1303458250446,-21.0391635321525,
-20.3122516409712));
#67945=CARTESIAN_POINT('Ctrl Pts',(-18.9535833238402,-21.0650899657821,
-20.3005607163423));
#67946=CARTESIAN_POINT('Ctrl Pts',(-18.7528410334991,-21.0690389430811,
-20.2882045749222));
#67947=CARTESIAN_POINT('Ctrl Pts',(-18.7300383420336,-21.0691190897398,
-20.2868128418573));
#67948=CARTESIAN_POINT('Ctrl Pts',(-18.6977240144483,-21.0687105576463,
-20.2848566525503));
#67949=CARTESIAN_POINT('Ctrl Pts',(-18.688210745538,-21.0685261351512,-20.2842827259889));
#67950=CARTESIAN_POINT('Ctrl Pts',(-18.6727398202443,-21.0681218597937,
-20.2833525042173));
#67951=CARTESIAN_POINT('Ctrl Pts',(-18.666781357925,-21.0679409704449,-20.2829949931335));
#67952=CARTESIAN_POINT('Ctrl Pts',(-18.6542980888031,-21.0675092152436,
-20.2822475400265));
#67953=CARTESIAN_POINT('Ctrl Pts',(-18.6477735098318,-21.0672533248515,
-20.2818577594565));
#67954=CARTESIAN_POINT('Ctrl Pts',(-18.6322316958416,-21.0665717536709,
-20.2809313521401));
#67955=CARTESIAN_POINT('Ctrl Pts',(-18.6232157471918,-21.0661185733841,
-20.2803955927166));
#67956=CARTESIAN_POINT('Ctrl Pts',(-18.5927428468242,-21.0643914004119,
-20.2785901865145));
#67957=CARTESIAN_POINT('Ctrl Pts',(-18.5713020456533,-21.0628482744101,
-20.2773289740498));
#67958=CARTESIAN_POINT('Ctrl Pts',(-18.3711083179642,-21.045371525015,-20.2656286284256));
#67959=CARTESIAN_POINT('Ctrl Pts',(-18.1950414036618,-21.0070974021979,
-20.255986337114));
#67960=CARTESIAN_POINT('Ctrl Pts',(-17.912350610632,-20.9067631532775,-20.2396611387924));
#67961=CARTESIAN_POINT('Ctrl Pts',(-17.8024648994558,-20.8568466047916,
-20.2330507520611));
#67962=CARTESIAN_POINT('Ctrl Pts',(-17.689157601094,-20.7932179504519,-20.2253490632511));
#67963=CARTESIAN_POINT('Ctrl Pts',(-17.6809090873663,-20.7885126467702,
-20.2247830198669));
#67964=CARTESIAN_POINT('Ctrl Pts',(-17.6687291735151,-20.7814556702144,
-20.223938765414));
#67965=CARTESIAN_POINT('Ctrl Pts',(-17.6647731694154,-20.7791463999616,
-20.2236632262537));
#67966=CARTESIAN_POINT('Ctrl Pts',(-17.6577458576165,-20.7750136530059,
-20.2231713438855));
#67967=CARTESIAN_POINT('Ctrl Pts',(-17.6546716392989,-20.77319522501,-20.2229553296198));
#67968=CARTESIAN_POINT('Ctrl Pts',(-17.6480696495257,-20.7692675003106,
-20.2224896238912));
#67969=CARTESIAN_POINT('Ctrl Pts',(-17.6445434662935,-20.7671557382954,
-20.2222397767971));
#67970=CARTESIAN_POINT('Ctrl Pts',(-17.6348213755042,-20.7612948342117,
-20.2215478992606));
#67971=CARTESIAN_POINT('Ctrl Pts',(-17.6286385898594,-20.7575241884657,
-20.2211044970959));
#67972=CARTESIAN_POINT('Ctrl Pts',(-17.594779280346,-20.7366355845876,-20.21865804214));
#67973=CARTESIAN_POINT('Ctrl Pts',(-17.5674825584837,-20.7189139218477,
-20.2166186347703));
#67974=CARTESIAN_POINT('Ctrl Pts',(-17.406223797779,-20.6088554531445,-20.2042125252644));
#67975=CARTESIAN_POINT('Ctrl Pts',(-17.2828649139191,-20.5019569440862,
-20.1932560141197));
#67976=CARTESIAN_POINT('Ctrl Pts',(-17.0940643354825,-20.2958542810069,
-20.1749988331776));
#67977=CARTESIAN_POINT('Ctrl Pts',(-17.0224166834121,-20.2033287611289,
-20.1675581752485));
#67978=CARTESIAN_POINT('Ctrl Pts',(-16.9509757412983,-20.0933665829838,
-20.1595512894083));
#67979=CARTESIAN_POINT('Ctrl Pts',(-16.943312257787,-20.0813053659112,-20.158683316669));
#67980=CARTESIAN_POINT('Ctrl Pts',(-16.9313097914056,-20.061985806313,-20.1573090128665));
#67981=CARTESIAN_POINT('Ctrl Pts',(-16.9268912628633,-20.0547776266239,
-20.1567997537533));
#67982=CARTESIAN_POINT('Ctrl Pts',(-16.9191746526594,-20.0420181868551,
-20.1559043780002));
#67983=CARTESIAN_POINT('Ctrl Pts',(-16.9158585869085,-20.0364779815466,
-20.1555176052367));
#67984=CARTESIAN_POINT('Ctrl Pts',(-16.9090523224986,-20.024987678131,-20.1547195381088));
#67985=CARTESIAN_POINT('Ctrl Pts',(-16.9055657515437,-20.0190355119874,
-20.1543083791258));
#67986=CARTESIAN_POINT('Ctrl Pts',(-16.8966908804898,-20.0037133763836,
-20.1532556708245));
#67987=CARTESIAN_POINT('Ctrl Pts',(-16.8913450922958,-19.9943189168253,
-20.1526156628088));
#67988=CARTESIAN_POINT('Ctrl Pts',(-16.869333938067,-19.9549388419176,-20.149954997782));
#67989=CARTESIAN_POINT('Ctrl Pts',(-16.8533261621608,-19.9245903327816,
-20.1479578695779));
#67990=CARTESIAN_POINT('Ctrl Pts',(-16.8135457967482,-19.8445139893793,
-20.1428137897843));
#67991=CARTESIAN_POINT('Ctrl Pts',(-16.7909643571484,-19.7942224789403,
-20.1397062273577));
#67992=CARTESIAN_POINT('Ctrl Pts',(-16.7295080994084,-19.6416795364478,
-20.1305618125667));
#67993=CARTESIAN_POINT('Ctrl Pts',(-16.6965647880973,-19.5372386551154,
-20.1246736897909));
#67994=CARTESIAN_POINT('Ctrl Pts',(-16.661495369825,-19.3861717633026,-20.1162302648609));
#67995=CARTESIAN_POINT('Ctrl Pts',(-16.6526001440765,-19.3413006095121,
-20.1137296440771));
#67996=CARTESIAN_POINT('Ctrl Pts',(-16.6414616925536,-19.2737007555004,
-20.1099306389502));
#67997=CARTESIAN_POINT('Ctrl Pts',(-16.6381212428452,-19.2511657195745,
-20.1086589341801));
#67998=CARTESIAN_POINT('Ctrl Pts',(-16.635014330211,-19.227588753746,-20.10731904276));
#67999=CARTESIAN_POINT('Ctrl Pts',(-16.6348841801674,-19.226595662919,-20.1072625875172));
#68000=CARTESIAN_POINT('Ctrl Pts',(-16.6324561181456,-19.2079660888138,
-20.1062032014243));
#68001=CARTESIAN_POINT('Ctrl Pts',(-16.6303799032461,-19.1903018723446,
-20.1051931370714));
#68002=CARTESIAN_POINT('Ctrl Pts',(-16.6249807896789,-19.1387743742033,
-20.1022251976505));
#68003=CARTESIAN_POINT('Ctrl Pts',(-16.6222515859022,-19.1048562620928,
-20.1002445439356));
#68004=CARTESIAN_POINT('Ctrl Pts',(-16.6199499410138,-19.0639367655804,
-20.0978069261055));
#68005=CARTESIAN_POINT('Ctrl Pts',(-16.6195931839441,-19.0569824012193,
-20.0973909755966));
#68006=CARTESIAN_POINT('Ctrl Pts',(-16.6190643340273,-19.0455735042,-20.0967056680271));
#68007=CARTESIAN_POINT('Ctrl Pts',(-16.6188719863389,-19.0411199017147,
-20.0964374191126));
#68008=CARTESIAN_POINT('Ctrl Pts',(-16.6185512358395,-19.0331062081705,
-20.0959533717234));
#68009=CARTESIAN_POINT('Ctrl Pts',(-16.6184177515004,-19.0295463752165,
-20.0957378607301));
#68010=CARTESIAN_POINT('Ctrl Pts',(-16.6181464746308,-19.0217889496004,
-20.0952671550356));
#68011=CARTESIAN_POINT('Ctrl Pts',(-16.6180121893519,-19.0175913316322,
-20.0950117718546));
#68012=CARTESIAN_POINT('Ctrl Pts',(-16.6176684706817,-19.0057440228531,
-20.0942891163123));
#68013=CARTESIAN_POINT('Ctrl Pts',(-16.6174880266073,-18.9980936477288,
-20.0938202690771));
#68014=CARTESIAN_POINT('Ctrl Pts',(-16.6166359125984,-18.9511762171222,
-20.0909322144367));
#68015=CARTESIAN_POINT('Ctrl Pts',(-16.6170156060812,-18.9119003966035,
-20.0884598542696));
#68016=CARTESIAN_POINT('Ctrl Pts',(-16.6246864730281,-18.7073629006315,
-20.0753759115104));
#68017=CARTESIAN_POINT('Ctrl Pts',(-16.650236814253,-18.5433629186059,-20.0642279664343));
#68018=CARTESIAN_POINT('Ctrl Pts',(-16.7233108427889,-18.2809906220141,
-20.0465068286882));
#68019=CARTESIAN_POINT('Ctrl Pts',(-16.7597694081222,-18.1802849572855,
-20.0397217322053));
#68020=CARTESIAN_POINT('Ctrl Pts',(-16.809486709708,-18.0698793026648,-20.0323300216615));
#68021=CARTESIAN_POINT('Ctrl Pts',(-16.8154125130484,-18.0570640250555,
-20.0314725683119));
#68022=CARTESIAN_POINT('Ctrl Pts',(-16.8250698839282,-18.0367156432777,
-20.030111726026));
#68023=CARTESIAN_POINT('Ctrl Pts',(-16.8287188044834,-18.0291439923261,
-20.0296054976374));
#68024=CARTESIAN_POINT('Ctrl Pts',(-16.8352469108427,-18.0158016813022,
-20.0287136402764));
#68025=CARTESIAN_POINT('Ctrl Pts',(-16.8381075357463,-18.0100221069842,
-20.028327371423));
#68026=CARTESIAN_POINT('Ctrl Pts',(-16.8440919083803,-17.9980690418548,
-20.0275285986674));
#68027=CARTESIAN_POINT('Ctrl Pts',(-16.8472196044384,-17.991897605279,-20.0271162387682));
#68028=CARTESIAN_POINT('Ctrl Pts',(-16.8553536454317,-17.9760411204043,
-20.0260568146678));
#68029=CARTESIAN_POINT('Ctrl Pts',(-16.8604046918547,-17.9663791356616,
-20.0254113305305));
#68030=CARTESIAN_POINT('Ctrl Pts',(-16.8820452178162,-17.925751221827,-20.0226969196544));
#68031=CARTESIAN_POINT('Ctrl Pts',(-16.8993300412366,-17.8951606446635,
-20.0206527521062));
#68032=CARTESIAN_POINT('Ctrl Pts',(-16.9466054074943,-17.8161515111259,
-20.0153593944998));
#68033=CARTESIAN_POINT('Ctrl Pts',(-16.9778026004702,-17.7684871719808,
-20.0121526604569));
#68034=CARTESIAN_POINT('Ctrl Pts',(-17.0973195531202,-17.6010366452894,
-20.000730128435));
#68035=CARTESIAN_POINT('Ctrl Pts',(-17.1962736690529,-17.4893926877315,
-19.9928376963955));
#68036=CARTESIAN_POINT('Ctrl Pts',(-17.3623928375813,-17.3376288201956,
-19.9803866816486));
#68037=CARTESIAN_POINT('Ctrl Pts',(-17.4214050181273,-17.2892936837539,
-19.9760811738258));
#68038=CARTESIAN_POINT('Ctrl Pts',(-17.4905593141391,-17.2386305962504,
-19.9710006087807));
#68039=CARTESIAN_POINT('Ctrl Pts',(-17.4982690461535,-17.2330618233827,
-19.9704337192039));
#68040=CARTESIAN_POINT('Ctrl Pts',(-17.5097495285106,-17.2248865723154,
-19.96958844097));
#68041=CARTESIAN_POINT('Ctrl Pts',(-17.5134917659741,-17.2222399996534,
-19.9693127336125));
#68042=CARTESIAN_POINT('Ctrl Pts',(-17.5201656867192,-17.2175525317936,
-19.9688206664646));
#68043=CARTESIAN_POINT('Ctrl Pts',(-17.523093969727,-17.2155068829146,-19.9686046365648));
#68044=CARTESIAN_POINT('Ctrl Pts',(-17.529401333355,-17.2111243781189,-19.9681390290221));
#68045=CARTESIAN_POINT('Ctrl Pts',(-17.5327819934348,-17.2087899786362,
-19.9678892964436));
#68046=CARTESIAN_POINT('Ctrl Pts',(-17.542133631928,-17.2023726442709,-19.9671980531526));
#68047=CARTESIAN_POINT('Ctrl Pts',(-17.5481187090696,-17.1983104939588,
-19.9667551747801));
#68048=CARTESIAN_POINT('Ctrl Pts',(-17.5810413238428,-17.1762110857246,
-19.9643168956794));
#68049=CARTESIAN_POINT('Ctrl Pts',(-17.608368080391,-17.1587647973197,-19.9622854205056));
#68050=CARTESIAN_POINT('Ctrl Pts',(-17.7752802366651,-17.05752111551,-19.9498819441189));
#68051=CARTESIAN_POINT('Ctrl Pts',(-17.9237483133758,-16.9894287408592,
-19.9389181278655));
#68052=CARTESIAN_POINT('Ctrl Pts',(-18.1896523479148,-16.902847314526,-19.9206516930896));
#68053=CARTESIAN_POINT('Ctrl Pts',(-18.3035711042056,-16.8759268142901,
-19.9132088157146));
#68054=CARTESIAN_POINT('Ctrl Pts',(-18.4332776908568,-16.8564191044806,
-19.9051998623574));
#68055=CARTESIAN_POINT('Ctrl Pts',(-18.4474299329633,-16.8544369355657,
-19.904331861564));
#68056=CARTESIAN_POINT('Ctrl Pts',(-18.4699857848919,-16.8515103011535,
-19.9029575213937));
#68057=CARTESIAN_POINT('Ctrl Pts',(-18.4783766664683,-16.8504726517761,
-19.9024482537379));
#68058=CARTESIAN_POINT('Ctrl Pts',(-18.4931861919352,-16.8487312584256,
-19.9015528674848));
#68059=CARTESIAN_POINT('Ctrl Pts',(-18.499602218835,-16.8480065658238,-19.9011660927221));
#68060=CARTESIAN_POINT('Ctrl Pts',(-18.5128794096425,-16.8465683893715,
-19.900368025793));
#68061=CARTESIAN_POINT('Ctrl Pts',(-18.5197409539613,-16.8458590632543,
-19.8999568689869));
#68062=CARTESIAN_POINT('Ctrl Pts',(-18.5373623443071,-16.8441244214811,
-19.8989041752007));
#68063=CARTESIAN_POINT('Ctrl Pts',(-18.5481268813494,-16.8431479396425,
-19.8982641794315));
#68064=CARTESIAN_POINT('Ctrl Pts',(-18.5930842496861,-16.8394166379384,
-19.8956036398859));
#68065=CARTESIAN_POINT('Ctrl Pts',(-18.6273351421491,-16.8374105563929,
-19.8936066220194));
#68066=CARTESIAN_POINT('Ctrl Pts',(-18.7166896998723,-16.8343537957907,
-19.8884628926149));
#68067=CARTESIAN_POINT('Ctrl Pts',(-18.7718132900223,-16.8346205127423,
-19.8853555631007));
#68068=CARTESIAN_POINT('Ctrl Pts',(-19.0100756690398,-16.8450824855816,
-19.872094512402));
#68069=CARTESIAN_POINT('Ctrl Pts',(-19.1914406303232,-16.8768962206083,
-19.8625018406128));
#68070=CARTESIAN_POINT('Ctrl Pts',(-19.4105435273638,-16.9454817878797,
-19.8495094779168));
#68071=CARTESIAN_POINT('Ctrl Pts',(-19.4541974694506,-16.9607337207652,
-19.8468428909266));
#68072=CARTESIAN_POINT('Ctrl Pts',(-19.5044480534193,-16.980158904741,-19.8436436569624));
#68073=CARTESIAN_POINT('Ctrl Pts',(-19.5115674651876,-16.9829554750961,
-19.843187308468));
#68074=CARTESIAN_POINT('Ctrl Pts',(-19.5229582137532,-16.9875012751231,
-19.8424519725694));
#68075=CARTESIAN_POINT('Ctrl Pts',(-19.5272393316553,-16.9892260280709,
-19.842174419653));
#68076=CARTESIAN_POINT('Ctrl Pts',(-19.5348348349426,-16.992314970882,-19.8416798264017));
#68077=CARTESIAN_POINT('Ctrl Pts',(-19.5381514343886,-16.9936735929365,
-19.8414631240229));
#68078=CARTESIAN_POINT('Ctrl Pts',(-19.5451998894675,-16.9965818690275,
-19.8410009980104));
#68079=CARTESIAN_POINT('Ctrl Pts',(-19.5489307051641,-16.9981337628289,
-19.8407554449695));
#68080=CARTESIAN_POINT('Ctrl Pts',(-19.558917228362,-17.0023213988837,-19.8400956656079));
#68081=CARTESIAN_POINT('Ctrl Pts',(-19.5651646779393,-17.0049765392887,
-19.8396802888679));
#68082=CARTESIAN_POINT('Ctrl Pts',(-19.5960844743466,-17.0182932601736,
-19.8376118515134));
#68083=CARTESIAN_POINT('Ctrl Pts',(-19.6205637811342,-17.0293934615107,
-19.8359341776948));
#68084=CARTESIAN_POINT('Ctrl Pts',(-19.6907536179436,-17.0628466800175,
-19.8310206464795));
#68085=CARTESIAN_POINT('Ctrl Pts',(-19.7358764250408,-17.086384635568,-19.82773328606));
#68086=CARTESIAN_POINT('Ctrl Pts',(-19.8667078395912,-17.1607476024165,
-19.8179014967938));
#68087=CARTESIAN_POINT('Ctrl Pts',(-19.9497283289733,-17.2160227873667,
-19.8112717116829));
#68088=CARTESIAN_POINT('Ctrl Pts',(-20.0405380766754,-17.2862038346826,
-19.803731910975));
#68089=CARTESIAN_POINT('Ctrl Pts',(-20.0524279870393,-17.2955983994748,
-19.802738437101));
#68090=CARTESIAN_POINT('Ctrl Pts',(-20.1576039360046,-17.3805509977562,
-19.7938970945792));
#68091=CARTESIAN_POINT('Ctrl Pts',(-20.2444184714402,-17.4637981947573,
-19.7862404440536));
#68092=CARTESIAN_POINT('Ctrl Pts',(-20.334095497553,-17.5657711831682,-19.7779483908196));
#68093=CARTESIAN_POINT('Ctrl Pts',(-20.3443413328403,-17.5776868091483,
-19.7769943256731));
#68094=CARTESIAN_POINT('Ctrl Pts',(-20.3596415887045,-17.5958866494414,
-19.7755590871145));
#68095=CARTESIAN_POINT('Ctrl Pts',(-20.3647941742819,-17.6020872774793,
-19.7750738944653));
#68096=CARTESIAN_POINT('Ctrl Pts',(-20.3739636688635,-17.6132509837842,
-19.7742070446102));
#68097=CARTESIAN_POINT('Ctrl Pts',(-20.377993761708,-17.6182030602599,-19.7738248544275));
#68098=CARTESIAN_POINT('Ctrl Pts',(-20.3864973809088,-17.6287491886064,
-19.7730158217329));
#68099=CARTESIAN_POINT('Ctrl Pts',(-20.3909650520357,-17.6343478751839,
-19.772589217814));
#68100=CARTESIAN_POINT('Ctrl Pts',(-20.4028443464048,-17.6493904413009,
-19.771450648905));
#68101=CARTESIAN_POINT('Ctrl Pts',(-20.4102042683554,-17.6588749578475,
-19.770740747503));
#68102=CARTESIAN_POINT('Ctrl Pts',(-20.4456332339009,-17.7053419868914,
-19.76730060182));
#68103=CARTESIAN_POINT('Ctrl Pts',(-20.4725624463873,-17.743180071677,-19.7646151981559));
#68104=CARTESIAN_POINT('Ctrl Pts',(-20.5482263636716,-17.857260510455,-19.7568168015629));
#68105=CARTESIAN_POINT('Ctrl Pts',(-20.5933452475915,-17.9357770445965,
-19.7518286380275));
#68106=CARTESIAN_POINT('Ctrl Pts',(-20.6664468123528,-18.0842624367219,
-19.7428027245657));
#68107=CARTESIAN_POINT('Ctrl Pts',(-20.6959858739097,-18.1532945405059,
-19.7387530398212));
#68108=CARTESIAN_POINT('Ctrl Pts',(-20.7571087062752,-18.3201322190897,
-19.7290386426034));
#68109=CARTESIAN_POINT('Ctrl Pts',(-20.785358515489,-18.4189443609152,-19.7233418224833));
#68110=CARTESIAN_POINT('Ctrl Pts',(-20.8083088064251,-18.5288855092317,
-19.716687994081));
#68111=CARTESIAN_POINT('Ctrl Pts',(-20.8102237312023,-18.5383843491317,
-19.7161105530016));
#68112=CARTESIAN_POINT('Ctrl Pts',(-20.8129549517807,-18.5524294310593,
-19.7152525289895));
#68113=CARTESIAN_POINT('Ctrl Pts',(-20.8138217188903,-18.5569658903304,
-19.7149747460142));
#68114=CARTESIAN_POINT('Ctrl Pts',(-20.8153331726451,-18.5650193680193,
-19.7144803978423));
#68115=CARTESIAN_POINT('Ctrl Pts',(-20.8159838012209,-18.5685352215321,
-19.7142641742975));
#68116=CARTESIAN_POINT('Ctrl Pts',(-20.8173588170755,-18.5760721708738,
-19.7137997612742));
#68117=CARTESIAN_POINT('Ctrl Pts',(-20.8180804607375,-18.5800936597507,
-19.7135514253113));
#68118=CARTESIAN_POINT('Ctrl Pts',(-20.819537503568,-18.5883507154137,-19.7130404633478));
#68119=CARTESIAN_POINT('Ctrl Pts',(-20.8202716512641,-18.5925864813869,
-19.7127777691835));
#68120=CARTESIAN_POINT('Ctrl Pts',(-20.8220969243962,-18.6033116893226,
-19.7121112034224));
#68121=CARTESIAN_POINT('Ctrl Pts',(-20.8231706938927,-18.6098039846676,
-19.7117064072045));
#68122=CARTESIAN_POINT('Ctrl Pts',(-20.8419516469325,-18.7267427419427,
-19.704393091252));
#68123=CARTESIAN_POINT('Ctrl Pts',(-20.8509055118865,-18.8384008838167,
-19.6970632585576));
#68124=CARTESIAN_POINT('Ctrl Pts',(-20.8509992561137,-18.9502252848438,
-19.6896814721675));
#68125=CARTESIAN_POINT('Ctrl Pts',(-20.8509992546728,-18.9502235668445,
-19.6896815855766));
#68126=CARTESIAN_POINT('Ctrl Pts',(-20.8510836457028,-19.0507934909693,
-19.6830427336087));
#68127=CARTESIAN_POINT('Ctrl Pts',(-20.844001378845,-19.1512504950245,-19.6763789318511));
#68128=CARTESIAN_POINT('Ctrl Pts',(-20.8172660724819,-19.3387551736086,
-19.6641118465099));
#68129=CARTESIAN_POINT('Ctrl Pts',(-20.7992074267082,-19.4258130985577,
-19.658486560603));
#68130=CARTESIAN_POINT('Ctrl Pts',(-20.7702875631048,-19.5313496542403,
-19.6517704142229));
#68131=CARTESIAN_POINT('Ctrl Pts',(-20.7645555899519,-19.5511302902294,
-19.6505158868579));
#68132=CARTESIAN_POINT('Ctrl Pts',(-20.755942028075,-19.5793102638725,-19.6487342543039));
#68133=CARTESIAN_POINT('Ctrl Pts',(-20.7532949575033,-19.5877795297144,
-19.648199525735));
#68134=CARTESIAN_POINT('Ctrl Pts',(-20.7486160613219,-19.6024255533593,
-19.6472760010289));
#68135=CARTESIAN_POINT('Ctrl Pts',(-20.7466088978239,-19.6086100066726,
-19.646886401071));
#68136=CARTESIAN_POINT('Ctrl Pts',(-20.7426965192785,-19.6204782922701,
-19.6461394126603));
#68137=CARTESIAN_POINT('Ctrl Pts',(-20.7407955948982,-19.6261634632885,
-19.6457818872301));
#68138=CARTESIAN_POINT('Ctrl Pts',(-20.7357563731666,-19.6410242824532,
-19.644848069307));
#68139=CARTESIAN_POINT('Ctrl Pts',(-20.7325791090231,-19.6501866434224,
-19.6442730699062));
#68140=CARTESIAN_POINT('Ctrl Pts',(-20.727115684882,-19.6655987280105,-19.6433069814357));
#68141=CARTESIAN_POINT('Ctrl Pts',(-20.7248628673184,-19.671859931052,-19.6429148193411));
#68142=CARTESIAN_POINT('Ctrl Pts',(-20.7225805821918,-19.6781103691105,
-19.6425236185391));
#68143=CARTESIAN_POINT('Origin',(-18.734,-18.952,0.));
#68144=CARTESIAN_POINT('',(-20.7225806288389,-19.6781102413592,-18.845275429269));
#68145=CARTESIAN_POINT('',(-20.7225805821191,-19.6781103693095,-19.0663245248053));
#68146=CARTESIAN_POINT('',(-20.7225805821191,-19.6781103693095,0.));
#68147=CARTESIAN_POINT('',(-20.8499619975019,-18.9538841873159,-19.1109437209775));
#68148=CARTESIAN_POINT('Ctrl Pts',(-20.7225805821191,-19.6781103693095,
-19.0663245248053));
#68149=CARTESIAN_POINT('Ctrl Pts',(-20.7389260930203,-19.6333453212442,
-19.0692018319792));
#68150=CARTESIAN_POINT('Ctrl Pts',(-20.7537412767065,-19.5880774322525,
-19.0720791391531));
#68151=CARTESIAN_POINT('Ctrl Pts',(-20.7670007520339,-19.5424209872875,
-19.074956446327));
#68152=CARTESIAN_POINT('Ctrl Pts',(-20.7921933233411,-19.4556752287257,
-19.0804232362535));
#68153=CARTESIAN_POINT('Ctrl Pts',(-20.8118478930247,-19.3672535084955,
-19.0858900261801));
#68154=CARTESIAN_POINT('Ctrl Pts',(-20.8257819138129,-19.2777873923974,
-19.0913568161066));
#68155=CARTESIAN_POINT('Ctrl Pts',(-20.839488073104,-19.1897843057774,-19.0967342082235));
#68156=CARTESIAN_POINT('Ctrl Pts',(-20.8476592207516,-19.1007706087727,
-19.1021116003405));
#68157=CARTESIAN_POINT('Ctrl Pts',(-20.8501673751619,-19.0113686811404,
-19.1074889924574));
#68158=CARTESIAN_POINT('Ctrl Pts',(-20.8507044999978,-18.9922231311271,
-19.1086405686307));
#68159=CARTESIAN_POINT('Ctrl Pts',(-20.8509820862726,-18.9730598582293,
-19.1097921448041));
#68160=CARTESIAN_POINT('Ctrl Pts',(-20.8509991606888,-18.9538851108721,
-19.1109437209775));
#68161=CARTESIAN_POINT('Ctrl Pts',(-20.8499619975019,-18.9538841873159,
-19.1109437209775));
#68162=CARTESIAN_POINT('Ctrl Pts',(-20.8456331448199,-18.4480050364302,
-19.1413398983212));
#68163=CARTESIAN_POINT('Ctrl Pts',(-20.4101935050426,-17.2299119675837,
-19.2141280112252));
#68164=CARTESIAN_POINT('Ctrl Pts',(-18.3741968410994,-16.4747290082863,
-19.3293080596899));
#68165=CARTESIAN_POINT('Ctrl Pts',(-16.456252502104,-17.9136376975396,-19.4564838663714));
#68166=CARTESIAN_POINT('Ctrl Pts',(-16.6280001175491,-20.3051793956671,
-19.5836596730528));
#68167=CARTESIAN_POINT('Ctrl Pts',(-18.7318719157577,-21.4552629005109,
-19.7108354797342));
#68168=CARTESIAN_POINT('Ctrl Pts',(-20.2929104233135,-20.6053638626281,
-19.8051103644544));
#68169=CARTESIAN_POINT('Ctrl Pts',(-20.6701804022281,-19.8268832656859,
-19.8569933136142));
#68170=CARTESIAN_POINT('Ctrl Pts',(-20.7227693935251,-19.6781792853784,
-19.8664843272136));
#68171=CARTESIAN_POINT('Ctrl Pts',(-20.7225805821918,-19.6781103691105,
-19.6425236185391));
#68172=CARTESIAN_POINT('Ctrl Pts',(-20.7166653576808,-19.6943102487738,
-19.641509704657));
#68173=CARTESIAN_POINT('Ctrl Pts',(-20.710552187151,-19.7104378159453,-19.6405022550434));
#68174=CARTESIAN_POINT('Ctrl Pts',(-20.6468793838964,-19.8724165912212,
-19.630397967332));
#68175=CARTESIAN_POINT('Ctrl Pts',(-20.5734821739296,-20.0115218277049,
-19.6218861304148));
#68176=CARTESIAN_POINT('Ctrl Pts',(-20.4399820734497,-20.2081237322731,
-19.6089797865278));
#68177=CARTESIAN_POINT('Ctrl Pts',(-20.3907876123171,-20.2723314550053,
-19.6045896005813));
#68178=CARTESIAN_POINT('Ctrl Pts',(-20.3116702093477,-20.3641895034725,
-19.597801964565));
#68179=CARTESIAN_POINT('Ctrl Pts',(-20.2844242310254,-20.3940495134181,
-19.5955064655122));
#68180=CARTESIAN_POINT('Ctrl Pts',(-20.2404516176395,-20.4395535058783,
-19.5918318001489));
#68181=CARTESIAN_POINT('Ctrl Pts',(-20.2242964647885,-20.4557380955299,
-19.5904877078463));
#68182=CARTESIAN_POINT('Ctrl Pts',(-20.2032487008755,-20.476151874231,-19.5887389696148));
#68183=CARTESIAN_POINT('Ctrl Pts',(-20.1985938433898,-20.4806253799376,
-19.5883523717303));
#68184=CARTESIAN_POINT('Ctrl Pts',(-20.1914747000028,-20.4874047962422,
-19.5877611959693));
#68185=CARTESIAN_POINT('Ctrl Pts',(-20.1890251926361,-20.4897262688464,
-19.5875578037743));
#68186=CARTESIAN_POINT('Ctrl Pts',(-20.1839774699174,-20.4944872897189,
-19.587138677327));
#68187=CARTESIAN_POINT('Ctrl Pts',(-20.1813786655035,-20.4969261148266,
-19.5869228906763));
#68188=CARTESIAN_POINT('Ctrl Pts',(-20.1754965377455,-20.5024182773035,
-19.5864344824733));
#68189=CARTESIAN_POINT('Ctrl Pts',(-20.1722096841926,-20.5054677358632,
-19.5861615726575));
#68190=CARTESIAN_POINT('Ctrl Pts',(-20.1625003659489,-20.514418567213,-19.5853554863338));
#68191=CARTESIAN_POINT('Ctrl Pts',(-20.1560511801885,-20.5202906330141,
-19.5848201719844));
#68192=CARTESIAN_POINT('Ctrl Pts',(-20.1098730376359,-20.5618173928256,
-19.5809891224532));
#68193=CARTESIAN_POINT('Ctrl Pts',(-20.0688475906991,-20.5959949895138,
-19.5775961909825));
#68194=CARTESIAN_POINT('Ctrl Pts',(-20.0127922062523,-20.6392114662941,
-19.5730216044894));
#68195=CARTESIAN_POINT('Ctrl Pts',(-19.9988754170776,-20.6496696364701,
-19.5718906194675));
#68196=CARTESIAN_POINT('Ctrl Pts',(-19.8572280126433,-20.7534060115647,
-19.5604380159078));
#68197=CARTESIAN_POINT('Ctrl Pts',(-19.7195362708858,-20.8322741708811,
-19.549832160147));
#68198=CARTESIAN_POINT('Ctrl Pts',(-19.5237780860885,-20.9169363262836,
-19.5361230744716));
#68199=CARTESIAN_POINT('Ctrl Pts',(-19.4723744528574,-20.9368244707487,
-19.5326344323805));
#68200=CARTESIAN_POINT('Ctrl Pts',(-19.3878021241933,-20.965804423035,-19.5270775586395));
#68201=CARTESIAN_POINT('Ctrl Pts',(-19.3550877111118,-20.9761333313784,
-19.5249709002405));
#68202=CARTESIAN_POINT('Ctrl Pts',(-19.3117525959949,-20.9886658419112,
-19.522234597395));
#68203=CARTESIAN_POINT('Ctrl Pts',(-19.3013470283985,-20.9915889708319,
-19.5215816164418));
#68204=CARTESIAN_POINT('Ctrl Pts',(-19.2842644208192,-20.9962469636859,
-19.5205161453214));
#68205=CARTESIAN_POINT('Ctrl Pts',(-19.2776005744641,-20.9980290805736,
-19.520102125869));
#68206=CARTESIAN_POINT('Ctrl Pts',(-19.2646824261088,-21.0014162223706,
-19.5193026139653));
#68207=CARTESIAN_POINT('Ctrl Pts',(-19.2584292655106,-21.0030252647879,
-19.5189169952063));
#68208=CARTESIAN_POINT('Ctrl Pts',(-19.2439711248367,-21.0066751412676,
-19.5180285609203));
#68209=CARTESIAN_POINT('Ctrl Pts',(-19.2357610495381,-21.0086954895269,
-19.5175264115259));
#68210=CARTESIAN_POINT('Ctrl Pts',(-19.213642289766,-21.0139981793584,-19.516179748457));
#68211=CARTESIAN_POINT('Ctrl Pts',(-19.1997119578373,-21.0171889998374,
-19.5153381765576));
#68212=CARTESIAN_POINT('Ctrl Pts',(-19.0715533720643,-21.0451817361065,
-19.507653217771));
#68213=CARTESIAN_POINT('Ctrl Pts',(-18.9554801047576,-21.0606260671115,
-19.5011268231189));
#68214=CARTESIAN_POINT('Ctrl Pts',(-18.6759634182878,-21.0744685344132,
-19.4858063384499));
#68215=CARTESIAN_POINT('Ctrl Pts',(-18.5128492471517,-21.0637105212473,
-19.4771959195974));
#68216=CARTESIAN_POINT('Ctrl Pts',(-18.3208634474756,-21.0285472405061,
-19.4659860531521));
#68217=CARTESIAN_POINT('Ctrl Pts',(-18.2892619825469,-21.0220092011954,
-19.4641036529904));
#68218=CARTESIAN_POINT('Ctrl Pts',(-18.2507862158518,-21.0131272674601,
-19.4617524356487));
#68219=CARTESIAN_POINT('Ctrl Pts',(-18.2437566378528,-21.0114665853829,
-19.4613204217365));
#68220=CARTESIAN_POINT('Ctrl Pts',(-18.2327446160162,-21.0088055085237,
-19.4606396275385));
#68221=CARTESIAN_POINT('Ctrl Pts',(-18.2287562736889,-21.0078294278054,
-19.4603922250205));
#68222=CARTESIAN_POINT('Ctrl Pts',(-18.2213032589949,-21.0059824279431,
-19.4599283040653));
#68223=CARTESIAN_POINT('Ctrl Pts',(-18.2178379428988,-21.0051143398958,
-19.45971194965));
#68224=CARTESIAN_POINT('Ctrl Pts',(-18.2099281801634,-21.0031115933003,
-19.4592166284064));
#68225=CARTESIAN_POINT('Ctrl Pts',(-18.205485228663,-21.0019712622575,-19.4589373378272));
#68226=CARTESIAN_POINT('Ctrl Pts',(-18.1938960459762,-20.9989565947872,
-19.4582061026457));
#68227=CARTESIAN_POINT('Ctrl Pts',(-18.1867559296653,-20.9970592915401,
-19.45775288038));
#68228=CARTESIAN_POINT('Ctrl Pts',(-18.1399886753272,-20.9843696355961,
-19.4547671946653));
#68229=CARTESIAN_POINT('Ctrl Pts',(-18.1006756117236,-20.9724641787672,
-19.452176767735));
#68230=CARTESIAN_POINT('Ctrl Pts',(-18.0519404954401,-20.9561433487171,
-19.4488846754571));
#68231=CARTESIAN_POINT('Ctrl Pts',(-18.0421684963805,-20.9527910671409,
-19.4482204356643));
#68232=CARTESIAN_POINT('Ctrl Pts',(-18.0097868094912,-20.9414169491303,
-19.4460063895182));
#68233=CARTESIAN_POINT('Ctrl Pts',(-17.9872894114241,-20.9330824765389,
-19.4444471234952));
#68234=CARTESIAN_POINT('Ctrl Pts',(-17.837498545487,-20.8746763831487,-19.4339432249352));
#68235=CARTESIAN_POINT('Ctrl Pts',(-17.7151635432548,-20.812745882073,-19.4247959430838));
#68236=CARTESIAN_POINT('Ctrl Pts',(-17.515232337629,-20.6858665341907,-19.4094446777633));
#68237=CARTESIAN_POINT('Ctrl Pts',(-17.43469764991,-20.6263674018111,-19.4031231743271));
#68238=CARTESIAN_POINT('Ctrl Pts',(-17.3474673331981,-20.5518227933746,
-19.3961265280556));
#68239=CARTESIAN_POINT('Ctrl Pts',(-17.3363734622376,-20.5421402090508,
-19.3952335088317));
#68240=CARTESIAN_POINT('Ctrl Pts',(-17.3195949635958,-20.5271849018764,
-19.3938777331764));
#68241=CARTESIAN_POINT('Ctrl Pts',(-17.3138369481387,-20.5219955384412,
-19.3934115136352));
#68242=CARTESIAN_POINT('Ctrl Pts',(-17.3034061506601,-20.5124905300312,
-19.3925651587053));
#68243=CARTESIAN_POINT('Ctrl Pts',(-17.2987240895855,-20.5081852455403,
-19.3921845923967));
#68244=CARTESIAN_POINT('Ctrl Pts',(-17.2886503339771,-20.4988380110578,
-19.3913642997511));
#68245=CARTESIAN_POINT('Ctrl Pts',(-17.2832654510902,-20.4937888183022,
-19.3909248896101));
#68246=CARTESIAN_POINT('Ctrl Pts',(-17.2687174369311,-20.480004018176,-19.3897351486828));
#68247=CARTESIAN_POINT('Ctrl Pts',(-17.2596059848029,-20.4712141282978,
-19.3889871683275));
#68248=CARTESIAN_POINT('Ctrl Pts',(-17.2154438680406,-20.4278390493299,
-19.3853468848612));
#68249=CARTESIAN_POINT('Ctrl Pts',(-17.1815266991841,-20.3921183385539,
-19.382505046357));
#68250=CARTESIAN_POINT('Ctrl Pts',(-17.1219087889954,-20.3247735098996,
-19.3773957271431));
#68251=CARTESIAN_POINT('Ctrl Pts',(-17.0958168402788,-20.2935294852072,
-19.3751151727469));
#68252=CARTESIAN_POINT('Ctrl Pts',(-16.9975791072514,-20.1687504010045,
-19.3663044334865));
#68253=CARTESIAN_POINT('Ctrl Pts',(-16.9324124845035,-20.0699990351479,
-19.3599702655939));
#68254=CARTESIAN_POINT('Ctrl Pts',(-16.8401700281487,-19.9010170997785,
-19.3494529209928));
#68255=CARTESIAN_POINT('Ctrl Pts',(-16.8079896850523,-19.8338775324443,
-19.3453447514761));
#68256=CARTESIAN_POINT('Ctrl Pts',(-16.7661824035679,-19.7333892696328,
-19.3391085907452));
#68257=CARTESIAN_POINT('Ctrl Pts',(-16.7537311183882,-19.701273069552,-19.3371027601424));
#68258=CARTESIAN_POINT('Ctrl Pts',(-16.7395747353296,-19.6619374218935,
-19.3346143329801));
#68259=CARTESIAN_POINT('Ctrl Pts',(-16.7371161760444,-19.6549923679253,
-19.334173793948));
#68260=CARTESIAN_POINT('Ctrl Pts',(-16.7333335382878,-19.6441270330578,
-19.333482528196));
#68261=CARTESIAN_POINT('Ctrl Pts',(-16.7319845897272,-19.6402153858105,
-19.3332332500647));
#68262=CARTESIAN_POINT('Ctrl Pts',(-16.7294937195895,-19.6329231266423,
-19.3327677203345));
#68263=CARTESIAN_POINT('Ctrl Pts',(-16.72834887434,-19.6295435735896,-19.3325516444486));
#68264=CARTESIAN_POINT('Ctrl Pts',(-16.7257666516426,-19.6218570255782,
-19.3320594556358));
#68265=CARTESIAN_POINT('Ctrl Pts',(-16.724334589348,-19.6175483096756,-19.3317830348896));
#68266=CARTESIAN_POINT('Ctrl Pts',(-16.7201090336721,-19.6046966838548,
-19.3309570680216));
#68267=CARTESIAN_POINT('Ctrl Pts',(-16.7173561142753,-19.596140681044,-19.3304052269574));
#68268=CARTESIAN_POINT('Ctrl Pts',(-16.6964356281362,-19.5296715576422,
-19.3261044521384));
#68269=CARTESIAN_POINT('Ctrl Pts',(-16.6807134772718,-19.4710240846937,
-19.3222300748775));
#68270=CARTESIAN_POINT('Ctrl Pts',(-16.6545294519615,-19.3533430424406,
-19.3144035907617));
#68271=CARTESIAN_POINT('Ctrl Pts',(-16.6440111142916,-19.2943740081285,
-19.3104566838939));
#68272=CARTESIAN_POINT('Ctrl Pts',(-16.6214535394725,-19.1271696831847,
-19.2993103664967));
#68273=CARTESIAN_POINT('Ctrl Pts',(-16.6152406948084,-19.0183283631444,
-19.2921162118095));
#68274=CARTESIAN_POINT('Ctrl Pts',(-16.6189300604191,-18.8346522259922,
-19.2803137415875));
#68275=CARTESIAN_POINT('Ctrl Pts',(-16.6244009300767,-18.7599446834037,
-19.2756050152667));
#68276=CARTESIAN_POINT('Ctrl Pts',(-16.6361817721213,-18.6670430439444,
-19.2698683995353));
#68277=CARTESIAN_POINT('Ctrl Pts',(-16.6387925924027,-18.6484415396243,
-19.2687256112206));
#68278=CARTESIAN_POINT('Ctrl Pts',(-16.6429516208518,-18.6214265985706,
-19.2670740193754));
#68279=CARTESIAN_POINT('Ctrl Pts',(-16.6443037408855,-18.6129842987943,
-19.2665590394248));
#68280=CARTESIAN_POINT('Ctrl Pts',(-16.6467653338031,-18.5981892719056,
-19.2656584967923));
#68281=CARTESIAN_POINT('Ctrl Pts',(-16.647852751649,-18.5918330349496,-19.2652722397606));
#68282=CARTESIAN_POINT('Ctrl Pts',(-16.6500216555879,-18.5794946800263,
-19.2645236566506));
#68283=CARTESIAN_POINT('Ctrl Pts',(-16.6510998977407,-18.5735120628327,
-19.2641612316269));
#68284=CARTESIAN_POINT('Ctrl Pts',(-16.6537407757032,-18.5592123036426,
-19.2632962269793));
#68285=CARTESIAN_POINT('Ctrl Pts',(-16.6553275502313,-18.5508996828545,
-19.2627944194819));
#68286=CARTESIAN_POINT('Ctrl Pts',(-16.6612438231142,-18.5208845092304,
-19.2609860382192));
#68287=CARTESIAN_POINT('Ctrl Pts',(-16.6658638016498,-18.4992401798635,
-19.2596887196481));
#68288=CARTESIAN_POINT('Ctrl Pts',(-16.7123557174045,-18.2970151243205,
-19.2476207470718));
#68289=CARTESIAN_POINT('Ctrl Pts',(-16.7774332190802,-18.1226006641512,
-19.2377043115437));
#68290=CARTESIAN_POINT('Ctrl Pts',(-16.9020631158015,-17.887978516093,-19.2232222275414));
#68291=CARTESIAN_POINT('Ctrl Pts',(-16.9437254532753,-17.8192822510152,
-19.2188075830982));
#68292=CARTESIAN_POINT('Ctrl Pts',(-17.0096095335596,-17.7233961414507,
-19.2121531256959));
#68293=CARTESIAN_POINT('Ctrl Pts',(-17.0307903660063,-17.694197744066,-19.2100552283183));
#68294=CARTESIAN_POINT('Ctrl Pts',(-17.0572435838098,-17.6596251704274,
-19.2074646073566));
#68295=CARTESIAN_POINT('Ctrl Pts',(-17.0618133029625,-17.6537178943589,
-19.2070180967292));
#68296=CARTESIAN_POINT('Ctrl Pts',(-17.0689767432219,-17.6445582771865,
-19.2063195004738));
#68297=CARTESIAN_POINT('Ctrl Pts',(-17.0715490068382,-17.6412891246286,
-19.2060689139591));
#68298=CARTESIAN_POINT('Ctrl Pts',(-17.07634410704,-17.6352317379793,-19.2056022310631));
#68299=CARTESIAN_POINT('Ctrl Pts',(-17.0785643589448,-17.632441531023,-19.2053863184497));
#68300=CARTESIAN_POINT('Ctrl Pts',(-17.0836086488511,-17.6261351023063,
-19.2048961737008));
#68301=CARTESIAN_POINT('Ctrl Pts',(-17.0864368654595,-17.622622305093,-19.20462164427));
#68302=CARTESIAN_POINT('Ctrl Pts',(-17.0937677154814,-17.6135763215634,
-19.2039108419476));
#68303=CARTESIAN_POINT('Ctrl Pts',(-17.0982870892332,-17.6080568611652,
-19.2034734031579));
#68304=CARTESIAN_POINT('Ctrl Pts',(-17.1262011774338,-17.5743150713616,
-19.2007767533001));
#68305=CARTESIAN_POINT('Ctrl Pts',(-17.150296290211,-17.5466833087354,-19.1984713749365));
#68306=CARTESIAN_POINT('Ctrl Pts',(-17.2905170531057,-17.3940687675811,
-19.1852451970303));
#68307=CARTESIAN_POINT('Ctrl Pts',(-17.4206992528575,-17.282857403795,-19.1737337219581));
#68308=CARTESIAN_POINT('Ctrl Pts',(-17.6422278129316,-17.1357376190495,
-19.1564523379592));
#68309=CARTESIAN_POINT('Ctrl Pts',(-17.7251142125269,-17.0884203111888,
-19.1503961515445));
#68310=CARTESIAN_POINT('Ctrl Pts',(-17.8301630321998,-17.0375222586462,
-19.1432260059483));
#68311=CARTESIAN_POINT('Ctrl Pts',(-17.8495480862174,-17.0284898878957,
-19.1419225599029));
#68312=CARTESIAN_POINT('Ctrl Pts',(-17.8772896192678,-17.0160719337491,
-19.1400844149171));
#68313=CARTESIAN_POINT('Ctrl Pts',(-17.8855355006895,-17.0124438261594,
-19.1395414139044));
#68314=CARTESIAN_POINT('Ctrl Pts',(-17.8997945231754,-17.0062783311374,
-19.1386081574022));
#68315=CARTESIAN_POINT('Ctrl Pts',(-17.9057966516453,-17.0037159330579,
-19.1382170514343));
#68316=CARTESIAN_POINT('Ctrl Pts',(-17.9173073022399,-16.9988646697857,
-19.1374702809543));
#68317=CARTESIAN_POINT('Ctrl Pts',(-17.9228138280109,-16.996571255146,-19.1371144646156));
#68318=CARTESIAN_POINT('Ctrl Pts',(-17.937148406578,-16.9906720130187,-19.1361918660068));
#68319=CARTESIAN_POINT('Ctrl Pts',(-17.9459913232665,-16.9871024799316,
-19.1356263158361));
#68320=CARTESIAN_POINT('Ctrl Pts',(-17.9761779552821,-16.9751539016862,
-19.1337076838583));
#68321=CARTESIAN_POINT('Ctrl Pts',(-17.997634016078,-16.9670617273971,-19.1323642327048));
#68322=CARTESIAN_POINT('Ctrl Pts',(-18.1851717970417,-16.8997912144435,
-19.1207861084486));
#68323=CARTESIAN_POINT('Ctrl Pts',(-18.357909126627,-16.8612260736904,-19.111310598646));
#68324=CARTESIAN_POINT('Ctrl Pts',(-18.6194791893889,-16.8363338261108,
-19.0970121190958));
#68325=CARTESIAN_POINT('Ctrl Pts',(-18.7059301568894,-16.8334230960824,
-19.0922789500323));
#68326=CARTESIAN_POINT('Ctrl Pts',(-18.8299712795888,-16.83684090002,-19.0851931276914));
#68327=CARTESIAN_POINT('Ctrl Pts',(-18.8675963009726,-16.838883784974,-19.0830043730105));
#68328=CARTESIAN_POINT('Ctrl Pts',(-18.9126826185291,-16.8425406556746,
-19.0803129997573));
#68329=CARTESIAN_POINT('Ctrl Pts',(-18.9202177044491,-16.8431924776871,
-19.0798608942191));
#68330=CARTESIAN_POINT('Ctrl Pts',(-18.9319119053231,-16.8442672480035,
-19.0791554335674));
#68331=CARTESIAN_POINT('Ctrl Pts',(-18.9360736205007,-16.8446621705784,
-19.078903625593));
#68332=CARTESIAN_POINT('Ctrl Pts',(-18.9437810865531,-16.8454166056384,
-19.0784358449493));
#68333=CARTESIAN_POINT('Ctrl Pts',(-18.9473271095425,-16.8457727460157,
-19.0782200635003));
#68334=CARTESIAN_POINT('Ctrl Pts',(-18.955331123892,-16.8465970394489,-19.0777317305294));
#68335=CARTESIAN_POINT('Ctrl Pts',(-18.9597885121036,-16.8470703955601,
-19.077458891137));
#68336=CARTESIAN_POINT('Ctrl Pts',(-18.9729093915315,-16.8485059341782,
-19.0766532012215));
#68337=CARTESIAN_POINT('Ctrl Pts',(-18.9815683593811,-16.8495074592901,
-19.0761182159341));
#68338=CARTESIAN_POINT('Ctrl Pts',(-19.0431255462348,-16.8570129055434,
-19.0722928079547));
#68339=CARTESIAN_POINT('Ctrl Pts',(-19.0957633011967,-16.8654584093374,
-19.0689054950545));
#68340=CARTESIAN_POINT('Ctrl Pts',(-19.1656388383923,-16.8793930337781,
-19.0643007329114));
#68341=CARTESIAN_POINT('Ctrl Pts',(-19.1832106628471,-16.8831303864347,
-19.0631334583941));
#68342=CARTESIAN_POINT('Ctrl Pts',(-19.247762684622,-16.8977211115999,-19.0588155672159));
#68343=CARTESIAN_POINT('Ctrl Pts',(-19.2944148912027,-16.9099547594957,
-19.0556369323652));
#68344=CARTESIAN_POINT('Ctrl Pts',(-19.4454004603957,-16.9551118536413,
-19.0452267183417));
#68345=CARTESIAN_POINT('Ctrl Pts',(-19.5476150532436,-16.9945304867991,
-19.0379941552358));
#68346=CARTESIAN_POINT('Ctrl Pts',(-19.7146197639511,-17.0742883792042,
-19.0260981926706));
#68347=CARTESIAN_POINT('Ctrl Pts',(-19.7811167750216,-17.1105427750303,
-19.02133540524));
#68348=CARTESIAN_POINT('Ctrl Pts',(-19.8616163712297,-17.1602055579949,
-19.0155404663254));
#68349=CARTESIAN_POINT('Ctrl Pts',(-19.8775637900329,-17.1703412511018,
-19.0143907715948));
#68350=CARTESIAN_POINT('Ctrl Pts',(-19.9005446215904,-17.1853828666926,
-19.012731102403));
#68351=CARTESIAN_POINT('Ctrl Pts',(-19.9076869637124,-17.1901199347167,
-19.0122148662593));
#68352=CARTESIAN_POINT('Ctrl Pts',(-19.9201552883205,-17.1984988576672,
-19.0113128741283));
#68353=CARTESIAN_POINT('Ctrl Pts',(-19.9254937183086,-17.2021219057221,
-19.0109264168999));
#68354=CARTESIAN_POINT('Ctrl Pts',(-19.9358248360724,-17.2092025524012,
-19.0101779871691));
#68355=CARTESIAN_POINT('Ctrl Pts',(-19.9408193670174,-17.212657337805,-19.0098159131762));
#68356=CARTESIAN_POINT('Ctrl Pts',(-19.9527192151025,-17.2209645577646,
-19.0089526065529));
#68357=CARTESIAN_POINT('Ctrl Pts',(-19.9596105511618,-17.225836911659,-19.0084521390993));
#68358=CARTESIAN_POINT('Ctrl Pts',(-19.9843472102746,-17.2435491921045,
-19.00665364209));
#68359=CARTESIAN_POINT('Ctrl Pts',(-20.0020217954633,-17.2566259737511,
-19.0053647341329));
#68360=CARTESIAN_POINT('Ctrl Pts',(-20.1679063497703,-17.3834035594385,
-18.9932203827108));
#68361=CARTESIAN_POINT('Ctrl Pts',(-20.3006543931763,-17.5159700118114,
-18.9832348475224));
#68362=CARTESIAN_POINT('Ctrl Pts',(-20.4625576818018,-17.7272251792347,
-18.9687214806273));
#68363=CARTESIAN_POINT('Ctrl Pts',(-20.5072415291622,-17.79286345203,-18.9643555453313));
#68364=CARTESIAN_POINT('Ctrl Pts',(-20.5665926695611,-17.8915398015072,
-18.9577673506855));
#68365=CARTESIAN_POINT('Ctrl Pts',(-20.5842696000682,-17.9226925680994,
-18.9556837747955));
#68366=CARTESIAN_POINT('Ctrl Pts',(-20.6046593272031,-17.9608500459633,
-18.9531090434137));
#68367=CARTESIAN_POINT('Ctrl Pts',(-20.6081371455009,-17.9674419743132,
-18.9526634411636));
#68368=CARTESIAN_POINT('Ctrl Pts',(-20.6135001060839,-17.9777384193655,
-18.9519659597463));
#68369=CARTESIAN_POINT('Ctrl Pts',(-20.6154093087419,-17.9814304308465,
-18.9517155719581));
#68370=CARTESIAN_POINT('Ctrl Pts',(-20.6189363544477,-17.9883005357199,
-18.9512490657672));
#68371=CARTESIAN_POINT('Ctrl Pts',(-20.6205570443778,-17.9914771030985,
-18.9510331299139));
#68372=CARTESIAN_POINT('Ctrl Pts',(-20.6242111984938,-17.9986842049165,
-18.9505426817761));
#68373=CARTESIAN_POINT('Ctrl Pts',(-20.6262397910603,-18.0027171378762,
-18.9502678706272));
#68374=CARTESIAN_POINT('Ctrl Pts',(-20.6322139783063,-18.0146893297531,
-18.9494510467547));
#68375=CARTESIAN_POINT('Ctrl Pts',(-20.6361225596381,-18.0226468045976,
-18.9489068120163));
#68376=CARTESIAN_POINT('Ctrl Pts',(-20.6648568493489,-18.082087546218,-18.9448329805944));
#68377=CARTESIAN_POINT('Ctrl Pts',(-20.6876362615745,-18.1345283096112,
-18.9411920412909));
#68378=CARTESIAN_POINT('Ctrl Pts',(-20.7683686241143,-18.3431011474956,
-18.9267030005516));
#68379=CARTESIAN_POINT('Ctrl Pts',(-20.809946228261,-18.5049335841527,-18.9155001551014));
#68380=CARTESIAN_POINT('Ctrl Pts',(-20.8399080681384,-18.727838418948,-18.9010061891986));
#68381=CARTESIAN_POINT('Ctrl Pts',(-20.8452891034385,-18.7859985162162,
-18.8973011530895));
#68382=CARTESIAN_POINT('Ctrl Pts',(-20.8500786755013,-18.880032259341,-18.8914414621977));
#68383=CARTESIAN_POINT('Ctrl Pts',(-20.8509926290197,-18.9157954380901,
-18.8892429548497));
#68384=CARTESIAN_POINT('Ctrl Pts',(-20.8510022031581,-18.9625398042562,
-18.8864068683001));
#68385=CARTESIAN_POINT('Ctrl Pts',(-20.850919130275,-18.9735132198352,-18.8857437716456));
#68386=CARTESIAN_POINT('Ctrl Pts',(-20.8506443290979,-18.9914191399575,
-18.8846660223645));
#68387=CARTESIAN_POINT('Ctrl Pts',(-20.8505038547557,-18.9983521205708,
-18.8842497718997));
#68388=CARTESIAN_POINT('Ctrl Pts',(-20.8501671510663,-19.0117252006668,
-18.8834488320296));
#68389=CARTESIAN_POINT('Ctrl Pts',(-20.8499755814384,-19.0181653309523,
-18.8830640011775));
#68390=CARTESIAN_POINT('Ctrl Pts',(-20.8494626513394,-19.0331125256614,
-18.882172829525));
#68391=CARTESIAN_POINT('Ctrl Pts',(-20.8491193704855,-19.0416187639829,
-18.881667180825));
#68392=CARTESIAN_POINT('Ctrl Pts',(-20.8478634330838,-19.068686500085,-18.8800627833598));
#68393=CARTESIAN_POINT('Ctrl Pts',(-20.8467576624232,-19.0872384764525,
-18.878970085231));
#68394=CARTESIAN_POINT('Ctrl Pts',(-20.8436139253888,-19.130403857889,-18.8764424037144));
#68395=CARTESIAN_POINT('Ctrl Pts',(-20.8413892477373,-19.1550011838357,
-18.8750132232758));
#68396=CARTESIAN_POINT('Ctrl Pts',(-20.8320826336087,-19.241081379516,-18.8700446278674));
#68397=CARTESIAN_POINT('Ctrl Pts',(-20.8227356923287,-19.3022896673205,
-18.8665717938389));
#68398=CARTESIAN_POINT('Ctrl Pts',(-20.7895029612841,-19.4702078065612,
-18.857102788481));
#68399=CARTESIAN_POINT('Ctrl Pts',(-20.7600278810369,-19.5755543537232,
-18.8512347937857));
#68400=CARTESIAN_POINT('Ctrl Pts',(-20.7225806288389,-19.6781102413592,
-18.845275429269));
#68401=CARTESIAN_POINT('Origin',(-18.734,-18.952,0.));
#68402=CARTESIAN_POINT('',(-20.7225806448396,-19.6781101975385,-18.0457833736847));
#68403=CARTESIAN_POINT('',(-20.7225805813239,-19.6781103714872,-18.2676550109742));
#68404=CARTESIAN_POINT('',(-20.7225805821191,-19.6781103693095,0.));
#68405=CARTESIAN_POINT('',(-20.8509999976816,-18.9519009238279,-18.3109437209775));
#68406=CARTESIAN_POINT('Ctrl Pts',(-20.7225805813239,-19.6781103714872,
-18.2676550109742));
#68407=CARTESIAN_POINT('Ctrl Pts',(-20.7255215254997,-19.6700560801449,
-18.2681338976806));
#68408=CARTESIAN_POINT('Ctrl Pts',(-20.7284136840267,-19.6619835175783,
-18.2686116714034));
#68409=CARTESIAN_POINT('Ctrl Pts',(-20.7649458433877,-19.5580302170336,
-18.2747374158079));
#68410=CARTESIAN_POINT('Ctrl Pts',(-20.7916902777909,-19.4598634697817,
-18.280222863525));
#68411=CARTESIAN_POINT('Ctrl Pts',(-20.8346520007344,-19.2412122723913,
-18.2923391376341));
#68412=CARTESIAN_POINT('Ctrl Pts',(-20.8477603784538,-19.1204977421627,
-18.2989652682401));
#68413=CARTESIAN_POINT('Ctrl Pts',(-20.8507279701885,-18.9878359543606,
-18.3067852888075));
#68414=CARTESIAN_POINT('Ctrl Pts',(-20.8508915333075,-18.9763256758259,
-18.3074682690814));
#68415=CARTESIAN_POINT('Ctrl Pts',(-20.8509827804114,-18.9612521100644,
-18.308369215915));
#68416=CARTESIAN_POINT('Ctrl Pts',(-20.8509953532782,-18.9576892778179,
-18.3085826443122));
#68417=CARTESIAN_POINT('Ctrl Pts',(-20.8509997175536,-18.9533444198951,
-18.3088435204735));
#68418=CARTESIAN_POINT('Ctrl Pts',(-20.8510000697472,-18.9525623810612,
-18.3088904997976));
#68419=CARTESIAN_POINT('Ctrl Pts',(-20.8509999886044,-18.9517803438104,
-18.3089375029375));
#68420=CARTESIAN_POINT('Ctrl Pts',(-20.8509999976816,-18.9519009238279,
-18.3109437209775));
#68421=CARTESIAN_POINT('Ctrl Pts',(-20.8509997507685,-18.9466250329455,
-18.3112630160645));
#68422=CARTESIAN_POINT('Ctrl Pts',(-20.8509797813958,-18.9413491960952,
-18.3115823111514));
#68423=CARTESIAN_POINT('Ctrl Pts',(-20.8509400905189,-18.936073507803,-18.3119016062384));
#68424=CARTESIAN_POINT('Ctrl Pts',(-20.8503946018242,-18.8635674674005,
-18.3162898151688));
#68425=CARTESIAN_POINT('Ctrl Pts',(-20.8461186979221,-18.7909479534651,
-18.3206780240991));
#68426=CARTESIAN_POINT('Ctrl Pts',(-20.8380978239802,-18.7186304494545,
-18.3250662330295));
#68427=CARTESIAN_POINT('Ctrl Pts',(-20.8300888543451,-18.6464202766104,
-18.3294479291303));
#68428=CARTESIAN_POINT('Ctrl Pts',(-20.8183460011054,-18.5745116993627,
-18.333829625231));
#68429=CARTESIAN_POINT('Ctrl Pts',(-20.8029067175878,-18.5033197197112,
-18.3382113213317));
#68430=CARTESIAN_POINT('Ctrl Pts',(-20.787485576457,-18.4322113963014,-18.3425878685909));
#68431=CARTESIAN_POINT('Ctrl Pts',(-20.7683767353657,-18.3618184668112,
-18.34696441585));
#68432=CARTESIAN_POINT('Ctrl Pts',(-20.7456691798647,-18.292548628948,-18.3513409631091));
#68433=CARTESIAN_POINT('Ctrl Pts',(-20.7229760251654,-18.2233227210093,
-18.3557147348256));
#68434=CARTESIAN_POINT('Ctrl Pts',(-20.6966888342334,-18.1552189487538,
-18.360088506542));
#68435=CARTESIAN_POINT('Ctrl Pts',(-20.66694683346,-18.0886312844346,-18.3644622782585));
#68436=CARTESIAN_POINT('Ctrl Pts',(-20.6372138832772,-18.0220638829652,
-18.3688347190215));
#68437=CARTESIAN_POINT('Ctrl Pts',(-20.6040284070361,-17.9570121136714,
-18.3732071597846));
#68438=CARTESIAN_POINT('Ctrl Pts',(-20.567577676683,-17.8938497726835,-18.3775796005476));
#68439=CARTESIAN_POINT('Ctrl Pts',(-20.5311260142806,-17.8306858166275,
-18.3819521531145));
#68440=CARTESIAN_POINT('Ctrl Pts',(-20.4914091748402,-17.7694118015958,
-18.3863247056813));
#68441=CARTESIAN_POINT('Ctrl Pts',(-20.4486594348621,-17.7103752489426,
-18.3906972582482));
#68442=CARTESIAN_POINT('Ctrl Pts',(-20.4058653275914,-17.6512774259282,
-18.395074348815));
#68443=CARTESIAN_POINT('Ctrl Pts',(-20.3600323187913,-17.5944220931037,
-18.3994514393818));
#68444=CARTESIAN_POINT('Ctrl Pts',(-20.3114344316444,-17.5401254964188,
-18.4038285299487));
#68445=CARTESIAN_POINT('Ctrl Pts',(-20.2628100033876,-17.4857992463471,
-18.4082080110071));
#68446=CARTESIAN_POINT('Ctrl Pts',(-20.2114180304778,-17.434034857225,-18.4125874920656));
#68447=CARTESIAN_POINT('Ctrl Pts',(-20.1575691237198,-17.3851113792003,
-18.416966973124));
#68448=CARTESIAN_POINT('Ctrl Pts',(-20.1036247701359,-17.3361011846391,
-18.4213542167833));
#68449=CARTESIAN_POINT('Ctrl Pts',(-20.0472151597982,-17.2899422626071,
-18.4257414604425));
#68450=CARTESIAN_POINT('Ctrl Pts',(-19.9886831896908,-17.2468727046031,
-18.4301287041018));
#68451=CARTESIAN_POINT('Ctrl Pts',(-19.9488870900799,-17.2175895552853,
-18.4331116070411));
#68452=CARTESIAN_POINT('Ctrl Pts',(-19.9081105258033,-17.1897336331323,
-18.4360945099805));
#68453=CARTESIAN_POINT('Ctrl Pts',(-19.8664678605231,-17.1633676887403,
-18.4390774129199));
#68454=CARTESIAN_POINT('Ctrl Pts',(-19.8052064921926,-17.1245802139255,
-18.4434656218502));
#68455=CARTESIAN_POINT('Ctrl Pts',(-19.7418305075797,-17.0888680068776,
-18.4478538307804));
#68456=CARTESIAN_POINT('Ctrl Pts',(-19.6766813842659,-17.0564681992226,
-18.4522420397107));
#68457=CARTESIAN_POINT('Ctrl Pts',(-19.6116289530532,-17.0241164782542,
-18.4566237358114));
#68458=CARTESIAN_POINT('Ctrl Pts',(-19.544809035632,-16.9950676104731,-18.461005431912));
#68459=CARTESIAN_POINT('Ctrl Pts',(-19.476590855784,-16.9695147362702,-18.4653871280126));
#68460=CARTESIAN_POINT('Ctrl Pts',(-19.4084528377265,-16.943991888728,-18.4697636752716));
#68461=CARTESIAN_POINT('Ctrl Pts',(-19.338920270696,-16.9219570424212,-18.4741402225306));
#68462=CARTESIAN_POINT('Ctrl Pts',(-19.2683841301356,-16.9035560536204,
-18.4785167697896));
#68463=CARTESIAN_POINT('Ctrl Pts',(-19.1978927225705,-16.8851667344593,
-18.482890541506));
#68464=CARTESIAN_POINT('Ctrl Pts',(-19.1263994698867,-16.8704068217633,
-18.4872643132223));
#68465=CARTESIAN_POINT('Ctrl Pts',(-19.0543110010062,-16.8593724978787,
-18.4916380849386));
#68466=CARTESIAN_POINT('Ctrl Pts',(-18.9822444688891,-16.848341531776,-18.4960105257015));
#68467=CARTESIAN_POINT('Ctrl Pts',(-18.9095835567044,-16.8410339766645,
-18.5003829664644));
#68468=CARTESIAN_POINT('Ctrl Pts',(-18.8367439345959,-16.8374946952292,
-18.5047554072273));
#68469=CARTESIAN_POINT('Ctrl Pts',(-18.7639024499703,-16.8339553232942,
-18.509127959794));
#68470=CARTESIAN_POINT('Ctrl Pts',(-18.6908827282545,-16.8341844377533,
-18.5135005123607));
#68471=CARTESIAN_POINT('Ctrl Pts',(-18.6181027067752,-16.8381748375461,
-18.5178730649274));
#68472=CARTESIAN_POINT('Ctrl Pts',(-18.5452471514446,-16.8421693787263,
-18.5222501554941));
#68473=CARTESIAN_POINT('Ctrl Pts',(-18.4726322757212,-16.8499329725835,
-18.5266272460608));
#68474=CARTESIAN_POINT('Ctrl Pts',(-18.4006723159531,-16.8614063869207,
-18.5310043366275));
#68475=CARTESIAN_POINT('Ctrl Pts',(-18.3286730561801,-16.8728860673153,
-18.5353838176857));
#68476=CARTESIAN_POINT('Ctrl Pts',(-18.2573298966123,-16.8880795015318,
-18.539763298744));
#68477=CARTESIAN_POINT('Ctrl Pts',(-18.1870456020006,-16.9068765595913,
-18.5441427798023));
#68478=CARTESIAN_POINT('Ctrl Pts',(-18.1166367289484,-16.92570693531,-18.5485300234614));
#68479=CARTESIAN_POINT('Ctrl Pts',(-18.0472909281459,-16.9481535415646,
-18.5529172671205));
#68480=CARTESIAN_POINT('Ctrl Pts',(-17.9793940004985,-16.9740569306685,
-18.5573045107795));
#68481=CARTESIAN_POINT('Ctrl Pts',(-17.9332306321349,-16.9916687392511,
-18.5602874137201));
#68482=CARTESIAN_POINT('Ctrl Pts',(-17.8877366290263,-17.0108774944519,
-18.5632703166607));
#68483=CARTESIAN_POINT('Ctrl Pts',(-17.8430266573748,-17.0316210002369,
-18.5662532196012));
#68484=CARTESIAN_POINT('Ctrl Pts',(-17.7772529124845,-17.0621371917538,
-18.5706414285354));
#68485=CARTESIAN_POINT('Ctrl Pts',(-17.7129203794319,-17.0960960250395,
-18.5750296374695));
#68486=CARTESIAN_POINT('Ctrl Pts',(-17.6504132837262,-17.1333387263388,
-18.5794178464036));
#68487=CARTESIAN_POINT('Ctrl Pts',(-17.5879989589142,-17.1705261532945,
-18.5837995425081));
#68488=CARTESIAN_POINT('Ctrl Pts',(-17.5274051041878,-17.2109875282323,
-18.5881812386126));
#68489=CARTESIAN_POINT('Ctrl Pts',(-17.4689939738811,-17.2545169356124,
-18.5925629347171));
#68490=CARTESIAN_POINT('Ctrl Pts',(-17.410651481301,-17.2979951924746,-18.59693948198));
#68491=CARTESIAN_POINT('Ctrl Pts',(-17.3544870028672,-17.3445340332485,
-18.6013160292429));
#68492=CARTESIAN_POINT('Ctrl Pts',(-17.3008348082133,-17.393883658692,-18.6056925765057));
#68493=CARTESIAN_POINT('Ctrl Pts',(-17.2472166390015,-17.4432019873203,
-18.6100663482259));
#68494=CARTESIAN_POINT('Ctrl Pts',(-17.1961079465048,-17.4953272380339,
-18.6144401199461));
#68495=CARTESIAN_POINT('Ctrl Pts',(-17.1478097053788,-17.5499695619391,
-18.6188138916663));
#68496=CARTESIAN_POINT('Ctrl Pts',(-17.0995261615698,-17.6045952580014,
-18.6231863324331));
#68497=CARTESIAN_POINT('Ctrl Pts',(-17.0540516905101,-17.6617361453902,
-18.6275587731999));
#68498=CARTESIAN_POINT('Ctrl Pts',(-17.0116490089833,-17.7210669946159,
-18.6319312139666));
#68499=CARTESIAN_POINT('Ctrl Pts',(-16.9692452432155,-17.7803993609378,
-18.6363037665372));
#68500=CARTESIAN_POINT('Ctrl Pts',(-16.9299137017786,-17.8419214066584,
-18.6406763191077));
#68501=CARTESIAN_POINT('Ctrl Pts',(-16.8938745512688,-17.9052778148278,
-18.6450488716783));
#68502=CARTESIAN_POINT('Ctrl Pts',(-16.8577979979695,-17.9686999766668,
-18.6494259622488));
#68503=CARTESIAN_POINT('Ctrl Pts',(-16.8250208968186,-18.0339598817744,
-18.6538030528193));
#68504=CARTESIAN_POINT('Ctrl Pts',(-16.7957176611908,-18.1006771616711,
-18.6581801433897));
#68505=CARTESIAN_POINT('Ctrl Pts',(-16.7663984219786,-18.1674308783503,
-18.6625596244518));
#68506=CARTESIAN_POINT('Ctrl Pts',(-16.7405569966195,-18.2356431030953,
-18.6669391055139));
#68507=CARTESIAN_POINT('Ctrl Pts',(-16.7183187921507,-18.3049155632198,
-18.671318586576));
#68508=CARTESIAN_POINT('Ctrl Pts',(-16.6960411706141,-18.3743108083137,
-18.6757058302388));
#68509=CARTESIAN_POINT('Ctrl Pts',(-16.6773796475295,-18.444769574883,-18.6800930739016));
#68510=CARTESIAN_POINT('Ctrl Pts',(-16.662408979339,-18.5158811594111,-18.6844803175644));
#68511=CARTESIAN_POINT('Ctrl Pts',(-16.6522303676447,-18.5642301840949,
-18.6874632204705));
#68512=CARTESIAN_POINT('Ctrl Pts',(-16.6437568500116,-18.6128807754369,
-18.6904461233766));
#68513=CARTESIAN_POINT('Ctrl Pts',(-16.6369981960583,-18.6617028517788,
-18.6934290262827));
#68514=CARTESIAN_POINT('Ctrl Pts',(-16.6270554032346,-18.7335259978735,
-18.6978172352091));
#68515=CARTESIAN_POINT('Ctrl Pts',(-16.6207874279489,-18.8060007495847,
-18.7022054441356));
#68516=CARTESIAN_POINT('Ctrl Pts',(-16.6182687405808,-18.8787180928431,
-18.706593653062));
#68517=CARTESIAN_POINT('Ctrl Pts',(-16.6157537913624,-18.9513275115075,
-18.7109753491589));
#68518=CARTESIAN_POINT('Ctrl Pts',(-16.6169771002007,-19.0241783288748,
-18.7153570452557));
#68519=CARTESIAN_POINT('Ctrl Pts',(-16.6219616061143,-19.0968544882031,
-18.7197387413525));
#68520=CARTESIAN_POINT('Ctrl Pts',(-16.6269402548368,-19.169445247261,-18.7241152886078));
#68521=CARTESIAN_POINT('Ctrl Pts',(-16.6356712880178,-19.241861277126,-18.728491835863));
#68522=CARTESIAN_POINT('Ctrl Pts',(-16.6481255978392,-19.3136862983448,
-18.7328683831182));
#68523=CARTESIAN_POINT('Ctrl Pts',(-16.6605720093185,-19.3854657691794,
-18.7372421548308));
#68524=CARTESIAN_POINT('Ctrl Pts',(-16.6767369302053,-19.4566545009215,
-18.7416159265435));
#68525=CARTESIAN_POINT('Ctrl Pts',(-16.6965395553228,-19.5268425318082,
-18.7459896982561));
#68526=CARTESIAN_POINT('Ctrl Pts',(-16.716336154435,-19.5970092042419,-18.7503621390153));
#68527=CARTESIAN_POINT('Ctrl Pts',(-16.7397681292056,-19.6661753164048,
-18.7547345797745));
#68528=CARTESIAN_POINT('Ctrl Pts',(-16.7667042167151,-19.7339439245044,
-18.7591070205337));
#68529=CARTESIAN_POINT('Ctrl Pts',(-16.7936409929835,-19.8017142654554,
-18.7634795730968));
#68530=CARTESIAN_POINT('Ctrl Pts',(-16.8240818798531,-19.8680865838683,
-18.7678521256598));
#68531=CARTESIAN_POINT('Ctrl Pts',(-16.8578472840023,-19.9326834281533,
-18.7722246782229));
#68532=CARTESIAN_POINT('Ctrl Pts',(-16.8916477311622,-19.9973473134812,
-18.776601768786));
#68533=CARTESIAN_POINT('Ctrl Pts',(-16.9287793604415,-20.060231617285,-18.7809788593491));
#68534=CARTESIAN_POINT('Ctrl Pts',(-16.9690167487956,-20.1209837992753,
-18.7853559499122));
#68535=CARTESIAN_POINT('Ctrl Pts',(-17.0092761122814,-20.1817691602876,
-18.789735430967));
#68536=CARTESIAN_POINT('Ctrl Pts',(-17.0526443249046,-20.240419692987,-18.7941149120218));
#68537=CARTESIAN_POINT('Ctrl Pts',(-17.0988543828153,-20.296614372451,-18.7984943930766));
#68538=CARTESIAN_POINT('Ctrl Pts',(-17.1451463477448,-20.3529086566087,
-18.8028816367322));
#68539=CARTESIAN_POINT('Ctrl Pts',(-17.1942898914284,-20.4067380382408,
-18.8072688803879));
#68540=CARTESIAN_POINT('Ctrl Pts',(-17.245980141449,-20.4578173529873,-18.8116561240436));
#68541=CARTESIAN_POINT('Ctrl Pts',(-17.2811245310909,-20.4925463655067,
-18.8146390270171));
#68542=CARTESIAN_POINT('Ctrl Pts',(-17.3174454256977,-20.5260048960133,
-18.8176219299906));
#68543=CARTESIAN_POINT('Ctrl Pts',(-17.3548387352824,-20.5581143190641,
-18.8206048329642));
#68544=CARTESIAN_POINT('Ctrl Pts',(-17.4098487897263,-20.6053511411,-18.8249930418924));
#68545=CARTESIAN_POINT('Ctrl Pts',(-17.4673958504111,-20.6498507248998,
-18.8293812508206));
#68546=CARTESIAN_POINT('Ctrl Pts',(-17.5271763106365,-20.6913290611011,
-18.8337694597488));
#68547=CARTESIAN_POINT('Ctrl Pts',(-17.5868680467462,-20.7327458365737,
-18.8381511558473));
#68548=CARTESIAN_POINT('Ctrl Pts',(-17.6487862091488,-20.7711499931513,
-18.8425328519459));
#68549=CARTESIAN_POINT('Ctrl Pts',(-17.7125933764222,-20.806297039126,-18.8469145480444));
#68550=CARTESIAN_POINT('Ctrl Pts',(-17.776325565195,-20.8414027845239,-18.8512910953012));
#68551=CARTESIAN_POINT('Ctrl Pts',(-17.8419419289072,-20.873258790821,-18.855667642558));
#68552=CARTESIAN_POINT('Ctrl Pts',(-17.9090766869063,-20.9016642089125,
-18.8600441898149));
#68553=CARTESIAN_POINT('Ctrl Pts',(-17.9761688690169,-20.9300516127005,
-18.864417961529));
#68554=CARTESIAN_POINT('Ctrl Pts',(-18.0447770916536,-20.9549925826758,
-18.8687917332431));
#68555=CARTESIAN_POINT('Ctrl Pts',(-18.114512903542,-20.9763331586777,-18.8731655049572));
#68556=CARTESIAN_POINT('Ctrl Pts',(-18.184227494588,-20.9976672406704,-18.8775379457179));
#68557=CARTESIAN_POINT('Ctrl Pts',(-18.255068532683,-21.0154029627463,-18.8819103864785));
#68558=CARTESIAN_POINT('Ctrl Pts',(-18.3266312007864,-21.0294358381012,
-18.8862828272392));
#68559=CARTESIAN_POINT('Ctrl Pts',(-18.3981956987546,-21.0434690722781,
-18.8906553798036));
#68560=CARTESIAN_POINT('Ctrl Pts',(-18.4704813896189,-21.0537991808911,
-18.895027932368));
#68561=CARTESIAN_POINT('Ctrl Pts',(-18.5430736858662,-21.0603728661153,
-18.8994004849324));
#68562=CARTESIAN_POINT('Ctrl Pts',(-18.6157413211363,-21.0669533737579,
-18.9037775754968));
#68563=CARTESIAN_POINT('Ctrl Pts',(-18.6887157156707,-21.0697696306808,
-18.9081546660611));
#68564=CARTESIAN_POINT('Ctrl Pts',(-18.7615784216581,-21.0688203586178,
-18.9125317566255));
#68565=CARTESIAN_POINT('Ctrl Pts',(-18.8344809206732,-21.0678705681221,
-18.9169112376815));
#68566=CARTESIAN_POINT('Ctrl Pts',(-18.9072711279956,-21.0631511854102,
-18.9212907187374));
#68567=CARTESIAN_POINT('Ctrl Pts',(-18.9795345883492,-21.0547129537634,
-18.9256701997934));
#68568=CARTESIAN_POINT('Ctrl Pts',(-19.0519261352012,-21.0462597654076,
-18.9300574434501));
#68569=CARTESIAN_POINT('Ctrl Pts',(-19.123788594604,-21.0340746456029,-18.9344446871069));
#68570=CARTESIAN_POINT('Ctrl Pts',(-19.1947171668018,-21.0182595897452,
-18.9388319307636));
#68571=CARTESIAN_POINT('Ctrl Pts',(-19.2429417616859,-21.0075068755967,
-18.9418148337242));
#68572=CARTESIAN_POINT('Ctrl Pts',(-19.2907349020827,-20.9950772191557,
-18.9447977366849));
#68573=CARTESIAN_POINT('Ctrl Pts',(-19.3379741345032,-20.9810155851671,
-18.9477806396456));
#68574=CARTESIAN_POINT('Ctrl Pts',(-19.4074719557487,-20.9603282692375,
-18.9521690525416));
#68575=CARTESIAN_POINT('Ctrl Pts',(-19.4760413397801,-20.9360257809649,
-18.9565574654376));
#68576=CARTESIAN_POINT('Ctrl Pts',(-19.5432790871468,-20.9082096920082,
-18.9609458783336));
#68577=CARTESIAN_POINT('Ctrl Pts',(-19.6105530555228,-20.8803786185101,
-18.96533665527));
#68578=CARTESIAN_POINT('Ctrl Pts',(-19.6764934757503,-20.849030254655,-18.9697274322063));
#68579=CARTESIAN_POINT('Ctrl Pts',(-19.7407097293466,-20.8143169764675,
-18.9741182091426));
#68580=CARTESIAN_POINT('Ctrl Pts',(-19.8047168405566,-20.7797167540474,
-18.9784946859989));
#68581=CARTESIAN_POINT('Ctrl Pts',(-19.8670105560363,-20.741773696628,-18.9828711628552));
#68582=CARTESIAN_POINT('Ctrl Pts',(-19.9272240703357,-20.7006867409492,
-18.9872476397115));
#68583=CARTESIAN_POINT('Ctrl Pts',(-19.987398312053,-20.6596265830891,-18.991621262133));
#68584=CARTESIAN_POINT('Ctrl Pts',(-20.0454946477979,-20.6154268676538,
-18.9959948845546));
#68585=CARTESIAN_POINT('Ctrl Pts',(-20.1011734566812,-20.5683309498201,
-19.0003685069761));
#68586=CARTESIAN_POINT('Ctrl Pts',(-20.1568343181235,-20.5212502128284,
-19.0047407196094));
#68587=CARTESIAN_POINT('Ctrl Pts',(-20.2100788325333,-20.4712754389994,
-19.0091129322427));
#68588=CARTESIAN_POINT('Ctrl Pts',(-20.2606001433951,-20.418690492976,-19.0134851448761));
#68589=CARTESIAN_POINT('Ctrl Pts',(-20.3114804596682,-20.36573187731,-19.0178884265368));
#68590=CARTESIAN_POINT('Ctrl Pts',(-20.3595983474391,-20.3101261777265,
-19.0222917081976));
#68591=CARTESIAN_POINT('Ctrl Pts',(-20.4046790961748,-20.2522001221368,
-19.0266949898584));
#68592=CARTESIAN_POINT('Ctrl Pts',(-20.4494793719813,-20.1946344574222,
-19.0310708762043));
#68593=CARTESIAN_POINT('Ctrl Pts',(-20.4912799489289,-20.1347776523353,
-19.0354467625502));
#68594=CARTESIAN_POINT('Ctrl Pts',(-20.5298538380763,-20.0729808170823,
-19.0398226488961));
#68595=CARTESIAN_POINT('Ctrl Pts',(-20.5687899660098,-20.0106036615382,
-19.0442396282143));
#68596=CARTESIAN_POINT('Ctrl Pts',(-20.6044382264007,-19.9462502770228,
-19.0486566075325));
#68597=CARTESIAN_POINT('Ctrl Pts',(-20.6366128839545,-19.8803066378144,
-19.0530735868507));
#68598=CARTESIAN_POINT('Ctrl Pts',(-20.6687875415084,-19.8143629986061,
-19.0574905661689));
#68599=CARTESIAN_POINT('Ctrl Pts',(-20.6974884458848,-19.7468295847188,
-19.0619075454871));
#68600=CARTESIAN_POINT('Ctrl Pts',(-20.7225805821191,-19.6781103693095,
-19.0663245248053));
#68601=CARTESIAN_POINT('',(-20.8509990913815,-18.9539458517612,-18.0890147820491));
#68602=CARTESIAN_POINT('Ctrl Pts',(-20.7225806288389,-19.6781102413592,
-18.845275429269));
#68603=CARTESIAN_POINT('Ctrl Pts',(-20.7113120014844,-19.7089713596775,
-18.8434821372632));
#68604=CARTESIAN_POINT('Ctrl Pts',(-20.6993214725324,-19.7395797295342,
-18.8416797662662));
#68605=CARTESIAN_POINT('Ctrl Pts',(-20.657531029883,-19.8393471149109,-18.8356908521596));
#68606=CARTESIAN_POINT('Ctrl Pts',(-20.6247651395845,-19.9071759854405,
-18.831436247592));
#68607=CARTESIAN_POINT('Ctrl Pts',(-20.5838855794443,-19.9814184507202,
-18.8264131589613));
#68608=CARTESIAN_POINT('Ctrl Pts',(-20.5792539165066,-19.9896979231735,
-18.8258476608105));
#68609=CARTESIAN_POINT('Ctrl Pts',(-20.5723045560486,-20.0019268191934,
-18.8250040650667));
#68610=CARTESIAN_POINT('Ctrl Pts',(-20.5700293673794,-20.0059004353672,
-18.8247286333159));
#68611=CARTESIAN_POINT('Ctrl Pts',(-20.5659565592962,-20.012960377082,-18.8242368678269));
#68612=CARTESIAN_POINT('Ctrl Pts',(-20.5641640033352,-20.0160495653639,
-18.8240208624185));
#68613=CARTESIAN_POINT('Ctrl Pts',(-20.5602911303876,-20.0226851128661,
-18.8235550902555));
#68614=CARTESIAN_POINT('Ctrl Pts',(-20.5582083279712,-20.0262299005994,
-18.8233051674174));
#68615=CARTESIAN_POINT('Ctrl Pts',(-20.552425525058,-20.0360065202143,-18.8226128731409));
#68616=CARTESIAN_POINT('Ctrl Pts',(-20.5487038691006,-20.042225384965,-18.8221691273205));
#68617=CARTESIAN_POINT('Ctrl Pts',(-20.5280540936028,-20.0763323439591,
-18.8197173080956));
#68618=CARTESIAN_POINT('Ctrl Pts',(-20.5105159779353,-20.1038437478274,
-18.8176726958952));
#68619=CARTESIAN_POINT('Ctrl Pts',(-20.4017833033109,-20.2660153666386,
-18.8052648011962));
#68620=CARTESIAN_POINT('Ctrl Pts',(-20.2959558676007,-20.3902042065759,
-18.7943130197274));
#68621=CARTESIAN_POINT('Ctrl Pts',(-20.0915015931583,-20.5806550692884,
-18.7760619429663));
#68622=CARTESIAN_POINT('Ctrl Pts',(-19.9995962833844,-20.6530590110026,
-18.7686228267474));
#68623=CARTESIAN_POINT('Ctrl Pts',(-19.8902556562268,-20.7254052083604,
-18.7606173743255));
#68624=CARTESIAN_POINT('Ctrl Pts',(-19.8782592711468,-20.7331692540876,
-18.7597494193885));
#68625=CARTESIAN_POINT('Ctrl Pts',(-19.8590411958269,-20.7453328706065,
-18.7583751378124));
#68626=CARTESIAN_POINT('Ctrl Pts',(-19.8518703300315,-20.7498115600863,
-18.7578658832841));
#68627=CARTESIAN_POINT('Ctrl Pts',(-19.8391760167595,-20.7576346975449,
-18.7569705122325));
#68628=CARTESIAN_POINT('Ctrl Pts',(-19.833663773786,-20.7609970356675,-18.756583739615));
#68629=CARTESIAN_POINT('Ctrl Pts',(-19.8222308215271,-20.7678992986477,
-18.7557856695663));
#68630=CARTESIAN_POINT('Ctrl Pts',(-19.8163080136316,-20.7714356127963,
-18.7553745075329));
#68631=CARTESIAN_POINT('Ctrl Pts',(-19.80106051524,-20.7804385928158,-18.7543217847417));
#68632=CARTESIAN_POINT('Ctrl Pts',(-19.7917109782977,-20.7858629512126,
-18.7536817653604));
#68633=CARTESIAN_POINT('Ctrl Pts',(-19.7525150524015,-20.8082039324084,
-18.7510209970589));
#68634=CARTESIAN_POINT('Ctrl Pts',(-19.7223002406934,-20.8244659627158,
-18.7490237792016));
#68635=CARTESIAN_POINT('Ctrl Pts',(-19.6425552346503,-20.8649174921721,
-18.7438794181247));
#68636=CARTESIAN_POINT('Ctrl Pts',(-19.5924513304059,-20.887920428399,-18.7407716695933));
#68637=CARTESIAN_POINT('Ctrl Pts',(-19.4404220406322,-20.9506530887483,
-18.7316269284304));
#68638=CARTESIAN_POINT('Ctrl Pts',(-19.3362576097056,-20.9844696611473,
-18.7257386640872));
#68639=CARTESIAN_POINT('Ctrl Pts',(-19.1852142672726,-21.0208673072533,
-18.7172798235204));
#68640=CARTESIAN_POINT('Ctrl Pts',(-19.1401428396125,-21.030185266342,-18.714763825996));
#68641=CARTESIAN_POINT('Ctrl Pts',(-19.0730020841226,-21.0417981189295,
-18.7109848868922));
#68642=CARTESIAN_POINT('Ctrl Pts',(-19.0511418440706,-21.0452270766129,
-18.7097496572829));
#68643=CARTESIAN_POINT('Ctrl Pts',(-18.9782520515958,-21.0554924490003,
-18.7056034796288));
#68644=CARTESIAN_POINT('Ctrl Pts',(-18.9270310870913,-21.0608095271028,
-18.7026453572159));
#68645=CARTESIAN_POINT('Ctrl Pts',(-18.8670519165732,-21.0648324182433,
-18.6990774396262));
#68646=CARTESIAN_POINT('Ctrl Pts',(-18.8584285431047,-21.0653577955407,
-18.6985619652811));
#68647=CARTESIAN_POINT('Ctrl Pts',(-18.8453432492029,-21.0660746496338,
-18.697775650207));
#68648=CARTESIAN_POINT('Ctrl Pts',(-18.8408834209665,-21.0663048211763,
-18.6975069263177));
#68649=CARTESIAN_POINT('Ctrl Pts',(-18.8328642341613,-21.0666932537225,
-18.6970223773891));
#68650=CARTESIAN_POINT('Ctrl Pts',(-18.829305178454,-21.0668566421357,-18.6968068425429));
#68651=CARTESIAN_POINT('Ctrl Pts',(-18.8215561841759,-21.0671927807098,
-18.6963365033543));
#68652=CARTESIAN_POINT('Ctrl Pts',(-18.817366193203,-21.0673620640641,-18.696081512834));
#68653=CARTESIAN_POINT('Ctrl Pts',(-18.8055578732189,-21.0678040042509,
-18.695361054302));
#68654=CARTESIAN_POINT('Ctrl Pts',(-18.7979386252067,-21.0680479582875,
-18.6948940263355));
#68655=CARTESIAN_POINT('Ctrl Pts',(-18.7515931440459,-21.0692813194536,
-18.6920408113324));
#68656=CARTESIAN_POINT('Ctrl Pts',(-18.7128496717674,-21.0692486698572,
-18.6896029164142));
#68657=CARTESIAN_POINT('Ctrl Pts',(-18.5834887913314,-21.0655889202006,
-18.6813341067842));
#68658=CARTESIAN_POINT('Ctrl Pts',(-18.4931095474332,-21.0572034424621,
-18.675349326038));
#68659=CARTESIAN_POINT('Ctrl Pts',(-18.3372563683629,-21.0325740657137,
-18.6649223481402));
#68660=CARTESIAN_POINT('Ctrl Pts',(-18.2714938439103,-21.0189500604532,
-18.660487904005));
#68661=CARTESIAN_POINT('Ctrl Pts',(-18.0953526853012,-20.9736298699137,
-18.648616843998));
#68662=CARTESIAN_POINT('Ctrl Pts',(-17.9867127657187,-20.9360430775046,
-18.6413129705392));
#68663=CARTESIAN_POINT('Ctrl Pts',(-17.8685879973835,-20.8840855037306,
-18.6334336929697));
#68664=CARTESIAN_POINT('Ctrl Pts',(-17.8555936246965,-20.8782124969595,
-18.6325675657634));
#68665=CARTESIAN_POINT('Ctrl Pts',(-17.8349986264041,-20.8686525146428,
-18.631195622191));
#68666=CARTESIAN_POINT('Ctrl Pts',(-17.8273591882732,-20.8650506457892,
-18.6306868934148));
#68667=CARTESIAN_POINT('Ctrl Pts',(-17.813919146972,-20.8586152980352,-18.6297921337245));
#68668=CARTESIAN_POINT('Ctrl Pts',(-17.8081096039757,-20.8558008422081,
-18.6294054495358));
#68669=CARTESIAN_POINT('Ctrl Pts',(-17.7961156771543,-20.8499224507735,
-18.6286072618506));
#68670=CARTESIAN_POINT('Ctrl Pts',(-17.7899332142322,-20.8468547537831,
-18.6281958952319));
#68671=CARTESIAN_POINT('Ctrl Pts',(-17.7740927191565,-20.8388980335203,
-18.6271420265877));
#68672=CARTESIAN_POINT('Ctrl Pts',(-17.7644569079766,-20.8339650304978,
-18.6265010725312));
#68673=CARTESIAN_POINT('Ctrl Pts',(-17.7243188539029,-20.8130264692688,
-18.6238312039699));
#68674=CARTESIAN_POINT('Ctrl Pts',(-17.6941707057632,-20.796351044109,-18.6218260264653));
#68675=CARTESIAN_POINT('Ctrl Pts',(-17.616617273751,-20.7509485536852,-18.6166565084999));
#68676=CARTESIAN_POINT('Ctrl Pts',(-17.5699085705251,-20.7210822067612,
-18.6135320699503));
#68677=CARTESIAN_POINT('Ctrl Pts',(-17.434470496904,-20.6267911356964,-18.6043582237157));
#68678=CARTESIAN_POINT('Ctrl Pts',(-17.3495148293822,-20.5572737907738,
-18.5984574440118));
#68679=CARTESIAN_POINT('Ctrl Pts',(-17.2253041719961,-20.4384080444049,
-18.5890958148823));
#68680=CARTESIAN_POINT('Ctrl Pts',(-17.1822100864807,-20.3933602271417,
-18.585682958005));
#68681=CARTESIAN_POINT('Ctrl Pts',(-17.104104148923,-20.304144414272,-18.5790303522828));
#68682=CARTESIAN_POINT('Ctrl Pts',(-17.0687465329632,-20.2603519082761,
-18.5758083529987));
#68683=CARTESIAN_POINT('Ctrl Pts',(-17.0299078677744,-20.2081198272265,
-18.5719466220178));
#68684=CARTESIAN_POINT('Ctrl Pts',(-17.0246819733804,-20.200999156603,-18.5714197689891));
#68685=CARTESIAN_POINT('Ctrl Pts',(-17.0168568449586,-20.1901957443923,
-18.5706194961107));
#68686=CARTESIAN_POINT('Ctrl Pts',(-17.0142244882095,-20.1865369595597,
-18.570348307424));
#68687=CARTESIAN_POINT('Ctrl Pts',(-17.0095307140478,-20.1799688089324,
-18.569861135059));
#68688=CARTESIAN_POINT('Ctrl Pts',(-17.0074649452116,-20.1770626180777,
-18.5696454556193));
#68689=CARTESIAN_POINT('Ctrl Pts',(-17.003003953687,-20.1707530542269,-18.5691769229234));
#68690=CARTESIAN_POINT('Ctrl Pts',(-17.0006114540789,-20.1673478793003,
-18.5689238950526));
#68691=CARTESIAN_POINT('Ctrl Pts',(-16.993948598028,-20.1578051353874,-18.568214386248));
#68692=CARTESIAN_POINT('Ctrl Pts',(-16.9897007434413,-20.1516520352862,
-18.5677564187599));
#68693=CARTESIAN_POINT('Ctrl Pts',(-16.9650726556814,-20.1155704208854,
-18.5650687277761));
#68694=CARTESIAN_POINT('Ctrl Pts',(-16.9454316630597,-20.0851473932677,
-18.5627938810971));
#68695=CARTESIAN_POINT('Ctrl Pts',(-16.8845095968982,-19.9852491355776,
-18.555333839777));
#68696=CARTESIAN_POINT('Ctrl Pts',(-16.8464245338091,-19.9139124956362,
-18.5500237818227));
#68697=CARTESIAN_POINT('Ctrl Pts',(-16.7350527949056,-19.6730792752924,
-18.5325039700128));
#68698=CARTESIAN_POINT('Ctrl Pts',(-16.6798106516438,-19.4961310049149,
-18.5203486591922));
#68699=CARTESIAN_POINT('Ctrl Pts',(-16.6444211093995,-19.2923560817245,
-18.507628026634));
#68700=CARTESIAN_POINT('Ctrl Pts',(-16.6409655354423,-19.2704163807884,
-18.5062729822592));
#68701=CARTESIAN_POINT('Ctrl Pts',(-16.6366690847654,-19.2400344645843,
-18.5044159417195));
#68702=CARTESIAN_POINT('Ctrl Pts',(-16.6355328265435,-19.2316360956322,
-18.5039046447781));
#68703=CARTESIAN_POINT('Ctrl Pts',(-16.6336677699776,-19.2171990121298,
-18.5030291452845));
#68704=CARTESIAN_POINT('Ctrl Pts',(-16.6329145149182,-19.211163612579,-18.5026641739058));
#68705=CARTESIAN_POINT('Ctrl Pts',(-16.6314164406909,-19.198724416687,-18.5019140428557));
#68706=CARTESIAN_POINT('Ctrl Pts',(-16.6306748418307,-19.1923202906492,
-18.5015289884933));
#68707=CARTESIAN_POINT('Ctrl Pts',(-16.629019016596,-19.1774262016551,-18.5006360669791));
#68708=CARTESIAN_POINT('Ctrl Pts',(-16.6281268752855,-19.1689338580068,
-18.5001289006083));
#68709=CARTESIAN_POINT('Ctrl Pts',(-16.6254426100705,-19.1418033628106,
-18.498514751802));
#68710=CARTESIAN_POINT('Ctrl Pts',(-16.6238463273348,-19.1231464117051,
-18.4974139260147));
#68711=CARTESIAN_POINT('Ctrl Pts',(-16.6207021656623,-19.0796041267272,
-18.4948646782173));
#68712=CARTESIAN_POINT('Ctrl Pts',(-16.6193459403488,-19.0547075029223,
-18.4934221991562));
#68713=CARTESIAN_POINT('Ctrl Pts',(-16.6161240824696,-18.9670883485719,
-18.4883922207389));
#68714=CARTESIAN_POINT('Ctrl Pts',(-16.6166071118363,-18.904310285101,-18.4848732209941));
#68715=CARTESIAN_POINT('Ctrl Pts',(-16.6251112675776,-18.7413959343469,
-18.4758544023313));
#68716=CARTESIAN_POINT('Ctrl Pts',(-16.6374678711437,-18.6416465530865,
-18.4704480962761));
#68717=CARTESIAN_POINT('Ctrl Pts',(-16.6712069353561,-18.4702362445365,
-18.4609310074807));
#68718=CARTESIAN_POINT('Ctrl Pts',(-16.6893873909543,-18.3981323554564,
-18.4568528280256));
#68719=CARTESIAN_POINT('Ctrl Pts',(-16.7240800811799,-18.2858318337492,
-18.4501826082381));
#68720=CARTESIAN_POINT('Ctrl Pts',(-16.7381023266811,-18.2449285683577,
-18.4476835083764));
#68721=CARTESIAN_POINT('Ctrl Pts',(-16.756014289516,-18.1974684920272,-18.4446701367022));
#68722=CARTESIAN_POINT('Ctrl Pts',(-16.7587001891292,-18.1904647606305,
-18.4442224990094));
#68723=CARTESIAN_POINT('Ctrl Pts',(-16.7631007724207,-18.1791697540896,
-18.4434955822653));
#68724=CARTESIAN_POINT('Ctrl Pts',(-16.7647924122323,-18.1748694899721,
-18.443217650574));
#68725=CARTESIAN_POINT('Ctrl Pts',(-16.7678180275156,-18.1672514810208,
-18.4427231382059));
#68726=CARTESIAN_POINT('Ctrl Pts',(-16.7691463436995,-18.1639315409957,
-18.442506900023));
#68727=CARTESIAN_POINT('Ctrl Pts',(-16.7720098480995,-18.1568268588732,
-18.4420425691746));
#68728=CARTESIAN_POINT('Ctrl Pts',(-16.7735475558735,-18.1530432463576,
-18.4417943306171));
#68729=CARTESIAN_POINT('Ctrl Pts',(-16.7777974175703,-18.1426723750164,
-18.4411113243718));
#68730=CARTESIAN_POINT('Ctrl Pts',(-16.7805318585027,-18.1360943897149,
-18.4406752412043));
#68731=CARTESIAN_POINT('Ctrl Pts',(-16.7952897290834,-18.1010922591209,
-18.4383399539933));
#68732=CARTESIAN_POINT('Ctrl Pts',(-16.8078997887866,-18.072921367308,-18.4364081065725));
#68733=CARTESIAN_POINT('Ctrl Pts',(-16.8478987707588,-17.9885592467277,
-18.4304848560207));
#68734=CARTESIAN_POINT('Ctrl Pts',(-16.8771637006213,-17.9332979839508,
-18.4264164714451));
#68735=CARTESIAN_POINT('Ctrl Pts',(-16.9237407496424,-17.8540397004061,
-18.4203757142423));
#68736=CARTESIAN_POINT('Ctrl Pts',(-16.9391811343044,-17.8289770377254,
-18.4184335686013));
#68737=CARTESIAN_POINT('Ctrl Pts',(-17.0519720908878,-17.6541667271171,
-18.4046906165094));
#68738=CARTESIAN_POINT('Ctrl Pts',(-17.167429798326,-17.5169140828983,-18.3929511552596));
#68739=CARTESIAN_POINT('Ctrl Pts',(-17.3154944095117,-17.3803613025191,
-18.3805564180322));
#68740=CARTESIAN_POINT('Ctrl Pts',(-17.3324618116889,-17.365211710495,-18.379168173424));
#68741=CARTESIAN_POINT('Ctrl Pts',(-17.3568622310037,-17.3441222307585,
-18.3772159864981));
#68742=CARTESIAN_POINT('Ctrl Pts',(-17.364095737645,-17.337954872933,-18.3766426264557));
#68743=CARTESIAN_POINT('Ctrl Pts',(-17.375931476834,-17.3280004921146,-18.3757130708945));
#68744=CARTESIAN_POINT('Ctrl Pts',(-17.3805085345386,-17.3241838650271,
-18.3753556629683));
#68745=CARTESIAN_POINT('Ctrl Pts',(-17.3901352674176,-17.3162251882643,
-18.3746082251605));
#68746=CARTESIAN_POINT('Ctrl Pts',(-17.3951881235144,-17.3120870708959,
-18.3742183576119));
#68747=CARTESIAN_POINT('Ctrl Pts',(-17.4072768174534,-17.302279952568,-18.3732913778916));
#68748=CARTESIAN_POINT('Ctrl Pts',(-17.4143299943915,-17.2966324522461,
-18.3727551359065));
#68749=CARTESIAN_POINT('Ctrl Pts',(-17.4383218841956,-17.2776728695598,
-18.3709463729434));
#68750=CARTESIAN_POINT('Ctrl Pts',(-17.4554279173697,-17.2645739721611,
-18.3696823296548));
#68751=CARTESIAN_POINT('Ctrl Pts',(-17.5503688680766,-17.1941459748197,
-18.3627999857183));
#68752=CARTESIAN_POINT('Ctrl Pts',(-17.6318643975335,-17.1419354394404,
-18.3573829234189));
#68753=CARTESIAN_POINT('Ctrl Pts',(-17.8504842710984,-17.0221350728713,
-18.3436780779384));
#68754=CARTESIAN_POINT('Ctrl Pts',(-17.9918426882678,-16.9634893468507,
-18.3356006764855));
#68755=CARTESIAN_POINT('Ctrl Pts',(-18.1878327932578,-16.9060140012061,
-18.3240979319656));
#68756=CARTESIAN_POINT('Ctrl Pts',(-18.2379123479768,-16.8932981195625,
-18.3211302723438));
#68757=CARTESIAN_POINT('Ctrl Pts',(-18.2968551847896,-16.8806071889227,
-18.317551744146));
#68758=CARTESIAN_POINT('Ctrl Pts',(-18.3053191833905,-16.8788390031324,
-18.3170358364379));
#68759=CARTESIAN_POINT('Ctrl Pts',(-18.3181721130978,-16.8762360138858,
-18.3162489893915));
#68760=CARTESIAN_POINT('Ctrl Pts',(-18.3225533635816,-16.8753631463077,
-18.3159801711957));
#68761=CARTESIAN_POINT('Ctrl Pts',(-18.3304337895588,-16.873819062592,-18.3154955225473));
#68762=CARTESIAN_POINT('Ctrl Pts',(-18.3339319222591,-16.8731428072905,
-18.315279982826));
#68763=CARTESIAN_POINT('Ctrl Pts',(-18.3415497639809,-16.8716900743654,
-18.3148097157304));
#68764=CARTESIAN_POINT('Ctrl Pts',(-18.3456700244796,-16.870917011781,-18.3145548026325));
#68765=CARTESIAN_POINT('Ctrl Pts',(-18.3572834573702,-16.8687737348109,
-18.3138347771251));
#68766=CARTESIAN_POINT('Ctrl Pts',(-18.3647816792995,-16.867431734609,-18.3133681076938));
#68767=CARTESIAN_POINT('Ctrl Pts',(-18.4094321068722,-16.8596888509005,
-18.3105792426965));
#68768=CARTESIAN_POINT('Ctrl Pts',(-18.4467402320654,-16.8542412717936,
-18.3082081649991));
#68769=CARTESIAN_POINT('Ctrl Pts',(-18.5704103869233,-16.8395441557004,
-18.3002571137243));
#68770=CARTESIAN_POINT('Ctrl Pts',(-18.6571933006942,-16.8346124412187,
-18.2945346038622));
#68771=CARTESIAN_POINT('Ctrl Pts',(-18.9147598837674,-16.8358324561702,
-18.2775169135569));
#68772=CARTESIAN_POINT('Ctrl Pts',(-19.084801403749,-16.857292691771,-18.2662989567347));
#68773=CARTESIAN_POINT('Ctrl Pts',(-19.2762097564064,-16.9054409816596,
-18.2541083349811));
#68774=CARTESIAN_POINT('Ctrl Pts',(-19.3018584799974,-16.9124088441307,
-18.2524823509199));
#68775=CARTESIAN_POINT('Ctrl Pts',(-19.3370961451349,-16.9226979772032,
-18.2502580194705));
#68776=CARTESIAN_POINT('Ctrl Pts',(-19.3468017509425,-16.9256077182263,
-18.2496463689467));
#68777=CARTESIAN_POINT('Ctrl Pts',(-19.3622940292873,-16.9303737893198,
-18.2486715527861));
#68778=CARTESIAN_POINT('Ctrl Pts',(-19.36809415871,-16.9321855228674,-18.2483069334462));
#68779=CARTESIAN_POINT('Ctrl Pts',(-19.3800345708687,-16.9359717429511,
-18.2475569834793));
#68780=CARTESIAN_POINT('Ctrl Pts',(-19.3861737973517,-16.937949370188,-18.2471717605544));
#68781=CARTESIAN_POINT('Ctrl Pts',(-19.4004378523211,-16.942616305479,-18.2462775337754));
#68782=CARTESIAN_POINT('Ctrl Pts',(-19.4085556385679,-16.9453268984285,
-18.2457692371758));
#68783=CARTESIAN_POINT('Ctrl Pts',(-19.4330556420134,-16.9536731153638,
-18.2442368731848));
#68784=CARTESIAN_POINT('Ctrl Pts',(-19.4493855825662,-16.9594607599333,
-18.2432178346807));
#68785=CARTESIAN_POINT('Ctrl Pts',(-19.4876382795282,-16.9735491517817,
-18.2408350647805));
#68786=CARTESIAN_POINT('Ctrl Pts',(-19.5094980762103,-16.9820149212567,
-18.2394767974568));
#68787=CARTESIAN_POINT('Ctrl Pts',(-19.5843781190441,-17.0124537643067,
-18.2348305730171));
#68788=CARTESIAN_POINT('Ctrl Pts',(-19.6366445080963,-17.0362191793076,
-18.2315996158654));
#68789=CARTESIAN_POINT('Ctrl Pts',(-19.7978121302769,-17.1175640011375,
-18.2215795037399));
#68790=CARTESIAN_POINT('Ctrl Pts',(-19.9026884797029,-17.1825314089948,
-18.2149861629799));
#68791=CARTESIAN_POINT('Ctrl Pts',(-20.0821187421126,-17.3166288804899,
-18.2027317641182));
#68792=CARTESIAN_POINT('Ctrl Pts',(-20.1584847322518,-17.3827005773451,
-18.1971273731389));
#68793=CARTESIAN_POINT('Ctrl Pts',(-20.2367001191189,-17.4608007143964,
-18.1905789943473));
#68794=CARTESIAN_POINT('Ctrl Pts',(-20.2435120032152,-17.4676966410243,
-18.190001369143));
#68795=CARTESIAN_POINT('Ctrl Pts',(-20.2534996574553,-17.4779473795998,
-18.1891431228434));
#68796=CARTESIAN_POINT('Ctrl Pts',(-20.2567122996807,-17.481266309562,-18.1888653037972));
#68797=CARTESIAN_POINT('Ctrl Pts',(-20.26239251635,-17.4871730131163,-18.1883709157996));
#68798=CARTESIAN_POINT('Ctrl Pts',(-20.2648644238387,-17.4897565520224,
-18.1881546887043));
#68799=CARTESIAN_POINT('Ctrl Pts',(-20.2701466396751,-17.4953053883241,
-18.1876902956425));
#68800=CARTESIAN_POINT('Ctrl Pts',(-20.2729548709297,-17.4982725169895,
-18.1874419833355));
#68801=CARTESIAN_POINT('Ctrl Pts',(-20.2787001087953,-17.5043781397853,
-18.1869310788197));
#68802=CARTESIAN_POINT('Ctrl Pts',(-20.2816361788512,-17.5075174859291,
-18.1866684185065));
#68803=CARTESIAN_POINT('Ctrl Pts',(-20.2950866022405,-17.5219872201699,
-18.1854580198056));
#68804=CARTESIAN_POINT('Ctrl Pts',(-20.3054859071369,-17.5334232689213,
-18.184502075058));
#68805=CARTESIAN_POINT('Ctrl Pts',(-20.3737946210223,-17.6102148361597,
-18.1780936618964));
#68806=CARTESIAN_POINT('Ctrl Pts',(-20.4277326240544,-17.6789797776092,
-18.1724087601117));
#68807=CARTESIAN_POINT('Ctrl Pts',(-20.5185471941585,-17.8107839014612,
-18.1618727497343));
#68808=CARTESIAN_POINT('Ctrl Pts',(-20.5567126316442,-17.8727865441772,
-18.1570468443867));
#68809=CARTESIAN_POINT('Ctrl Pts',(-20.5938784842887,-17.9407812358528,
-18.1519508018364));
#68810=CARTESIAN_POINT('Ctrl Pts',(-20.596132823833,-17.9449385758964,-18.1516399652404));
#68811=CARTESIAN_POINT('Ctrl Pts',(-20.6621274724152,-18.0676218725202,
-18.1424894559388));
#68812=CARTESIAN_POINT('Ctrl Pts',(-20.7144446144191,-18.1919664245569,
-18.1338570828094));
#68813=CARTESIAN_POINT('Ctrl Pts',(-20.7593064019422,-18.3355007146892,
-18.1246738597621));
#68814=CARTESIAN_POINT('Ctrl Pts',(-20.7638400038434,-18.350595834386,-18.1237169480434));
#68815=CARTESIAN_POINT('Ctrl Pts',(-20.7704400293477,-18.3734966198158,
-18.1222782877187));
#68816=CARTESIAN_POINT('Ctrl Pts',(-20.7726309949981,-18.3812655406726,
-18.1217924912484));
#68817=CARTESIAN_POINT('Ctrl Pts',(-20.7764755741626,-18.3952026350265,
-18.1209249741425));
#68818=CARTESIAN_POINT('Ctrl Pts',(-20.778145804565,-18.4013660855376,-18.1205427172853));
#68819=CARTESIAN_POINT('Ctrl Pts',(-20.7816287326791,-18.4144529871121,
-18.1197339702438));
#68820=CARTESIAN_POINT('Ctrl Pts',(-20.7834342647165,-18.4213782755158,
-18.1193077164557));
#68821=CARTESIAN_POINT('Ctrl Pts',(-20.7870376484727,-18.4354921883167,
-18.1184424317947));
#68822=CARTESIAN_POINT('Ctrl Pts',(-20.7888329462385,-18.4426813661912,
-18.1180034881602));
#68823=CARTESIAN_POINT('Ctrl Pts',(-20.7932123904979,-18.4606187545168,
-18.116912704427));
#68824=CARTESIAN_POINT('Ctrl Pts',(-20.7957501857015,-18.4713781359163,
-18.1162623491113));
#68825=CARTESIAN_POINT('Ctrl Pts',(-20.8334344639406,-18.6369398937002,
-18.1063131487805));
#68826=CARTESIAN_POINT('Ctrl Pts',(-20.8511450347541,-18.7951910216362,
-18.0976370133688));
#68827=CARTESIAN_POINT('Ctrl Pts',(-20.8509991056242,-18.9539459667055,
-18.0890147524363));
#68828=CARTESIAN_POINT('Ctrl Pts',(-20.850999105731,-18.9539458505088,-18.0890147587472));
#68829=CARTESIAN_POINT('Ctrl Pts',(-20.8508677551986,-19.096849407723,-18.0812534146201));
#68830=CARTESIAN_POINT('Ctrl Pts',(-20.8362671717255,-19.2393578459244,
-18.0735575723068));
#68831=CARTESIAN_POINT('Ctrl Pts',(-20.8054602106998,-19.3888487512122,
-18.0645864802766));
#68832=CARTESIAN_POINT('Ctrl Pts',(-20.8034244703069,-19.3983928649445,
-18.0640096594921));
#68833=CARTESIAN_POINT('Ctrl Pts',(-20.8001174997201,-19.4133879088025,
-18.0630965012489));
#68834=CARTESIAN_POINT('Ctrl Pts',(-20.798890487582,-19.4188485811966,-18.0627625166399));
#68835=CARTESIAN_POINT('Ctrl Pts',(-20.7965251623351,-19.4291834111655,
-18.0621275712305));
#68836=CARTESIAN_POINT('Ctrl Pts',(-20.7953911859381,-19.4340585343316,
-18.0618268523904));
#68837=CARTESIAN_POINT('Ctrl Pts',(-20.7934048894696,-19.4424627223062,
-18.0613062949401));
#68838=CARTESIAN_POINT('Ctrl Pts',(-20.7925607517554,-19.4459937367306,
-18.0610869260083));
#68839=CARTESIAN_POINT('Ctrl Pts',(-20.7909045652851,-19.4528435715514,
-18.0606600682991));
#68840=CARTESIAN_POINT('Ctrl Pts',(-20.7900935636639,-19.4561626036618,
-18.0604526460464));
#68841=CARTESIAN_POINT('Ctrl Pts',(-20.7878796790763,-19.465128757864,-18.0598907349418));
#68842=CARTESIAN_POINT('Ctrl Pts',(-20.7864615546186,-19.470772033985,-18.0595353804882));
#68843=CARTESIAN_POINT('Ctrl Pts',(-20.7810870793073,-19.4917921744127,
-18.0582056344514));
#68844=CARTESIAN_POINT('Ctrl Pts',(-20.7769811537,-19.5071297803452,-18.0572231410393));
#68845=CARTESIAN_POINT('Ctrl Pts',(-20.7579998303821,-19.5749698604786,
-18.052827473929));
#68846=CARTESIAN_POINT('Ctrl Pts',(-20.7412777861463,-19.626904783481,-18.049329319184));
#68847=CARTESIAN_POINT('Ctrl Pts',(-20.7225806448396,-19.6781101975385,
-18.0457833736847));
#68848=CARTESIAN_POINT('Origin',(-18.734,-18.952,0.));
#68849=CARTESIAN_POINT('',(-20.7225805822089,-19.6781103690637,-17.242699000807));
#68850=CARTESIAN_POINT('',(-20.7225805818549,-19.6781103700332,-17.4677765722177));
#68851=CARTESIAN_POINT('',(-20.7225805821191,-19.6781103693095,0.));
#68852=CARTESIAN_POINT('Ctrl Pts',(-20.7225805818549,-19.6781103700332,
-17.4677765722177));
#68853=CARTESIAN_POINT('Ctrl Pts',(-20.7401854861152,-19.6298962524523,
-17.471069514147));
#68854=CARTESIAN_POINT('Ctrl Pts',(-20.7560325913588,-19.5810537941813,
-17.474316044063));
#68855=CARTESIAN_POINT('Ctrl Pts',(-20.7795153229111,-19.4985720222208,
-17.4796471969592));
#68856=CARTESIAN_POINT('Ctrl Pts',(-20.7881324598313,-19.4652387044823,
-17.4817615361231));
#68857=CARTESIAN_POINT('Ctrl Pts',(-20.7983855430847,-19.4211678249985,
-17.4845062026776));
#68858=CARTESIAN_POINT('Ctrl Pts',(-20.8007569917464,-19.4106083976442,
-17.4851600453581));
#68859=CARTESIAN_POINT('Ctrl Pts',(-20.8045078951291,-19.3932863925522,
-17.4862265621788));
#68860=CARTESIAN_POINT('Ctrl Pts',(-20.8059354161732,-19.3865345291287,
-17.4866407714016));
#68861=CARTESIAN_POINT('Ctrl Pts',(-20.8086343585082,-19.3734533809918,
-17.4874404011248));
#68862=CARTESIAN_POINT('Ctrl Pts',(-20.8099098928274,-19.3671250319341,
-17.4878259492365));
#68863=CARTESIAN_POINT('Ctrl Pts',(-20.8127876275962,-19.3525026283939,
-17.4887138658021));
#68864=CARTESIAN_POINT('Ctrl Pts',(-20.8143691793209,-19.3442045854958,
-17.4892155706158));
#68865=CARTESIAN_POINT('Ctrl Pts',(-20.8184877290584,-19.321869406054,-17.4905602545672));
#68866=CARTESIAN_POINT('Ctrl Pts',(-20.8209326204345,-19.3078155740382,
-17.4914003056032));
#68867=CARTESIAN_POINT('Ctrl Pts',(-20.8418093117342,-19.1801846375292,
-17.4989769688998));
#68868=CARTESIAN_POINT('Ctrl Pts',(-20.8510962905051,-19.0652992221111,
-17.5054071708765));
#68869=CARTESIAN_POINT('Ctrl Pts',(-20.8508421940714,-18.7639639427916,
-17.5219135939307));
#68870=CARTESIAN_POINT('Ctrl Pts',(-20.8261075481732,-18.5785810131941,
-17.5316811786551));
#68871=CARTESIAN_POINT('Ctrl Pts',(-20.7737437540389,-18.3851344241272,
-17.5434581358864));
#68872=CARTESIAN_POINT('Ctrl Pts',(-20.7698906309289,-18.3714481266278,
-17.5443005254895));
#68873=CARTESIAN_POINT('Ctrl Pts',(-20.7643392700289,-18.3524648712353,
-17.5454830647105));
#68874=CARTESIAN_POINT('Ctrl Pts',(-20.7627574775413,-18.3471338844243,
-17.5458167097691));
#68875=CARTESIAN_POINT('Ctrl Pts',(-20.7601843572634,-18.3385855526011,
-17.5463543107302));
#68876=CARTESIAN_POINT('Ctrl Pts',(-20.7592063133516,-18.33536419023,-17.5465574940822));
#68877=CARTESIAN_POINT('Ctrl Pts',(-20.757146922833,-18.3286389689199,-17.5469829456692));
#68878=CARTESIAN_POINT('Ctrl Pts',(-20.7560641559174,-18.3251355847886,
-17.5472052993924));
#68879=CARTESIAN_POINT('Ctrl Pts',(-20.7534222731797,-18.3166656150336,
-17.5477445943649));
#68880=CARTESIAN_POINT('Ctrl Pts',(-20.7518539351081,-18.3117019495744,
-17.5480620717639));
#68881=CARTESIAN_POINT('Ctrl Pts',(-20.7463005713028,-18.2943490398617,
-17.5491768673399));
#68882=CARTESIAN_POINT('Ctrl Pts',(-20.7422197140405,-18.2819910930458,
-17.5499795316202));
#68883=CARTESIAN_POINT('Ctrl Pts',(-20.7174287695851,-18.2091790822462,
-17.5547574141077));
#68884=CARTESIAN_POINT('Ctrl Pts',(-20.694105627527,-18.1496553270635,-17.5588616249813));
#68885=CARTESIAN_POINT('Ctrl Pts',(-20.5919079167676,-17.920005290123,-17.5752529078129));
#68886=CARTESIAN_POINT('Ctrl Pts',(-20.4932542179064,-17.7595743407234,
-17.5878515668483));
#68887=CARTESIAN_POINT('Ctrl Pts',(-20.3393459548716,-17.5708073277645,
-17.6032549052734));
#68888=CARTESIAN_POINT('Ctrl Pts',(-20.3022245158644,-17.5287988102026,
-17.6067354644614));
#68889=CARTESIAN_POINT('Ctrl Pts',(-20.255157559347,-17.4796164013013,-17.6108793950905));
#68890=CARTESIAN_POINT('Ctrl Pts',(-20.2467641838835,-17.4709941541593,
-17.6116086314705));
#68891=CARTESIAN_POINT('Ctrl Pts',(-20.2327633598476,-17.456854770822,-17.6128092320561));
#68892=CARTESIAN_POINT('Ctrl Pts',(-20.2271979436423,-17.4512965753145,
-17.61328242557));
#68893=CARTESIAN_POINT('Ctrl Pts',(-20.2170712612416,-17.4412951387361,
-17.6141361980115));
#68894=CARTESIAN_POINT('Ctrl Pts',(-20.2125207008507,-17.4368412352841,
-17.6145172454367));
#68895=CARTESIAN_POINT('Ctrl Pts',(-20.202714665704,-17.4273297313886,-17.6153328385272));
#68896=CARTESIAN_POINT('Ctrl Pts',(-20.197452997426,-17.4222786124235,-17.615767098652));
#68897=CARTESIAN_POINT('Ctrl Pts',(-20.1830323070875,-17.4085774787785,
-17.6169482259019));
#68898=CARTESIAN_POINT('Ctrl Pts',(-20.1738219181304,-17.3999817783296,
-17.6176927481422));
#68899=CARTESIAN_POINT('Ctrl Pts',(-20.1246868229696,-17.3549397587563,
-17.6216138226633));
#68900=CARTESIAN_POINT('Ctrl Pts',(-20.0834517989649,-17.3199485854839,
-17.624728530735));
#68901=CARTESIAN_POINT('Ctrl Pts',(-19.8904575622519,-17.1684992483461,
-17.6386248336708));
#68902=CARTESIAN_POINT('Ctrl Pts',(-19.7247043987413,-17.0713702819603,
-17.6486489049994));
#68903=CARTESIAN_POINT('Ctrl Pts',(-19.5328954563912,-16.9914570081762,
-17.6601999008382));
#68904=CARTESIAN_POINT('Ctrl Pts',(-19.5175481405615,-16.9852730071484,
-17.6611244838335));
#68905=CARTESIAN_POINT('Ctrl Pts',(-19.4525654555233,-16.9599704292826,
-17.6650467943258));
#68906=CARTESIAN_POINT('Ctrl Pts',(-19.4022953006937,-16.9425477103398,
-17.668099220139));
#68907=CARTESIAN_POINT('Ctrl Pts',(-19.3430953509111,-16.9244971691108,
-17.6717720662578));
#68908=CARTESIAN_POINT('Ctrl Pts',(-19.3347479435923,-16.9220081827417,
-17.6722917359694));
#68909=CARTESIAN_POINT('Ctrl Pts',(-19.3220834208956,-16.9183168951466,
-17.6730831997672));
#68910=CARTESIAN_POINT('Ctrl Pts',(-19.3177773400454,-16.9170766360133,
-17.6733528351883));
#68911=CARTESIAN_POINT('Ctrl Pts',(-19.3100396639071,-16.9148745726947,
-17.6738383501984));
#68912=CARTESIAN_POINT('Ctrl Pts',(-19.3066095517231,-16.9139077543091,
-17.6740539343943));
#68913=CARTESIAN_POINT('Ctrl Pts',(-19.2991494813891,-16.911825363292,-17.6745235868459));
#68914=CARTESIAN_POINT('Ctrl Pts',(-19.295118707193,-16.9107130823128,-17.6747778369294));
#68915=CARTESIAN_POINT('Ctrl Pts',(-19.2837834659244,-16.9076212643585,
-17.6754941578965));
#68916=CARTESIAN_POINT('Ctrl Pts',(-19.2764717266792,-16.9056689671687,
-17.6759577608106));
#68917=CARTESIAN_POINT('Ctrl Pts',(-19.2326183085346,-16.8942112758065,
-17.6787468758586));
#68918=CARTESIAN_POINT('Ctrl Pts',(-19.1958405304369,-16.8856463111251,
-17.6811214910051));
#68919=CARTESIAN_POINT('Ctrl Pts',(-19.0738764096172,-16.8606612779821,
-17.68906959481));
#68920=CARTESIAN_POINT('Ctrl Pts',(-18.9879122289604,-16.8484933339368,
-17.6947851606618));
#68921=CARTESIAN_POINT('Ctrl Pts',(-18.7261823111601,-16.8277259621054,
-17.7121319592443));
#68922=CARTESIAN_POINT('Ctrl Pts',(-18.5498275851324,-16.835704789497,-17.7236766568872));
#68923=CARTESIAN_POINT('Ctrl Pts',(-18.3538340284923,-16.8692877840743,
-17.7359159094666));
#68924=CARTESIAN_POINT('Ctrl Pts',(-18.3312639400846,-16.8735342024731,
-17.7373177514194));
#68925=CARTESIAN_POINT('Ctrl Pts',(-18.2994195019062,-16.8800637476046,
-17.7392855358154));
#68926=CARTESIAN_POINT('Ctrl Pts',(-18.2900852584993,-16.8820435390437,
-17.7398611017316));
#68927=CARTESIAN_POINT('Ctrl Pts',(-18.2749369402658,-16.8853636748998,
-17.740793252841));
#68928=CARTESIAN_POINT('Ctrl Pts',(-18.2691146619857,-16.8866655920486,
-17.7411510639488));
#68929=CARTESIAN_POINT('Ctrl Pts',(-18.2569360423183,-16.8894429562582,
-17.7418985679055));
#68930=CARTESIAN_POINT('Ctrl Pts',(-18.2505808540461,-16.8909232160826,
-17.74228810183));
#68931=CARTESIAN_POINT('Ctrl Pts',(-18.2354732429854,-16.894515823417,-17.7432128746599));
#68932=CARTESIAN_POINT('Ctrl Pts',(-18.2267272065016,-16.8966546808044,
-17.7437472544271));
#68933=CARTESIAN_POINT('Ctrl Pts',(-18.197284262263,-16.9040543846259,-17.7455430827491));
#68934=CARTESIAN_POINT('Ctrl Pts',(-18.176652961178,-16.909572680828,-17.7467962201684));
#68935=CARTESIAN_POINT('Ctrl Pts',(-18.0646398377423,-16.9413568062523,
-17.7535764826653));
#68936=CARTESIAN_POINT('Ctrl Pts',(-17.975018359019,-16.9734452245979,-17.7589092896504));
#68937=CARTESIAN_POINT('Ctrl Pts',(-17.7316741726181,-17.0795524129059,
-17.7735143763218));
#68938=CARTESIAN_POINT('Ctrl Pts',(-17.5843097503121,-17.1662459757609,
-17.7824772334188));
#68939=CARTESIAN_POINT('Ctrl Pts',(-17.4194318623883,-17.2921871970481,
-17.7943233017074));
#68940=CARTESIAN_POINT('Ctrl Pts',(-17.3905221604003,-17.3154992064986,
-17.7964797261972));
#68941=CARTESIAN_POINT('Ctrl Pts',(-17.3567866104648,-17.3441991451115,
-17.799112841559));
#68942=CARTESIAN_POINT('Ctrl Pts',(-17.3513544538886,-17.348868190131,-17.7995405541146));
#68943=CARTESIAN_POINT('Ctrl Pts',(-17.3425342763275,-17.3565274808376,
-17.8002413280508));
#68944=CARTESIAN_POINT('Ctrl Pts',(-17.3391318992228,-17.3595012087532,
-17.8005131948968));
#68945=CARTESIAN_POINT('Ctrl Pts',(-17.3330612455963,-17.3648414299601,
-17.8010010950864));
#68946=CARTESIAN_POINT('Ctrl Pts',(-17.3303894056283,-17.3672037925531,
-17.8012168203345));
#68947=CARTESIAN_POINT('Ctrl Pts',(-17.3246189958244,-17.3723318592769,
-17.8016848832848));
#68948=CARTESIAN_POINT('Ctrl Pts',(-17.3215226340736,-17.3750998954252,
-17.8019373925274));
#68949=CARTESIAN_POINT('Ctrl Pts',(-17.3129034377732,-17.3828509016506,
-17.8026440171153));
#68950=CARTESIAN_POINT('Ctrl Pts',(-17.3073987545363,-17.3878538384509,
-17.8030995999471));
#68951=CARTESIAN_POINT('Ctrl Pts',(-17.2757195551927,-17.4169518489541,
-17.8057458069974));
#68952=CARTESIAN_POINT('Ctrl Pts',(-17.25013101886,-17.4416731536205,-17.8079799766362));
#68953=CARTESIAN_POINT('Ctrl Pts',(-17.170135650724,-17.5229531200549,-17.8152468071432));
#68954=CARTESIAN_POINT('Ctrl Pts',(-17.118247789956,-17.5818942296853,-17.8203977703006));
#68955=CARTESIAN_POINT('Ctrl Pts',(-16.953492832108,-17.7914534657815,-17.8379924651614));
#68956=CARTESIAN_POINT('Ctrl Pts',(-16.8574322263416,-17.9542043349617,
-17.850398086955));
#68957=CARTESIAN_POINT('Ctrl Pts',(-16.7756371588606,-18.1476487008244,
-17.8633108495524));
#68958=CARTESIAN_POINT('Ctrl Pts',(-16.7674427358968,-18.167896299497,-17.8646431667679));
#68959=CARTESIAN_POINT('Ctrl Pts',(-16.756526405379,-18.1961177171648,-17.866474275795));
#68960=CARTESIAN_POINT('Ctrl Pts',(-16.7535367473027,-18.2039858618691,
-17.8669820337858));
#68961=CARTESIAN_POINT('Ctrl Pts',(-16.7484730049532,-18.2175557481883,
-17.8678530725593));
#68962=CARTESIAN_POINT('Ctrl Pts',(-16.7463763772549,-18.2232489159007,
-17.8682171046256));
#68963=CARTESIAN_POINT('Ctrl Pts',(-16.7420995917008,-18.235017831786,-17.8689667624978));
#68964=CARTESIAN_POINT('Ctrl Pts',(-16.7399226884386,-18.2410947017641,
-17.8693522765633));
#68965=CARTESIAN_POINT('Ctrl Pts',(-16.7349133460213,-18.2552824414518,
-17.8702487306718));
#68966=CARTESIAN_POINT('Ctrl Pts',(-16.7321024046534,-18.263400822271,-17.8707589524153));
#68967=CARTESIAN_POINT('Ctrl Pts',(-16.7232311904579,-18.289535584376,-17.8723928486743));
#68968=CARTESIAN_POINT('Ctrl Pts',(-16.7173640073555,-18.3076168721773,
-17.8735101488881));
#68969=CARTESIAN_POINT('Ctrl Pts',(-16.6891047480586,-18.3988741001927,
-17.8790869964669));
#68970=CARTESIAN_POINT('Ctrl Pts',(-16.6704471663584,-18.4731510172963,
-17.8834235159508));
#68971=CARTESIAN_POINT('Ctrl Pts',(-16.6348971005142,-18.6561457115751,
-17.8937835424958));
#68972=CARTESIAN_POINT('Ctrl Pts',(-16.6223719831967,-18.7654773956982,
-17.8996976506881));
#68973=CARTESIAN_POINT('Ctrl Pts',(-16.6158517440397,-18.9453001108026,
-17.9094975582051));
#68974=CARTESIAN_POINT('Ctrl Pts',(-16.6167901534409,-19.0153896009238,
-17.9133382942622));
#68975=CARTESIAN_POINT('Ctrl Pts',(-16.6226174751437,-19.1077530992226,
-17.9185657552509));
#68976=CARTESIAN_POINT('Ctrl Pts',(-16.6243919466964,-19.1301824547245,
-17.9198482894585));
#68977=CARTESIAN_POINT('Ctrl Pts',(-16.6291864459383,-19.180558218768,-17.9227666829439));
#68978=CARTESIAN_POINT('Ctrl Pts',(-16.6324062069207,-19.208480629486,-17.9244106055936));
#68979=CARTESIAN_POINT('Ctrl Pts',(-16.6371419761922,-19.2434217874193,
-17.9265100428424));
#68980=CARTESIAN_POINT('Ctrl Pts',(-16.6381392346461,-19.250509428852,-17.9269380957575));
#68981=CARTESIAN_POINT('Ctrl Pts',(-16.6397691328093,-19.2616823598337,
-17.9276165300285));
#68982=CARTESIAN_POINT('Ctrl Pts',(-16.6403778405237,-19.2657711614613,
-17.9278655802577));
#68983=CARTESIAN_POINT('Ctrl Pts',(-16.6415343445789,-19.2733863979493,
-17.9283309116397));
#68984=CARTESIAN_POINT('Ctrl Pts',(-16.6420790832379,-19.2769132396271,
-17.9285470184905));
#68985=CARTESIAN_POINT('Ctrl Pts',(-16.6433380160572,-19.2849296245236,
-17.9290395748299));
#68986=CARTESIAN_POINT('Ctrl Pts',(-16.644057752191,-19.289418235905,-17.9293163340189));
#68987=CARTESIAN_POINT('Ctrl Pts',(-16.6462971863751,-19.3031023047266,
-17.9301629313079));
#68988=CARTESIAN_POINT('Ctrl Pts',(-16.6478631337355,-19.3122899308938,
-17.9307352940335));
#68989=CARTESIAN_POINT('Ctrl Pts',(-16.6690630663666,-19.4318987510933,
-17.9382354395378));
#68990=CARTESIAN_POINT('Ctrl Pts',(-16.697378932201,-19.5405881364994,-17.9455856423567));
#68991=CARTESIAN_POINT('Ctrl Pts',(-16.7954140475729,-19.822879879384,-17.9653126596922));
#68992=CARTESIAN_POINT('Ctrl Pts',(-16.8797423009026,-19.9904140676861,
-17.9776195768835));
#68993=CARTESIAN_POINT('Ctrl Pts',(-16.9973638158794,-20.1628952612935,
-17.9904569702309));
#68994=CARTESIAN_POINT('Ctrl Pts',(-17.0100358787283,-20.1808695356474,
-17.9917985229709));
#68995=CARTESIAN_POINT('Ctrl Pts',(-17.0279565165576,-20.205465546407,-17.9936401846737));
#68996=CARTESIAN_POINT('Ctrl Pts',(-17.0329677550768,-20.2122577309365,
-17.9941493950113));
#68997=CARTESIAN_POINT('Ctrl Pts',(-17.0416542973813,-20.2238851779148,
-17.9950222637246));
#68998=CARTESIAN_POINT('Ctrl Pts',(-17.0453100037779,-20.2287348905807,
-17.9953866805701));
#68999=CARTESIAN_POINT('Ctrl Pts',(-17.052892133641,-20.238703914709,-17.9961365283828));
#69000=CARTESIAN_POINT('Ctrl Pts',(-17.0568211945744,-20.2438211480367,
-17.9965218502619));
#69001=CARTESIAN_POINT('Ctrl Pts',(-17.066023445091,-20.2556934637922,-17.997416837854));
#69002=CARTESIAN_POINT('Ctrl Pts',(-17.0713144040846,-20.26243467891,-17.9979257925395));
#69003=CARTESIAN_POINT('Ctrl Pts',(-17.0883990241637,-20.283932151617,-17.9995514806227));
#69004=CARTESIAN_POINT('Ctrl Pts',(-17.1003495162504,-20.2985630172221,
-18.0006619306715));
#69005=CARTESIAN_POINT('Ctrl Pts',(-17.1611267347661,-20.3709717249482,
-18.0061812600895));
#69006=CARTESIAN_POINT('Ctrl Pts',(-17.2128322848691,-20.4262664574954,
-18.0104700605032));
#69007=CARTESIAN_POINT('Ctrl Pts',(-17.3462271448384,-20.5544125889058,
-18.0207555885344));
#69008=CARTESIAN_POINT('Ctrl Pts',(-17.4308125953392,-20.6239279523162,
-18.026642361794));
#69009=CARTESIAN_POINT('Ctrl Pts',(-17.6175210890745,-20.7545584837677,
-18.0390483178221));
#69010=CARTESIAN_POINT('Ctrl Pts',(-17.7201773575577,-20.8142292450865,
-18.0455602415365));
#69011=CARTESIAN_POINT('Ctrl Pts',(-17.8358751192896,-20.869068441837,-18.0531480800421));
#69012=CARTESIAN_POINT('Ctrl Pts',(-17.8445088197518,-20.8730895722569,
-18.0537157704433));
#69013=CARTESIAN_POINT('Ctrl Pts',(-17.8573395695598,-20.8789604363245,
-18.0545620164123));
#69014=CARTESIAN_POINT('Ctrl Pts',(-17.8615161076739,-20.8808550723636,
-18.0548378817539));
#69015=CARTESIAN_POINT('Ctrl Pts',(-17.8689567843353,-20.8842013344618,
-18.0553301216175));
#69016=CARTESIAN_POINT('Ctrl Pts',(-17.8722184733929,-20.8856582847119,
-18.0555461653519));
#69017=CARTESIAN_POINT('Ctrl Pts',(-17.87923762588,-20.8887723531228,-18.0560116782155));
#69018=CARTESIAN_POINT('Ctrl Pts',(-17.8829961725166,-20.8904267716317,
-18.0562613016241));
#69019=CARTESIAN_POINT('Ctrl Pts',(-17.8933810528223,-20.8949619123441,
-18.0569519423051));
#69020=CARTESIAN_POINT('Ctrl Pts',(-17.9000172851446,-20.8978196306515,
-18.0573943233906));
#69021=CARTESIAN_POINT('Ctrl Pts',(-17.936401001052,-20.913267001808,-18.0598248828219));
#69022=CARTESIAN_POINT('Ctrl Pts',(-17.9664173000941,-20.9252077819085,
-18.061848872269));
#69023=CARTESIAN_POINT('Ctrl Pts',(-18.149395863999,-20.9931918247272,-18.0742498508666));
#69024=CARTESIAN_POINT('Ctrl Pts',(-18.308132352176,-21.032111224602,-18.0852205525414));
#69025=CARTESIAN_POINT('Ctrl Pts',(-18.5857202943358,-21.0670323183666,
-18.1034957546379));
#69026=CARTESIAN_POINT('Ctrl Pts',(-18.7027036719987,-21.0719945605717,
-18.1109407661892));
#69027=CARTESIAN_POINT('Ctrl Pts',(-18.8337944032507,-21.0666948446787,
-18.1189517061858));
#69028=CARTESIAN_POINT('Ctrl Pts',(-18.8480669670608,-21.065973025319,-18.1198197331435));
#69029=CARTESIAN_POINT('Ctrl Pts',(-18.8707706118965,-21.0645942067892,
-18.1211941068338));
#69030=CARTESIAN_POINT('Ctrl Pts',(-18.8792067632627,-21.0640311271334,
-18.1217033820663));
#69031=CARTESIAN_POINT('Ctrl Pts',(-18.8940791427192,-21.0629489235369,
-18.122598777195));
#69032=CARTESIAN_POINT('Ctrl Pts',(-18.9005167507343,-21.0624508672018,
-18.1229855532969));
#69033=CARTESIAN_POINT('Ctrl Pts',(-18.9138269366389,-21.0613598210612,
-18.1237836187335));
#69034=CARTESIAN_POINT('Ctrl Pts',(-18.9206991042232,-21.0607626770365,
-18.1241947727285));
#69035=CARTESIAN_POINT('Ctrl Pts',(-18.9383312239533,-21.059143698998,-18.1252474505101));
#69036=CARTESIAN_POINT('Ctrl Pts',(-18.9490865755848,-21.0580730255312,
-18.1258874331789));
#69037=CARTESIAN_POINT('Ctrl Pts',(-18.9939389302393,-21.0532608901094,
-18.128547844724));
#69038=CARTESIAN_POINT('Ctrl Pts',(-19.0279517884252,-21.0487732634634,
-18.1305447505903));
#69039=CARTESIAN_POINT('Ctrl Pts',(-19.1162738059897,-21.034928551885,-18.1356881264718));
#69040=CARTESIAN_POINT('Ctrl Pts',(-19.1703541838453,-21.0242741822414,
-18.1387952215826));
#69041=CARTESIAN_POINT('Ctrl Pts',(-19.3893465596709,-20.9721758682196,
-18.1513119061741));
#69042=CARTESIAN_POINT('Ctrl Pts',(-19.5493765534055,-20.9130568436342,
-18.1602560318618));
#69043=CARTESIAN_POINT('Ctrl Pts',(-19.7072213182256,-20.8320490854616,
-18.1701910795476));
#69044=CARTESIAN_POINT('Ctrl Pts',(-19.7138191888339,-20.8286189419307,
-18.17060861938));
#69045=CARTESIAN_POINT('Ctrl Pts',(-19.7661388625077,-20.801067518496,-18.1739386610872));
#69046=CARTESIAN_POINT('Ctrl Pts',(-19.8109774221947,-20.7753156653979,
-18.1769084506207));
#69047=CARTESIAN_POINT('Ctrl Pts',(-19.8621009869288,-20.7434102629205,
-18.1804851115094));
#69048=CARTESIAN_POINT('Ctrl Pts',(-19.869349551062,-20.7388251056207,-18.1809968357557));
#69049=CARTESIAN_POINT('Ctrl Pts',(-19.8802770325903,-20.7318194727903,
-18.1817755946933));
#69050=CARTESIAN_POINT('Ctrl Pts',(-19.8839766894152,-20.7294312937958,
-18.1820405339688));
#69051=CARTESIAN_POINT('Ctrl Pts',(-19.8905140982894,-20.7251823526583,
-18.1825110095978));
#69052=CARTESIAN_POINT('Ctrl Pts',(-19.8933548548627,-20.7233262928215,
-18.1827162308012));
#69053=CARTESIAN_POINT('Ctrl Pts',(-19.8962134283951,-20.7214487694101,
-18.1829235345918));
#69054=CARTESIAN_POINT('Ctrl Pts',(-19.8962356816485,-20.7214341527765,
-18.1829251484465));
#69055=CARTESIAN_POINT('Ctrl Pts',(-19.8962797191912,-20.7214052263504,
-18.1829283422414));
#69056=CARTESIAN_POINT('Ctrl Pts',(-19.8963015032605,-20.7213909167275,
-18.1829299221637));
#69057=CARTESIAN_POINT('Ctrl Pts',(-19.8963446318564,-20.7213625850703,
-18.1829330502217));
#69058=CARTESIAN_POINT('Ctrl Pts',(-19.8963659759384,-20.7213485633512,
-18.1829345983233));
#69059=CARTESIAN_POINT('Ctrl Pts',(-19.8964082500977,-20.7213207907929,
-18.1829376645868));
#69060=CARTESIAN_POINT('Ctrl Pts',(-19.8964291804592,-20.7213070397882,
-18.1829391827675));
#69061=CARTESIAN_POINT('Ctrl Pts',(-19.8964706525528,-20.7212797920503,
-18.1829421910247));
#69062=CARTESIAN_POINT('Ctrl Pts',(-19.8964911941522,-20.7212662954238,
-18.18294368109));
#69063=CARTESIAN_POINT('Ctrl Pts',(-19.8965319108553,-20.7212395419575,
-18.1829466347172));
#69064=CARTESIAN_POINT('Ctrl Pts',(-19.8965520863329,-20.72122628489,-18.1829480983047));
#69065=CARTESIAN_POINT('Ctrl Pts',(-19.8965920920005,-20.7211999966598,
-18.1829510005107));
#69066=CARTESIAN_POINT('Ctrl Pts',(-19.8966119224368,-20.7211869653519,
-18.1829524391455));
#69067=CARTESIAN_POINT('Ctrl Pts',(-19.8966512586304,-20.7211611151475,
-18.1829552929372));
#69068=CARTESIAN_POINT('Ctrl Pts',(-19.8966707640526,-20.7211482964868,
-18.1829567080684));
#69069=CARTESIAN_POINT('Ctrl Pts',(-19.8967094685502,-20.7211228595752,
-18.182959516179));
#69070=CARTESIAN_POINT('Ctrl Pts',(-19.896728667493,-20.7211102414258,-18.1829609091476));
#69071=CARTESIAN_POINT('Ctrl Pts',(-19.8967667755203,-20.7210851947428,
-18.1829636741259));
#69072=CARTESIAN_POINT('Ctrl Pts',(-19.8967856849602,-20.7210727659889,
-18.1829650461603));
#69073=CARTESIAN_POINT('Ctrl Pts',(-19.896823230357,-20.7210480873734,-18.1829677704551));
#69074=CARTESIAN_POINT('Ctrl Pts',(-19.8968418663888,-20.721035837475,-18.1829691227199));
#69075=CARTESIAN_POINT('Ctrl Pts',(-19.8968788806954,-20.7210115062702,
-18.1829718086137));
#69076=CARTESIAN_POINT('Ctrl Pts',(-19.8968972586385,-20.7209994251935,
-18.1829731422177));
#69077=CARTESIAN_POINT('Ctrl Pts',(-19.8969337709767,-20.7209754223258,
-18.1829757918182));
#69078=CARTESIAN_POINT('Ctrl Pts',(-19.896951905184,-20.7209635006692,-18.1829771078001));
#69079=CARTESIAN_POINT('Ctrl Pts',(-19.8969879426736,-20.7209398083753,
-18.1829797230699));
#69080=CARTESIAN_POINT('Ctrl Pts',(-19.8970058463033,-20.7209280375197,
-18.1829810223822));
#69081=CARTESIAN_POINT('Ctrl Pts',(-19.8970414351949,-20.720904638602,-18.1829836052215));
#69082=CARTESIAN_POINT('Ctrl Pts',(-19.8970591206562,-20.7208930104182,
-18.1829848887623));
#69083=CARTESIAN_POINT('Ctrl Pts',(-19.8970942864667,-20.7208698881563,
-18.1829874410185));
#69084=CARTESIAN_POINT('Ctrl Pts',(-19.8971117662386,-20.7208583944666,
-18.1829887096913));
#69085=CARTESIAN_POINT('Ctrl Pts',(-19.897146530569,-20.7208355347101,-18.1829912329278));
#69086=CARTESIAN_POINT('Ctrl Pts',(-19.8971638154642,-20.7208241684302,
-18.1829924875154));
#69087=CARTESIAN_POINT('Ctrl Pts',(-19.8971982013371,-20.7208015560897,
-18.1829949833993));
#69088=CARTESIAN_POINT('Ctrl Pts',(-19.8972153022018,-20.720790310111,-18.1829962246868));
#69089=CARTESIAN_POINT('Ctrl Pts',(-19.8972493300429,-20.7207679318003,
-18.182998694697));
#69090=CARTESIAN_POINT('Ctrl Pts',(-19.8972662569826,-20.7207567994996,
-18.1829999234163));
#69091=CARTESIAN_POINT('Ctrl Pts',(-19.8972999465503,-20.7207346422679,
-18.1830023689834));
#69092=CARTESIAN_POINT('Ctrl Pts',(-19.8973167091712,-20.7207236173483,
-18.1830035858302));
#69093=CARTESIAN_POINT('Ctrl Pts',(-19.8973500793006,-20.7207016688482,
-18.1830060083183));
#69094=CARTESIAN_POINT('Ctrl Pts',(-19.8973666868106,-20.720690745273,-18.1830072139593));
#69095=CARTESIAN_POINT('Ctrl Pts',(-19.8973997550678,-20.7206689939885,
-18.1830096146406));
#69096=CARTESIAN_POINT('Ctrl Pts',(-19.8974162160191,-20.7206581661508,
-18.1830108096952));
#69097=CARTESIAN_POINT('Ctrl Pts',(-19.8974489997398,-20.7206366007143,
-18.1830131898253));
#69098=CARTESIAN_POINT('Ctrl Pts',(-19.8974653224463,-20.7206258631623,
-18.1830143748958));
#69099=CARTESIAN_POINT('Ctrl Pts',(-19.8974978379949,-20.720604472842,-18.1830167356602));
#69100=CARTESIAN_POINT('Ctrl Pts',(-19.8975140305315,-20.7205938202798,
-18.1830179113315));
#69101=CARTESIAN_POINT('Ctrl Pts',(-19.9010411141942,-20.7182733931061,
-18.1832740034795));
#69102=CARTESIAN_POINT('Ctrl Pts',(-19.9045450846592,-20.7159531925442,
-18.1835296228759));
#69103=CARTESIAN_POINT('Ctrl Pts',(-19.9146520459037,-20.7092173582621,
-18.1842703754439));
#69104=CARTESIAN_POINT('Ctrl Pts',(-19.9212370382047,-20.7047750306903,
-18.1847572541746));
#69105=CARTESIAN_POINT('Ctrl Pts',(-19.9650511532819,-20.6748572402252,
-18.1880244528397));
#69106=CARTESIAN_POINT('Ctrl Pts',(-20.0014799916308,-20.6482363683382,
-18.1908749773723));
#69107=CARTESIAN_POINT('Ctrl Pts',(-20.1318630099769,-20.5464112232603,
-18.2014991280105));
#69108=CARTESIAN_POINT('Ctrl Pts',(-20.2202075162418,-20.4643999648833,
-18.2095229599269));
#69109=CARTESIAN_POINT('Ctrl Pts',(-20.3988404465469,-20.2677230962314,
-18.2270189211216));
#69110=CARTESIAN_POINT('Ctrl Pts',(-20.4852486801041,-20.150316983744,-18.236382428185));
#69111=CARTESIAN_POINT('Ctrl Pts',(-20.5661837883021,-20.0126579127701,
-18.2461327768856));
#69112=CARTESIAN_POINT('Ctrl Pts',(-20.5732919825117,-20.0002831968325,
-18.2469995817129));
#69113=CARTESIAN_POINT('Ctrl Pts',(-20.584408696955,-19.9804687840582,-18.248372392136));
#69114=CARTESIAN_POINT('Ctrl Pts',(-20.5884986450101,-19.9730754939952,
-18.2488813158762));
#69115=CARTESIAN_POINT('Ctrl Pts',(-20.5956354296389,-19.9599901808339,
-18.2497763022316));
#69116=CARTESIAN_POINT('Ctrl Pts',(-20.5987006749914,-19.954308371542,-18.2501630191671));
#69117=CARTESIAN_POINT('Ctrl Pts',(-20.604988339472,-19.9425247335344,-18.2509611630096));
#69118=CARTESIAN_POINT('Ctrl Pts',(-20.6082070156386,-19.9364209863916,
-18.2513724535886));
#69119=CARTESIAN_POINT('Ctrl Pts',(-20.6163954079357,-19.9207071674811,
-18.2524258964183));
#69120=CARTESIAN_POINT('Ctrl Pts',(-20.621321442429,-19.9110744640908,-18.2530665031507));
#69121=CARTESIAN_POINT('Ctrl Pts',(-20.6415981741794,-19.8706627081341,
-18.2557329865273));
#69122=CARTESIAN_POINT('Ctrl Pts',(-20.6562719922963,-19.8395486190453,
-18.2577352028925));
#69123=CARTESIAN_POINT('Ctrl Pts',(-20.6890778951259,-19.765352874987,-18.2624020880917));
#69124=CARTESIAN_POINT('Ctrl Pts',(-20.706553647153,-19.7220029411599,-18.2650452757123));
#69125=CARTESIAN_POINT('Ctrl Pts',(-20.7225805813239,-19.6781103714872,
-18.2676550109742));
#69126=CARTESIAN_POINT('Ctrl Pts',(-20.7225806448396,-19.6781101975385,
-18.0457833736847));
#69127=CARTESIAN_POINT('Ctrl Pts',(-20.6985992167088,-19.743787561633,-18.0412352539614));
#69128=CARTESIAN_POINT('Ctrl Pts',(-20.6713684492053,-19.8082648318828,
-18.0366093886528));
#69129=CARTESIAN_POINT('Ctrl Pts',(-20.6100512330559,-19.9354601153677,
-18.0272785871659));
#69130=CARTESIAN_POINT('Ctrl Pts',(-20.5759024792062,-19.9980201263964,
-18.022581895011));
#69131=CARTESIAN_POINT('Ctrl Pts',(-20.4894060415052,-20.1390620405839,
-18.0118326270559));
#69132=CARTESIAN_POINT('Ctrl Pts',(-20.4348362291936,-20.2160122140981,
-18.0058467969157));
#69133=CARTESIAN_POINT('Ctrl Pts',(-20.3617162823741,-20.3057696090812,
-17.9987328433445));
#69134=CARTESIAN_POINT('Ctrl Pts',(-20.3478652721742,-20.3222523079263,
-17.9974201993456));
#69135=CARTESIAN_POINT('Ctrl Pts',(-20.3291374813325,-20.34386038572,-17.9956903943503));
#69136=CARTESIAN_POINT('Ctrl Pts',(-20.3244833832923,-20.3491762691418,
-17.9952640983138));
#69137=CARTESIAN_POINT('Ctrl Pts',(-20.3152196348101,-20.3596509958889,
-17.9944225874072));
#69138=CARTESIAN_POINT('Ctrl Pts',(-20.3106111379901,-20.36481073788,-17.9940073320007));
#69139=CARTESIAN_POINT('Ctrl Pts',(-20.3016579801493,-20.3747364638025,
-17.9932070404168));
#69140=CARTESIAN_POINT('Ctrl Pts',(-20.297316677266,-20.3795053611674,-17.9928218694959));
#69141=CARTESIAN_POINT('Ctrl Pts',(-20.287266415397,-20.3904446832533,-17.9919367482262));
#69142=CARTESIAN_POINT('Ctrl Pts',(-20.2815423358339,-20.3966011165341,
-17.9914374480582));
#69143=CARTESIAN_POINT('Ctrl Pts',(-20.2661035773263,-20.4130089276943,
-17.9901034512516));
#69144=CARTESIAN_POINT('Ctrl Pts',(-20.2563226277584,-20.4231975699665,
-17.9892716094273));
#69145=CARTESIAN_POINT('Ctrl Pts',(-20.1714503993181,-20.5098547204957,
-17.9821641180485));
#69146=CARTESIAN_POINT('Ctrl Pts',(-20.0907499509967,-20.5806217774676,
-17.9761515338725));
#69147=CARTESIAN_POINT('Ctrl Pts',(-19.9106080183978,-20.7158657530999,
-17.9637760064709));
#69148=CARTESIAN_POINT('Ctrl Pts',(-19.8104277411408,-20.7787268359861,
-17.9574616387272));
#69149=CARTESIAN_POINT('Ctrl Pts',(-19.6539894100173,-20.8595308514712,
-17.9477550185748));
#69150=CARTESIAN_POINT('Ctrl Pts',(-19.6013774391923,-20.8840222273987,
-17.9445117946365));
#69151=CARTESIAN_POINT('Ctrl Pts',(-19.5207479925468,-20.9175984431095,
-17.9394791790417));
#69152=CARTESIAN_POINT('Ctrl Pts',(-19.4934356535838,-20.9283114470924,
-17.9377639594655));
#69153=CARTESIAN_POINT('Ctrl Pts',(-19.4593565842697,-20.9408679242767,
-17.9356005824247));
#69154=CARTESIAN_POINT('Ctrl Pts',(-19.4527902218378,-20.9432504635159,
-17.9351826874201));
#69155=CARTESIAN_POINT('Ctrl Pts',(-19.4423651837297,-20.9469748007534,
-17.9345173707888));
#69156=CARTESIAN_POINT('Ctrl Pts',(-19.4385141417142,-20.9483380256452,
-17.9342712024428));
#69157=CARTESIAN_POINT('Ctrl Pts',(-19.4312850051266,-20.9508735346393,
-17.9338083091325));
#69158=CARTESIAN_POINT('Ctrl Pts',(-19.4279078781634,-20.9520484098639,
-17.9335917403934));
#69159=CARTESIAN_POINT('Ctrl Pts',(-19.4201610685147,-20.9547214800779,
-17.9330942165664));
#69160=CARTESIAN_POINT('Ctrl Pts',(-19.4157894603182,-20.9562139280964,
-17.9328129266505));
#69161=CARTESIAN_POINT('Ctrl Pts',(-19.4022284822096,-20.9607940846542,
-17.9319387807732));
#69162=CARTESIAN_POINT('Ctrl Pts',(-19.3930229135797,-20.963832937933,-17.9313431595033));
#69163=CARTESIAN_POINT('Ctrl Pts',(-19.2884804287144,-20.9975489942562,
-17.9245564472342));
#69164=CARTESIAN_POINT('Ctrl Pts',(-19.1911133244138,-21.0214834811473,
-17.9180287429307));
#69165=CARTESIAN_POINT('Ctrl Pts',(-18.9235549270968,-21.067447692445,-17.9001409442158));
#69166=CARTESIAN_POINT('Ctrl Pts',(-18.7517479980882,-21.0758534142306,
-17.8887649758942));
#69167=CARTESIAN_POINT('Ctrl Pts',(-18.552076248789,-21.0613652529006,-17.8762269883954));
#69168=CARTESIAN_POINT('Ctrl Pts',(-18.5234034898055,-21.0586958151084,
-17.8744409990253));
#69169=CARTESIAN_POINT('Ctrl Pts',(-18.474140917004,-21.0530935915597,-17.8713968166211));
#69170=CARTESIAN_POINT('Ctrl Pts',(-18.4535240130681,-21.0504409194983,
-17.8701301536283));
#69171=CARTESIAN_POINT('Ctrl Pts',(-18.4240277792312,-21.0462032976491,
-17.8683279767776));
#69172=CARTESIAN_POINT('Ctrl Pts',(-18.4151148028715,-21.0448646550869,
-17.8677847202948));
#69173=CARTESIAN_POINT('Ctrl Pts',(-18.3997623697167,-21.0424585158982,
-17.8668511624229));
#69174=CARTESIAN_POINT('Ctrl Pts',(-18.3933188544185,-21.0414180909323,
-17.8664600091059));
#69175=CARTESIAN_POINT('Ctrl Pts',(-18.3809968245796,-21.0393699548819,
-17.8657132416991));
#69176=CARTESIAN_POINT('Ctrl Pts',(-18.3751175649468,-21.0383671703063,
-17.8653574753327));
#69177=CARTESIAN_POINT('Ctrl Pts',(-18.359853935092,-21.0356973305977,-17.8644352079534));
#69178=CARTESIAN_POINT('Ctrl Pts',(-18.3504763787318,-21.033991709847,-17.8638699372506));
#69179=CARTESIAN_POINT('Ctrl Pts',(-18.3186082338191,-21.0279728073589,
-17.8619532887333));
#69180=CARTESIAN_POINT('Ctrl Pts',(-18.2961757548717,-21.0233578654834,
-17.8606115141048));
#69181=CARTESIAN_POINT('Ctrl Pts',(-18.1013603417009,-20.9799729131537,
-17.8490127194019));
#69182=CARTESIAN_POINT('Ctrl Pts',(-17.9343872183227,-20.9201293438453,
-17.8395186852023));
#69183=CARTESIAN_POINT('Ctrl Pts',(-17.6999263807577,-20.8012713769272,
-17.8252130389209));
#69184=CARTESIAN_POINT('Ctrl Pts',(-17.6255313458058,-20.7576599270118,
-17.8204935063282));
#69185=CARTESIAN_POINT('Ctrl Pts',(-17.5227815950948,-20.6886788482865,
-17.8134260837131));
#69186=CARTESIAN_POINT('Ctrl Pts',(-17.4921228769797,-20.6668889949062,
-17.8112411213368));
#69187=CARTESIAN_POINT('Ctrl Pts',(-17.4560200241897,-20.6397539295148,
-17.8085539517204));
#69188=CARTESIAN_POINT('Ctrl Pts',(-17.450001601535,-20.6351798044172,-17.8081020740588));
#69189=CARTESIAN_POINT('Ctrl Pts',(-17.4406938917621,-20.6280267836449,
-17.8073968929144));
#69190=CARTESIAN_POINT('Ctrl Pts',(-17.4373874567062,-20.6254701613654,
-17.8071451346013));
#69191=CARTESIAN_POINT('Ctrl Pts',(-17.4312756465815,-20.6207153625459,
-17.8066773989691));
#69192=CARTESIAN_POINT('Ctrl Pts',(-17.4284682432846,-20.6185198870129,
-17.8064616125685));
#69193=CARTESIAN_POINT('Ctrl Pts',(-17.422141549697,-20.613546420914,-17.8059732076661));
#69194=CARTESIAN_POINT('Ctrl Pts',(-17.4186255528399,-20.6107643489616,
-17.8057003009175));
#69195=CARTESIAN_POINT('Ctrl Pts',(-17.4082960053871,-20.602537484983,-17.8048942318478));
#69196=CARTESIAN_POINT('Ctrl Pts',(-17.4015073313391,-20.5970618081456,
-17.8043589318196));
#69197=CARTESIAN_POINT('Ctrl Pts',(-17.3534129281117,-20.557776326218,-17.8005281183443));
#69198=CARTESIAN_POINT('Ctrl Pts',(-17.3133685901279,-20.5224596882375,
-17.7971354213675));
#69199=CARTESIAN_POINT('Ctrl Pts',(-17.262061964801,-20.4736412183802,-17.7925582246905));
#69200=CARTESIAN_POINT('Ctrl Pts',(-17.249568163393,-20.4614554235845,-17.791424360477));
#69201=CARTESIAN_POINT('Ctrl Pts',(-17.2028393473679,-20.4147373291041,
-17.7871140456336));
#69202=CARTESIAN_POINT('Ctrl Pts',(-17.1696475462279,-20.3791841500694,
-17.7839085274046));
#69203=CARTESIAN_POINT('Ctrl Pts',(-17.0658627852009,-20.2600413371745,
-17.7734710134909));
#69204=CARTESIAN_POINT('Ctrl Pts',(-17.0005103316433,-20.1721110369868,
-17.7662381123081));
#69205=CARTESIAN_POINT('Ctrl Pts',(-16.9128955757416,-20.0328811380464,
-17.7556642494986));
#69206=CARTESIAN_POINT('Ctrl Pts',(-16.8853777886072,-19.9851128202315,
-17.7521749114311));
#69207=CARTESIAN_POINT('Ctrl Pts',(-16.8438032680044,-19.9059507927004,
-17.7466170589514));
#69208=CARTESIAN_POINT('Ctrl Pts',(-16.8285928973241,-19.8751954234934,
-17.7445101009141));
#69209=CARTESIAN_POINT('Ctrl Pts',(-16.809581353943,-19.8342803978335,-17.7417734717013));
#69210=CARTESIAN_POINT('Ctrl Pts',(-16.8051017923191,-19.8244434290454,
-17.7411204570575));
#69211=CARTESIAN_POINT('Ctrl Pts',(-16.7978870878274,-19.808272955516,-17.7400549450428));
#69212=CARTESIAN_POINT('Ctrl Pts',(-16.7951072574144,-19.8019597152397,
-17.7396409181602));
#69213=CARTESIAN_POINT('Ctrl Pts',(-16.7897852784013,-19.7897110513713,
-17.7388414016324));
#69214=CARTESIAN_POINT('Ctrl Pts',(-16.7872393324841,-19.7837773705202,
-17.7384557856285));
#69215=CARTESIAN_POINT('Ctrl Pts',(-16.7814224725198,-19.7700473571059,
-17.737567371586));
#69216=CARTESIAN_POINT('Ctrl Pts',(-16.7781710218343,-19.7622428590363,
-17.7370652395822));
#69217=CARTESIAN_POINT('Ctrl Pts',(-16.7695501595302,-19.7411958012982,
-17.7357186539877));
#69218=CARTESIAN_POINT('Ctrl Pts',(-16.7642678686016,-19.7279178654694,
-17.734877141636));
#69219=CARTESIAN_POINT('Ctrl Pts',(-16.7170425207028,-19.6056179137501,
-17.7271967971292));
#69220=CARTESIAN_POINT('Ctrl Pts',(-16.6840528963727,-19.4933464543303,
-17.7206745015522));
#69221=CARTESIAN_POINT('Ctrl Pts',(-16.6276808696708,-19.2195486913437,
-17.705371054411));
#69222=CARTESIAN_POINT('Ctrl Pts',(-16.6133548999859,-19.0569528627794,
-17.6967728845433));
#69223=CARTESIAN_POINT('Ctrl Pts',(-16.6186718954416,-18.8618019649981,
-17.6855640193953));
#69224=CARTESIAN_POINT('Ctrl Pts',(-16.6203088644817,-18.8292881553707,
-17.6836654624941));
#69225=CARTESIAN_POINT('Ctrl Pts',(-16.623225504645,-18.789603923699,-17.6812962694845));
#69226=CARTESIAN_POINT('Ctrl Pts',(-16.6237934346789,-18.7823836562483,
-17.6808631038559));
#69227=CARTESIAN_POINT('Ctrl Pts',(-16.6247417335092,-18.7710705653313,
-17.6801808945602));
#69228=CARTESIAN_POINT('Ctrl Pts',(-16.6250969981053,-18.7669756150441,
-17.6799332381386));
#69229=CARTESIAN_POINT('Ctrl Pts',(-16.6257832670682,-18.7593241969135,
-17.6794691026115));
#69230=CARTESIAN_POINT('Ctrl Pts',(-16.6261113472134,-18.7557675233129,
-17.679252789121));
#69231=CARTESIAN_POINT('Ctrl Pts',(-16.6268807041034,-18.747651635749,-17.6787579065834));
#69232=CARTESIAN_POINT('Ctrl Pts',(-16.6273277763972,-18.743093029074,-17.6784790160038));
#69233=CARTESIAN_POINT('Ctrl Pts',(-16.6287470647711,-18.7290891721719,
-17.6776195212924));
#69234=CARTESIAN_POINT('Ctrl Pts',(-16.6297680199109,-18.7196491344887,
-17.6770362812199));
#69235=CARTESIAN_POINT('Ctrl Pts',(-16.6395752256174,-18.6343414109738,
-17.6717327447863));
#69236=CARTESIAN_POINT('Ctrl Pts',(-16.6523967615574,-18.559001924081,-17.66681493842));
#69237=CARTESIAN_POINT('Ctrl Pts',(-16.6708311433045,-18.4775803266455,
-17.6613539437278));
#69238=CARTESIAN_POINT('Ctrl Pts',(-16.6724394045865,-18.4706397731387,
-17.6608872430014));
#69239=CARTESIAN_POINT('Ctrl Pts',(-16.7048775657934,-18.3337957051517,
-17.6516633272659));
#69240=CARTESIAN_POINT('Ctrl Pts',(-16.7478961666825,-18.2070770008716,
-17.6427531064208));
#69241=CARTESIAN_POINT('Ctrl Pts',(-16.8280081432266,-18.0285576436559,
-17.6301080429714));
#69242=CARTESIAN_POINT('Ctrl Pts',(-16.8559365444506,-17.9730058488077,
-17.6261544149705));
#69243=CARTESIAN_POINT('Ctrl Pts',(-16.9045255954434,-17.8861147889895,
-17.6199504218185));
#69244=CARTESIAN_POINT('Ctrl Pts',(-16.9236428699102,-17.853958460988,-17.6176495302413));
#69245=CARTESIAN_POINT('Ctrl Pts',(-16.9495530746944,-17.8128939930676,
-17.6147027916065));
#69246=CARTESIAN_POINT('Ctrl Pts',(-16.9555774871667,-17.8035111243199,
-17.6140288856109));
#69247=CARTESIAN_POINT('Ctrl Pts',(-16.9654896543488,-17.7883382002817,
-17.6129380108901));
#69248=CARTESIAN_POINT('Ctrl Pts',(-16.9693323245552,-17.7825190793135,
-17.61251936986));
#69249=CARTESIAN_POINT('Ctrl Pts',(-16.9767732295691,-17.7713711769132,
-17.6117168028945));
#69250=CARTESIAN_POINT('Ctrl Pts',(-16.9803671205189,-17.7660396018274,
-17.611332719701));
#69251=CARTESIAN_POINT('Ctrl Pts',(-16.9886456148864,-17.753878278721,-17.6104560097564));
#69252=CARTESIAN_POINT('Ctrl Pts',(-16.9933461366148,-17.747059453959,-17.6099639926086));
#69253=CARTESIAN_POINT('Ctrl Pts',(-17.0059270941754,-17.7290361134634,
-17.6086621888729));
#69254=CARTESIAN_POINT('Ctrl Pts',(-17.013876549892,-17.7178800847709,-17.6078550418735));
#69255=CARTESIAN_POINT('Ctrl Pts',(-17.0744631666554,-17.63457744702,-17.6018159181769));
#69256=CARTESIAN_POINT('Ctrl Pts',(-17.1315133690548,-17.565744587087,-17.5967623212738));
#69257=CARTESIAN_POINT('Ctrl Pts',(-17.2884850846914,-17.3990419468733,
-17.5840804871437));
#69258=CARTESIAN_POINT('Ctrl Pts',(-17.3940439899097,-17.3070962886841,
-17.5766518411665));
#69259=CARTESIAN_POINT('Ctrl Pts',(-17.5534533491994,-17.1938409483206,
-17.5658553959733));
#69260=CARTESIAN_POINT('Ctrl Pts',(-17.6002833114379,-17.1632855893545,
-17.5627248869781));
#69261=CARTESIAN_POINT('Ctrl Pts',(-17.6728937552751,-17.1199067468825,
-17.5578472689787));
#69262=CARTESIAN_POINT('Ctrl Pts',(-17.6978189655542,-17.1056953580475,
-17.5561688116792));
#69263=CARTESIAN_POINT('Ctrl Pts',(-17.7291388095643,-17.0886719483782,
-17.5540449891703));
#69264=CARTESIAN_POINT('Ctrl Pts',(-17.7352700482102,-17.085378474266,-17.5536285338077));
#69265=CARTESIAN_POINT('Ctrl Pts',(-17.744992736391,-17.0802174222796,-17.5529668666106));
#69266=CARTESIAN_POINT('Ctrl Pts',(-17.7485735562737,-17.0783297757871,
-17.5527229072413));
#69267=CARTESIAN_POINT('Ctrl Pts',(-17.7553337898359,-17.0747908255488,
-17.5522617854239));
#69268=CARTESIAN_POINT('Ctrl Pts',(-17.7585119892116,-17.073137318574,-17.5520447650108));
#69269=CARTESIAN_POINT('Ctrl Pts',(-17.7657835211257,-17.0693776157916,
-17.5515477175492));
#69270=CARTESIAN_POINT('Ctrl Pts',(-17.7698795310851,-17.0672767014806,
-17.5512673631174));
#69271=CARTESIAN_POINT('Ctrl Pts',(-17.7807630372948,-17.0617391254021,
-17.5505215178186));
#69272=CARTESIAN_POINT('Ctrl Pts',(-17.7875621910878,-17.0583257009259,
-17.5500546314522));
#69273=CARTESIAN_POINT('Ctrl Pts',(-17.8350485104516,-17.0348054468173,
-17.5467880612411));
#69274=CARTESIAN_POINT('Ctrl Pts',(-17.8763515972135,-17.0159764254801,
-17.5439176359258));
#69275=CARTESIAN_POINT('Ctrl Pts',(-17.9235895562848,-16.9962500874831,
-17.5406275739431));
#69276=CARTESIAN_POINT('Ctrl Pts',(-17.9289641176092,-16.9940316563879,
-17.5402531364634));
#69277=CARTESIAN_POINT('Ctrl Pts',(-18.0801760273008,-16.9323445148577,
-17.5297166909062));
#69278=CARTESIAN_POINT('Ctrl Pts',(-18.2321878966764,-16.8893118555842,
-17.5191262198398));
#69279=CARTESIAN_POINT('Ctrl Pts',(-18.489180696128,-16.8466827395006,-17.502214494249));
#69280=CARTESIAN_POINT('Ctrl Pts',(-18.5918943469089,-16.8372639153502,
-17.495695274456));
#69281=CARTESIAN_POINT('Ctrl Pts',(-18.7097046581973,-16.835087626326,-17.4885096620398));
#69282=CARTESIAN_POINT('Ctrl Pts',(-18.7245123588162,-16.8349694703209,
-17.4876115365446));
#69283=CARTESIAN_POINT('Ctrl Pts',(-18.7470890134317,-16.8350262094805,
-17.4862496405256));
#69284=CARTESIAN_POINT('Ctrl Pts',(-18.7548575580758,-16.8350884957562,
-17.4857823586322));
#69285=CARTESIAN_POINT('Ctrl Pts',(-18.7689864733627,-16.8352795616905,
-17.4849348837307));
#69286=CARTESIAN_POINT('Ctrl Pts',(-18.7753469141363,-16.8353942499052,
-17.4845542540677));
#69287=CARTESIAN_POINT('Ctrl Pts',(-18.7890725678174,-16.8357036373795,
-17.483734725267));
#69288=CARTESIAN_POINT('Ctrl Pts',(-18.7964374932963,-16.8359081202126,
-17.4832961374704));
#69289=CARTESIAN_POINT('Ctrl Pts',(-18.8163931797336,-16.8365664528046,
-17.482110806357));
#69290=CARTESIAN_POINT('Ctrl Pts',(-18.8289813257046,-16.8370942605501,
-17.4813663839479));
#69291=CARTESIAN_POINT('Ctrl Pts',(-18.890049833593,-16.8402011485294,-17.4777700938631));
#69292=CARTESIAN_POINT('Ctrl Pts',(-18.9384386531467,-16.8443351053112,
-17.4749672011889));
#69293=CARTESIAN_POINT('Ctrl Pts',(-19.0271592539814,-16.8549993479368,
-17.4698883422315));
#69294=CARTESIAN_POINT('Ctrl Pts',(-19.0675251277346,-16.8610396182918,
-17.4676006621723));
#69295=CARTESIAN_POINT('Ctrl Pts',(-19.240032468628,-16.8919764056235,-17.4578739050451));
#69296=CARTESIAN_POINT('Ctrl Pts',(-19.3698060735372,-16.9282618728386,
-17.4507040792665));
#69297=CARTESIAN_POINT('Ctrl Pts',(-19.5537918318525,-16.9991648854428,
-17.4398677829608));
#69298=CARTESIAN_POINT('Ctrl Pts',(-19.6112870808457,-17.0243097083801,
-17.4363742441128));
#69299=CARTESIAN_POINT('Ctrl Pts',(-19.6953392890889,-17.065608575186,-17.4309875260399));
#69300=CARTESIAN_POINT('Ctrl Pts',(-19.7227978722138,-17.0798556740738,
-17.4291811433687));
#69301=CARTESIAN_POINT('Ctrl Pts',(-19.7561871479493,-17.0981194064623,
-17.4269145719479));
#69302=CARTESIAN_POINT('Ctrl Pts',(-19.7624240619938,-17.101572004657,-17.4264881299539));
#69303=CARTESIAN_POINT('Ctrl Pts',(-19.7722074760035,-17.1070525952048,
-17.4258141834715));
#69304=CARTESIAN_POINT('Ctrl Pts',(-19.775765812932,-17.1090595017616,-17.425568011292));
#69305=CARTESIAN_POINT('Ctrl Pts',(-19.782427697071,-17.1128422716382,-17.4251051148299));
#69306=CARTESIAN_POINT('Ctrl Pts',(-19.7855325616823,-17.1146157024669,
-17.4248885467968));
#69307=CARTESIAN_POINT('Ctrl Pts',(-19.7926381809225,-17.1186981864264,
-17.4243910299956));
#69308=CARTESIAN_POINT('Ctrl Pts',(-19.7966358694327,-17.1210124670493,
-17.4241097464343));
#69309=CARTESIAN_POINT('Ctrl Pts',(-19.8089993446969,-17.1282238685638,
-17.4232356395496));
#69310=CARTESIAN_POINT('Ctrl Pts',(-19.8173389552097,-17.1331652992591,
-17.422640051266));
#69311=CARTESIAN_POINT('Ctrl Pts',(-19.9078157475782,-17.1876180976281,
-17.4161156738663));
#69312=CARTESIAN_POINT('Ctrl Pts',(-19.9865225158485,-17.2425936984073,
-17.4098777262563));
#69313=CARTESIAN_POINT('Ctrl Pts',(-20.1599394870345,-17.3821460663,-17.3952247396011));
#69314=CARTESIAN_POINT('Ctrl Pts',(-20.2513337290229,-17.470295712805,-17.3867948646594));
#69315=CARTESIAN_POINT('Ctrl Pts',(-20.3724501451461,-17.6101480943695,
-17.3748732318351));
#69316=CARTESIAN_POINT('Ctrl Pts',(-20.4087696807897,-17.6557620235852,
-17.3711748599224));
#69317=CARTESIAN_POINT('Ctrl Pts',(-20.4642422251247,-17.7316611235917,
-17.3653244509211));
#69318=CARTESIAN_POINT('Ctrl Pts',(-20.4845888555995,-17.7610323120921,
-17.3631287336968));
#69319=CARTESIAN_POINT('Ctrl Pts',(-20.510199220617,-17.8000774174205,-17.3602956709622));
#69320=CARTESIAN_POINT('Ctrl Pts',(-20.5161437329624,-17.809295738289,-17.3596328756309));
#69321=CARTESIAN_POINT('Ctrl Pts',(-20.5257284581396,-17.8244157673421,
-17.3585554921701));
#69322=CARTESIAN_POINT('Ctrl Pts',(-20.5294117393818,-17.8302898068951,
-17.3581393082602));
#69323=CARTESIAN_POINT('Ctrl Pts',(-20.5364622258217,-17.8416575121252,
-17.3573384123058));
#69324=CARTESIAN_POINT('Ctrl Pts',(-20.5398333326735,-17.8471486561911,
-17.3569535592604));
#69325=CARTESIAN_POINT('Ctrl Pts',(-20.5475262651513,-17.8598088279156,
-17.3560708381274));
#69326=CARTESIAN_POINT('Ctrl Pts',(-20.5518307630405,-17.8669882992394,
-17.355573608656));
#69327=CARTESIAN_POINT('Ctrl Pts',(-20.5632211500836,-17.8862443847782,
-17.3542487915019));
#69328=CARTESIAN_POINT('Ctrl Pts',(-20.5702300778545,-17.8983662104354,
-17.3534239964177));
#69329=CARTESIAN_POINT('Ctrl Pts',(-20.6269882510109,-17.9988153189563,
-17.346662346183));
#69330=CARTESIAN_POINT('Ctrl Pts',(-20.6704578060138,-18.090547429438,-17.3409590585524));
#69331=CARTESIAN_POINT('Ctrl Pts',(-20.7617037772607,-18.3253034172797,
-17.3270884327748));
#69332=CARTESIAN_POINT('Ctrl Pts',(-20.801104883465,-18.4709561073493,-17.3191198091754));
#69333=CARTESIAN_POINT('Ctrl Pts',(-20.8309456096504,-18.6586173383895,
-17.3084711081853));
#69334=CARTESIAN_POINT('Ctrl Pts',(-20.8360618097048,-18.6978542603052,
-17.3062221383147));
#69335=CARTESIAN_POINT('Ctrl Pts',(-20.8416060205161,-18.7522165428395,
-17.3030474899831));
#69336=CARTESIAN_POINT('Ctrl Pts',(-20.8429760806296,-18.7672395279161,
-17.3021640059745));
#69337=CARTESIAN_POINT('Ctrl Pts',(-20.8450676747903,-18.7932443154418,
-17.3006220664936));
#69338=CARTESIAN_POINT('Ctrl Pts',(-20.8458643547452,-18.8042196548609,
-17.299967406966));
#69339=CARTESIAN_POINT('Ctrl Pts',(-20.8468897381119,-18.8200544988783,
-17.2990166524564));
#69340=CARTESIAN_POINT('Ctrl Pts',(-20.8471873278301,-18.8249095711491,
-17.298724300212));
#69341=CARTESIAN_POINT('Ctrl Pts',(-20.8476764826059,-18.833367196857,-17.2982134803064));
#69342=CARTESIAN_POINT('Ctrl Pts',(-20.8478755777288,-18.8369693221484,
-17.2979954343208));
#69343=CARTESIAN_POINT('Ctrl Pts',(-20.8482735902507,-18.8445206030594,
-17.2975372912288));
#69344=CARTESIAN_POINT('Ctrl Pts',(-20.8484706504524,-18.8484697967728,
-17.2972970960155));
#69345=CARTESIAN_POINT('Ctrl Pts',(-20.8489642020208,-18.8589506832107,
-17.296658100317));
#69346=CARTESIAN_POINT('Ctrl Pts',(-20.8492414963272,-18.8654831761259,
-17.2962582484209));
#69347=CARTESIAN_POINT('Ctrl Pts',(-20.8502933311974,-18.8933033080977,
-17.2945489587838));
#69348=CARTESIAN_POINT('Ctrl Pts',(-20.8507767751215,-18.9145998759567,
-17.2932244674539));
#69349=CARTESIAN_POINT('Ctrl Pts',(-20.8509781231638,-18.9410730908942,
-17.2915611068256));
#69350=CARTESIAN_POINT('Ctrl Pts',(-20.8509985064325,-18.9462471151322,
-17.2912352096919));
#69351=CARTESIAN_POINT('Ctrl Pts',(-20.851013182946,-18.9999278666397,-17.287846021773));
#69352=CARTESIAN_POINT('Ctrl Pts',(-20.8493592891962,-19.0484176143119,
-17.2847171782446));
#69353=CARTESIAN_POINT('Ctrl Pts',(-20.832613863639,-19.2926578376087,-17.2687464657044));
#69354=CARTESIAN_POINT('Ctrl Pts',(-20.7920024742,-19.485740026347,-17.2555538234773));
#69355=CARTESIAN_POINT('Ctrl Pts',(-20.724436348768,-19.6730128285728,-17.243039546343));
#69356=CARTESIAN_POINT('Ctrl Pts',(-20.7235109086517,-19.6755625069505,
-17.2428691976168));
#69357=CARTESIAN_POINT('Ctrl Pts',(-20.7225805822089,-19.6781103690637,
-17.242699000807));
#69358=CARTESIAN_POINT('Origin',(-18.734,-18.952,0.));
#69359=CARTESIAN_POINT('',(-20.7225805882177,-19.6781103526075,-16.4437314133151));
#69360=CARTESIAN_POINT('',(-20.7225805820307,-19.6781103695518,-16.6645990581914));
#69361=CARTESIAN_POINT('',(-20.7225805821191,-19.6781103693095,0.));
#69362=CARTESIAN_POINT('',(-20.8509997150765,-18.9530983468555,-16.7126937598086));
#69363=CARTESIAN_POINT('Ctrl Pts',(-20.7225805820307,-19.6781103695518,
-16.6645990581914));
#69364=CARTESIAN_POINT('Ctrl Pts',(-20.724617954831,-19.6725306668522,-16.6649758082994));
#69365=CARTESIAN_POINT('Ctrl Pts',(-20.7266318565325,-19.6669423541826,
-16.6653535212313));
#69366=CARTESIAN_POINT('Ctrl Pts',(-20.755309382627,-19.586303477032,-16.6708086650019));
#69367=CARTESIAN_POINT('Ctrl Pts',(-20.7777386604433,-19.5098199607894,
-16.6760396990613));
#69368=CARTESIAN_POINT('Ctrl Pts',(-20.8323931999723,-19.275182842516,-16.6919443777136));
#69369=CARTESIAN_POINT('Ctrl Pts',(-20.8509160191727,-19.1144173361511,
-16.7026019321524));
#69370=CARTESIAN_POINT('Ctrl Pts',(-20.8509997150765,-18.9530983468555,
-16.7126937598086));
#69371=CARTESIAN_POINT('Ctrl Pts',(-20.8509997162488,-18.9530960850687,
-16.7126939013019));
#69372=CARTESIAN_POINT('Ctrl Pts',(-20.8510131380886,-18.9271728863108,
-16.7143156094758));
#69373=CARTESIAN_POINT('Ctrl Pts',(-20.8505504063366,-18.9012505606405,
-16.7159233010165));
#69374=CARTESIAN_POINT('Ctrl Pts',(-20.8489736678282,-18.8577355730853,
-16.7185990754188));
#69375=CARTESIAN_POINT('Ctrl Pts',(-20.8481159277891,-18.8401372666953,
-16.7196748919229));
#69376=CARTESIAN_POINT('Ctrl Pts',(-20.8465415700014,-18.8144384493095,
-16.7212369878273));
#69377=CARTESIAN_POINT('Ctrl Pts',(-20.8459978380121,-18.8063284505031,
-16.7217286535888));
#69378=CARTESIAN_POINT('Ctrl Pts',(-20.8449526632468,-18.7919779884224,
-16.7225963976334));
#69379=CARTESIAN_POINT('Ctrl Pts',(-20.8444702241123,-18.7857362784398,
-16.7229730681296));
#69380=CARTESIAN_POINT('Ctrl Pts',(-20.8434611317316,-18.7733936435573,
-16.723716452697));
#69381=CARTESIAN_POINT('Ctrl Pts',(-20.8429356807584,-18.7672926842432,
-16.7240832007903));
#69382=CARTESIAN_POINT('Ctrl Pts',(-20.8418361311527,-18.7551427884005,
-16.7248121932608));
#69383=CARTESIAN_POINT('Ctrl Pts',(-20.8412624475386,-18.749093874097,-16.7251744470071));
#69384=CARTESIAN_POINT('Ctrl Pts',(-20.8398285557079,-18.7346373542702,
-16.7260386236379));
#69385=CARTESIAN_POINT('Ctrl Pts',(-20.8389440230463,-18.726232223773,-16.7265397777864));
#69386=CARTESIAN_POINT('Ctrl Pts',(-20.8360988459888,-18.7006681331952,
-16.7280602738497));
#69387=CARTESIAN_POINT('Ctrl Pts',(-20.8339785134003,-18.6835274037956,
-16.729074601943));
#69388=CARTESIAN_POINT('Ctrl Pts',(-20.8260337980322,-18.6251728964754,
-16.7325119101018));
#69389=CARTESIAN_POINT('Ctrl Pts',(-20.8192037210801,-18.584104449838,-16.7349036449326));
#69390=CARTESIAN_POINT('Ctrl Pts',(-20.7779734452175,-18.374576171713,-16.7470134350623));
#69391=CARTESIAN_POINT('Ctrl Pts',(-20.72435859662,-18.2105701549565,-16.7561209992149));
#69392=CARTESIAN_POINT('Ctrl Pts',(-20.6249327975613,-17.9980645897377,
-16.769015153791));
#69393=CARTESIAN_POINT('Ctrl Pts',(-20.5958562709737,-17.942490371582,-16.7725069951293));
#69394=CARTESIAN_POINT('Ctrl Pts',(-20.5488219970765,-17.8615568214716,
-16.7778913461385));
#69395=CARTESIAN_POINT('Ctrl Pts',(-20.5327016305221,-17.8351663400157,
-16.7796971488983));
#69396=CARTESIAN_POINT('Ctrl Pts',(-20.512161980929,-17.8031397910929,-16.7819630741043));
#69397=CARTESIAN_POINT('Ctrl Pts',(-20.5082836580815,-17.7971591852528,
-16.7823894725882));
#69398=CARTESIAN_POINT('Ctrl Pts',(-20.5021352894321,-17.7877821137658,
-16.7830633655851));
#69399=CARTESIAN_POINT('Ctrl Pts',(-20.4998854481123,-17.7843723744879,
-16.7833095281413));
#69400=CARTESIAN_POINT('Ctrl Pts',(-20.4956478280947,-17.7779903255335,
-16.7837724166871));
#69401=CARTESIAN_POINT('Ctrl Pts',(-20.4936623832969,-17.7750165327831,
-16.7839889864883));
#69402=CARTESIAN_POINT('Ctrl Pts',(-20.4890946293522,-17.7682123576569,
-16.7844865209106));
#69403=CARTESIAN_POINT('Ctrl Pts',(-20.4865073177234,-17.7643853989878,
-16.7847678204131));
#69404=CARTESIAN_POINT('Ctrl Pts',(-20.4784512076748,-17.7525530530541,
-16.7856420251302));
#69405=CARTESIAN_POINT('Ctrl Pts',(-20.4729400170964,-17.7445768748147,
-16.7862376961793));
#69406=CARTESIAN_POINT('Ctrl Pts',(-20.4106714911215,-17.6557681447812,
-16.7929390766375));
#69407=CARTESIAN_POINT('Ctrl Pts',(-20.3483849201451,-17.5789737756689,
-16.7993723401165));
#69408=CARTESIAN_POINT('Ctrl Pts',(-20.1664592961763,-17.3842341394247,
-16.8169267902971));
#69409=CARTESIAN_POINT('Ctrl Pts',(-20.0377573445236,-17.2756758282441,
-16.8280724934787));
#69410=CARTESIAN_POINT('Ctrl Pts',(-19.8712093187778,-17.166099638103,-16.8405986465004));
#69411=CARTESIAN_POINT('Ctrl Pts',(-19.844456895574,-17.1493434088667,-16.8425612660863));
#69412=CARTESIAN_POINT('Ctrl Pts',(-19.8041716999014,-17.1253483069514,
-16.8454447891522));
#69413=CARTESIAN_POINT('Ctrl Pts',(-19.790919729861,-17.1176487307524,-16.8463820970399));
#69414=CARTESIAN_POINT('Ctrl Pts',(-19.7666473131505,-17.1038964952453,
-16.8480787964603));
#69415=CARTESIAN_POINT('Ctrl Pts',(-19.7556544262716,-17.0977968607478,
-16.8488398499652));
#69416=CARTESIAN_POINT('Ctrl Pts',(-19.7382624433009,-17.0883481842936,
-16.8500325341717));
#69417=CARTESIAN_POINT('Ctrl Pts',(-19.7318995612018,-17.0849334203156,
-16.850466505087));
#69418=CARTESIAN_POINT('Ctrl Pts',(-19.7254731392043,-17.0815267933058,
-16.850902449066));
#69419=CARTESIAN_POINT('Ctrl Pts',(-19.7254270071262,-17.0815023410157,
-16.8509055783682));
#69420=CARTESIAN_POINT('Ctrl Pts',(-19.7253331168546,-17.0814525789632,
-16.8509119470292));
#69421=CARTESIAN_POINT('Ctrl Pts',(-19.7252853576638,-17.0814272688287,
-16.8509151864468));
#69422=CARTESIAN_POINT('Ctrl Pts',(-19.7251881538843,-17.081375760146,-16.8509217793332));
#69423=CARTESIAN_POINT('Ctrl Pts',(-19.7251387082889,-17.0813495612324,
-16.8509251328607));
#69424=CARTESIAN_POINT('Ctrl Pts',(-19.7250380701728,-17.0812962429013,
-16.8509319581113));
#69425=CARTESIAN_POINT('Ctrl Pts',(-19.7249868767742,-17.081269123199,-16.8509354298838));
#69426=CARTESIAN_POINT('Ctrl Pts',(-19.7248826792599,-17.0812139300446,
-16.8509424959198));
#69427=CARTESIAN_POINT('Ctrl Pts',(-19.7248296743174,-17.0811858563479,
-16.8509460902286));
#69428=CARTESIAN_POINT('Ctrl Pts',(-19.7247217876403,-17.081128720796,-16.850953405785));
#69429=CARTESIAN_POINT('Ctrl Pts',(-19.7246669050773,-17.0810996587096,
-16.8509571270772));
#69430=CARTESIAN_POINT('Ctrl Pts',(-19.7245551946518,-17.0810405107319,
-16.8509647012105));
#69431=CARTESIAN_POINT('Ctrl Pts',(-19.724498366005,-17.0810104246481,-16.8509685540922));
#69432=CARTESIAN_POINT('Ctrl Pts',(-19.7243826923224,-17.0809491917159,
-16.8509763961865));
#69433=CARTESIAN_POINT('Ctrl Pts',(-19.7243238466558,-17.0809180447727,
-16.8509803854284));
#69434=CARTESIAN_POINT('Ctrl Pts',(-19.7242040653581,-17.0808546519042,
-16.8509885051904));
#69435=CARTESIAN_POINT('Ctrl Pts',(-19.7241431290711,-17.0808224058882,
-16.8509926357406));
#69436=CARTESIAN_POINT('Ctrl Pts',(-19.7240190902981,-17.0807567753119,
-16.8510010432431));
#69437=CARTESIAN_POINT('Ctrl Pts',(-19.7239559872454,-17.0807233907268,
-16.8510053202185));
#69438=CARTESIAN_POINT('Ctrl Pts',(-19.7238275359928,-17.0806554420805,
-16.8510140258757));
#69439=CARTESIAN_POINT('Ctrl Pts',(-19.723762187258,-17.0806208780316,-16.8510184545774));
#69440=CARTESIAN_POINT('Ctrl Pts',(-19.7236291608479,-17.0805505270352,
-16.8510274693158));
#69441=CARTESIAN_POINT('Ctrl Pts',(-19.7235614857846,-17.0805147417862,
-16.8510320551578));
#69442=CARTESIAN_POINT('Ctrl Pts',(-19.7234348766143,-17.0804478021219,
-16.851040634041));
#69443=CARTESIAN_POINT('Ctrl Pts',(-19.7233759417252,-17.0804166461579,
-16.8510446271985));
#69444=CARTESIAN_POINT('Ctrl Pts',(-19.7232483209136,-17.0803491870531,
-16.8510532737683));
#69445=CARTESIAN_POINT('Ctrl Pts',(-19.7231796333278,-17.0803128843086,
-16.8510579272222));
#69446=CARTESIAN_POINT('Ctrl Pts',(-19.7230309106786,-17.0802342919276,
-16.8510680023154));
#69447=CARTESIAN_POINT('Ctrl Pts',(-19.7229508740339,-17.0801920031847,
-16.8510734239655));
#69448=CARTESIAN_POINT('Ctrl Pts',(-19.7227776033407,-17.0801004668387,
-16.8510851604592));
#69449=CARTESIAN_POINT('Ctrl Pts',(-19.7226843676137,-17.0800512206916,
-16.8510914752859));
#69450=CARTESIAN_POINT('Ctrl Pts',(-19.7224825586956,-17.0799446465905,
-16.8511051426651));
#69451=CARTESIAN_POINT('Ctrl Pts',(-19.7223739837106,-17.0798873208594,
-16.8511124951622));
#69452=CARTESIAN_POINT('Ctrl Pts',(-19.7221390256547,-17.0797632931704,
-16.8511284046293));
#69453=CARTESIAN_POINT('Ctrl Pts',(-19.7220126410725,-17.0796965946987,
-16.8511369614626));
#69454=CARTESIAN_POINT('Ctrl Pts',(-19.721726714621,-17.0795457362701,-16.8511563179702));
#69455=CARTESIAN_POINT('Ctrl Pts',(-19.7215671687158,-17.0794615838891,
-16.8511671173765));
#69456=CARTESIAN_POINT('Ctrl Pts',(-19.7156957081335,-17.0763656450527,
-16.851564493651));
#69457=CARTESIAN_POINT('Ctrl Pts',(-19.7099700060516,-17.0733799624352,
-16.8519501429257));
#69458=CARTESIAN_POINT('Ctrl Pts',(-19.6967131573479,-17.0665441091715,
-16.8528388002148));
#69459=CARTESIAN_POINT('Ctrl Pts',(-19.6891723860932,-17.0627127651934,
-16.8533411410233));
#69460=CARTESIAN_POINT('Ctrl Pts',(-19.6688197882023,-17.0525249399193,
-16.8546886564778));
#69461=CARTESIAN_POINT('Ctrl Pts',(-19.6559660359483,-17.0462528541833,
-16.8555308834503));
#69462=CARTESIAN_POINT('Ctrl Pts',(-19.5375050260952,-16.9899279627722,
-16.8632151229833));
#69463=CARTESIAN_POINT('Ctrl Pts',(-19.4279800945321,-16.9485669714425,
-16.8697402894631));
#69464=CARTESIAN_POINT('Ctrl Pts',(-19.1589136982039,-16.8716904318624,
-16.88505936679));
#69465=CARTESIAN_POINT('Ctrl Pts',(-18.997615162597,-16.8451695239618,-16.893669571053));
#69466=CARTESIAN_POINT('Ctrl Pts',(-18.8026567586164,-16.8358674841518,
-16.9048794202438));
#69467=CARTESIAN_POINT('Ctrl Pts',(-18.7703909923844,-16.8350668374245,
-16.906762104127));
#69468=CARTESIAN_POINT('Ctrl Pts',(-18.7308980986525,-16.8349899487626,
-16.9091136371913));
#69469=CARTESIAN_POINT('Ctrl Pts',(-18.7236747143635,-16.8350128569384,
-16.9095456714452));
#69470=CARTESIAN_POINT('Ctrl Pts',(-18.7123456960382,-16.8351067689632,
-16.9102264906488));
#69471=CARTESIAN_POINT('Ctrl Pts',(-18.7082398322799,-16.8351527514745,
-16.9104738976636));
#69472=CARTESIAN_POINT('Ctrl Pts',(-18.7005620656589,-16.8352610772688,
-16.9109378224223));
#69473=CARTESIAN_POINT('Ctrl Pts',(-18.6969901780054,-16.835320516735,-16.911154176116));
#69474=CARTESIAN_POINT('Ctrl Pts',(-18.6888324315153,-16.8354769242404,
-16.9116494895984));
#69475=CARTESIAN_POINT('Ctrl Pts',(-18.6842467421793,-16.8355797553682,
-16.9119287730984));
#69476=CARTESIAN_POINT('Ctrl Pts',(-18.6701369837262,-16.8359420398154,
-16.9127906574356));
#69477=CARTESIAN_POINT('Ctrl Pts',(-18.6606144566246,-16.8362508820904,
-16.9133759151013));
#69478=CARTESIAN_POINT('Ctrl Pts',(-18.5315880865436,-16.8413076614831,
-16.9213515081989));
#69479=CARTESIAN_POINT('Ctrl Pts',(-18.4127068930046,-16.8561095355057,
-16.9292186583405));
#69480=CARTESIAN_POINT('Ctrl Pts',(-18.1891141765261,-16.9034239902712,
-16.9443169102164));
#69481=CARTESIAN_POINT('Ctrl Pts',(-18.0843942606154,-16.9341843275615,
-16.9515201160467));
#69482=CARTESIAN_POINT('Ctrl Pts',(-17.9123465694994,-16.9995128164646,
-16.9633445893002));
#69483=CARTESIAN_POINT('Ctrl Pts',(-17.843650472363,-17.0298656583292,-16.9680660297628));
#69484=CARTESIAN_POINT('Ctrl Pts',(-17.7599286851908,-17.0723117678669,
-16.9738163683881));
#69485=CARTESIAN_POINT('Ctrl Pts',(-17.7432663110306,-17.0810404681722,
-16.9749607847386));
#69486=CARTESIAN_POINT('Ctrl Pts',(-17.7191978610519,-17.0940606039165,
-16.9766142811101));
#69487=CARTESIAN_POINT('Ctrl Pts',(-17.7116983322456,-17.0981765229141,
-16.9771295576006));
#69488=CARTESIAN_POINT('Ctrl Pts',(-17.6985890472135,-17.1054749523511,
-16.978030442223));
#69489=CARTESIAN_POINT('Ctrl Pts',(-17.6929685405135,-17.1086378287129,
-16.9784167463307));
#69490=CARTESIAN_POINT('Ctrl Pts',(-17.6820797469114,-17.1148310591907,
-16.9791652924963));
#69491=CARTESIAN_POINT('Ctrl Pts',(-17.6768098890246,-17.1178585097182,
-16.9795276341023));
#69492=CARTESIAN_POINT('Ctrl Pts',(-17.6642381533248,-17.1251529582114,
-16.9803922356098));
#69493=CARTESIAN_POINT('Ctrl Pts',(-17.6569486277487,-17.1294411210117,
-16.9808937250359));
#69494=CARTESIAN_POINT('Ctrl Pts',(-17.6307080097925,-17.1450899351325,
-16.9826997496359));
#69495=CARTESIAN_POINT('Ctrl Pts',(-17.6119089444366,-17.156703669194,-16.9839950615846));
#69496=CARTESIAN_POINT('Ctrl Pts',(-17.4368578876178,-17.268671144437,-16.996080703535));
#69497=CARTESIAN_POINT('Ctrl Pts',(-17.2942700190669,-17.388875794406,-17.0060131877644));
#69498=CARTESIAN_POINT('Ctrl Pts',(-17.1152583045133,-17.5853343146682,
-17.020502549017));
#69499=CARTESIAN_POINT('Ctrl Pts',(-17.0647361392392,-17.6475246522873,
-17.0249059401472));
#69500=CARTESIAN_POINT('Ctrl Pts',(-16.9967760617693,-17.7416121664945,
-17.0315450959902));
#69501=CARTESIAN_POINT('Ctrl Pts',(-16.9764405726915,-17.7713348355755,
-17.033639694912));
#69502=CARTESIAN_POINT('Ctrl Pts',(-16.9528175910555,-17.8078260828551,
-17.0362266564704));
#69503=CARTESIAN_POINT('Ctrl Pts',(-16.948794117962,-17.8141139417414,-17.0366729585263));
#69504=CARTESIAN_POINT('Ctrl Pts',(-16.9425809571116,-17.8239378959757,
-17.0373712988066));
#69505=CARTESIAN_POINT('Ctrl Pts',(-16.9403682463315,-17.8274594585754,
-17.0376218396951));
#69506=CARTESIAN_POINT('Ctrl Pts',(-16.9362776842916,-17.8340124367917,
-17.0380884819651));
#69507=CARTESIAN_POINT('Ctrl Pts',(-16.9343971097411,-17.8370420848076,
-17.0383043998584));
#69508=CARTESIAN_POINT('Ctrl Pts',(-16.9301549094423,-17.8439150585005,
-17.0387946140153));
#69509=CARTESIAN_POINT('Ctrl Pts',(-16.9277979197851,-17.8477611703697,
-17.0390692079335));
#69510=CARTESIAN_POINT('Ctrl Pts',(-16.9217434753202,-17.8577119995996,
-17.0397802858899));
#69511=CARTESIAN_POINT('Ctrl Pts',(-16.918064602519,-17.8638278776182,-17.0402179373027));
#69512=CARTESIAN_POINT('Ctrl Pts',(-16.8956519085938,-17.9015176509563,
-17.0429182214243));
#69513=CARTESIAN_POINT('Ctrl Pts',(-16.8777123346157,-17.9335538309219,
-17.0452271610942));
#69514=CARTESIAN_POINT('Ctrl Pts',(-16.7812822564166,-18.1167764476263,
-17.0584410732572));
#69515=CARTESIAN_POINT('Ctrl Pts',(-16.7204315137949,-18.2765372061968,
-17.0699344810719));
#69516=CARTESIAN_POINT('Ctrl Pts',(-16.6563721613909,-18.5345434963653,
-17.0872113786762));
#69517=CARTESIAN_POINT('Ctrl Pts',(-16.6396562682331,-18.628679777685,-17.0932786383464));
#69518=CARTESIAN_POINT('Ctrl Pts',(-16.6270442361961,-18.7449141568,-17.100460398315));
#69519=CARTESIAN_POINT('Ctrl Pts',(-16.6250581161765,-18.766227772416,-17.1017650734341));
#69520=CARTESIAN_POINT('Ctrl Pts',(-16.6226955460807,-18.7965531682359,
-17.1036046351112));
#69521=CARTESIAN_POINT('Ctrl Pts',(-16.6220529425179,-18.8055423441286,
-17.1041478411478));
#69522=CARTESIAN_POINT('Ctrl Pts',(-16.6210439472005,-18.8210484167295,
-17.1050813395013));
#69523=CARTESIAN_POINT('Ctrl Pts',(-16.6206502605931,-18.8275633548632,
-17.1054724834599));
#69524=CARTESIAN_POINT('Ctrl Pts',(-16.6199544879947,-18.8400350697693,
-17.1062192514445));
#69525=CARTESIAN_POINT('Ctrl Pts',(-16.6196474346163,-18.8459914965316,
-17.1065750276583));
#69526=CARTESIAN_POINT('Ctrl Pts',(-16.6189150607854,-18.8614706606631,
-17.1074973603473));
#69527=CARTESIAN_POINT('Ctrl Pts',(-16.6185288738891,-18.8709951823553,
-17.1080626861599));
#69528=CARTESIAN_POINT('Ctrl Pts',(-16.6174336371598,-18.90341491521,-17.1099797258332));
#69529=CARTESIAN_POINT('Ctrl Pts',(-16.6170318270614,-18.9263193886757,
-17.111321831094));
#69530=CARTESIAN_POINT('Ctrl Pts',(-16.616770440827,-19.1258378891143,-17.1229165409291));
#69531=CARTESIAN_POINT('Ctrl Pts',(-16.6386384415009,-19.30178164891,-17.1324069158117));
#69532=CARTESIAN_POINT('Ctrl Pts',(-16.7033227085838,-19.5565424655574,
-17.1467111447771));
#69533=CARTESIAN_POINT('Ctrl Pts',(-16.7296225909621,-19.6387246227305,
-17.1514333719584));
#69534=CARTESIAN_POINT('Ctrl Pts',(-16.774488171413,-19.7541333054791,-17.1585044308519));
#69535=CARTESIAN_POINT('Ctrl Pts',(-16.789051571883,-19.7888271415139,-17.1606901432653));
#69536=CARTESIAN_POINT('Ctrl Pts',(-16.8076413561941,-19.8300025809461,
-17.1633781442775));
#69537=CARTESIAN_POINT('Ctrl Pts',(-16.8107890970171,-19.8368762486663,
-17.1638300670417));
#69538=CARTESIAN_POINT('Ctrl Pts',(-16.8157341570418,-19.8475236603388,
-17.164535303506));
#69539=CARTESIAN_POINT('Ctrl Pts',(-16.8175059857057,-19.851309269922,-17.1647870716465));
#69540=CARTESIAN_POINT('Ctrl Pts',(-16.8208093596306,-19.8583130119818,
-17.1652548161795));
#69541=CARTESIAN_POINT('Ctrl Pts',(-16.8223378247949,-19.8615325334425,
-17.1654706015937));
#69542=CARTESIAN_POINT('Ctrl Pts',(-16.8258074231513,-19.8687934283163,
-17.1659589922363));
#69543=CARTESIAN_POINT('Ctrl Pts',(-16.8277532579283,-19.8728324809812,
-17.1662318856367));
#69544=CARTESIAN_POINT('Ctrl Pts',(-16.8335218106989,-19.8847098719027,
-17.1670378795736));
#69545=CARTESIAN_POINT('Ctrl Pts',(-16.8373800957909,-19.8925306938647,
-17.1675731172341));
#69546=CARTESIAN_POINT('Ctrl Pts',(-16.8651908430789,-19.9480366110126,
-17.1714028920744));
#69547=CARTESIAN_POINT('Ctrl Pts',(-16.8908884514517,-19.9948208753516,
-17.1747945565816));
#69548=CARTESIAN_POINT('Ctrl Pts',(-16.9273694294093,-20.0556686479437,
-17.1793797742828));
#69549=CARTESIAN_POINT('Ctrl Pts',(-16.9366033100326,-20.0706436509309,
-17.1805228082439));
#69550=CARTESIAN_POINT('Ctrl Pts',(-16.9719941498716,-20.126468915809,-17.1848347503723));
#69551=CARTESIAN_POINT('Ctrl Pts',(-16.9993654293923,-20.1665305753368,
-17.1880324235468));
#69552=CARTESIAN_POINT('Ctrl Pts',(-17.0928605092622,-20.2937580924798,
-17.1984619701991));
#69553=CARTESIAN_POINT('Ctrl Pts',(-17.1643723170991,-20.3767547191093,
-17.2056947721282));
#69554=CARTESIAN_POINT('Ctrl Pts',(-17.28107317332,-20.4926910179978,-17.2162684264486));
#69555=CARTESIAN_POINT('Ctrl Pts',(-17.3216672997978,-20.5299868002108,
-17.2197576559781));
#69556=CARTESIAN_POINT('Ctrl Pts',(-17.3898211222542,-20.5878633481733,
-17.2253153558215));
#69557=CARTESIAN_POINT('Ctrl Pts',(-17.4165057313679,-20.6094301848731,
-17.227422267129));
#69558=CARTESIAN_POINT('Ctrl Pts',(-17.4522728772119,-20.636927715525,-17.2301588454392));
#69559=CARTESIAN_POINT('Ctrl Pts',(-17.4608922188826,-20.6434497947852,
-17.2308118548246));
#69560=CARTESIAN_POINT('Ctrl Pts',(-17.4750937102978,-20.6540257155861,
-17.2318773604536));
#69561=CARTESIAN_POINT('Ctrl Pts',(-17.4806463151711,-20.6581187312863,
-17.2322913861736));
#69562=CARTESIAN_POINT('Ctrl Pts',(-17.491434844316,-20.6659902342917,-17.2330909019716));
#69563=CARTESIAN_POINT('Ctrl Pts',(-17.4966682378424,-20.6697720457467,
-17.2334765184006));
#69564=CARTESIAN_POINT('Ctrl Pts',(-17.508794110066,-20.6784504068582,-17.2343649355882));
#69565=CARTESIAN_POINT('Ctrl Pts',(-17.5156988128512,-20.6833297492462,
-17.2348670702967));
#69566=CARTESIAN_POINT('Ctrl Pts',(-17.5343516583174,-20.6963443035617,
-17.2362136679501));
#69567=CARTESIAN_POINT('Ctrl Pts',(-17.5461533725958,-20.7044022362873,
-17.2370551895728));
#69568=CARTESIAN_POINT('Ctrl Pts',(-17.6551775605434,-20.7772339086621,
-17.2447362506206));
#69569=CARTESIAN_POINT('Ctrl Pts',(-17.7575296766802,-20.8339797147863,
-17.2512591827382));
#69570=CARTESIAN_POINT('Ctrl Pts',(-18.0124219919546,-20.9488725005736,
-17.2665652530841));
#69571=CARTESIAN_POINT('Ctrl Pts',(-18.1679882457019,-20.9984098918762,
-17.2751653043777));
#69572=CARTESIAN_POINT('Ctrl Pts',(-18.3595750826726,-21.0358790289379,
-17.2863743156676));
#69573=CARTESIAN_POINT('Ctrl Pts',(-18.3916170567969,-21.0413825606828,
-17.288270383163));
#69574=CARTESIAN_POINT('Ctrl Pts',(-18.4309324842728,-21.0472067901356,
-17.2906368068298));
#69575=CARTESIAN_POINT('Ctrl Pts',(-18.4380992549803,-21.0482309410399,
-17.2910697957271));
#69576=CARTESIAN_POINT('Ctrl Pts',(-18.4493423236919,-21.0497788007801,
-17.2917517878829));
#69577=CARTESIAN_POINT('Ctrl Pts',(-18.4534152114387,-21.0503274447643,
-17.2919994053521));
#69578=CARTESIAN_POINT('Ctrl Pts',(-18.4610309745763,-21.0513307671587,
-17.2924635078914));
#69579=CARTESIAN_POINT('Ctrl Pts',(-18.4645734119163,-21.0517883397518,
-17.2926798275905));
#69580=CARTESIAN_POINT('Ctrl Pts',(-18.4726622072493,-21.0528123543676,
-17.2931747771159));
#69581=CARTESIAN_POINT('Ctrl Pts',(-18.4772092407399,-21.0533730024036,
-17.293453728814));
#69582=CARTESIAN_POINT('Ctrl Pts',(-18.4911905548546,-21.0550508380933,
-17.2943135949957));
#69583=CARTESIAN_POINT('Ctrl Pts',(-18.5006304132317,-21.0561192652739,
-17.2948971486615));
#69584=CARTESIAN_POINT('Ctrl Pts',(-18.5854810223028,-21.0651448653258,
-17.3001673611239));
#69585=CARTESIAN_POINT('Ctrl Pts',(-18.6612537132996,-21.0691075897821,
-17.3050487058846));
#69586=CARTESIAN_POINT('Ctrl Pts',(-18.9219965594145,-21.0687299178882,
-17.3221015383477));
#69587=CARTESIAN_POINT('Ctrl Pts',(-19.1061342193762,-21.0442294878566,
-17.3344988871995));
#69588=CARTESIAN_POINT('Ctrl Pts',(-19.3361763460763,-20.9822486172945,
-17.3495263661884));
#69589=CARTESIAN_POINT('Ctrl Pts',(-19.3870659874507,-20.9664556124278,
-17.3528279537341));
#69590=CARTESIAN_POINT('Ctrl Pts',(-19.449137866429,-20.9445923063702,-17.3568296339874));
#69591=CARTESIAN_POINT('Ctrl Pts',(-19.4609291538828,-20.9403209708827,
-17.3575886868804));
#69592=CARTESIAN_POINT('Ctrl Pts',(-19.4795054214978,-20.9334044716238,
-17.3587829174995));
#69593=CARTESIAN_POINT('Ctrl Pts',(-19.4863157631402,-20.930828696034,-17.3592203989941));
#69594=CARTESIAN_POINT('Ctrl Pts',(-19.4990578944801,-20.9259341372074,
-17.3600383309089));
#69595=CARTESIAN_POINT('Ctrl Pts',(-19.5049927555579,-20.9236236284308,
-17.360419053224));
#69596=CARTESIAN_POINT('Ctrl Pts',(-19.5182499787068,-20.9183934271379,
-17.3612690029372));
#69597=CARTESIAN_POINT('Ctrl Pts',(-19.5255666661395,-20.9154595374035,
-17.3617377465269));
#69598=CARTESIAN_POINT('Ctrl Pts',(-19.5440619417602,-20.9079230021293,
-17.3629218690996));
#69599=CARTESIAN_POINT('Ctrl Pts',(-19.5552179008716,-20.9032653095175,
-17.3636353825342));
#69600=CARTESIAN_POINT('Ctrl Pts',(-19.6186384189793,-20.876146536511,-17.3676884087989));
#69601=CARTESIAN_POINT('Ctrl Pts',(-19.6700234558743,-20.8516804855319,
-17.3709588146022));
#69602=CARTESIAN_POINT('Ctrl Pts',(-19.744123272148,-20.8126614410897,-17.3756896257241));
#69603=CARTESIAN_POINT('Ctrl Pts',(-19.7676428155683,-20.7996992781501,
-17.3771936400324));
#69604=CARTESIAN_POINT('Ctrl Pts',(-19.8912853531918,-20.7284570932604,
-17.3851311464127));
#69605=CARTESIAN_POINT('Ctrl Pts',(-19.9867437427206,-20.662480368478,-17.3913560778331));
#69606=CARTESIAN_POINT('Ctrl Pts',(-20.1382166992282,-20.5382755794598,
-17.4020349591394));
#69607=CARTESIAN_POINT('Ctrl Pts',(-20.1971741751657,-20.4840620368269,
-17.406436719338));
#69608=CARTESIAN_POINT('Ctrl Pts',(-20.277994110509,-20.4008158256283,-17.4130736571843));
#69609=CARTESIAN_POINT('Ctrl Pts',(-20.3024071722651,-20.3743514699397,
-17.4151677775558));
#69610=CARTESIAN_POINT('Ctrl Pts',(-20.3310517304236,-20.3416656034103,
-17.4177542081874));
#69611=CARTESIAN_POINT('Ctrl Pts',(-20.3359416575026,-20.3360258816741,
-17.418200479953));
#69612=CARTESIAN_POINT('Ctrl Pts',(-20.3435094272081,-20.3272038759969,
-17.4188987830594));
#69613=CARTESIAN_POINT('Ctrl Pts',(-20.3462079462934,-20.3240392975618,
-17.4191493173223));
#69614=CARTESIAN_POINT('Ctrl Pts',(-20.3512028609173,-20.318146632908,-17.4196159536965));
#69615=CARTESIAN_POINT('Ctrl Pts',(-20.3535016950404,-20.3154206889733,
-17.4198318723601));
#69616=CARTESIAN_POINT('Ctrl Pts',(-20.3586930877582,-20.3092331119848,
-17.4203220966116));
#69617=CARTESIAN_POINT('Ctrl Pts',(-20.3615814610908,-20.305768051152,-17.4205966999062));
#69618=CARTESIAN_POINT('Ctrl Pts',(-20.3701034798719,-20.2954778465404,
-17.4214123466882));
#69619=CARTESIAN_POINT('Ctrl Pts',(-20.3757053452268,-20.288626677189,-17.4219556028854));
#69620=CARTESIAN_POINT('Ctrl Pts',(-20.4168973094689,-20.2375986553026,
-17.4260020148012));
#69621=CARTESIAN_POINT('Ctrl Pts',(-20.4507386861598,-20.1920460965375,
-17.4296148682213));
#69622=CARTESIAN_POINT('Ctrl Pts',(-20.517596219775,-20.0940618788603,-17.4372975613278));
#69623=CARTESIAN_POINT('Ctrl Pts',(-20.5502247308369,-20.0414255110625,
-17.4413751905982));
#69624=CARTESIAN_POINT('Ctrl Pts',(-20.6341054112911,-19.891840852066,-17.4527033103477));
#69625=CARTESIAN_POINT('Ctrl Pts',(-20.6802113289033,-19.7922180217654,
-17.4599518896997));
#69626=CARTESIAN_POINT('Ctrl Pts',(-20.7198023112215,-19.6856855302226,
-17.4672586538775));
#69627=CARTESIAN_POINT('Ctrl Pts',(-20.7211968761186,-19.6818998908439,
-17.467517754415));
#69628=CARTESIAN_POINT('Ctrl Pts',(-20.7225805818549,-19.6781103700332,
-17.4677765722177));
#69629=CARTESIAN_POINT('',(-20.8509993557814,-18.9503484488822,-16.4878149381751));
#69630=CARTESIAN_POINT('Ctrl Pts',(-20.7225805822089,-19.6781103690637,
-17.242699000807));
#69631=CARTESIAN_POINT('Ctrl Pts',(-20.7071866862069,-19.7202692528619,
-17.2398827936462));
#69632=CARTESIAN_POINT('Ctrl Pts',(-20.690454937598,-19.7619308775447,-17.2371085597985));
#69633=CARTESIAN_POINT('Ctrl Pts',(-20.6673796263601,-19.8144898843245,
-17.2336175936552));
#69634=CARTESIAN_POINT('Ctrl Pts',(-20.6622477609682,-19.8259028338721,
-17.2328600682927));
#69635=CARTESIAN_POINT('Ctrl Pts',(-20.6539422314611,-19.8439444038136,
-17.2316632398376));
#69636=CARTESIAN_POINT('Ctrl Pts',(-20.6508347871509,-19.8506030227701,
-17.231221670051));
#69637=CARTESIAN_POINT('Ctrl Pts',(-20.6449719417752,-19.8629971034382,
-17.2303999732908));
#69638=CARTESIAN_POINT('Ctrl Pts',(-20.642225237177,-19.8687365653734,-17.2300195510647));
#69639=CARTESIAN_POINT('Ctrl Pts',(-20.6360566856785,-19.8814784045976,
-17.2291751572373));
#69640=CARTESIAN_POINT('Ctrl Pts',(-20.6326219514571,-19.8884744673926,
-17.2287116400382));
#69641=CARTESIAN_POINT('Ctrl Pts',(-20.6224963090696,-19.9088142493045,
-17.2273642520349));
#69642=CARTESIAN_POINT('Ctrl Pts',(-20.6157027234671,-19.9221065377609,
-17.2264839788105));
#69643=CARTESIAN_POINT('Ctrl Pts',(-20.5587597245865,-20.0306717084962,
-17.2192939450419));
#69644=CARTESIAN_POINT('Ctrl Pts',(-20.5015468824836,-20.1220697236977,
-17.2132499861037));
#69645=CARTESIAN_POINT('Ctrl Pts',(-20.358246833973,-20.316327360521,-17.1999842110649));
#69646=CARTESIAN_POINT('Ctrl Pts',(-20.2688620494572,-20.4161593055845,
-17.1928654177092));
#69647=CARTESIAN_POINT('Ctrl Pts',(-20.1586099418722,-20.5180283742549,
-17.1845194666834));
#69648=CARTESIAN_POINT('Ctrl Pts',(-20.1464267508641,-20.5290253673553,
-17.1836022384472));
#69649=CARTESIAN_POINT('Ctrl Pts',(-20.0943129960234,-20.5749768186359,
-17.1796939028036));
#69650=CARTESIAN_POINT('Ctrl Pts',(-20.0532066678058,-20.6085620917094,
-17.1766481849095));
#69651=CARTESIAN_POINT('Ctrl Pts',(-20.0039435205832,-20.6458146936984,
-17.1729828937423));
#69652=CARTESIAN_POINT('Ctrl Pts',(-19.9969687336073,-20.6510216991269,
-17.1724636086201));
#69653=CARTESIAN_POINT('Ctrl Pts',(-19.9863559594371,-20.6588431735676,
-17.1716726166858));
#69654=CARTESIAN_POINT('Ctrl Pts',(-19.9827413591033,-20.6614894224618,
-17.1714030646887));
#69655=CARTESIAN_POINT('Ctrl Pts',(-19.9762362410141,-20.6662201789241,
-17.1709176382968));
#69656=CARTESIAN_POINT('Ctrl Pts',(-19.9733488372088,-20.6683088765515,
-17.1707020588194));
#69657=CARTESIAN_POINT('Ctrl Pts',(-19.967061127155,-20.6728331558745,-17.1702323444344));
#69658=CARTESIAN_POINT('Ctrl Pts',(-19.9636589172788,-20.6752659226353,
-17.1699780273047));
#69659=CARTESIAN_POINT('Ctrl Pts',(-19.954076393472,-20.6820751266686,-17.1692613320313));
#69660=CARTESIAN_POINT('Ctrl Pts',(-19.9478798457932,-20.6864284550889,
-17.1687974193406));
#69661=CARTESIAN_POINT('Ctrl Pts',(-19.9105768638137,-20.712337509496,-17.1660025855319));
#69662=CARTESIAN_POINT('Ctrl Pts',(-19.87892237179,-20.7330877619598,-17.1636223318261));
#69663=CARTESIAN_POINT('Ctrl Pts',(-19.7726421312894,-20.7987528646892,
-17.1556460148323));
#69664=CARTESIAN_POINT('Ctrl Pts',(-19.6958035077543,-20.839910409374,-17.1499068520919));
#69665=CARTESIAN_POINT('Ctrl Pts',(-19.4572948563072,-20.9493163566282,
-17.1325694314782));
#69666=CARTESIAN_POINT('Ctrl Pts',(-19.2894380187928,-21.0023512103457,
-17.1210591786638));
#69667=CARTESIAN_POINT('Ctrl Pts',(-19.0943178486237,-21.0382380192877,
-17.1088476171765));
#69668=CARTESIAN_POINT('Ctrl Pts',(-19.0716297582314,-21.0420297215623,
-17.1074435045073));
#69669=CARTESIAN_POINT('Ctrl Pts',(-19.0394421739339,-21.0468711742535,
-17.1054731158105));
#69670=CARTESIAN_POINT('Ctrl Pts',(-19.0299910750183,-21.0482274319636,
-17.1048971817548));
#69671=CARTESIAN_POINT('Ctrl Pts',(-19.01461882742,-21.0503273528613,-17.1039645972939));
#69672=CARTESIAN_POINT('Ctrl Pts',(-19.008703218845,-21.051109989676,-17.103606718715));
#69673=CARTESIAN_POINT('Ctrl Pts',(-18.996312872,-21.0526959616169,-17.1028592026194));
#69674=CARTESIAN_POINT('Ctrl Pts',(-18.989837561471,-21.0534943991314,-17.1024697234617));
#69675=CARTESIAN_POINT('Ctrl Pts',(-18.9744229206164,-21.0553227971764,
-17.1015453145216));
#69676=CARTESIAN_POINT('Ctrl Pts',(-18.9654804646222,-21.0563257276822,
-17.1010112420568));
#69677=CARTESIAN_POINT('Ctrl Pts',(-18.935326154409,-21.059513103711,-17.0992175417359));
#69678=CARTESIAN_POINT('Ctrl Pts',(-18.9140873320884,-21.0614341194959,
-17.0979661977834));
#69679=CARTESIAN_POINT('Ctrl Pts',(-18.7982699741764,-21.0701475770386,
-17.0912026408854));
#69680=CARTESIAN_POINT('Ctrl Pts',(-18.7033405889997,-21.070901323857,-17.0858836269407));
#69681=CARTESIAN_POINT('Ctrl Pts',(-18.4394889542103,-21.0552535595164,
-17.071340366986));
#69682=CARTESIAN_POINT('Ctrl Pts',(-18.2721439774644,-21.0249423035023,
-17.0624221720012));
#69683=CARTESIAN_POINT('Ctrl Pts',(-18.0737080529918,-20.9637563220821,
-17.0505790012312));
#69684=CARTESIAN_POINT('Ctrl Pts',(-18.0375090321643,-20.9515121601701,
-17.0483619499862));
#69685=CARTESIAN_POINT('Ctrl Pts',(-17.9948825451487,-20.9357960135558,
-17.0456614960739));
#69686=CARTESIAN_POINT('Ctrl Pts',(-17.9881143132747,-20.9332611575503,
-17.0452299896042));
#69687=CARTESIAN_POINT('Ctrl Pts',(-17.9771174268945,-20.9290782400852,
-17.0445242321988));
#69688=CARTESIAN_POINT('Ctrl Pts',(-17.9728807944107,-20.9274511259182,
-17.0442512042675));
#69689=CARTESIAN_POINT('Ctrl Pts',(-17.9653227269763,-20.9245204640644,
-17.043762052238));
#69690=CARTESIAN_POINT('Ctrl Pts',(-17.9619993258327,-20.9232221310761,
-17.0435462428319));
#69691=CARTESIAN_POINT('Ctrl Pts',(-17.9548275239862,-20.9203994477586,
-17.0430789581784));
#69692=CARTESIAN_POINT('Ctrl Pts',(-17.9509803611275,-20.9188722321941,
-17.0428273165514));
#69693=CARTESIAN_POINT('Ctrl Pts',(-17.9402917488547,-20.9145928238902,
-17.0421255088));
#69694=CARTESIAN_POINT('Ctrl Pts',(-17.9334602411006,-20.9118161829777,
-17.0416739067873));
#69695=CARTESIAN_POINT('Ctrl Pts',(-17.8947048219833,-20.8958277432965,
-17.039095154228));
#69696=CARTESIAN_POINT('Ctrl Pts',(-17.8630955614699,-20.8818724911,-17.0369269617804));
#69697=CARTESIAN_POINT('Ctrl Pts',(-17.7641898542309,-20.83528171978,-17.0299668299418));
#69698=CARTESIAN_POINT('Ctrl Pts',(-17.6982762974552,-20.7998518963342,
-17.0250666955627));
#69699=CARTESIAN_POINT('Ctrl Pts',(-17.4686460672905,-20.6602696858083,
-17.0073424438745));
#69700=CARTESIAN_POINT('Ctrl Pts',(-17.3175009378047,-20.5372027735794,
-16.994526052063));
#69701=CARTESIAN_POINT('Ctrl Pts',(-17.1708028446326,-20.3797783180298,
-16.9813057681638));
#69702=CARTESIAN_POINT('Ctrl Pts',(-17.1566170577805,-20.364090427883,-16.9800162855291));
#69703=CARTESIAN_POINT('Ctrl Pts',(-17.137192247565,-20.3419506986549,-16.9782343438223));
#69704=CARTESIAN_POINT('Ctrl Pts',(-17.1317528823488,-20.3356770287819,
-16.9777335321091));
#69705=CARTESIAN_POINT('Ctrl Pts',(-17.1224225354394,-20.3247867729303,
-16.9768712312965));
#69706=CARTESIAN_POINT('Ctrl Pts',(-17.1185141624667,-20.3201852791619,
-16.9765090250333));
#69707=CARTESIAN_POINT('Ctrl Pts',(-17.1104566484757,-20.3106161623903,
-16.9757601894134));
#69708=CARTESIAN_POINT('Ctrl Pts',(-17.1063104930697,-20.3056460990419,
-16.9753736847491));
#69709=CARTESIAN_POINT('Ctrl Pts',(-17.0966453061623,-20.2939516686291,
-16.9744698764629));
#69710=CARTESIAN_POINT('Ctrl Pts',(-17.0911447734072,-20.2872121113402,
-16.9739533276104));
#69711=CARTESIAN_POINT('Ctrl Pts',(-17.0733833441665,-20.2651738996425,
-16.9722780336536));
#69712=CARTESIAN_POINT('Ctrl Pts',(-17.061293164061,-20.2497385127684,-16.9711261320998));
#69713=CARTESIAN_POINT('Ctrl Pts',(-17.0003348531068,-20.1696462749427,
-16.9652542428423));
#69714=CARTESIAN_POINT('Ctrl Pts',(-16.9549916123088,-20.1023862495792,
-16.960673051698));
#69715=CARTESIAN_POINT('Ctrl Pts',(-16.8275352258754,-19.8876892612267,
-16.9468346645544));
#69716=CARTESIAN_POINT('Ctrl Pts',(-16.7590966086046,-19.732942507968,-16.9379622994223));
#69717=CARTESIAN_POINT('Ctrl Pts',(-16.693950348518,-19.5201514423581,-16.9254531481011));
#69718=CARTESIAN_POINT('Ctrl Pts',(-16.6801381357566,-19.4679932502747,
-16.9223592526132));
#69719=CARTESIAN_POINT('Ctrl Pts',(-16.6664201032264,-19.4068393105263,
-16.9186401764896));
#69720=CARTESIAN_POINT('Ctrl Pts',(-16.6645594797102,-19.3982973839974,
-16.9181186432813));
#69721=CARTESIAN_POINT('Ctrl Pts',(-16.661823846647,-19.3853533563472,-16.9173248934283));
#69722=CARTESIAN_POINT('Ctrl Pts',(-16.6609098159649,-19.3809594735953,
-16.917054854149));
#69723=CARTESIAN_POINT('Ctrl Pts',(-16.6592949574965,-19.3730708857045,
-16.9165689095406));
#69724=CARTESIAN_POINT('Ctrl Pts',(-16.6585889778861,-19.3695772900585,
-16.9163533019061));
#69725=CARTESIAN_POINT('Ctrl Pts',(-16.6570749505426,-19.3619863167144,
-16.9158839466009));
#69726=CARTESIAN_POINT('Ctrl Pts',(-16.6562702140935,-19.3578883799985,
-16.9156300190016));
#69727=CARTESIAN_POINT('Ctrl Pts',(-16.6540458423031,-19.3463813039791,
-16.9149154975508));
#69728=CARTESIAN_POINT('Ctrl Pts',(-16.6526536943265,-19.3389670050186,
-16.9144533837424));
#69729=CARTESIAN_POINT('Ctrl Pts',(-16.6446066028301,-19.2948098084948,
-16.9116915464598));
#69730=CARTESIAN_POINT('Ctrl Pts',(-16.6388855588433,-19.2579058937774,
-16.9093438074189));
#69731=CARTESIAN_POINT('Ctrl Pts',(-16.6233337069865,-19.1364482469166,
-16.9015292338294));
#69732=CARTESIAN_POINT('Ctrl Pts',(-16.6176256454316,-19.051453917579,-16.8959251206881));
#69733=CARTESIAN_POINT('Ctrl Pts',(-16.6158406826574,-18.78818729055,-16.878533024447));
#69734=CARTESIAN_POINT('Ctrl Pts',(-16.6371296155216,-18.6105434024813,
-16.8668240609378));
#69735=CARTESIAN_POINT('Ctrl Pts',(-16.6859698298717,-18.4155483783197,
-16.8544535671671));
#69736=CARTESIAN_POINT('Ctrl Pts',(-16.6918609646271,-18.3935412781592,
-16.8530631262047));
#69737=CARTESIAN_POINT('Ctrl Pts',(-16.7007138570992,-18.362485854435,-16.8511084190362));
#69738=CARTESIAN_POINT('Ctrl Pts',(-16.7033830170029,-18.3533564167923,
-16.8505347020114));
#69739=CARTESIAN_POINT('Ctrl Pts',(-16.7078248126257,-18.3385355447495,
-16.8496047265275));
#69740=CARTESIAN_POINT('Ctrl Pts',(-16.7095600960045,-18.3328331371699,
-16.8492472534786));
#69741=CARTESIAN_POINT('Ctrl Pts',(-16.7132468937457,-18.3208989578979,
-16.8484998057258));
#69742=CARTESIAN_POINT('Ctrl Pts',(-16.7152032074452,-18.314668725369,-16.8481099928008));
#69743=CARTESIAN_POINT('Ctrl Pts',(-16.7199334445207,-18.2998447620535,
-16.8471833733078));
#69744=CARTESIAN_POINT('Ctrl Pts',(-16.7227336023176,-18.2912594868768,
-16.846647435122));
#69745=CARTESIAN_POINT('Ctrl Pts',(-16.7323900265568,-18.2622831702968,
-16.8448407869392));
#69746=CARTESIAN_POINT('Ctrl Pts',(-16.7395022823547,-18.2419783838035,
-16.8435785272793));
#69747=CARTESIAN_POINT('Ctrl Pts',(-16.8090401333256,-18.0527504743123,
-16.8318408310221));
#69748=CARTESIAN_POINT('Ctrl Pts',(-16.8924688536244,-17.8923348809369,
-16.8221685232437));
#69749=CARTESIAN_POINT('Ctrl Pts',(-17.0635436363908,-17.6460073937686,
-16.8058446646909));
#69750=CARTESIAN_POINT('Ctrl Pts',(-17.1401008123895,-17.5536015661253,
-16.7992692549738));
#69751=CARTESIAN_POINT('Ctrl Pts',(-17.230717692082,-17.4613887419886,-16.7916073449943));
#69752=CARTESIAN_POINT('Ctrl Pts',(-17.2374355232953,-17.454644204198,-16.7910399395474));
#69753=CARTESIAN_POINT('Ctrl Pts',(-17.2474561487413,-17.4447185388798,
-16.790194038014));
#69754=CARTESIAN_POINT('Ctrl Pts',(-17.25072426686,-17.4415023590478,-16.7899182289783));
#69755=CARTESIAN_POINT('Ctrl Pts',(-17.2565570365676,-17.4357994687324,
-16.7894260507636));
#69756=CARTESIAN_POINT('Ctrl Pts',(-17.2591175591865,-17.4333086071344,
-16.789210012053));
#69757=CARTESIAN_POINT('Ctrl Pts',(-17.2646356565874,-17.4279677511664,
-16.7887444657326));
#69758=CARTESIAN_POINT('Ctrl Pts',(-17.2675951807656,-17.4251199213295,
-16.7884948036104));
#69759=CARTESIAN_POINT('Ctrl Pts',(-17.2757860291863,-17.4172839794755,
-16.7878039492048));
#69760=CARTESIAN_POINT('Ctrl Pts',(-17.281034585023,-17.4123140749686,-16.7873613917444));
#69761=CARTESIAN_POINT('Ctrl Pts',(-17.3099070969077,-17.3852535322104,
-16.7849280974778));
#69762=CARTESIAN_POINT('Ctrl Pts',(-17.3340081094426,-17.3636809096826,
-16.782901456387));
#69763=CARTESIAN_POINT('Ctrl Pts',(-17.4824025498713,-17.236856144322,-16.7704995961213));
#69764=CARTESIAN_POINT('Ctrl Pts',(-17.6180060813219,-17.1456854922775,
-16.7595313373077));
#69765=CARTESIAN_POINT('Ctrl Pts',(-17.8665964558168,-17.0173249683642,
-16.7412563215257));
#69766=CARTESIAN_POINT('Ctrl Pts',(-17.9747506811773,-16.9723776410568,
-16.7338093065157));
#69767=CARTESIAN_POINT('Ctrl Pts',(-18.0996607031708,-16.9322212624601,
-16.725798119577));
#69768=CARTESIAN_POINT('Ctrl Pts',(-18.1132852745798,-16.9279926538168,
-16.7249316381733));
#69769=CARTESIAN_POINT('Ctrl Pts',(-18.1350445415138,-16.9214796926512,
-16.7235592414817));
#69770=CARTESIAN_POINT('Ctrl Pts',(-18.1431517848276,-16.9191058193637,
-16.7230504107868));
#69771=CARTESIAN_POINT('Ctrl Pts',(-18.1574792978406,-16.9150035458274,
-16.722155532609));
#69772=CARTESIAN_POINT('Ctrl Pts',(-18.1636936307481,-16.9132549642114,
-16.7217688313049));
#69773=CARTESIAN_POINT('Ctrl Pts',(-18.1765673585127,-16.9096960380549,
-16.7209706665603));
#69774=CARTESIAN_POINT('Ctrl Pts',(-18.1832278091489,-16.9078897734488,
-16.7205593397101));
#69775=CARTESIAN_POINT('Ctrl Pts',(-18.2003552145358,-16.9033347388086,
-16.7195056937699));
#69776=CARTESIAN_POINT('Ctrl Pts',(-18.2108347110444,-16.9006335782022,
-16.7188649213668));
#69777=CARTESIAN_POINT('Ctrl Pts',(-18.2547291176205,-16.889677743759,-16.7161968238502));
#69778=CARTESIAN_POINT('Ctrl Pts',(-18.2883232148034,-16.8821579603937,
-16.7141931955809));
#69779=CARTESIAN_POINT('Ctrl Pts',(-18.3763862066593,-16.8646893451843,
-16.7090285773441));
#69780=CARTESIAN_POINT('Ctrl Pts',(-18.4310892375177,-16.8560517378061,
-16.7059073901907));
#69781=CARTESIAN_POINT('Ctrl Pts',(-18.5948725391548,-16.8367376252915,
-16.6967392121255));
#69782=CARTESIAN_POINT('Ctrl Pts',(-18.7045087158893,-16.832372087458,-16.690840869258));
#69783=CARTESIAN_POINT('Ctrl Pts',(-18.8740567160749,-16.8387829452223,
-16.6816022197807));
#69784=CARTESIAN_POINT('Ctrl Pts',(-18.9339971675003,-16.8436113513292,
-16.6783108407253));
#69785=CARTESIAN_POINT('Ctrl Pts',(-19.0516894609793,-16.8581560058829,
-16.6716691057979));
#69786=CARTESIAN_POINT('Ctrl Pts',(-19.1094034033004,-16.8677302851486,
-16.6683254482368));
#69787=CARTESIAN_POINT('Ctrl Pts',(-19.1753664736535,-16.8815014889161,
-16.6643281468837));
#69788=CARTESIAN_POINT('Ctrl Pts',(-19.1840799764115,-16.8833781261451,
-16.6637965388849));
#69789=CARTESIAN_POINT('Ctrl Pts',(-19.1971982837832,-16.8862902377051,
-16.6629904394672));
#69790=CARTESIAN_POINT('Ctrl Pts',(-19.2016121709663,-16.8872849279304,
-16.6627182278152));
#69791=CARTESIAN_POINT('Ctrl Pts',(-19.2094999626009,-16.8890890690967,
-16.662229956609));
#69792=CARTESIAN_POINT('Ctrl Pts',(-19.2129750399456,-16.8898931564741,
-16.6620142071101));
#69793=CARTESIAN_POINT('Ctrl Pts',(-19.2204880050938,-16.8916515742056,
-16.6615463786556));
#69794=CARTESIAN_POINT('Ctrl Pts',(-19.224525068488,-16.8926089804809,-16.6612941297055));
#69795=CARTESIAN_POINT('Ctrl Pts',(-19.2357732147725,-16.8953114756195,
-16.6605889512874));
#69796=CARTESIAN_POINT('Ctrl Pts',(-19.2429778949755,-16.8970825943458,
-16.6601345638521));
#69797=CARTESIAN_POINT('Ctrl Pts',(-19.2843731053505,-16.9074897841288,
-16.6575088449693));
#69798=CARTESIAN_POINT('Ctrl Pts',(-19.3183507857377,-16.9169406888622,
-16.6552947366187));
#69799=CARTESIAN_POINT('Ctrl Pts',(-19.4260418951529,-16.9498141803089,
-16.6481220216415));
#69800=CARTESIAN_POINT('Ctrl Pts',(-19.4987119360344,-16.9764281657833,
-16.6430482549039));
#69801=CARTESIAN_POINT('Ctrl Pts',(-19.7400456206873,-17.0801257844027,
-16.6257144912326));
#69802=CARTESIAN_POINT('Ctrl Pts',(-19.9000262360672,-17.1753597451589,
-16.6134772632227));
#69803=CARTESIAN_POINT('Ctrl Pts',(-20.065107849679,-17.3056524096765,-16.6005085396931));
#69804=CARTESIAN_POINT('Ctrl Pts',(-20.0843724871826,-17.3214164466501,
-16.5989872567154));
#69805=CARTESIAN_POINT('Ctrl Pts',(-20.1108795009821,-17.3438988898489,
-16.5968820931309));
#69806=CARTESIAN_POINT('Ctrl Pts',(-20.1183590845592,-17.3503332834673,
-16.5962866999898));
#69807=CARTESIAN_POINT('Ctrl Pts',(-20.1303340992737,-17.3607814748257,
-16.5953311476197));
#69808=CARTESIAN_POINT('Ctrl Pts',(-20.1348577854917,-17.3647625326856,
-16.5949696389318));
#69809=CARTESIAN_POINT('Ctrl Pts',(-20.1439190803303,-17.3728058140691,
-16.5942443919374));
#69810=CARTESIAN_POINT('Ctrl Pts',(-20.1484562811448,-17.3768684118831,
-16.5938806743387));
#69811=CARTESIAN_POINT('Ctrl Pts',(-20.1591620619209,-17.3865379008501,
-16.5930210682899));
#69812=CARTESIAN_POINT('Ctrl Pts',(-20.165315210729,-17.3921617849334,-16.5925259031136));
#69813=CARTESIAN_POINT('Ctrl Pts',(-20.184442593567,-17.4098524028828,-16.5909830312592));
#69814=CARTESIAN_POINT('Ctrl Pts',(-20.1972988745386,-17.4220459612747,
-16.5899407438504));
#69815=CARTESIAN_POINT('Ctrl Pts',(-20.2268685762946,-17.4508051194123,
-16.5875298221538));
#69816=CARTESIAN_POINT('Ctrl Pts',(-20.2434620592698,-17.4674909870972,
-16.5861664509592));
#69817=CARTESIAN_POINT('Ctrl Pts',(-20.2997786791785,-17.5260419643163,
-16.5814972966395));
#69818=CARTESIAN_POINT('Ctrl Pts',(-20.3380674688943,-17.569253648664,-16.5782491676903));
#69819=CARTESIAN_POINT('Ctrl Pts',(-20.4763746941787,-17.738831802744,-16.5661065345472));
#69820=CARTESIAN_POINT('Ctrl Pts',(-20.5636115001708,-17.8748912568406,
-16.5576023127839));
#69821=CARTESIAN_POINT('Ctrl Pts',(-20.6416459971465,-18.0339402135876,
-16.5477154509039));
#69822=CARTESIAN_POINT('Ctrl Pts',(-20.6485568417914,-18.0484408698823,
-16.5468141071445));
#69823=CARTESIAN_POINT('Ctrl Pts',(-20.6755174583762,-18.1067092160545,
-16.5431871370101));
#69824=CARTESIAN_POINT('Ctrl Pts',(-20.6942352162063,-18.1510732387471,
-16.5404143891016));
#69825=CARTESIAN_POINT('Ctrl Pts',(-20.7141874622809,-18.2032633720555,
-16.5370970994278));
#69826=CARTESIAN_POINT('Ctrl Pts',(-20.7169120126994,-18.210509022611,-16.5366353337055));
#69827=CARTESIAN_POINT('Ctrl Pts',(-20.72120687568,-18.2221237183024,-16.5358929335549));
#69828=CARTESIAN_POINT('Ctrl Pts',(-20.7228026895865,-18.2264833466497,
-16.5356137777783));
#69829=CARTESIAN_POINT('Ctrl Pts',(-20.7256062610715,-18.2342212233973,
-16.5351173748902));
#69830=CARTESIAN_POINT('Ctrl Pts',(-20.7268197865733,-18.2375973338817,
-16.5349004746183));
#69831=CARTESIAN_POINT('Ctrl Pts',(-20.729376641007,-18.2447678865605,-16.5344391096293));
#69832=CARTESIAN_POINT('Ctrl Pts',(-20.7307177109276,-18.248563020591,-16.5341945215084));
#69833=CARTESIAN_POINT('Ctrl Pts',(-20.7343141464232,-18.2588338316283,
-16.5335315464735));
#69834=CARTESIAN_POINT('Ctrl Pts',(-20.7365488624792,-18.2653166146142,
-16.5331119673121));
#69835=CARTESIAN_POINT('Ctrl Pts',(-20.7475603537765,-18.2977712382975,
-16.5310062601364));
#69836=CARTESIAN_POINT('Ctrl Pts',(-20.755863102756,-18.3238996905106,-16.529294496797));
#69837=CARTESIAN_POINT('Ctrl Pts',(-20.7784982102654,-18.4002373205132,
-16.524260424197));
#69838=CARTESIAN_POINT('Ctrl Pts',(-20.7914828668915,-18.4508228823952,
-16.5208839991854));
#69839=CARTESIAN_POINT('Ctrl Pts',(-20.8346493259577,-18.6491790801985,
-16.5076111963695));
#69840=CARTESIAN_POINT('Ctrl Pts',(-20.8508817057974,-18.7995417691991,
-16.4975179105289));
#69841=CARTESIAN_POINT('Ctrl Pts',(-20.8509993557814,-18.9503484488822,
-16.4878149381751));
#69842=CARTESIAN_POINT('Ctrl Pts',(-20.8509993578169,-18.9503510600803,
-16.4878147701694));
#69843=CARTESIAN_POINT('Ctrl Pts',(-20.8510649773497,-19.0345970093956,
-16.4823943487751));
#69844=CARTESIAN_POINT('Ctrl Pts',(-20.8461018015119,-19.1187818254321,
-16.4770994536599));
#69845=CARTESIAN_POINT('Ctrl Pts',(-20.8349011937254,-19.2127900061834,
-16.4713270646499));
#69846=CARTESIAN_POINT('Ctrl Pts',(-20.833594094072,-19.2231123371005,-16.4706950869428));
#69847=CARTESIAN_POINT('Ctrl Pts',(-20.8312616504181,-19.240502273878,-16.4696334224317));
#69848=CARTESIAN_POINT('Ctrl Pts',(-20.8302765584432,-19.2475750071037,
-16.469202473263));
#69849=CARTESIAN_POINT('Ctrl Pts',(-20.8283990623356,-19.2605732870644,
-16.4684119901868));
#69850=CARTESIAN_POINT('Ctrl Pts',(-20.8275172529268,-19.2665002681227,
-16.4680521249301));
#69851=CARTESIAN_POINT('Ctrl Pts',(-20.8256463302589,-19.2787188236985,
-16.4673114273671));
#69852=CARTESIAN_POINT('Ctrl Pts',(-20.8246539659489,-19.2850098447147,
-16.4669307021733));
#69853=CARTESIAN_POINT('Ctrl Pts',(-20.8223696973859,-19.2990780288716,
-16.466080705912));
#69854=CARTESIAN_POINT('Ctrl Pts',(-20.8210627049252,-19.3068526727633,
-16.465611918897));
#69855=CARTESIAN_POINT('Ctrl Pts',(-20.8176411994243,-19.3265324415733,
-16.4644276122011));
#69856=CARTESIAN_POINT('Ctrl Pts',(-20.8154680485809,-19.3384271853317,
-16.4637139590921));
#69857=CARTESIAN_POINT('Ctrl Pts',(-20.8024833847127,-19.4062088330175,
-16.4596586629898));
#69858=CARTESIAN_POINT('Ctrl Pts',(-20.7895226652581,-19.4616632041659,
-16.4563862199873));
#69859=CARTESIAN_POINT('Ctrl Pts',(-20.7635221215107,-19.5556348933712,
-16.4508784060091));
#69860=CARTESIAN_POINT('Ctrl Pts',(-20.7515805991621,-19.5944203261352,
-16.4486161568553));
#69861=CARTESIAN_POINT('Ctrl Pts',(-20.7333849108257,-19.6479921359283,
-16.4454902009214));
#69862=CARTESIAN_POINT('Ctrl Pts',(-20.7280675950838,-19.6630832216733,
-16.4446094526583));
#69863=CARTESIAN_POINT('Ctrl Pts',(-20.7225805882177,-19.6781103526075,
-16.4437314133151));
#69864=CARTESIAN_POINT('Origin',(-18.734,-18.952,0.));
#69865=CARTESIAN_POINT('',(-20.7225805821192,-19.6781103693094,-15.6464962362309));
#69866=CARTESIAN_POINT('',(-20.7225805818996,-19.6781103699107,-15.8662165012922));
#69867=CARTESIAN_POINT('',(-20.7225805821191,-19.6781103693095,0.));
#69868=CARTESIAN_POINT('Ctrl Pts',(-20.7225805818996,-19.6781103699108,
-15.8662165012922));
#69869=CARTESIAN_POINT('Ctrl Pts',(-20.7307297073631,-19.6557925607626,
-15.8675067386898));
#69870=CARTESIAN_POINT('Ctrl Pts',(-20.7385063359538,-19.6333287725036,
-15.8687972801593));
#69871=CARTESIAN_POINT('Ctrl Pts',(-20.7729860297178,-19.5280199103041,
-15.8748265072091));
#69872=CARTESIAN_POINT('Ctrl Pts',(-20.7949379644017,-19.4437268313758,
-15.8795908542221));
#69873=CARTESIAN_POINT('Ctrl Pts',(-20.8189001336634,-19.3212038664771,
-15.8867187228425));
#69874=CARTESIAN_POINT('Ctrl Pts',(-20.8251640472988,-19.2838924378082,
-15.8889161159917));
#69875=CARTESIAN_POINT('Ctrl Pts',(-20.8314778232722,-19.2389374792607,
-15.891617064197));
#69876=CARTESIAN_POINT('Ctrl Pts',(-20.8324907022321,-19.2314335428028,
-15.8920696870342));
#69877=CARTESIAN_POINT('Ctrl Pts',(-20.8340004993622,-19.2197767627973,
-15.8927757821714));
#69878=CARTESIAN_POINT('Ctrl Pts',(-20.8345254155855,-19.2156275209463,
-15.8930277028585));
#69879=CARTESIAN_POINT('Ctrl Pts',(-20.8354748338075,-19.2079398824014,
-15.8934955857831));
#69880=CARTESIAN_POINT('Ctrl Pts',(-20.8359026977986,-19.204401959056,-15.8937113561156));
#69881=CARTESIAN_POINT('Ctrl Pts',(-20.836848273341,-19.1964140132555,-15.8941995263774));
#69882=CARTESIAN_POINT('Ctrl Pts',(-20.8373607906041,-19.1919634435997,
-15.8944722133263));
#69883=CARTESIAN_POINT('Ctrl Pts',(-20.8388276183908,-19.1788600437951,
-15.8952770454309));
#69884=CARTESIAN_POINT('Ctrl Pts',(-20.839742674446,-19.1702030376726,-15.8958113186995));
#69885=CARTESIAN_POINT('Ctrl Pts',(-20.8458591842089,-19.1087111214722,
-15.8996232153201));
#69886=CARTESIAN_POINT('Ctrl Pts',(-20.8491244442865,-19.0557070469998,
-15.9029969900621));
#69887=CARTESIAN_POINT('Ctrl Pts',(-20.8507874982691,-18.9862051756932,
-15.9074893528494));
#69888=CARTESIAN_POINT('Ctrl Pts',(-20.8509892979632,-18.9697651435171,
-15.9085570237302));
#69889=CARTESIAN_POINT('Ctrl Pts',(-20.8510113340041,-18.9345499588899,
-15.9108527723505));
#69890=CARTESIAN_POINT('Ctrl Pts',(-20.8507733234041,-18.9157761482131,
-15.9120820035659));
#69891=CARTESIAN_POINT('Ctrl Pts',(-20.8462294455872,-18.7409108018803,
-15.9235687182214));
#69892=CARTESIAN_POINT('Ctrl Pts',(-20.824913746761,-18.5857188053272,-15.9339903193705));
#69893=CARTESIAN_POINT('Ctrl Pts',(-20.785542695512,-18.4296163464068,-15.9442510920221));
#69894=CARTESIAN_POINT('Ctrl Pts',(-20.7843510914448,-18.4249587156732,
-15.9445570831285));
#69895=CARTESIAN_POINT('Ctrl Pts',(-20.7672392267998,-18.3590098563247,
-15.9488873945985));
#69896=CARTESIAN_POINT('Ctrl Pts',(-20.7485914678273,-18.2984545857325,
-15.9528337086067));
#69897=CARTESIAN_POINT('Ctrl Pts',(-20.723039946784,-18.2270409458947,-15.9574538815467));
#69898=CARTESIAN_POINT('Ctrl Pts',(-20.7187205985596,-18.2152980954052,
-15.9582125358089));
#69899=CARTESIAN_POINT('Ctrl Pts',(-20.711464542166,-18.1960984236054,-15.9594513604962));
#69900=CARTESIAN_POINT('Ctrl Pts',(-20.7085891943353,-18.1886188860803,
-15.9599335680101));
#69901=CARTESIAN_POINT('Ctrl Pts',(-20.7033484027647,-18.1752139482393,
-15.9607971315853));
#69902=CARTESIAN_POINT('Ctrl Pts',(-20.7009985212042,-18.1692826048676,
-15.9611790045827));
#69903=CARTESIAN_POINT('Ctrl Pts',(-20.695942226651,-18.1566865775832,-15.9619895093439));
#69904=CARTESIAN_POINT('Ctrl Pts',(-20.6932285809807,-18.1500248694498,
-15.962417891435));
#69905=CARTESIAN_POINT('Ctrl Pts',(-20.6858430804973,-18.1321554884538,
-15.9635663282357));
#69906=CARTESIAN_POINT('Ctrl Pts',(-20.6811086239729,-18.1209738573857,
-15.9642842555008));
#69907=CARTESIAN_POINT('Ctrl Pts',(-20.6571507113779,-18.0657200273455,
-15.9678291910116));
#69908=CARTESIAN_POINT('Ctrl Pts',(-20.6365250241544,-18.0222689096136,
-15.9706079109111));
#69909=CARTESIAN_POINT('Ctrl Pts',(-20.5374247689133,-17.8306367182849,
-15.982882583839));
#69910=CARTESIAN_POINT('Ctrl Pts',(-20.4430001204703,-17.6913983093555,
-15.9918006202372));
#69911=CARTESIAN_POINT('Ctrl Pts',(-20.2684487327962,-17.490185758686,-16.0063842130121));
#69912=CARTESIAN_POINT('Ctrl Pts',(-20.1986330781035,-17.4202432918067,
-16.0118768798071));
#69913=CARTESIAN_POINT('Ctrl Pts',(-20.116893153225,-17.3490684601606,-16.0182980400643));
#69914=CARTESIAN_POINT('Ctrl Pts',(-20.1095379792872,-17.3427522707442,
-16.0188757783208));
#69915=CARTESIAN_POINT('Ctrl Pts',(-20.0986146014658,-17.3335015200414,
-16.0197341610803));
#69916=CARTESIAN_POINT('Ctrl Pts',(-20.0950796391646,-17.330527658242,-16.0200120022496));
#69917=CARTESIAN_POINT('Ctrl Pts',(-20.0887912534383,-17.3252724735151,
-16.0205064146653));
#69918=CARTESIAN_POINT('Ctrl Pts',(-20.0860417539721,-17.3229865313253,
-16.0207226439304));
#69919=CARTESIAN_POINT('Ctrl Pts',(-20.0801385597367,-17.3181038385677,
-16.0211870247424));
#69920=CARTESIAN_POINT('Ctrl Pts',(-20.0769831838498,-17.315509286431,-16.0214353225418));
#69921=CARTESIAN_POINT('Ctrl Pts',(-20.0683014467751,-17.308412625049,-16.022118654952));
#69922=CARTESIAN_POINT('Ctrl Pts',(-20.0627598849563,-17.3039293174251,
-16.0225550070918));
#69923=CARTESIAN_POINT('Ctrl Pts',(-20.0330578005015,-17.2801465270536,
-16.0248942708288));
#69924=CARTESIAN_POINT('Ctrl Pts',(-20.0085005815772,-17.2613512374302,
-16.0268299549707));
#69925=CARTESIAN_POINT('Ctrl Pts',(-19.9329337739125,-17.2060969789132,
-16.0327693242548));
#69926=CARTESIAN_POINT('Ctrl Pts',(-19.8807099396329,-17.1713611346017,
-16.0368504395713));
#69927=CARTESIAN_POINT('Ctrl Pts',(-19.7118261973956,-17.069544292936,-16.0498094577686));
#69928=CARTESIAN_POINT('Ctrl Pts',(-19.5902576567293,-17.011223973896,-16.0587751100883));
#69929=CARTESIAN_POINT('Ctrl Pts',(-19.4256424332872,-16.9507535730585,
-16.0700685598907));
#69930=CARTESIAN_POINT('Ctrl Pts',(-19.3869105182043,-16.9377843483163,
-16.0726705063229));
#69931=CARTESIAN_POINT('Ctrl Pts',(-19.3014162312955,-16.9118825127892,
-16.078289482811));
#69932=CARTESIAN_POINT('Ctrl Pts',(-19.2545346260604,-16.8994199531673,
-16.0812910948842));
#69933=CARTESIAN_POINT('Ctrl Pts',(-19.1949880224102,-16.885762441544,-16.0850069640793));
#69934=CARTESIAN_POINT('Ctrl Pts',(-19.1826878327295,-16.8830565874611,
-16.0857694323499));
#69935=CARTESIAN_POINT('Ctrl Pts',(-19.1631556963317,-16.8789421971943,
-16.0869723028478));
#69936=CARTESIAN_POINT('Ctrl Pts',(-19.1559394293538,-16.8774614041765,
-16.0874150104652));
#69937=CARTESIAN_POINT('Ctrl Pts',(-19.1424773022615,-16.8747720968182,
-16.0882377754221));
#69938=CARTESIAN_POINT('Ctrl Pts',(-19.1362334589182,-16.8735540146271,
-16.0886181344525));
#69939=CARTESIAN_POINT('Ctrl Pts',(-19.1223512337462,-16.8709106955121,
-16.0894610799128));
#69940=CARTESIAN_POINT('Ctrl Pts',(-19.1147102805593,-16.8694993256313,
-16.0899232197061));
#69941=CARTESIAN_POINT('Ctrl Pts',(-19.0924792282726,-16.8655194452934,
-16.0912625979884));
#69942=CARTESIAN_POINT('Ctrl Pts',(-19.07786953696,-16.8630619395223,-16.0921363050671));
#69943=CARTESIAN_POINT('Ctrl Pts',(-18.9612384673987,-16.8447001116722,
-16.0990619156478));
#69944=CARTESIAN_POINT('Ctrl Pts',(-18.8581971845694,-16.8361244791702,
-16.1048707927129));
#69945=CARTESIAN_POINT('Ctrl Pts',(-18.5952941200334,-16.8335251301355,
-16.1193460039176));
#69946=CARTESIAN_POINT('Ctrl Pts',(-18.4360075589186,-16.8500086332339,
-16.1277742615311));
#69947=CARTESIAN_POINT('Ctrl Pts',(-18.2326901373384,-16.8946391933719,
-16.1395293310831));
#69948=CARTESIAN_POINT('Ctrl Pts',(-18.1856554523271,-16.9066730003033,
-16.1423242163451));
#69949=CARTESIAN_POINT('Ctrl Pts',(-18.1316341104387,-16.9224915547226,
-16.1456660586379));
#69950=CARTESIAN_POINT('Ctrl Pts',(-18.1242004327744,-16.9247127292859,
-16.1461288521409));
#69951=CARTESIAN_POINT('Ctrl Pts',(-18.1123335104085,-16.9283297263186,
-16.1468725918947));
#69952=CARTESIAN_POINT('Ctrl Pts',(-18.1078922821448,-16.9296993978238,
-16.1471520510458));
#69953=CARTESIAN_POINT('Ctrl Pts',(-18.1000301754268,-16.9321524469193,
-16.1476487975376));
#69954=CARTESIAN_POINT('Ctrl Pts',(-18.0966074987592,-16.933229910229,-16.147865736357));
#69955=CARTESIAN_POINT('Ctrl Pts',(-18.0893539728442,-16.9355336159061,
-16.148326962341));
#69956=CARTESIAN_POINT('Ctrl Pts',(-18.0855239340054,-16.9367620563027,
-16.1485713717932));
#69957=CARTESIAN_POINT('Ctrl Pts',(-18.0751862449485,-16.9401102715605,
-16.1492333693634));
#69958=CARTESIAN_POINT('Ctrl Pts',(-18.0686854010582,-16.942250681124,-16.1496521438467));
#69959=CARTESIAN_POINT('Ctrl Pts',(-18.0363464092235,-16.9530724261805,
-16.1517473348381));
#69960=CARTESIAN_POINT('Ctrl Pts',(-18.0106685216641,-16.9622202666219,
-16.1534490867683));
#69961=CARTESIAN_POINT('Ctrl Pts',(-17.9367563134362,-16.9901714554309,
-16.1584442879741));
#69962=CARTESIAN_POINT('Ctrl Pts',(-17.8890277863969,-17.010250796015,-16.1617909400697));
#69963=CARTESIAN_POINT('Ctrl Pts',(-17.7166886170026,-17.0903113315996,
-16.1742124396346));
#69964=CARTESIAN_POINT('Ctrl Pts',(-17.597288628506,-17.1607159740872,-16.1834585095198));
#69965=CARTESIAN_POINT('Ctrl Pts',(-17.4531469320556,-17.2659632502434,
-16.1950149431767));
#69966=CARTESIAN_POINT('Ctrl Pts',(-17.4213661164519,-17.29058581986,-16.1975929186163));
#69967=CARTESIAN_POINT('Ctrl Pts',(-17.344704883126,-17.3535538163037,-16.2038798760515));
#69968=CARTESIAN_POINT('Ctrl Pts',(-17.3006884029328,-17.3929008792986,
-16.2075501422267));
#69969=CARTESIAN_POINT('Ctrl Pts',(-17.2496029708767,-17.4425617087246,
-16.2118882697548));
#69970=CARTESIAN_POINT('Ctrl Pts',(-17.2409097805524,-17.4511602011974,
-16.212629434554));
#69971=CARTESIAN_POINT('Ctrl Pts',(-17.2267051619272,-17.4654556568296,
-16.213845546833));
#69972=CARTESIAN_POINT('Ctrl Pts',(-17.2211504544276,-17.4711090289222,
-16.2143224067282));
#69973=CARTESIAN_POINT('Ctrl Pts',(-17.2111873122963,-17.4813637021452,
-16.2151801361274));
#69974=CARTESIAN_POINT('Ctrl Pts',(-17.2067676778156,-17.485953944158,-16.2155614938385));
#69975=CARTESIAN_POINT('Ctrl Pts',(-17.1973631353017,-17.4958102032354,
-16.2163748935207));
#69976=CARTESIAN_POINT('Ctrl Pts',(-17.192384411972,-17.5010820288839,-16.2168066650069));
#69977=CARTESIAN_POINT('Ctrl Pts',(-17.1789621322447,-17.515441575901,-16.2179739357592));
#69978=CARTESIAN_POINT('Ctrl Pts',(-17.1705711219523,-17.5245781880762,
-16.2187071834209));
#69979=CARTESIAN_POINT('Ctrl Pts',(-17.1278099758911,-17.5719684084614,
-16.2224630341443));
#69980=CARTESIAN_POINT('Ctrl Pts',(-17.0947600209543,-17.6113932318482,
-16.2254299769808));
#69981=CARTESIAN_POINT('Ctrl Pts',(-16.9576006213985,-17.787675166661,-16.2381062496942));
#69982=CARTESIAN_POINT('Ctrl Pts',(-16.8689509324528,-17.9357130626752,
-16.2472181060822));
#69983=CARTESIAN_POINT('Ctrl Pts',(-16.7623787979088,-18.1757136384445,
-16.2616422174618));
#69984=CARTESIAN_POINT('Ctrl Pts',(-16.7309467633218,-18.2608529208552,
-16.2667142656139));
#69985=CARTESIAN_POINT('Ctrl Pts',(-16.7023147312639,-18.3569896908033,
-16.2726574334312));
#69986=CARTESIAN_POINT('Ctrl Pts',(-16.6996211110768,-18.3662655656631,
-16.2732330582019));
#69987=CARTESIAN_POINT('Ctrl Pts',(-16.6957351603995,-18.3799976229443,
-16.2740888894661));
#69988=CARTESIAN_POINT('Ctrl Pts',(-16.6944937228095,-18.384439941428,-16.2743663166008));
#69989=CARTESIAN_POINT('Ctrl Pts',(-16.6923158902063,-18.3923324411364,
-16.274860272318));
#69990=CARTESIAN_POINT('Ctrl Pts',(-16.6913737063379,-18.3957809740255,
-16.2750764612642));
#69991=CARTESIAN_POINT('Ctrl Pts',(-16.6893724302406,-18.4031796055299,
-16.2755410727289));
#69992=CARTESIAN_POINT('Ctrl Pts',(-16.6883160633632,-18.4071303319706,
-16.2757896431559));
#69993=CARTESIAN_POINT('Ctrl Pts',(-16.6854447442728,-18.417994888008,-16.2764744769912));
#69994=CARTESIAN_POINT('Ctrl Pts',(-16.6836533712204,-18.4249148134376,
-16.2769120673802));
#69995=CARTESIAN_POINT('Ctrl Pts',(-16.6742310377856,-18.4620874721685,
-16.2792697415396));
#69996=CARTESIAN_POINT('Ctrl Pts',(-16.6672349675675,-18.4924953491425,
-16.2812231993285));
#69997=CARTESIAN_POINT('Ctrl Pts',(-16.627713372978,-18.6834981951835,-16.2936015929701));
#69998=CARTESIAN_POINT('Ctrl Pts',(-16.6132535348419,-18.847258617052,-16.3046384230338));
#69999=CARTESIAN_POINT('Ctrl Pts',(-16.6210914435983,-19.1281630343,-16.3229964133678));
#70000=CARTESIAN_POINT('Ctrl Pts',(-16.6340762233565,-19.2448207436232,
-16.3304606218551));
#70001=CARTESIAN_POINT('Ctrl Pts',(-16.6594065554811,-19.3738475502771,
-16.3384894234507));
#70002=CARTESIAN_POINT('Ctrl Pts',(-16.6623021869892,-19.387845733046,-16.3393576801774));
#70003=CARTESIAN_POINT('Ctrl Pts',(-16.6671360999906,-19.4100765437877,
-16.3407323477502));
#70004=CARTESIAN_POINT('Ctrl Pts',(-16.6689822792973,-19.4183285510831,
-16.3412416890449));
#70005=CARTESIAN_POINT('Ctrl Pts',(-16.6723253280806,-19.4328619751784,
-16.3421371610188));
#70006=CARTESIAN_POINT('Ctrl Pts',(-16.6738015773789,-19.43914797841,-16.3425239482581));
#70007=CARTESIAN_POINT('Ctrl Pts',(-16.6769142396259,-19.4521347321018,
-16.3433219990456));
#70008=CARTESIAN_POINT('Ctrl Pts',(-16.6785546895061,-19.4588344434708,
-16.3437331274398));
#70009=CARTESIAN_POINT('Ctrl Pts',(-16.6828491576146,-19.4760095379292,
-16.3447856618007));
#70010=CARTESIAN_POINT('Ctrl Pts',(-16.6855507126369,-19.4864729157916,
-16.345425527474));
#70011=CARTESIAN_POINT('Ctrl Pts',(-16.6971569570993,-19.5300439431081,
-16.3480848022351));
#70012=CARTESIAN_POINT('Ctrl Pts',(-16.706785395659,-19.5629546020533,-16.350080713964));
#70013=CARTESIAN_POINT('Ctrl Pts',(-16.7339482874076,-19.6480700559076,
-16.3552209509689));
#70014=CARTESIAN_POINT('Ctrl Pts',(-16.7527277832449,-19.6998512037049,
-16.3583259643344));
#70015=CARTESIAN_POINT('Ctrl Pts',(-16.8147527759494,-19.8520706556725,
-16.3674659334321));
#70016=CARTESIAN_POINT('Ctrl Pts',(-16.863778822177,-19.949953268635,-16.3733521450796));
#70017=CARTESIAN_POINT('Ctrl Pts',(-16.9416095219262,-20.0792791547855,
-16.3815697480987));
#70018=CARTESIAN_POINT('Ctrl Pts',(-16.9641216557007,-20.1143047773691,
-16.3838450139904));
#70019=CARTESIAN_POINT('Ctrl Pts',(-17.0311327162433,-20.2120989320846,
-16.3904026078436));
#70020=CARTESIAN_POINT('Ctrl Pts',(-17.0780359042314,-20.2731307736757,
-16.3947452003717));
#70021=CARTESIAN_POINT('Ctrl Pts',(-17.1343438796865,-20.3386793683199,
-16.3998664796256));
#70022=CARTESIAN_POINT('Ctrl Pts',(-17.1405868348899,-20.3458485754957,
-16.4004331242079));
#70023=CARTESIAN_POINT('Ctrl Pts',(-17.1499104684294,-20.3564110357957,
-16.4012781059771));
#70024=CARTESIAN_POINT('Ctrl Pts',(-17.1529543207881,-20.3598368374339,
-16.4015537645834));
#70025=CARTESIAN_POINT('Ctrl Pts',(-17.1583904642936,-20.3659152557592,
-16.4020457781542));
#70026=CARTESIAN_POINT('Ctrl Pts',(-17.1607783691927,-20.3685717276609,
-16.402261803503));
#70027=CARTESIAN_POINT('Ctrl Pts',(-17.1659275891408,-20.3742709999359,
-16.4027274394942));
#70028=CARTESIAN_POINT('Ctrl Pts',(-17.1686910023114,-20.3773117638076,
-16.4029772052739));
#70029=CARTESIAN_POINT('Ctrl Pts',(-17.1763453185439,-20.3856851997488,
-16.40366863207));
#70030=CARTESIAN_POINT('Ctrl Pts',(-17.1812546833882,-20.3910008119867,
-16.4041116619195));
#70031=CARTESIAN_POINT('Ctrl Pts',(-17.2083326956934,-20.4200196081166,
-16.406552299704));
#70032=CARTESIAN_POINT('Ctrl Pts',(-17.2310156302216,-20.4432343914375,
-16.4085860627614));
#70033=CARTESIAN_POINT('Ctrl Pts',(-17.3706243523507,-20.5796949415688,
-16.4209903017239));
#70034=CARTESIAN_POINT('Ctrl Pts',(-17.4997570231484,-20.6796655268624,
-16.431952013662));
#70035=CARTESIAN_POINT('Ctrl Pts',(-17.7390557556664,-20.8242776971859,
-16.4502154948345));
#70036=CARTESIAN_POINT('Ctrl Pts',(-17.8438866526415,-20.8763294579752,
-16.4576574610546));
#70037=CARTESIAN_POINT('Ctrl Pts',(-17.9657765122672,-20.924745785803,-16.4656657234253));
#70038=CARTESIAN_POINT('Ctrl Pts',(-17.9791123996447,-20.9298872538807,
-16.4665338655643));
#70039=CARTESIAN_POINT('Ctrl Pts',(-18.0004192664867,-20.9378549290987,
-16.4679083865762));
#70040=CARTESIAN_POINT('Ctrl Pts',(-18.0083566990605,-20.9407690401476,
-16.4684176949259));
#70041=CARTESIAN_POINT('Ctrl Pts',(-18.0223859534902,-20.9458245007206,
-16.4693131285768));
#70042=CARTESIAN_POINT('Ctrl Pts',(-18.0284704724675,-20.9479856657993,
-16.4696999102613));
#70043=CARTESIAN_POINT('Ctrl Pts',(-18.0410752305636,-20.9523979210925,
-16.4704979683508));
#70044=CARTESIAN_POINT('Ctrl Pts',(-18.0475967820586,-20.9546450516606,
-16.4709091095094));
#70045=CARTESIAN_POINT('Ctrl Pts',(-18.0643639933708,-20.9603310021628,
-16.4719617153794));
#70046=CARTESIAN_POINT('Ctrl Pts',(-18.0746252935829,-20.9637233405008,
-16.4726016393864));
#70047=CARTESIAN_POINT('Ctrl Pts',(-18.1175531244837,-20.9775513388981,
-16.475261480885));
#70048=CARTESIAN_POINT('Ctrl Pts',(-18.1504458883981,-20.9872714246678,
-16.4772578882314));
#70049=CARTESIAN_POINT('Ctrl Pts',(-18.2367445345147,-21.0105090455725,
-16.482399690011));
#70050=CARTESIAN_POINT('Ctrl Pts',(-18.2904683501457,-21.0227493350961,
-16.4855057411379));
#70051=CARTESIAN_POINT('Ctrl Pts',(-18.4520695669314,-21.0529892443179,
-16.4946475209051));
#70052=CARTESIAN_POINT('Ctrl Pts',(-18.5609267548231,-21.064743976899,-16.5005345114323));
#70053=CARTESIAN_POINT('Ctrl Pts',(-18.7135619749919,-21.0693457143934,
-16.5088482751542));
#70054=CARTESIAN_POINT('Ctrl Pts',(-18.7569483798989,-21.0693199480965,
-16.5112195249736));
#70055=CARTESIAN_POINT('Ctrl Pts',(-18.8292945691319,-21.0670530332496,
-16.5152274137375));
#70056=CARTESIAN_POINT('Ctrl Pts',(-18.8582643923496,-21.0655488262737,
-16.5168468049708));
#70057=CARTESIAN_POINT('Ctrl Pts',(-18.934671416717,-21.0600052256225,-16.5211766017069));
#70058=CARTESIAN_POINT('Ctrl Pts',(-18.9820161163156,-21.054960367503,-16.5239194265345));
#70059=CARTESIAN_POINT('Ctrl Pts',(-19.0367909684201,-21.0472484879392,
-16.5272036879119));
#70060=CARTESIAN_POINT('Ctrl Pts',(-19.0444293916131,-21.0461304127202,
-16.5276642081705));
#70061=CARTESIAN_POINT('Ctrl Pts',(-19.056645123054,-21.0442740308887,-16.5284049847111));
#70062=CARTESIAN_POINT('Ctrl Pts',(-19.0612264989245,-21.0435624095942,
-16.5286837725493));
#70063=CARTESIAN_POINT('Ctrl Pts',(-19.0693479602099,-21.0422735732448,
-16.5291797591694));
#70064=CARTESIAN_POINT('Ctrl Pts',(-19.0728889590211,-21.0417024043409,
-16.5293966131512));
#70065=CARTESIAN_POINT('Ctrl Pts',(-19.0804041624123,-21.0404705854899,
-16.5298581488512));
#70066=CARTESIAN_POINT('Ctrl Pts',(-19.0843778756344,-21.039807599812,-16.5301029553359));
#70067=CARTESIAN_POINT('Ctrl Pts',(-19.0951257728073,-21.0379828416812,
-16.5307671253537));
#70068=CARTESIAN_POINT('Ctrl Pts',(-19.1018961622764,-21.0367994268902,
-16.5311876883415));
#70069=CARTESIAN_POINT('Ctrl Pts',(-19.1358330208706,-21.0306970532555,
-16.5333063336567));
#70070=CARTESIAN_POINT('Ctrl Pts',(-19.1629058272887,-21.0252802121215,
-16.5350304228148));
#70071=CARTESIAN_POINT('Ctrl Pts',(-19.2413869743396,-21.0079745173343,
-16.5401125336286));
#70072=CARTESIAN_POINT('Ctrl Pts',(-19.2924644680803,-20.9946917149017,
-16.5435258094916));
#70073=CARTESIAN_POINT('Ctrl Pts',(-19.4895943261432,-20.9354813986299,
-16.5569879476815));
#70074=CARTESIAN_POINT('Ctrl Pts',(-19.6310094190138,-20.8756691335443,
-16.5672342660921));
#70075=CARTESIAN_POINT('Ctrl Pts',(-19.8353826395793,-20.7617476874904,
-16.5822648906721));
#70076=CARTESIAN_POINT('Ctrl Pts',(-19.903719246692,-20.7183493440658,-16.5873428662116));
#70077=CARTESIAN_POINT('Ctrl Pts',(-19.9802669652236,-20.6633405086758,
-16.5930915676057));
#70078=CARTESIAN_POINT('Ctrl Pts',(-19.9910481576296,-20.6554370042672,
-16.5939028141868));
#70079=CARTESIAN_POINT('Ctrl Pts',(-20.008308359053,-20.6425307409812,-16.5952043446949));
#70080=CARTESIAN_POINT('Ctrl Pts',(-20.0148343478352,-20.6375916932928,
-16.5956970935598));
#70081=CARTESIAN_POINT('Ctrl Pts',(-20.026272329459,-20.6288303313179,-16.5965619293752));
#70082=CARTESIAN_POINT('Ctrl Pts',(-20.0311963830989,-20.6250239921982,
-16.5969346386755));
#70083=CARTESIAN_POINT('Ctrl Pts',(-20.0414236845828,-20.6170458958003,
-16.5977096249164));
#70084=CARTESIAN_POINT('Ctrl Pts',(-20.0467239238317,-20.6128703825253,
-16.5981117469378));
#70085=CARTESIAN_POINT('Ctrl Pts',(-20.0603108395095,-20.6020609780745,
-16.5991438941817));
#70086=CARTESIAN_POINT('Ctrl Pts',(-20.068567811867,-20.5953899221138,-16.5997724252275));
#70087=CARTESIAN_POINT('Ctrl Pts',(-20.086430415661,-20.5807347760682,-16.6011351766353));
#70088=CARTESIAN_POINT('Ctrl Pts',(-20.0960163054245,-20.5727271804937,
-16.6018684283294));
#70089=CARTESIAN_POINT('Ctrl Pts',(-20.123608919686,-20.5492599225391,-16.603985285176));
#70090=CARTESIAN_POINT('Ctrl Pts',(-20.1414275846905,-20.5335814450706,
-16.605360082202));
#70091=CARTESIAN_POINT('Ctrl Pts',(-20.2021858590854,-20.4782806373543,
-16.610080719691));
#70092=CARTESIAN_POINT('Ctrl Pts',(-20.243747922432,-20.437181557718,-16.613367421976));
#70093=CARTESIAN_POINT('Ctrl Pts',(-20.3971128987807,-20.2724242825409,
-16.6258507220206));
#70094=CARTESIAN_POINT('Ctrl Pts',(-20.4958546396415,-20.13746453344,-16.6346274445503));
#70095=CARTESIAN_POINT('Ctrl Pts',(-20.6057404058206,-19.9427180856376,
-16.6471659685301));
#70096=CARTESIAN_POINT('Ctrl Pts',(-20.631719340746,-19.891997105722,-16.6504265390946));
#70097=CARTESIAN_POINT('Ctrl Pts',(-20.6593362816642,-19.832254327075,-16.6543312422468));
#70098=CARTESIAN_POINT('Ctrl Pts',(-20.6630028482097,-19.8241900499486,
-16.6548596342938));
#70099=CARTESIAN_POINT('Ctrl Pts',(-20.6684606891082,-19.8119832609207,
-16.6556617934192));
#70100=CARTESIAN_POINT('Ctrl Pts',(-20.6702895594041,-19.8078575278895,
-16.6559333136565));
#70101=CARTESIAN_POINT('Ctrl Pts',(-20.6735399307298,-19.8004612978634,
-16.6564208415383));
#70102=CARTESIAN_POINT('Ctrl Pts',(-20.6749663723949,-19.7971930299199,
-16.6566365430581));
#70103=CARTESIAN_POINT('Ctrl Pts',(-20.678038007097,-19.7901065040981,-16.6571048446689));
#70104=CARTESIAN_POINT('Ctrl Pts',(-20.6796801896291,-19.7862870514682,
-16.6573576178657));
#70105=CARTESIAN_POINT('Ctrl Pts',(-20.684236790219,-19.7756025047067,-16.6580657099068));
#70106=CARTESIAN_POINT('Ctrl Pts',(-20.687126163031,-19.7687268889667,-16.658522505925));
#70107=CARTESIAN_POINT('Ctrl Pts',(-20.70143825064,-19.734159229708,-16.6608242189666));
#70108=CARTESIAN_POINT('Ctrl Pts',(-20.712307776493,-19.7062442490166,-16.6626994153792));
#70109=CARTESIAN_POINT('Ctrl Pts',(-20.7225805820307,-19.6781103695518,
-16.6645990581914));
#70110=CARTESIAN_POINT('Ctrl Pts',(-20.7225805882177,-19.6781103526075,
-16.4437314133151));
#70111=CARTESIAN_POINT('Ctrl Pts',(-20.6965443416094,-19.7494151817003,
-16.4395650527784));
#70112=CARTESIAN_POINT('Ctrl Pts',(-20.6666873095021,-19.8192801308043,
-16.4354619668037));
#70113=CARTESIAN_POINT('Ctrl Pts',(-20.5942956802539,-19.9662562803097,
-16.4265492207356));
#70114=CARTESIAN_POINT('Ctrl Pts',(-20.5505851114218,-20.0426107945465,
-16.42173972251));
#70115=CARTESIAN_POINT('Ctrl Pts',(-20.4813387103453,-20.1478027480543,
-16.414551017801));
#70116=CARTESIAN_POINT('Ctrl Pts',(-20.4595656891349,-20.1790123990853,
-16.412341193437));
#70117=CARTESIAN_POINT('Ctrl Pts',(-20.4324595281259,-20.2157174357495,
-16.4096264675339));
#70118=CARTESIAN_POINT('Ctrl Pts',(-20.4279211758614,-20.2217943030754,
-16.4091731046042));
#70119=CARTESIAN_POINT('Ctrl Pts',(-20.4208281426725,-20.2311861990604,
-16.4084661017703));
#70120=CARTESIAN_POINT('Ctrl Pts',(-20.4182960678511,-20.2345183312157,
-16.4082140198899));
#70121=CARTESIAN_POINT('Ctrl Pts',(-20.413589689593,-20.2406738041639,-16.407745990402));
#70122=CARTESIAN_POINT('Ctrl Pts',(-20.4114181316746,-20.2434991714577,
-16.4075302356777));
#70123=CARTESIAN_POINT('Ctrl Pts',(-20.4065025452937,-20.2498614236785,
-16.4070422968037));
#70124=CARTESIAN_POINT('Ctrl Pts',(-20.403754442111,-20.2533950750197,-16.4067698268464));
#70125=CARTESIAN_POINT('Ctrl Pts',(-20.3956392669153,-20.2637619622676,
-16.4059662150643));
#70126=CARTESIAN_POINT('Ctrl Pts',(-20.390241384442,-20.2705708056536,-16.4054329545714));
#70127=CARTESIAN_POINT('Ctrl Pts',(-20.3519510790968,-20.318263787291,-16.4016602557134));
#70128=CARTESIAN_POINT('Ctrl Pts',(-20.3175931800649,-20.357942416745,-16.3983268976479));
#70129=CARTESIAN_POINT('Ctrl Pts',(-20.2680017203592,-20.4110876587015,
-16.3936317155812));
#70130=CARTESIAN_POINT('Ctrl Pts',(-20.2539921342721,-20.4256763379892,
-16.3923172380323));
#70131=CARTESIAN_POINT('Ctrl Pts',(-20.1944852553819,-20.4858916029021,
-16.3867903869416));
#70132=CARTESIAN_POINT('Ctrl Pts',(-20.1471268370527,-20.5296288550271,
-16.3825280283716));
#70133=CARTESIAN_POINT('Ctrl Pts',(-20.0268922266698,-20.6309061502357,
-16.372140645233));
#70134=CARTESIAN_POINT('Ctrl Pts',(-19.9520786154108,-20.6859501140268,
-16.3660355233576));
#70135=CARTESIAN_POINT('Ctrl Pts',(-19.8280107558721,-20.7652274675031,
-16.3565767560004));
#70136=CARTESIAN_POINT('Ctrl Pts',(-19.781014536084,-20.7927647155573,-16.3531305809863));
#70137=CARTESIAN_POINT('Ctrl Pts',(-19.7130843996956,-20.8291236711577,
-16.3483426168123));
#70138=CARTESIAN_POINT('Ctrl Pts',(-19.6929933449978,-20.8394669174303,
-16.3469494302334));
#70139=CARTESIAN_POINT('Ctrl Pts',(-19.6573339834099,-20.8571086029881,
-16.34451617133));
#70140=CARTESIAN_POINT('Ctrl Pts',(-19.6418354483742,-20.8645426165517,
-16.3434714780255));
#70141=CARTESIAN_POINT('Ctrl Pts',(-19.6187996745499,-20.8752488117673,
-16.3419372810226));
#70142=CARTESIAN_POINT('Ctrl Pts',(-19.6113314609758,-20.8786670616894,
-16.3414427414028));
#70143=CARTESIAN_POINT('Ctrl Pts',(-19.5982633387782,-20.8845566857527,
-16.3405822779501));
#70144=CARTESIAN_POINT('Ctrl Pts',(-19.5926722919433,-20.8870473789219,
-16.3402156928396));
#70145=CARTESIAN_POINT('Ctrl Pts',(-19.5815134480694,-20.8919605208084,
-16.3394871056638));
#70146=CARTESIAN_POINT('Ctrl Pts',(-19.5759458758095,-20.894383332492,-16.3391250938649));
#70147=CARTESIAN_POINT('Ctrl Pts',(-19.5626185698565,-20.9001148386649,
-16.3382620884902));
#70148=CARTESIAN_POINT('Ctrl Pts',(-19.554849294018,-20.9034011885252,-16.3377618588597));
#70149=CARTESIAN_POINT('Ctrl Pts',(-19.52678593254,-20.9150745393023,-16.3359651047281));
#70150=CARTESIAN_POINT('Ctrl Pts',(-19.5063808511285,-20.923192292935,-16.3346776783996));
#70151=CARTESIAN_POINT('Ctrl Pts',(-19.3109591509058,-20.9974363318907,
-16.3225174746201));
#70152=CARTESIAN_POINT('Ctrl Pts',(-19.1280358034047,-21.0404044882605,
-16.3125178271639));
#70153=CARTESIAN_POINT('Ctrl Pts',(-18.8630650279926,-21.0665439589387,
-16.2979982313434));
#70154=CARTESIAN_POINT('Ctrl Pts',(-18.7839281003975,-21.0698902634106,
-16.2936425055498));
#70155=CARTESIAN_POINT('Ctrl Pts',(-18.6690381780632,-21.0683052405551,
-16.2870682099507));
#70156=CARTESIAN_POINT('Ctrl Pts',(-18.6333003361813,-21.0669059425486,
-16.2849876505455));
#70157=CARTESIAN_POINT('Ctrl Pts',(-18.5901830977223,-21.0641224396186,
-16.2824162662473));
#70158=CARTESIAN_POINT('Ctrl Pts',(-18.5827513630383,-21.0636032646771,
-16.2819708562686));
#70159=CARTESIAN_POINT('Ctrl Pts',(-18.5711785764213,-21.0627333925416,
-16.2812736108339));
#70160=CARTESIAN_POINT('Ctrl Pts',(-18.5670354706511,-21.0624097032623,
-16.281023265122));
#70161=CARTESIAN_POINT('Ctrl Pts',(-18.559338781334,-21.0617855760697,-16.2805567962744));
#70162=CARTESIAN_POINT('Ctrl Pts',(-18.5557849942619,-21.0614883572606,
-16.2803408554299));
#70163=CARTESIAN_POINT('Ctrl Pts',(-18.5477332527692,-21.0607944631246,
-16.2798503427349));
#70164=CARTESIAN_POINT('Ctrl Pts',(-18.5432358284837,-21.0603923778133,
-16.2795754716863));
#70165=CARTESIAN_POINT('Ctrl Pts',(-18.5316183722626,-21.0593162615627,
-16.2788632089119));
#70166=CARTESIAN_POINT('Ctrl Pts',(-18.5245004749634,-21.0586205389605,
-16.2784246434546));
#70167=CARTESIAN_POINT('Ctrl Pts',(-18.4806283489905,-21.054107811997,-16.2757086713008));
#70168=CARTESIAN_POINT('Ctrl Pts',(-18.4439781266975,-21.0493653420743,
-16.2733843522618));
#70169=CARTESIAN_POINT('Ctrl Pts',(-18.2390314256798,-21.0173714603862,
-16.2601434386274));
#70170=CARTESIAN_POINT('Ctrl Pts',(-18.0743837399871,-20.9708270668219,
-16.2486402118437));
#70171=CARTESIAN_POINT('Ctrl Pts',(-17.8293240934374,-20.868325234724,-16.2313797227007));
#70172=CARTESIAN_POINT('Ctrl Pts',(-17.7441172019323,-20.8257334837867,
-16.225335611227));
#70173=CARTESIAN_POINT('Ctrl Pts',(-17.6436334443798,-20.7667303196802,
-16.2181781335989));
#70174=CARTESIAN_POINT('Ctrl Pts',(-17.6253762065773,-20.7556348565989,
-16.2168760293727));
#70175=CARTESIAN_POINT('Ctrl Pts',(-17.5996659066338,-20.739472028513,-16.2150394312111));
#70176=CARTESIAN_POINT('Ctrl Pts',(-17.5920728779454,-20.7346307918136,
-16.2144966541862));
#70177=CARTESIAN_POINT('Ctrl Pts',(-17.5790311576359,-20.7261980032417,
-16.213563661872));
#70178=CARTESIAN_POINT('Ctrl Pts',(-17.5735678025254,-20.7226294638018,
-16.2131725973743));
#70179=CARTESIAN_POINT('Ctrl Pts',(-17.5631414715522,-20.7157502363238,
-16.2124258240154));
#70180=CARTESIAN_POINT('Ctrl Pts',(-17.5581758275329,-20.7124437242739,
-16.2120699637226));
#70181=CARTESIAN_POINT('Ctrl Pts',(-17.5453058330529,-20.7037951341314,
-16.2111470739568));
#70182=CARTESIAN_POINT('Ctrl Pts',(-17.5374234418328,-20.698420499042,-16.2105812781564));
#70183=CARTESIAN_POINT('Ctrl Pts',(-17.5106998882713,-20.6799330878844,
-16.2086609029701));
#70184=CARTESIAN_POINT('Ctrl Pts',(-17.4920353678397,-20.6665669519341,
-16.2073159784082));
#70185=CARTESIAN_POINT('Ctrl Pts',(-17.3322184999601,-20.5481386973109,
-16.1957569848153));
#70186=CARTESIAN_POINT('Ctrl Pts',(-17.2044585721606,-20.4261641064983,
-16.1862985668844));
#70187=CARTESIAN_POINT('Ctrl Pts',(-17.0384864671159,-20.2226040308097,
-16.1720066095259));
#70188=CARTESIAN_POINT('Ctrl Pts',(-16.9878986156312,-20.152136793481,-16.1672607827379));
#70189=CARTESIAN_POINT('Ctrl Pts',(-16.9216892225718,-20.0468254857366,
-16.1601578865959));
#70190=CARTESIAN_POINT('Ctrl Pts',(-16.9024621345172,-20.0143473296375,
-16.1579656194571));
#70191=CARTESIAN_POINT('Ctrl Pts',(-16.8804352765808,-19.9747629606103,
-16.1552703528791));
#70192=CARTESIAN_POINT('Ctrl Pts',(-16.8767914847811,-19.9681312831427,
-16.1548180366995));
#70193=CARTESIAN_POINT('Ctrl Pts',(-16.8711895947806,-19.9578050888675,
-16.1541123176822));
#70194=CARTESIAN_POINT('Ctrl Pts',(-16.8692067153094,-19.9541239879695,
-16.1538604638047));
#70195=CARTESIAN_POINT('Ctrl Pts',(-16.8655539493425,-19.9472944574292,
-16.1533926415227));
#70196=CARTESIAN_POINT('Ctrl Pts',(-16.8638811029683,-19.9441476763009,
-16.1531768646174));
#70197=CARTESIAN_POINT('Ctrl Pts',(-16.8601226002057,-19.9370343010358,
-16.1526885979885));
#70198=CARTESIAN_POINT('Ctrl Pts',(-16.8580416005881,-19.9330653222381,
-16.1524158207411));
#70199=CARTESIAN_POINT('Ctrl Pts',(-16.8519522145636,-19.9213611474503,
-16.1516104805792));
#70200=CARTESIAN_POINT('Ctrl Pts',(-16.8479790138307,-19.9136078902488,
-16.1510757856137));
#70201=CARTESIAN_POINT('Ctrl Pts',(-16.8200772633822,-19.8583225891709,
-16.1472557105644));
#70202=CARTESIAN_POINT('Ctrl Pts',(-16.7979026066462,-19.8099316589153,
-16.1438737312689));
#70203=CARTESIAN_POINT('Ctrl Pts',(-16.7705880070477,-19.7438566544947,
-16.1392532703864));
#70204=CARTESIAN_POINT('Ctrl Pts',(-16.7638192297955,-19.726862130293,-16.138064623739));
#70205=CARTESIAN_POINT('Ctrl Pts',(-16.7400954038232,-19.664976871626,-16.1337399864725));
#70206=CARTESIAN_POINT('Ctrl Pts',(-16.7244478887265,-19.6196014091021,
-16.1305765881988));
#70207=CARTESIAN_POINT('Ctrl Pts',(-16.678233488877,-19.4691811711211,-16.1201818439999));
#70208=CARTESIAN_POINT('Ctrl Pts',(-16.6542595794201,-19.3622871688752,
-16.1129494699686));
#70209=CARTESIAN_POINT('Ctrl Pts',(-16.6307936785877,-19.1994824469219,
-16.1023767144949));
#70210=CARTESIAN_POINT('Ctrl Pts',(-16.6250650848887,-19.1446622344003,
-16.0988879529153));
#70211=CARTESIAN_POINT('Ctrl Pts',(-16.6192508866047,-19.055449097107,-16.0933309111094));
#70212=CARTESIAN_POINT('Ctrl Pts',(-16.6178522780413,-19.0211705386633,
-16.091224201238));
#70213=CARTESIAN_POINT('Ctrl Pts',(-16.6171091901768,-18.9760648108973,
-16.0884878423123));
#70214=CARTESIAN_POINT('Ctrl Pts',(-16.6170139158796,-18.965256781772,-16.087834855556));
#70215=CARTESIAN_POINT('Ctrl Pts',(-16.6169934382055,-18.9475503969162,
-16.0867693773816));
#70216=CARTESIAN_POINT('Ctrl Pts',(-16.6170191745592,-18.9406523959966,
-16.0863553566392));
#70217=CARTESIAN_POINT('Ctrl Pts',(-16.6171342735599,-18.9272980564383,
-16.0855558439122));
#70218=CARTESIAN_POINT('Ctrl Pts',(-16.6172194597147,-18.9208417669398,
-16.0851702256111));
#70219=CARTESIAN_POINT('Ctrl Pts',(-16.6174844047218,-18.9059324582976,
-16.0842817947634));
#70220=CARTESIAN_POINT('Ctrl Pts',(-16.6176852682019,-18.8974798881866,
-16.0837796483325));
#70221=CARTESIAN_POINT('Ctrl Pts',(-16.6183618392589,-18.8747446725737,
-16.0824329984989));
#70222=CARTESIAN_POINT('Ctrl Pts',(-16.6189315397412,-18.860465109764,-16.0815914367793));
#70223=CARTESIAN_POINT('Ctrl Pts',(-16.6254872555825,-18.7294624991767,
-16.0739072700658));
#70224=CARTESIAN_POINT('Ctrl Pts',(-16.6409851955418,-18.6134099410587,
-16.0673815790405));
#70225=CARTESIAN_POINT('Ctrl Pts',(-16.7008296409307,-18.3400803476614,
-16.0520640353285));
#70226=CARTESIAN_POINT('Ctrl Pts',(-16.7539192634356,-18.1855173050976,
-16.0434557340808));
#70227=CARTESIAN_POINT('Ctrl Pts',(-16.8381356195767,-18.0094334670877,
-16.0322460479717));
#70228=CARTESIAN_POINT('Ctrl Pts',(-16.8527443984693,-17.980603828165,-16.0303608616284));
#70229=CARTESIAN_POINT('Ctrl Pts',(-16.8714195007549,-17.9457519657349,
-16.0280065440628));
#70230=CARTESIAN_POINT('Ctrl Pts',(-16.8748651898488,-17.9393998929047,
-16.0275743307229));
#70231=CARTESIAN_POINT('Ctrl Pts',(-16.8803199322535,-17.9294658575846,
-16.0268932914705));
#70232=CARTESIAN_POINT('Ctrl Pts',(-16.8823070391383,-17.9258718189221,
-16.0266458449649));
#70233=CARTESIAN_POINT('Ctrl Pts',(-16.8860421809167,-17.9191623260885,
-16.0261818868966));
#70234=CARTESIAN_POINT('Ctrl Pts',(-16.8877876479322,-17.9160455067061,
-16.025965539632));
#70235=CARTESIAN_POINT('Ctrl Pts',(-16.8917918282189,-17.9089376423198,
-16.0254702946773));
#70236=CARTESIAN_POINT('Ctrl Pts',(-16.8940556183048,-17.9049495229261,
-16.0251910736221));
#70237=CARTESIAN_POINT('Ctrl Pts',(-16.8999983905922,-17.8945589266312,
-16.0244601380707));
#70238=CARTESIAN_POINT('Ctrl Pts',(-16.9036979083874,-17.8881683513176,
-16.0240071475843));
#70239=CARTESIAN_POINT('Ctrl Pts',(-16.9281580618464,-17.8464209629312,
-16.0210259776634));
#70240=CARTESIAN_POINT('Ctrl Pts',(-16.9499072548813,-17.8116567705678,
-16.0184400296505));
#70241=CARTESIAN_POINT('Ctrl Pts',(-16.9784220097713,-17.7688925822809,
-16.0151478810514));
#70242=CARTESIAN_POINT('Ctrl Pts',(-16.9842574587583,-17.7602792799255,
-16.0144789710384));
#70243=CARTESIAN_POINT('Ctrl Pts',(-16.9905359304933,-17.7511575926876,
-16.0137646197196));
#70244=CARTESIAN_POINT('Ctrl Pts',(-16.9909160501452,-17.7506058962115,
-16.0137213910916));
#70245=CARTESIAN_POINT('Ctrl Pts',(-17.0042631372199,-17.7312539256193,
-16.0122042346666));
#70246=CARTESIAN_POINT('Ctrl Pts',(-17.0175329087981,-17.712664990839,-16.010719851013));
#70247=CARTESIAN_POINT('Ctrl Pts',(-17.0582332092904,-17.6575578589333,
-16.0062449637163));
#70248=CARTESIAN_POINT('Ctrl Pts',(-17.0865470416795,-17.6217092975655,
-16.0032337948508));
#70249=CARTESIAN_POINT('Ctrl Pts',(-17.1865154718374,-17.503228617464,-15.9929935042399));
#70250=CARTESIAN_POINT('Ctrl Pts',(-17.2634088020367,-17.425234831801,-15.9857629243905));
#70251=CARTESIAN_POINT('Ctrl Pts',(-17.3875660012394,-17.3174246452061,
-15.9751939373817));
#70252=CARTESIAN_POINT('Ctrl Pts',(-17.4305385756909,-17.2829552916756,
-15.9717071375522));
#70253=CARTESIAN_POINT('Ctrl Pts',(-17.5023719887934,-17.2298045860117,
-15.9661528545762));
#70254=CARTESIAN_POINT('Ctrl Pts',(-17.5304270146847,-17.2100824109653,
-15.9640469893386));
#70255=CARTESIAN_POINT('Ctrl Pts',(-17.5679391598864,-17.1850512459489,
-15.9613115503641));
#70256=CARTESIAN_POINT('Ctrl Pts',(-17.5769741543946,-17.1791218367659,
-15.9606586585461));
#70257=CARTESIAN_POINT('Ctrl Pts',(-17.5918497696444,-17.1695215490091,
-15.9595932955746));
#70258=CARTESIAN_POINT('Ctrl Pts',(-17.5976635479298,-17.1658096276162,
-15.9591792957351));
#70259=CARTESIAN_POINT('Ctrl Pts',(-17.6089545764444,-17.1586780862025,
-15.9583797959415));
#70260=CARTESIAN_POINT('Ctrl Pts',(-17.6144295271651,-17.155254984882,-15.9579941698146));
#70261=CARTESIAN_POINT('Ctrl Pts',(-17.6271101524313,-17.1474071475838,
-15.9571056817313));
#70262=CARTESIAN_POINT('Ctrl Pts',(-17.6343268775291,-17.143000407816,-15.9566034861661));
#70263=CARTESIAN_POINT('Ctrl Pts',(-17.6538130472162,-17.131261292063,-15.955256617545));
#70264=CARTESIAN_POINT('Ctrl Pts',(-17.6661308009899,-17.1240096596888,
-15.9544148876857));
#70265=CARTESIAN_POINT('Ctrl Pts',(-17.780028306882,-17.0585008084712,-15.9467174988472));
#70266=CARTESIAN_POINT('Ctrl Pts',(-17.8862102738099,-17.0086371804574,
-15.9401800616163));
#70267=CARTESIAN_POINT('Ctrl Pts',(-18.1493513031603,-16.9107625393754,
-15.9248116845903));
#70268=CARTESIAN_POINT('Ctrl Pts',(-18.3087952433243,-16.8716987866076,
-15.9161664348669));
#70269=CARTESIAN_POINT('Ctrl Pts',(-18.5023526822931,-16.8474765297415,
-15.9049530743373));
#70270=CARTESIAN_POINT('Ctrl Pts',(-18.5336629784919,-16.8442655869463,
-15.9031159586999));
#70271=CARTESIAN_POINT('Ctrl Pts',(-18.5721758991528,-16.8411818331747,
-15.900815151354));
#70272=CARTESIAN_POINT('Ctrl Pts',(-18.5793232726317,-16.8406460553281,
-15.9003864256964));
#70273=CARTESIAN_POINT('Ctrl Pts',(-18.5905569835468,-16.8398613065372,
-15.8997096723339));
#70274=CARTESIAN_POINT('Ctrl Pts',(-18.5946416339385,-16.8395878705736,
-15.8994629954906));
#70275=CARTESIAN_POINT('Ctrl Pts',(-18.6022940441297,-16.8390978922176,
-15.8989996818882));
#70276=CARTESIAN_POINT('Ctrl Pts',(-18.6058615679212,-16.8388785369894,
-15.8987832045772));
#70277=CARTESIAN_POINT('Ctrl Pts',(-18.6140274945244,-16.8383971962887,
-15.8982866024987));
#70278=CARTESIAN_POINT('Ctrl Pts',(-18.6186261938086,-16.8381411830859,
-15.898006147527));
#70279=CARTESIAN_POINT('Ctrl Pts',(-18.6328371884397,-16.8373965570278,
-15.8971371162434));
#70280=CARTESIAN_POINT('Ctrl Pts',(-18.6424518513076,-16.8369584959363,
-15.8965458201374));
#70281=CARTESIAN_POINT('Ctrl Pts',(-18.7385993237839,-16.8332346561243,
-15.8906016737341));
#70282=CARTESIAN_POINT('Ctrl Pts',(-18.8252443275426,-16.8351961035337,
-15.8849958294741));
#70283=CARTESIAN_POINT('Ctrl Pts',(-19.0379889979674,-16.8530982102727,
-15.8709781822543));
#70284=CARTESIAN_POINT('Ctrl Pts',(-19.1632599948797,-16.8750942572814,
-15.8625168311259));
#70285=CARTESIAN_POINT('Ctrl Pts',(-19.3790109474436,-16.9333445130452,
-15.8480526332529));
#70286=CARTESIAN_POINT('Ctrl Pts',(-19.4703936016526,-16.9648567998986,
-15.8419579584493));
#70287=CARTESIAN_POINT('Ctrl Pts',(-19.5727827907089,-17.008203136903,-15.8351790325248));
#70288=CARTESIAN_POINT('Ctrl Pts',(-19.5861890734478,-17.0140431854904,
-15.834292273398));
#70289=CARTESIAN_POINT('Ctrl Pts',(-19.6065883488697,-17.0231821432437,
-15.8329440050806));
#70290=CARTESIAN_POINT('Ctrl Pts',(-19.6136253662043,-17.0263811465591,
-15.8324790915359));
#70291=CARTESIAN_POINT('Ctrl Pts',(-19.6264196572196,-17.03228215644,-15.8316341081777));
#70292=CARTESIAN_POINT('Ctrl Pts',(-19.6321825534869,-17.0349716889277,
-15.8312536145012));
#70293=CARTESIAN_POINT('Ctrl Pts',(-19.6446241860039,-17.0408465938407,
-15.830432357548));
#70294=CARTESIAN_POINT('Ctrl Pts',(-19.6512985338632,-17.0440411031908,
-15.829991916534));
#70295=CARTESIAN_POINT('Ctrl Pts',(-19.6694152820357,-17.0528292696567,
-15.8287966431054));
#70296=CARTESIAN_POINT('Ctrl Pts',(-19.6808242885097,-17.058491354599,-15.8280441983949));
#70297=CARTESIAN_POINT('Ctrl Pts',(-19.736864649105,-17.0869363407314,-15.8243486947409));
#70298=CARTESIAN_POINT('Ctrl Pts',(-19.7807305280544,-17.1111969848351,
-15.8214580021697));
#70299=CARTESIAN_POINT('Ctrl Pts',(-19.972520243798,-17.2263440055466,-15.8087586334641));
#70300=CARTESIAN_POINT('Ctrl Pts',(-20.1097822604082,-17.3336539136657,
-15.7995651478959));
#70301=CARTESIAN_POINT('Ctrl Pts',(-20.2767028774611,-17.5009007693087,
-15.7865789028613));
#70302=CARTESIAN_POINT('Ctrl Pts',(-20.3190029925107,-17.5472275947927,
-15.7830864138879));
#70303=CARTESIAN_POINT('Ctrl Pts',(-20.3790003013521,-17.6191011083125,
-15.777701159777));
#70304=CARTESIAN_POINT('Ctrl Pts',(-20.3982951698573,-17.6432728292479,
-15.7758951357452));
#70305=CARTESIAN_POINT('Ctrl Pts',(-20.4213765038163,-17.6735242089087,
-15.7736289639643));
#70306=CARTESIAN_POINT('Ctrl Pts',(-20.4256717692097,-17.6792131223155,
-15.7732025488737));
#70307=CARTESIAN_POINT('Ctrl Pts',(-20.4323832446634,-17.6881962007036,
-15.772528635461));
#70308=CARTESIAN_POINT('Ctrl Pts',(-20.43481883605,-17.6914759125037,-15.7722824692301));
#70309=CARTESIAN_POINT('Ctrl Pts',(-20.4393684433719,-17.6976395022762,
-15.7718195776586));
#70310=CARTESIAN_POINT('Ctrl Pts',(-20.4414846510287,-17.700521693468,-15.7716030085297));
#70311=CARTESIAN_POINT('Ctrl Pts',(-20.4463180500014,-17.7071396725437,
-15.7711054808261));
#70312=CARTESIAN_POINT('Ctrl Pts',(-20.4490303146206,-17.710878991301,-15.7708241874036));
#70313=CARTESIAN_POINT('Ctrl Pts',(-20.4573967018467,-17.7224932726025,
-15.7699500200099));
#70314=CARTESIAN_POINT('Ctrl Pts',(-20.4630088916803,-17.730398089008,-15.7693543805379));
#70315=CARTESIAN_POINT('Ctrl Pts',(-20.5258583273272,-17.8202227624746,
-15.7625810028211));
#70316=CARTESIAN_POINT('Ctrl Pts',(-20.5772738321383,-17.9060493234008,
-15.7560680765387));
#70317=CARTESIAN_POINT('Ctrl Pts',(-20.6995936513507,-18.1474645330186,
-15.7382365925715));
#70318=CARTESIAN_POINT('Ctrl Pts',(-20.7580649171488,-18.3085600868519,
-15.7269007381697));
#70319=CARTESIAN_POINT('Ctrl Pts',(-20.8065479299507,-18.5181762317816,
-15.7134188188318));
#70320=CARTESIAN_POINT('Ctrl Pts',(-20.8151860565393,-18.5617141470192,
-15.7106795887598));
#70321=CARTESIAN_POINT('Ctrl Pts',(-20.8243855588279,-18.6171611118075,
-15.7072652976819));
#70322=CARTESIAN_POINT('Ctrl Pts',(-20.8262235214717,-18.6288442934155,
-15.7065499894799));
#70323=CARTESIAN_POINT('Ctrl Pts',(-20.8290114871888,-18.6475880950504,
-15.7054088301419));
#70324=CARTESIAN_POINT('Ctrl Pts',(-20.8300239038325,-18.6546390479199,
-15.7049810097001));
#70325=CARTESIAN_POINT('Ctrl Pts',(-20.8318772341575,-18.6680264701936,
-15.7041714350991));
#70326=CARTESIAN_POINT('Ctrl Pts',(-20.832725073561,-18.6743618862296,-15.7037894660422));
#70327=CARTESIAN_POINT('Ctrl Pts',(-20.8345859301933,-18.6887627952022,
-15.7029237900794));
#70328=CARTESIAN_POINT('Ctrl Pts',(-20.835581216502,-18.6968305085283,-15.702440647848));
#70329=CARTESIAN_POINT('Ctrl Pts',(-20.8380346042422,-18.7177062736724,
-15.7011950975299));
#70330=CARTESIAN_POINT('Ctrl Pts',(-20.8394222483241,-18.7305223864685,
-15.7004349106064));
#70331=CARTESIAN_POINT('Ctrl Pts',(-20.8476032824,-18.8131247065847,-15.6955629343406));
#70332=CARTESIAN_POINT('Ctrl Pts',(-20.8510436183218,-18.8832033407658,
-15.6915582742407));
#70333=CARTESIAN_POINT('Ctrl Pts',(-20.8508787729878,-19.1457165811452,
-15.6768592876656));
#70334=CARTESIAN_POINT('Ctrl Pts',(-20.8245352123181,-19.3371656299188,
-15.6668249584927));
#70335=CARTESIAN_POINT('Ctrl Pts',(-20.7592947613957,-19.5703427201073,
-15.6531662356899));
#70336=CARTESIAN_POINT('Ctrl Pts',(-20.744197906492,-19.6177853425968,-15.6503027376871));
#70337=CARTESIAN_POINT('Ctrl Pts',(-20.7258385662826,-19.669140776792,-15.6470652387553));
#70338=CARTESIAN_POINT('Ctrl Pts',(-20.7242171427525,-19.6736283610162,
-15.6467811654567));
#70339=CARTESIAN_POINT('Ctrl Pts',(-20.7225805821192,-19.6781103693094,
-15.6464962362309));
#70340=CARTESIAN_POINT('Origin',(-18.734,-18.952,0.));
#70341=CARTESIAN_POINT('',(-20.7225805876025,-19.6781103542923,-14.843838552956));
#70342=CARTESIAN_POINT('',(-20.7193262595591,-19.6769292106295,-15.0663814047069));
#70343=CARTESIAN_POINT('',(-20.7225805821191,-19.6781103693095,0.));
#70344=CARTESIAN_POINT('',(-20.8523539179813,-18.9502594238256,-15.1109429533473));
#70345=CARTESIAN_POINT('Ctrl Pts',(-20.7193262595591,-19.6769292106295,
-15.0663814047069));
#70346=CARTESIAN_POINT('Ctrl Pts',(-20.8041091735384,-19.4439526196368,
-15.0812352542537));
#70347=CARTESIAN_POINT('Ctrl Pts',(-20.8501556558155,-19.196755797096,-15.0960891038005));
#70348=CARTESIAN_POINT('Ctrl Pts',(-20.8523539179813,-18.9502594238256,
-15.1109429533473));
#70349=CARTESIAN_POINT('Ctrl Pts',(-20.8509992391747,-18.95020519253,-15.1101643819126));
#70350=CARTESIAN_POINT('Ctrl Pts',(-20.8509308803988,-18.8695751088215,
-15.1145732053535));
#70351=CARTESIAN_POINT('Ctrl Pts',(-20.8462561257343,-18.7890199711534,
-15.1190367568054));
#70352=CARTESIAN_POINT('Ctrl Pts',(-20.8342751942077,-18.6853612765408,
-15.125069794828));
#70353=CARTESIAN_POINT('Ctrl Pts',(-20.8311546074106,-18.6618370303696,
-15.1264585298021));
#70354=CARTESIAN_POINT('Ctrl Pts',(-20.826756724514,-18.6324788069517,-15.1282217721656));
#70355=CARTESIAN_POINT('Ctrl Pts',(-20.8258491617714,-18.6265901302598,
-15.1285769647661));
#70356=CARTESIAN_POINT('Ctrl Pts',(-20.8242842195382,-18.6167132280723,
-15.1291753914717));
#70357=CARTESIAN_POINT('Ctrl Pts',(-20.8236402483669,-18.6127228718675,
-15.1294178945615));
#70358=CARTESIAN_POINT('Ctrl Pts',(-20.8224405319096,-18.6054218499359,
-15.1298629776525));
#70359=CARTESIAN_POINT('Ctrl Pts',(-20.821888330269,-18.6021106040616,-15.1300653585031));
#70360=CARTESIAN_POINT('Ctrl Pts',(-20.8207318336752,-18.595275969606,-15.1304841894194));
#70361=CARTESIAN_POINT('Ctrl Pts',(-20.8201264943957,-18.5917528234121,
-15.1307007002396));
#70362=CARTESIAN_POINT('Ctrl Pts',(-20.8187199420528,-18.5836889585382,
-15.1311976430554));
#70363=CARTESIAN_POINT('Ctrl Pts',(-20.8179128183668,-18.5791493267093,
-15.1314784069666));
#70364=CARTESIAN_POINT('Ctrl Pts',(-20.8153705427579,-18.5651165620324,
-15.1323493287048));
#70365=CARTESIAN_POINT('Ctrl Pts',(-20.8135853322361,-18.5556327855534,
-15.1329422231047));
#70366=CARTESIAN_POINT('Ctrl Pts',(-20.7945684717144,-18.4582737898767,
-15.1390707006034));
#70367=CARTESIAN_POINT('Ctrl Pts',(-20.7718442365237,-18.3715733301528,
-15.1448765239018));
#70368=CARTESIAN_POINT('Ctrl Pts',(-20.7294006552893,-18.2433845129372,
-15.1537504213448));
#70369=CARTESIAN_POINT('Ctrl Pts',(-20.7137086156514,-18.2006589367174,
-15.1567593942611));
#70370=CARTESIAN_POINT('Ctrl Pts',(-20.6822913302299,-18.1229537239433,
-15.1622977438439));
#70371=CARTESIAN_POINT('Ctrl Pts',(-20.6669687439335,-18.0878306009927,
-15.1648268511845));
#70372=CARTESIAN_POINT('Ctrl Pts',(-20.6103521144012,-17.9671027540647,
-15.1735853664));
#70373=CARTESIAN_POINT('Ctrl Pts',(-20.5642517997688,-17.883869940186,-15.1797341935906));
#70374=CARTESIAN_POINT('Ctrl Pts',(-20.4876366961899,-17.7651617441864,
-15.1886000796092));
#70375=CARTESIAN_POINT('Ctrl Pts',(-20.4612972481923,-17.7271443148118,
-15.1914568014498));
#70376=CARTESIAN_POINT('Ctrl Pts',(-20.426585568463,-17.6803920348148,-15.1949948796788));
#70377=CARTESIAN_POINT('Ctrl Pts',(-20.419357268767,-17.6708272522518,-15.1957201083331));
#70378=CARTESIAN_POINT('Ctrl Pts',(-20.4076833152254,-17.6556495796288,
-15.1968733115488));
#70379=CARTESIAN_POINT('Ctrl Pts',(-20.4032898418012,-17.6499970514318,
-15.1973033293901));
#70380=CARTESIAN_POINT('Ctrl Pts',(-20.3949236797005,-17.6393453227619,
-15.198114728903));
#70381=CARTESIAN_POINT('Ctrl Pts',(-20.390956890882,-17.6343416092918,-15.1984963387046));
#70382=CARTESIAN_POINT('Ctrl Pts',(-20.3819269075974,-17.6230564354904,
-15.1993580712028));
#70383=CARTESIAN_POINT('Ctrl Pts',(-20.3768503032154,-17.6167857945579,
-15.1998376492528));
#70384=CARTESIAN_POINT('Ctrl Pts',(-20.3617628824936,-17.5983660731065,
-15.2012487479317));
#70385=CARTESIAN_POINT('Ctrl Pts',(-20.351652125249,-17.5862992892667,-15.2021762150453));
#70386=CARTESIAN_POINT('Ctrl Pts',(-20.2604784484587,-17.4799204241743,
-15.2103833193024));
#70387=CARTESIAN_POINT('Ctrl Pts',(-20.1713821987607,-17.3928036884123,
-15.2173013409388));
#70388=CARTESIAN_POINT('Ctrl Pts',(-19.9454701124689,-17.2078337596716,
-15.2332484884381));
#70389=CARTESIAN_POINT('Ctrl Pts',(-19.8036698529555,-17.1174519136689,
-15.2421094361227));
#70390=CARTESIAN_POINT('Ctrl Pts',(-19.6396557105219,-17.0384464582166,
-15.2526982253465));
#70391=CARTESIAN_POINT('Ctrl Pts',(-19.6265229277816,-17.0322859007933,
-15.2535485548977));
#70392=CARTESIAN_POINT('Ctrl Pts',(-19.6037124115813,-17.0218701949354,
-15.2550315091401));
#70393=CARTESIAN_POINT('Ctrl Pts',(-19.5940640423333,-17.01755160938,-15.2556606039237));
#70394=CARTESIAN_POINT('Ctrl Pts',(-19.5800043974146,-17.011384522754,-15.2565805517638));
#70395=CARTESIAN_POINT('Ctrl Pts',(-19.5756183861498,-17.0094783496594,
-15.2568679898402));
#70396=CARTESIAN_POINT('Ctrl Pts',(-19.5679101949997,-17.0061593539945,
-15.2573740060357));
#70397=CARTESIAN_POINT('Ctrl Pts',(-19.5645907650565,-17.0047401267838,
-15.2575921945907));
#70398=CARTESIAN_POINT('Ctrl Pts',(-19.5576346682157,-17.0017870600549,
-15.2580500336323));
#70399=CARTESIAN_POINT('Ctrl Pts',(-19.553997350716,-17.0002549034147,-15.2582897793109));
#70400=CARTESIAN_POINT('Ctrl Pts',(-19.5443530978565,-16.9962241479842,
-15.2589263254252));
#70401=CARTESIAN_POINT('Ctrl Pts',(-19.538338948178,-16.9937430759912,-15.2593241632859));
#70402=CARTESIAN_POINT('Ctrl Pts',(-19.5128391712561,-16.9833607066627,
-15.2610144377901));
#70403=CARTESIAN_POINT('Ctrl Pts',(-19.4932485805838,-16.9757225302507,
-15.2623215259099));
#70404=CARTESIAN_POINT('Ctrl Pts',(-19.4671271787103,-16.9659837607493,
-15.2640725150997));
#70405=CARTESIAN_POINT('Ctrl Pts',(-19.4606944937141,-16.9636209935828,
-15.2645043668025));
#70406=CARTESIAN_POINT('Ctrl Pts',(-19.2917024445415,-16.9024786952497,
-15.2758644884146));
#70407=CARTESIAN_POINT('Ctrl Pts',(-19.1225682382837,-16.8637987004395,
-15.2875343842416));
#70408=CARTESIAN_POINT('Ctrl Pts',(-18.8418510692378,-16.8349237650268,
-15.3059395948085));
#70409=CARTESIAN_POINT('Ctrl Pts',(-18.7323719107138,-16.8321775126924,
-15.3128999613875));
#70410=CARTESIAN_POINT('Ctrl Pts',(-18.6051508991758,-16.83884786069,-15.3206977000676));
#70411=CARTESIAN_POINT('Ctrl Pts',(-18.587158732243,-16.8400218447377,-15.3217940493735));
#70412=CARTESIAN_POINT('Ctrl Pts',(-18.5607995007167,-16.8420802612564,
-15.3233911888492));
#70413=CARTESIAN_POINT('Ctrl Pts',(-18.552419574071,-16.8427849163734,-15.3238975964283));
#70414=CARTESIAN_POINT('Ctrl Pts',(-18.5376422210812,-16.8441162418849,
-15.3247883008332));
#70415=CARTESIAN_POINT('Ctrl Pts',(-18.5312430750704,-16.8447221479184,
-15.325173245206));
#70416=CARTESIAN_POINT('Ctrl Pts',(-18.5187537019778,-16.8459621270846,
-15.3259230945478));
#70417=CARTESIAN_POINT('Ctrl Pts',(-18.5126632759386,-16.8465934960775,
-15.3262880805584));
#70418=CARTESIAN_POINT('Ctrl Pts',(-18.4962625038533,-16.8483656484066,
-15.327269165779));
#70419=CARTESIAN_POINT('Ctrl Pts',(-18.4859575765167,-16.8495558118618,
-15.3278837058512));
#70420=CARTESIAN_POINT('Ctrl Pts',(-18.447709328535,-16.854258405811,-15.330157970957));
#70421=CARTESIAN_POINT('Ctrl Pts',(-18.419827439645,-16.858252675877,-15.3318025101184));
#70422=CARTESIAN_POINT('Ctrl Pts',(-18.3853154434712,-16.8639017244639,
-15.3338244722909));
#70423=CARTESIAN_POINT('Ctrl Pts',(-18.378603634609,-16.8650336003671,-15.3342170583226));
#70424=CARTESIAN_POINT('Ctrl Pts',(-18.1687040477466,-16.9014729129972,
-15.3464756590207));
#70425=CARTESIAN_POINT('Ctrl Pts',(-17.9717746191708,-16.9662432872382,
-15.3572865048384));
#70426=CARTESIAN_POINT('Ctrl Pts',(-17.7393115003368,-17.0824640721618,
-15.3716602622996));
#70427=CARTESIAN_POINT('Ctrl Pts',(-17.6922372995949,-17.1082810729171,
-15.3746717993785));
#70428=CARTESIAN_POINT('Ctrl Pts',(-17.6222407070437,-17.1502064063392,
-15.3793812548432));
#70429=CARTESIAN_POINT('Ctrl Pts',(-17.5985707045904,-17.1650279731896,
-15.3810160152549));
#70430=CARTESIAN_POINT('Ctrl Pts',(-17.5694284467914,-17.1840888898497,
-15.3830909759209));
#70431=CARTESIAN_POINT('Ctrl Pts',(-17.5636733720524,-17.1878933771279,
-15.3835038308042));
#70432=CARTESIAN_POINT('Ctrl Pts',(-17.5545824903361,-17.1939671179346,
-15.3841610694151));
#70433=CARTESIAN_POINT('Ctrl Pts',(-17.5512343397524,-17.1962179324193,
-15.3844042289519));
#70434=CARTESIAN_POINT('Ctrl Pts',(-17.5449227304335,-17.2004871957905,
-15.384864732702));
#70435=CARTESIAN_POINT('Ctrl Pts',(-17.5419579582829,-17.2025036077876,
-15.3850819401012));
#70436=CARTESIAN_POINT('Ctrl Pts',(-17.535179518464,-17.2071390151867,-15.3855805833949));
#70437=CARTESIAN_POINT('Ctrl Pts',(-17.531369307363,-17.209762984131,-15.3858623543444));
#70438=CARTESIAN_POINT('Ctrl Pts',(-17.5212520442076,-17.2167794178452,
-15.3866144216391));
#70439=CARTESIAN_POINT('Ctrl Pts',(-17.514960327722,-17.2211937294096,-15.3870861499966));
#70440=CARTESIAN_POINT('Ctrl Pts',(-17.4703777093284,-17.2528368781108,
-15.3904567642226));
#70441=CARTESIAN_POINT('Ctrl Pts',(-17.4329815702175,-17.2812974782625,
-15.3934314401874));
#70442=CARTESIAN_POINT('Ctrl Pts',(-17.3833349080328,-17.3217594753665,
-15.3975525970894));
#70443=CARTESIAN_POINT('Ctrl Pts',(-17.3702346136542,-17.332702527244,-15.3986571806867));
#70444=CARTESIAN_POINT('Ctrl Pts',(-17.2464260212764,-17.4386915067362,
-15.4092511989913));
#70445=CARTESIAN_POINT('Ctrl Pts',(-17.1456888572926,-17.5447863119784,
-15.4190325569378));
#70446=CARTESIAN_POINT('Ctrl Pts',(-16.9946655190774,-17.7409138466012,
-15.4350922951708));
#70447=CARTESIAN_POINT('Ctrl Pts',(-16.9385411023579,-17.8257910000771,
-15.4415203306821));
#70448=CARTESIAN_POINT('Ctrl Pts',(-16.88148535309,-17.9272577741716,-15.4486188870818));
#70449=CARTESIAN_POINT('Ctrl Pts',(-16.8743809509526,-17.9402074539809,
-15.4495146969995));
#70450=CARTESIAN_POINT('Ctrl Pts',(-16.8637510909029,-17.9600734666077,
-15.4508738179381));
#70451=CARTESIAN_POINT('Ctrl Pts',(-16.8601272900813,-17.9669363984239,
-15.4513406184065));
#70452=CARTESIAN_POINT('Ctrl Pts',(-16.8536021175323,-17.979460404038,-15.4521875853037));
#70453=CARTESIAN_POINT('Ctrl Pts',(-16.8506883782703,-17.9851148987971,
-15.4525681857889));
#70454=CARTESIAN_POINT('Ctrl Pts',(-16.8444520088777,-17.9973525441892,
-15.4533880584895));
#70455=CARTESIAN_POINT('Ctrl Pts',(-16.8411381918925,-18.0039401109855,
-15.4538270171722));
#70456=CARTESIAN_POINT('Ctrl Pts',(-16.8322437831059,-18.0218539287416,
-15.4550143367789));
#70457=CARTESIAN_POINT('Ctrl Pts',(-16.8267299339704,-18.0332131215612,
-15.4557603635027));
#70458=CARTESIAN_POINT('Ctrl Pts',(-16.8003761900956,-18.0887647062782,
-15.4593764127651));
#70459=CARTESIAN_POINT('Ctrl Pts',(-16.7809678607989,-18.1336222051621,
-15.4621967943453));
#70460=CARTESIAN_POINT('Ctrl Pts',(-16.754904355692,-18.2000845599324,-15.4662533971502));
#70461=CARTESIAN_POINT('Ctrl Pts',(-16.7470156733704,-18.2211855716913,
-15.467523885315));
#70462=CARTESIAN_POINT('Ctrl Pts',(-16.6860209092723,-18.3926310620439,
-15.4777214838548));
#70463=CARTESIAN_POINT('Ctrl Pts',(-16.649720985206,-18.5484019781177,-15.4861694750401));
#70464=CARTESIAN_POINT('Ctrl Pts',(-16.6245782312839,-18.7639904758771,
-15.4981383683942));
#70465=CARTESIAN_POINT('Ctrl Pts',(-16.6202438299625,-18.8214561593737,
-15.5013600872869));
#70466=CARTESIAN_POINT('Ctrl Pts',(-16.6172493382223,-18.9082717148673,
-15.5063661736089));
#70467=CARTESIAN_POINT('Ctrl Pts',(-16.6168471589145,-18.9375369349987,
-15.5080775254896));
#70468=CARTESIAN_POINT('Ctrl Pts',(-16.6171006974187,-18.9738038432122,
-15.5102380946414));
#70469=CARTESIAN_POINT('Ctrl Pts',(-16.6171844278859,-18.9808079047586,
-15.5106571949296));
#70470=CARTESIAN_POINT('Ctrl Pts',(-16.6173715576251,-18.9918685717879,
-15.5113221149092));
#70471=CARTESIAN_POINT('Ctrl Pts',(-16.6174518649233,-18.9959255888242,
-15.5115666611924));
#70472=CARTESIAN_POINT('Ctrl Pts',(-16.6176249921721,-19.0035620746099,
-15.5120282446984));
#70473=CARTESIAN_POINT('Ctrl Pts',(-16.6177152293857,-19.0071415474771,
-15.5122451360844));
#70474=CARTESIAN_POINT('Ctrl Pts',(-16.6179417807768,-19.0153060330385,
-15.5127410489168));
#70475=CARTESIAN_POINT('Ctrl Pts',(-16.6180839160088,-19.019890835571,-15.5130203922669));
#70476=CARTESIAN_POINT('Ctrl Pts',(-16.618499507527,-19.0320231629289,-15.5137618067763));
#70477=CARTESIAN_POINT('Ctrl Pts',(-16.6187984518493,-19.0395696697087,
-15.5142252477047));
#70478=CARTESIAN_POINT('Ctrl Pts',(-16.6211260833301,-19.0913244605158,
-15.5174183993767));
#70479=CARTESIAN_POINT('Ctrl Pts',(-16.624500053329,-19.1354580090972,-15.520215388163));
#70480=CARTESIAN_POINT('Ctrl Pts',(-16.6305885528259,-19.191799023117,-15.52385438502));
#70481=CARTESIAN_POINT('Ctrl Pts',(-16.6320317279074,-19.2041361943857,
-15.524655459839));
#70482=CARTESIAN_POINT('Ctrl Pts',(-16.6545170514119,-19.382721211433,-15.536306501986));
#70483=CARTESIAN_POINT('Ctrl Pts',(-16.6951167656538,-19.5459131751443,
-15.547585407901));
#70484=CARTESIAN_POINT('Ctrl Pts',(-16.7753276157099,-19.7574367102437,
-15.5621666260113));
#70485=CARTESIAN_POINT('Ctrl Pts',(-16.7983831848399,-19.8113685614429,
-15.5658877801012));
#70486=CARTESIAN_POINT('Ctrl Pts',(-16.8391093525476,-19.8966509727386,
-15.5717699087376));
#70487=CARTESIAN_POINT('Ctrl Pts',(-16.8553900987904,-19.9286274173903,
-15.5739751542906));
#70488=CARTESIAN_POINT('Ctrl Pts',(-16.8777080193095,-19.9698358211046,
-15.5768185415365));
#70489=CARTESIAN_POINT('Ctrl Pts',(-16.8830147061486,-19.9794546828792,
-15.5774823643719));
#70490=CARTESIAN_POINT('Ctrl Pts',(-16.891794215331,-19.9950795596287,-15.578560995279));
#70491=CARTESIAN_POINT('Ctrl Pts',(-16.8952220621483,-20.0011104888595,
-15.5789774061524));
#70492=CARTESIAN_POINT('Ctrl Pts',(-16.901890227451,-20.0127093287419,-15.5797784521697));
#70493=CARTESIAN_POINT('Ctrl Pts',(-16.9051264339512,-20.0182795034951,
-15.5801632298342));
#70494=CARTESIAN_POINT('Ctrl Pts',(-16.9126218844305,-20.0310461939897,
-15.5810453753683));
#70495=CARTESIAN_POINT('Ctrl Pts',(-16.9168984619197,-20.0382324484232,
-15.5815421073966));
#70496=CARTESIAN_POINT('Ctrl Pts',(-16.9284341611487,-20.057357967057,-15.5828647225167));
#70497=CARTESIAN_POINT('Ctrl Pts',(-16.9357691690271,-20.0692511473504,
-15.5836878278341));
#70498=CARTESIAN_POINT('Ctrl Pts',(-16.9966065026245,-20.1657430266225,
-15.5903731984827));
#70499=CARTESIAN_POINT('Ctrl Pts',(-17.055932749397,-20.2465278285754,-15.5960081273972));
#70500=CARTESIAN_POINT('Ctrl Pts',(-17.2320281650651,-20.4537645666326,
-15.6109932072816));
#70501=CARTESIAN_POINT('Ctrl Pts',(-17.3588112912004,-20.5706601199029,
-15.6200250113701));
#70502=CARTESIAN_POINT('Ctrl Pts',(-17.5307321932079,-20.6942485935035,
-15.6320880332919));
#70503=CARTESIAN_POINT('Ctrl Pts',(-17.5638065631404,-20.7166332288957,
-15.6344039137322));
#70504=CARTESIAN_POINT('Ctrl Pts',(-17.6039778686457,-20.7421949865848,
-15.6372361337777));
#70505=CARTESIAN_POINT('Ctrl Pts',(-17.6104865023576,-20.7462869123569,
-15.6376956093319));
#70506=CARTESIAN_POINT('Ctrl Pts',(-17.6205913264878,-20.7525631976271,
-15.6384101064369));
#70507=CARTESIAN_POINT('Ctrl Pts',(-17.6241720607498,-20.7547724890996,
-15.6386635165676));
#70508=CARTESIAN_POINT('Ctrl Pts',(-17.6307962253214,-20.7588323438168,
-15.6391327660087));
#70509=CARTESIAN_POINT('Ctrl Pts',(-17.6338377493117,-20.7606859065998,
-15.6393484044117));
#70510=CARTESIAN_POINT('Ctrl Pts',(-17.6406882381524,-20.7648370523335,
-15.639834492338));
#70511=CARTESIAN_POINT('Ctrl Pts',(-17.6444997500179,-20.7671302959734,
-15.6401052179113));
#70512=CARTESIAN_POINT('Ctrl Pts',(-17.6542698666072,-20.7729667483636,
-15.6407998143986));
#70513=CARTESIAN_POINT('Ctrl Pts',(-17.660238646548,-20.7764927000111,-15.641224765878));
#70514=CARTESIAN_POINT('Ctrl Pts',(-17.6951896539675,-20.7969084812697,
-15.643716171218));
#70515=CARTESIAN_POINT('Ctrl Pts',(-17.7245509896218,-20.8131358476201,
-15.6458212515246));
#70516=CARTESIAN_POINT('Ctrl Pts',(-17.7704989558741,-20.8371231642198,
-15.6491198083931));
#70517=CARTESIAN_POINT('Ctrl Pts',(-17.7868230982952,-20.8453777982325,
-15.6502925267748));
#70518=CARTESIAN_POINT('Ctrl Pts',(-17.8254385472691,-20.864280129405,-15.6530652774896));
#70519=CARTESIAN_POINT('Ctrl Pts',(-17.8478131982875,-20.8747511780483,
-15.6546708074526));
#70520=CARTESIAN_POINT('Ctrl Pts',(-17.9113760340621,-20.9031526032054,
-15.6592198089));
#70521=CARTESIAN_POINT('Ctrl Pts',(-17.9529587003891,-20.920166908421,-15.6621815075243));
#70522=CARTESIAN_POINT('Ctrl Pts',(-18.097517025324,-20.9740125240048,-15.6723716441283));
#70523=CARTESIAN_POINT('Ctrl Pts',(-18.2027950753033,-21.0041866433303,
-15.6796016753953));
#70524=CARTESIAN_POINT('Ctrl Pts',(-18.3638784998297,-21.0371211412524,
-15.690169510304));
#70525=CARTESIAN_POINT('Ctrl Pts',(-18.4182310026962,-21.046041751751,-15.6936557104331));
#70526=CARTESIAN_POINT('Ctrl Pts',(-18.5068944925558,-21.0570623285956,
-15.6992091499861));
#70527=CARTESIAN_POINT('Ctrl Pts',(-18.5410147599938,-21.0604641879492,
-15.7013147569704));
#70528=CARTESIAN_POINT('Ctrl Pts',(-18.5859799086462,-21.0638465438054,
-15.7040499146466));
#70529=CARTESIAN_POINT('Ctrl Pts',(-18.5967617771021,-21.0645746019926,
-15.704702777422));
#70530=CARTESIAN_POINT('Ctrl Pts',(-18.6144340912719,-21.065632079852,-15.705768105147));
#70531=CARTESIAN_POINT('Ctrl Pts',(-18.6213213107339,-21.0660104281309,
-15.7061820985873));
#70532=CARTESIAN_POINT('Ctrl Pts',(-18.6346591962457,-21.0666777761213,
-15.7069815944132));
#70533=CARTESIAN_POINT('Ctrl Pts',(-18.6411095689086,-21.0669709362895,
-15.7073672229278));
#70534=CARTESIAN_POINT('Ctrl Pts',(-18.6560100703333,-21.0675798431756,
-15.7082557285045));
#70535=CARTESIAN_POINT('Ctrl Pts',(-18.6644609875387,-21.0678744837279,
-15.7087579390911));
#70536=CARTESIAN_POINT('Ctrl Pts',(-18.6872016704759,-21.0685309440704,
-15.7101048746185));
#70537=CARTESIAN_POINT('Ctrl Pts',(-18.7014938661136,-21.0687986883588,
-15.7109466558997));
#70538=CARTESIAN_POINT('Ctrl Pts',(-18.8329520578782,-21.069929634311,-15.7186481553049));
#70539=CARTESIAN_POINT('Ctrl Pts',(-18.9500047372853,-21.0612094951556,
-15.7251892443868));
#70540=CARTESIAN_POINT('Ctrl Pts',(-19.2275945879108,-21.0171651695816,
-15.7405741597957));
#70541=CARTESIAN_POINT('Ctrl Pts',(-19.3858917006964,-20.9727839205466,
-15.7492315713575));
#70542=CARTESIAN_POINT('Ctrl Pts',(-19.566331432673,-20.8987631448044,-15.7604463711599));
#70543=CARTESIAN_POINT('Ctrl Pts',(-19.5949287816643,-20.8862863686575,
-15.7622678969541));
#70544=CARTESIAN_POINT('Ctrl Pts',(-19.6297250679824,-20.870180569253,-15.7645513400857));
#70545=CARTESIAN_POINT('Ctrl Pts',(-19.636196528423,-20.8671452985234,-15.7649789126623));
#70546=CARTESIAN_POINT('Ctrl Pts',(-19.6463460496562,-20.8623220696694,
-15.7656542488097));
#70547=CARTESIAN_POINT('Ctrl Pts',(-19.6500345816461,-20.8605560952633,
-15.7659006709));
#70548=CARTESIAN_POINT('Ctrl Pts',(-19.6569379597282,-20.8572263128842,
-15.7663637733777));
#70549=CARTESIAN_POINT('Ctrl Pts',(-19.6601539694199,-20.8556650453968,
-15.7665802959298));
#70550=CARTESIAN_POINT('Ctrl Pts',(-19.6675103568105,-20.8520707065325,
-15.7670773572291));
#70551=CARTESIAN_POINT('Ctrl Pts',(-19.6716480424145,-20.850032250443,-15.7673582284861));
#70552=CARTESIAN_POINT('Ctrl Pts',(-19.6824717760563,-20.8446558418092,
-15.7680962857257));
#70553=CARTESIAN_POINT('Ctrl Pts',(-19.6891468016376,-20.8412960141394,
-15.768554787734));
#70554=CARTESIAN_POINT('Ctrl Pts',(-19.7338274804456,-20.8185090032766,
-15.771645636902));
#70555=CARTESIAN_POINT('Ctrl Pts',(-19.7712531445933,-20.7979729673008,
-15.7743405811426));
#70556=CARTESIAN_POINT('Ctrl Pts',(-19.8142369072539,-20.7726672157876,
-15.7775397000198));
#70557=CARTESIAN_POINT('Ctrl Pts',(-19.8204255206058,-20.7689811425854,
-15.7780028777329));
#70558=CARTESIAN_POINT('Ctrl Pts',(-19.9612667917299,-20.6841162126135,
-15.7886011420379));
#70559=CARTESIAN_POINT('Ctrl Pts',(-20.086479597217,-20.5882189962405,-15.7991743953588));
#70560=CARTESIAN_POINT('Ctrl Pts',(-20.2683631254329,-20.4136489942513,
-15.8155535235058));
#70561=CARTESIAN_POINT('Ctrl Pts',(-20.3323175777072,-20.3434284351539,
-15.8215791495485));
#70562=CARTESIAN_POINT('Ctrl Pts',(-20.4046232472794,-20.2524468092857,
-15.8287172278721));
#70563=CARTESIAN_POINT('Ctrl Pts',(-20.4176410443256,-20.2355485282016,
-15.8300172747308));
#70564=CARTESIAN_POINT('Ctrl Pts',(-20.4357852640571,-20.2112445758436,
-15.8318515008308));
#70565=CARTESIAN_POINT('Ctrl Pts',(-20.4411229329346,-20.2039989147406,
-15.8323939340964));
#70566=CARTESIAN_POINT('Ctrl Pts',(-20.4502504309102,-20.191441820576,-15.8333265210172));
#70567=CARTESIAN_POINT('Ctrl Pts',(-20.4540621746829,-20.186146541095,-15.8337175219323));
#70568=CARTESIAN_POINT('Ctrl Pts',(-20.4613129493773,-20.1759749093206,
-15.8344643000007));
#70569=CARTESIAN_POINT('Ctrl Pts',(-20.4647559571994,-20.1711014812041,
-15.834820227979));
#70570=CARTESIAN_POINT('Ctrl Pts',(-20.4736538365658,-20.1583932471106,
-15.8357435658547));
#70571=CARTESIAN_POINT('Ctrl Pts',(-20.4790764370083,-20.1505359282427,
-15.8363097396569));
#70572=CARTESIAN_POINT('Ctrl Pts',(-20.4973780544504,-20.123629447374,-15.8382327969975));
#70573=CARTESIAN_POINT('Ctrl Pts',(-20.5100000716278,-20.1044068428274,
-15.8395799884682));
#70574=CARTESIAN_POINT('Ctrl Pts',(-20.6034752477959,-19.9568649445858,
-15.849729202511));
#70575=CARTESIAN_POINT('Ctrl Pts',(-20.6706038316627,-19.8204578153052,
-15.857987109407));
#70576=CARTESIAN_POINT('Ctrl Pts',(-20.7225805818996,-19.6781103699108,
-15.8662165012922));
#70577=CARTESIAN_POINT('',(-20.850999748114,-18.9530327076519,-14.890777192852));
#70578=CARTESIAN_POINT('Ctrl Pts',(-20.7225805821192,-19.6781103693094,
-15.6464962362309));
#70579=CARTESIAN_POINT('Ctrl Pts',(-20.7215382005989,-19.6809651139018,
-15.6463147550481));
#70580=CARTESIAN_POINT('Ctrl Pts',(-20.7204896781789,-19.6838175964211,
-15.6461329266281));
#70581=CARTESIAN_POINT('Ctrl Pts',(-20.7178168237568,-19.6910409683998,
-15.6456712114951));
#70582=CARTESIAN_POINT('Ctrl Pts',(-20.7161841986203,-19.6954087334581,
-15.6453908458301));
#70583=CARTESIAN_POINT('Ctrl Pts',(-20.713268966459,-19.703129981681,-15.6448930705602));
#70584=CARTESIAN_POINT('Ctrl Pts',(-20.711992242547,-19.7064856388513,-15.644676014502));
#70585=CARTESIAN_POINT('Ctrl Pts',(-20.7092701408642,-19.7135858327957,
-15.6442151944605));
#70586=CARTESIAN_POINT('Ctrl Pts',(-20.707822671301,-19.7173294530747,-15.6439713114886));
#70587=CARTESIAN_POINT('Ctrl Pts',(-20.7038921043828,-19.727409838564,-15.6433121929136));
#70588=CARTESIAN_POINT('Ctrl Pts',(-20.7013891053025,-19.7337387198285,
-15.6428957881994));
#70589=CARTESIAN_POINT('Ctrl Pts',(-20.6888792590765,-19.7649294771773,
-15.6408312283235));
#70590=CARTESIAN_POINT('Ctrl Pts',(-20.6784319306481,-19.7896106279086,
-15.6391586007787));
#70591=CARTESIAN_POINT('Ctrl Pts',(-20.6469617777437,-19.8601931391508,
-15.6342757408071));
#70592=CARTESIAN_POINT('Ctrl Pts',(-20.624762662322,-19.9055478045807,-15.6310149021864));
#70593=CARTESIAN_POINT('Ctrl Pts',(-20.5384183300512,-20.0670626330061,
-15.6190523714896));
#70594=CARTESIAN_POINT('Ctrl Pts',(-20.465010723893,-20.1779261629286,-15.6101841681029));
#70595=CARTESIAN_POINT('Ctrl Pts',(-20.3168837375819,-20.3615484045732,
-15.5948582422368));
#70596=CARTESIAN_POINT('Ctrl Pts',(-20.2462642317458,-20.4370622909368,
-15.5883172978543));
#70597=CARTESIAN_POINT('Ctrl Pts',(-20.1600892169511,-20.5166583489903,
-15.5811566450355));
#70598=CARTESIAN_POINT('Ctrl Pts',(-20.1496786630315,-20.5260839055539,
-15.5803038367314));
#70599=CARTESIAN_POINT('Ctrl Pts',(-20.1329049467825,-20.5409695473105,
-15.5789489441957));
#70600=CARTESIAN_POINT('Ctrl Pts',(-20.1266019392175,-20.546496508136,-15.5784440592285));
#70601=CARTESIAN_POINT('Ctrl Pts',(-20.1153950606441,-20.5562064165061,
-15.5775537585517));
#70602=CARTESIAN_POINT('Ctrl Pts',(-20.1105046347987,-20.5604046543496,
-15.5771677101394));
#70603=CARTESIAN_POINT('Ctrl Pts',(-20.1003178022324,-20.5690691576568,
-15.5763686079997));
#70604=CARTESIAN_POINT('Ctrl Pts',(-20.0950184846581,-20.5735318940789,
-15.5759557021595));
#70605=CARTESIAN_POINT('Ctrl Pts',(-20.0812910645662,-20.5849775189835,
-15.5748932258545));
#70606=CARTESIAN_POINT('Ctrl Pts',(-20.0728304786987,-20.5919212622195,
-15.5742452531959));
#70607=CARTESIAN_POINT('Ctrl Pts',(-20.0366931772938,-20.6211136748238,
-15.5715060498402));
#70608=CARTESIAN_POINT('Ctrl Pts',(-20.0085118919996,-20.6427305013262,
-15.5694401576718));
#70609=CARTESIAN_POINT('Ctrl Pts',(-19.9330683626312,-20.6976416156175,
-15.5640773526727));
#70610=CARTESIAN_POINT('Ctrl Pts',(-19.8849624425687,-20.7297276991296,
-15.5608243703641));
#70611=CARTESIAN_POINT('Ctrl Pts',(-19.6972067777359,-20.8441380470949,
-15.548624870114));
#70612=CARTESIAN_POINT('Ctrl Pts',(-19.549598286454,-20.9122927572047,-15.5400738501042));
#70613=CARTESIAN_POINT('Ctrl Pts',(-19.3750795392248,-20.9697155083056,
-15.5298130487453));
#70614=CARTESIAN_POINT('Ctrl Pts',(-19.3543872166229,-20.9761735346412,
-15.5285934138505));
#70615=CARTESIAN_POINT('Ctrl Pts',(-19.293322846051,-20.9942073073806,-15.5249757427993));
#70616=CARTESIAN_POINT('Ctrl Pts',(-19.2527036715844,-21.0049000715263,
-15.5225458747638));
#70617=CARTESIAN_POINT('Ctrl Pts',(-19.2045512407733,-21.0160556781879,
-15.5196092950154));
#70618=CARTESIAN_POINT('Ctrl Pts',(-19.197297201433,-21.0176960115941,-15.5191654218524));
#70619=CARTESIAN_POINT('Ctrl Pts',(-19.18554097764,-21.02028937109,-15.518443438665));
#70620=CARTESIAN_POINT('Ctrl Pts',(-19.181043993016,-21.0212660158721,-15.5181666465004));
#70621=CARTESIAN_POINT('Ctrl Pts',(-19.1730489573006,-21.0229750809553,
-15.5176733897125));
#70622=CARTESIAN_POINT('Ctrl Pts',(-19.1695521994188,-21.023713313711,-15.5174572611286));
#70623=CARTESIAN_POINT('Ctrl Pts',(-19.1620433600095,-21.0252787228024,
-15.5169922892256));
#70624=CARTESIAN_POINT('Ctrl Pts',(-19.1580308018883,-21.0261030974535,
-15.5167432954317));
#70625=CARTESIAN_POINT('Ctrl Pts',(-19.1469794525936,-21.0283401725998,
-15.5160561283976));
#70626=CARTESIAN_POINT('Ctrl Pts',(-19.1399359049353,-21.0297287066164,
-15.5156166134304));
#70627=CARTESIAN_POINT('Ctrl Pts',(-19.1018144991776,-21.0370425511314,
-15.5132299795146));
#70628=CARTESIAN_POINT('Ctrl Pts',(-19.0706156026954,-21.0423061099051,
-15.5112485289031));
#70629=CARTESIAN_POINT('Ctrl Pts',(-18.8775501419016,-21.0704440605135,
-15.4988613725745));
#70630=CARTESIAN_POINT('Ctrl Pts',(-18.7136063234049,-21.0752041327929,
-15.4878510547611));
#70631=CARTESIAN_POINT('Ctrl Pts',(-18.4341378647768,-21.0509217587739,
-15.4695259740205));
#70632=CARTESIAN_POINT('Ctrl Pts',(-18.3185533404816,-21.0311348620421,
-15.4620692031308));
#70633=CARTESIAN_POINT('Ctrl Pts',(-18.1913415565047,-20.9983174456796,
-15.4540473203771));
#70634=CARTESIAN_POINT('Ctrl Pts',(-18.1775384304006,-20.9946071115307,
-15.4531791517874));
#70635=CARTESIAN_POINT('Ctrl Pts',(-18.155630753867,-20.988479685448,-15.4518045969395));
#70636=CARTESIAN_POINT('Ctrl Pts',(-18.1475014682284,-20.9861533790708,
-15.4512952809801));
#70637=CARTESIAN_POINT('Ctrl Pts',(-18.1331893047511,-20.9819648271838,
-15.450399838472));
#70638=CARTESIAN_POINT('Ctrl Pts',(-18.1270006416119,-20.9801228935837,
-15.4500130554991));
#70639=CARTESIAN_POINT('Ctrl Pts',(-18.1142184360722,-20.9762547742637,
-15.4492149990802));
#70640=CARTESIAN_POINT('Ctrl Pts',(-18.1076261681221,-20.9742246172432,
-15.4488038608594));
#70641=CARTESIAN_POINT('Ctrl Pts',(-18.0907312497104,-20.9689311107601,
-15.4477512714696));
#70642=CARTESIAN_POINT('Ctrl Pts',(-18.0804433716501,-20.9656209997779,
-15.4471113609103));
#70643=CARTESIAN_POINT('Ctrl Pts',(-18.0376200206075,-20.9514798733221,
-15.4444516501353));
#70644=CARTESIAN_POINT('Ctrl Pts',(-18.0053236990031,-20.9399375956609,
-15.4424553571148));
#70645=CARTESIAN_POINT('Ctrl Pts',(-17.9219259782214,-20.9078266242942,
-15.4373139163172));
#70646=CARTESIAN_POINT('Ctrl Pts',(-17.8713207626631,-20.8860390841569,
-15.4342081046017));
#70647=CARTESIAN_POINT('Ctrl Pts',(-17.7229740603503,-20.8151871403612,
-15.4250667425354));
#70648=CARTESIAN_POINT('Ctrl Pts',(-17.6281230726459,-20.760501279765,-15.4191799316769));
#70649=CARTESIAN_POINT('Ctrl Pts',(-17.5024545718971,-20.674449547118,-15.4108878219961));
#70650=CARTESIAN_POINT('Ctrl Pts',(-17.4677376394491,-20.649090459584,-15.4085381838538));
#70651=CARTESIAN_POINT('Ctrl Pts',(-17.3741929581124,-20.5762912399506,
-15.4019762949796));
#70652=CARTESIAN_POINT('Ctrl Pts',(-17.3171014990814,-20.5267359424784,
-15.397707230493));
#70653=CARTESIAN_POINT('Ctrl Pts',(-17.2559605706217,-20.4676446069254,
-15.39266782742));
#70654=CARTESIAN_POINT('Ctrl Pts',(-17.2491787063536,-20.4610012748967,
-15.3921019399614));
#70655=CARTESIAN_POINT('Ctrl Pts',(-17.2391915853088,-20.4510856485608,
-15.3912578735231));
#70656=CARTESIAN_POINT('Ctrl Pts',(-17.2359517887871,-20.4478480986818,
-15.3909823647082));
#70657=CARTESIAN_POINT('Ctrl Pts',(-17.230204245092,-20.4420671412002,-15.3904905149705));
#70658=CARTESIAN_POINT('Ctrl Pts',(-17.2276924031895,-20.439527875814,-15.3902745028146));
#70659=CARTESIAN_POINT('Ctrl Pts',(-17.2223035852484,-20.4340525788117,
-15.3898087770304));
#70660=CARTESIAN_POINT('Ctrl Pts',(-17.2194287728867,-20.4311145642146,
-15.3895589076406));
#70661=CARTESIAN_POINT('Ctrl Pts',(-17.2115116896153,-20.4229761431723,
-15.3888669086129));
#70662=CARTESIAN_POINT('Ctrl Pts',(-17.2064875802117,-20.4177582586973,
-15.3884234064824));
#70663=CARTESIAN_POINT('Ctrl Pts',(-17.1790231774189,-20.3889400224135,
-15.3859754000312));
#70664=CARTESIAN_POINT('Ctrl Pts',(-17.1571042851005,-20.3648514363793,
-15.3839344879802));
#70665=CARTESIAN_POINT('Ctrl Pts',(-17.0290710793708,-20.2174527716086,
-15.3715278443063));
#70666=CARTESIAN_POINT('Ctrl Pts',(-16.9369053699052,-20.0827538043303,
-15.3605726816256));
#70667=CARTESIAN_POINT('Ctrl Pts',(-16.8066268175575,-19.8354954811239,
-15.342317278926));
#70668=CARTESIAN_POINT('Ctrl Pts',(-16.7608186066422,-19.7278186919677,
-15.334877095808));
#70669=CARTESIAN_POINT('Ctrl Pts',(-16.7196357931291,-19.6033294279771,
-15.3268706501961));
#70670=CARTESIAN_POINT('Ctrl Pts',(-16.7152852994567,-19.5897179276128,
-15.3260026821719));
#70671=CARTESIAN_POINT('Ctrl Pts',(-16.7085806030627,-19.5679843704653,
-15.324628383856));
#70672=CARTESIAN_POINT('Ctrl Pts',(-16.7061367273819,-19.559890638975,-15.3241191255642));
#70673=CARTESIAN_POINT('Ctrl Pts',(-16.7019120782303,-19.5455902352014,
-15.3232237501348));
#70674=CARTESIAN_POINT('Ctrl Pts',(-16.7001111036489,-19.5393896899517,
-15.3228369768826));
#70675=CARTESIAN_POINT('Ctrl Pts',(-16.6964447782729,-19.5265479108118,
-15.3220389076684));
#70676=CARTESIAN_POINT('Ctrl Pts',(-16.6945834615177,-19.5199055975265,
-15.3216277470936));
#70677=CARTESIAN_POINT('Ctrl Pts',(-16.6898890436285,-19.5028323033913,
-15.3205750324749));
#70678=CARTESIAN_POINT('Ctrl Pts',(-16.687103279785,-19.4923884267351,-15.3199350197606));
#70679=CARTESIAN_POINT('Ctrl Pts',(-16.6758102403467,-19.4487099715188,
-15.3172743162655));
#70680=CARTESIAN_POINT('Ctrl Pts',(-16.6680311637819,-19.4152913197268,
-15.3152771550845));
#70681=CARTESIAN_POINT('Ctrl Pts',(-16.6498822265504,-19.327737688799,-15.3101329729858));
#70682=CARTESIAN_POINT('Ctrl Pts',(-16.640807658563,-19.2733598786047,-15.3070253431617));
#70683=CARTESIAN_POINT('Ctrl Pts',(-16.6200900354575,-19.1102104048834,
-15.2978808090869));
#70684=CARTESIAN_POINT('Ctrl Pts',(-16.6147400597023,-19.0008268301613,
-15.2919926338135));
#70685=CARTESIAN_POINT('Ctrl Pts',(-16.6191736214412,-18.8457009827542,
-15.2835434786426));
#70686=CARTESIAN_POINT('Ctrl Pts',(-16.6219708881489,-18.7999378945219,
-15.2810371418153));
#70687=CARTESIAN_POINT('Ctrl Pts',(-16.6283556988882,-18.7318661195058,
-15.2772456994723));
#70688=CARTESIAN_POINT('Ctrl Pts',(-16.6308182625417,-18.7094646886026,
-15.2759876589647));
#70689=CARTESIAN_POINT('Ctrl Pts',(-16.6343888314768,-18.6811532594336,
-15.2743800372108));
#70690=CARTESIAN_POINT('Ctrl Pts',(-16.6351650644398,-18.6752023699536,
-15.2740411320029));
#70691=CARTESIAN_POINT('Ctrl Pts',(-16.6420724354838,-18.6239480927944,
-15.2711130222594));
#70692=CARTESIAN_POINT('Ctrl Pts',(-16.6496438015094,-18.578854508832,-15.2684752227161));
#70693=CARTESIAN_POINT('Ctrl Pts',(-16.6601732546215,-18.5265710909261,
-15.2653079566838));
#70694=CARTESIAN_POINT('Ctrl Pts',(-16.6617187981786,-18.5191053902604,
-15.2648530790375));
#70695=CARTESIAN_POINT('Ctrl Pts',(-16.66426314209,-18.5071409501252,-15.2641196620535));
#70696=CARTESIAN_POINT('Ctrl Pts',(-16.6652363801142,-18.5026367623359,
-15.2638425453159));
#70697=CARTESIAN_POINT('Ctrl Pts',(-16.6669925174339,-18.494635914592,-15.2633484426436));
#70698=CARTESIAN_POINT('Ctrl Pts',(-16.6677695966785,-18.4911380251998,
-15.2631317922469));
#70699=CARTESIAN_POINT('Ctrl Pts',(-16.6694428448938,-18.4836954878489,
-15.2626694507465));
#70700=CARTESIAN_POINT('Ctrl Pts',(-16.6703414263075,-18.4797514919101,
-15.2624236285701));
#70701=CARTESIAN_POINT('Ctrl Pts',(-16.6728139530036,-18.4690410555934,
-15.2617538953122));
#70702=CARTESIAN_POINT('Ctrl Pts',(-16.6744098945089,-18.4622798180716,
-15.2613287509825));
#70703=CARTESIAN_POINT('Ctrl Pts',(-16.6827294761852,-18.4277938285908,
-15.2591486617646));
#70704=CARTESIAN_POINT('Ctrl Pts',(-16.6899794236814,-18.4002006072036,
-15.2573659075871));
#70705=CARTESIAN_POINT('Ctrl Pts',(-16.7129483545565,-18.3194568455118,
-15.2520523826054));
#70706=CARTESIAN_POINT('Ctrl Pts',(-16.730198957188,-18.2667692837795,-15.2484607159687));
#70707=CARTESIAN_POINT('Ctrl Pts',(-16.7980417738446,-18.0841341650226,
-15.2356998065876));
#70708=CARTESIAN_POINT('Ctrl Pts',(-16.8593845123562,-17.9585478960011,
-15.2263847169485));
#70709=CARTESIAN_POINT('Ctrl Pts',(-16.9799883621592,-17.7631941414895,
-15.2115627947521));
#70710=CARTESIAN_POINT('Ctrl Pts',(-17.0322022829082,-17.6895799289483,
-15.2058809790918));
#70711=CARTESIAN_POINT('Ctrl Pts',(-17.0975939666049,-17.6088497740306,
-15.199542103372));
#70712=CARTESIAN_POINT('Ctrl Pts',(-17.1063331811176,-17.5982725620446,
-15.1987091711963));
#70713=CARTESIAN_POINT('Ctrl Pts',(-17.1205158216737,-17.5814429958551,
-15.1973797690614));
#70714=CARTESIAN_POINT('Ctrl Pts',(-17.1258941064206,-17.575136487009,-15.1968806613508));
#70715=CARTESIAN_POINT('Ctrl Pts',(-17.1355107893663,-17.5639933010039,
-15.1959970247908));
#70716=CARTESIAN_POINT('Ctrl Pts',(-17.1397344247621,-17.5591440742142,
-15.1956118940241));
#70717=CARTESIAN_POINT('Ctrl Pts',(-17.1485820545855,-17.5490789318872,
-15.1948112263512));
#70718=CARTESIAN_POINT('Ctrl Pts',(-17.1532098515782,-17.5438664504261,
-15.1943958545485));
#70719=CARTESIAN_POINT('Ctrl Pts',(-17.1652981621679,-17.5303855776059,
-15.1933196288962));
#70720=CARTESIAN_POINT('Ctrl Pts',(-17.1727983867463,-17.522152962056,-15.1926604536255));
#70721=CARTESIAN_POINT('Ctrl Pts',(-17.2056823888846,-17.4866250945433,
-15.1898067800555));
#70722=CARTESIAN_POINT('Ctrl Pts',(-17.2317205046333,-17.4599427283636,
-15.1876403909399));
#70723=CARTESIAN_POINT('Ctrl Pts',(-17.3027982590784,-17.3908544570607,
-15.1819520632266));
#70724=CARTESIAN_POINT('Ctrl Pts',(-17.349015341122,-17.3497103305656,-15.1784813768306));
#70725=CARTESIAN_POINT('Ctrl Pts',(-17.5080711926025,-17.2201450973463,
-15.1671327179264));
#70726=CARTESIAN_POINT('Ctrl Pts',(-17.6280672587318,-17.1411623411707,
-15.1595222932053));
#70727=CARTESIAN_POINT('Ctrl Pts',(-17.8209694150088,-17.0405659631828,
-15.1474692355978));
#70728=CARTESIAN_POINT('Ctrl Pts',(-17.8885766653055,-17.0097173607798,
-15.1432689572719));
#70729=CARTESIAN_POINT('Ctrl Pts',(-17.9664518545203,-16.9790204699717,
-15.1383075629105));
#70730=CARTESIAN_POINT('Ctrl Pts',(-17.9752703218368,-16.9756124748641,
-15.1377439976544));
#70731=CARTESIAN_POINT('Ctrl Pts',(-17.9883871164501,-16.9706440664972,
-15.1369027392614));
#70732=CARTESIAN_POINT('Ctrl Pts',(-17.9926682888784,-16.9690382755767,
-15.1366276905548));
#70733=CARTESIAN_POINT('Ctrl Pts',(-18.0003022405588,-16.9662030943809,
-15.1361363434057));
#70734=CARTESIAN_POINT('Ctrl Pts',(-18.0036529607038,-16.9649683056048,
-15.1359203711214));
#70735=CARTESIAN_POINT('Ctrl Pts',(-18.0108722935925,-16.9623286051126,
-15.1354543665416));
#70736=CARTESIAN_POINT('Ctrl Pts',(-18.0147418274363,-16.9609265156853,
-15.1352041765559));
#70737=CARTESIAN_POINT('Ctrl Pts',(-18.0254550431428,-16.9570799876455,
-15.134510406041));
#70738=CARTESIAN_POINT('Ctrl Pts',(-18.0323071852899,-16.9546595177993,
-15.1340654416635));
#70739=CARTESIAN_POINT('Ctrl Pts',(-18.070262434483,-16.9414715145958,-15.1315944476733));
#70740=CARTESIAN_POINT('Ctrl Pts',(-18.1015991007315,-16.9313958400787,
-15.1295312164146));
#70741=CARTESIAN_POINT('Ctrl Pts',(-18.2888648410165,-16.8759669699032,
-15.1171169597771));
#70742=CARTESIAN_POINT('Ctrl Pts',(-18.4493551482041,-16.8479477810541,
-15.1061821037736));
#70743=CARTESIAN_POINT('Ctrl Pts',(-18.7279782325901,-16.8317942015676,
-15.087952777577));
#70744=CARTESIAN_POINT('Ctrl Pts',(-18.8448602567619,-16.8346840862477,
-15.080519090292));
#70745=CARTESIAN_POINT('Ctrl Pts',(-18.975130882362,-16.8487289660873,-15.0725186922775));
#70746=CARTESIAN_POINT('Ctrl Pts',(-18.9893208711825,-16.850404317435,-15.0716508042757));
#70747=CARTESIAN_POINT('Ctrl Pts',(-19.0118784083963,-16.8532994349065,
-15.0702766083134));
#70748=CARTESIAN_POINT('Ctrl Pts',(-19.0202572980912,-16.8544258691753,
-15.0697673730315));
#70749=CARTESIAN_POINT('Ctrl Pts',(-19.0350231259204,-16.8565010699138,
-15.068872024366));
#70750=CARTESIAN_POINT('Ctrl Pts',(-19.0414128501888,-16.8574289151946,
-15.0684852549911));
#70751=CARTESIAN_POINT('Ctrl Pts',(-19.0546203077015,-16.8594084957146,
-15.0676871806656));
#70752=CARTESIAN_POINT('Ctrl Pts',(-19.0614373529596,-16.8604643519326,
-15.0672760111667));
#70753=CARTESIAN_POINT('Ctrl Pts',(-19.0789230127468,-16.8632601984035,
-15.0662232465561));
#70754=CARTESIAN_POINT('Ctrl Pts',(-19.0895837652939,-16.8650486263655,
-15.0655831930613));
#70755=CARTESIAN_POINT('Ctrl Pts',(-19.1340249684607,-16.8728544245807,
-15.0629220931672));
#70756=CARTESIAN_POINT('Ctrl Pts',(-19.167671425178,-16.8796111390781,-15.0609245853173));
#70757=CARTESIAN_POINT('Ctrl Pts',(-19.2549012942788,-16.8993458582374,
-15.055779308439));
#70758=CARTESIAN_POINT('Ctrl Pts',(-19.3081692601104,-16.9136041869511,
-15.052670952495));
#70759=CARTESIAN_POINT('Ctrl Pts',(-19.4636262519155,-16.9617943301914,
-15.0436213041689));
#70760=CARTESIAN_POINT('Ctrl Pts',(-19.5638523666862,-17.0014567341608,
-15.0378222665605));
#70761=CARTESIAN_POINT('Ctrl Pts',(-19.7686997248433,-17.1011804358314,
-15.025422299592));
#70762=CARTESIAN_POINT('Ctrl Pts',(-19.8720797850926,-17.1628933623888,
-15.0188266624207));
#70763=CARTESIAN_POINT('Ctrl Pts',(-19.977364919844,-17.2385756668261,-15.0111420220576));
#70764=CARTESIAN_POINT('Ctrl Pts',(-19.9850420139582,-17.2441729768176,
-15.0105757005653));
#70765=CARTESIAN_POINT('Ctrl Pts',(-19.9963649030556,-17.2525457219582,
-15.009731109385));
#70766=CARTESIAN_POINT('Ctrl Pts',(-20.0000399049371,-17.2552817117086,
-15.0094555146848));
#70767=CARTESIAN_POINT('Ctrl Pts',(-20.0064390939317,-17.2600781876615,
-15.0089729992529));
#70768=CARTESIAN_POINT('Ctrl Pts',(-20.0091672108293,-17.2621333629289,
-15.0087664512564));
#70769=CARTESIAN_POINT('Ctrl Pts',(-20.0150561291599,-17.2665920490921,
-15.0083187585703));
#70770=CARTESIAN_POINT('Ctrl Pts',(-20.0182150982555,-17.268997817038,-15.0080774586215));
#70771=CARTESIAN_POINT('Ctrl Pts',(-20.0266048131899,-17.2754245242627,
-15.0074335907187));
#70772=CARTESIAN_POINT('Ctrl Pts',(-20.0318235126544,-17.2794610150206,
-15.0070299489986));
#70773=CARTESIAN_POINT('Ctrl Pts',(-20.0434206209078,-17.2885179512195,
-15.0061261168653));
#70774=CARTESIAN_POINT('Ctrl Pts',(-20.0497891623606,-17.2935507952878,
-15.0056251116606));
#70775=CARTESIAN_POINT('Ctrl Pts',(-20.0690118635665,-17.3089222656419,
-15.0040990779448));
#70776=CARTESIAN_POINT('Ctrl Pts',(-20.0817739702814,-17.3193743826084,
-15.003067040158));
#70777=CARTESIAN_POINT('Ctrl Pts',(-20.1289504563412,-17.358941859414,-14.9991849236106));
#70778=CARTESIAN_POINT('Ctrl Pts',(-20.1625525541588,-17.389003488229,-14.9962845061265));
#70779=CARTESIAN_POINT('Ctrl Pts',(-20.2500826201925,-17.4724926968091,
-14.9884117506999));
#70780=CARTESIAN_POINT('Ctrl Pts',(-20.3021401358658,-17.5277864305359,
-14.9833857751019));
#70781=CARTESIAN_POINT('Ctrl Pts',(-20.4510375815278,-17.7040243071374,
-14.9681454430927));
#70782=CARTESIAN_POINT('Ctrl Pts',(-20.5377009563585,-17.832919720385,-14.9580580753843));
#70783=CARTESIAN_POINT('Ctrl Pts',(-20.6206412514692,-17.9913506668948,
-14.947040598894));
#70784=CARTESIAN_POINT('Ctrl Pts',(-20.6313864541042,-18.012751858876,-14.9455779571933));
#70785=CARTESIAN_POINT('Ctrl Pts',(-20.645973430585,-18.0430771293405,-14.94354034568));
#70786=CARTESIAN_POINT('Ctrl Pts',(-20.6501201139051,-18.0518517355091,
-14.9429548089173));
#70787=CARTESIAN_POINT('Ctrl Pts',(-20.6567308726811,-18.0660931530048,
-14.9420109045188));
#70788=CARTESIAN_POINT('Ctrl Pts',(-20.6592322829528,-18.0715423870848,
-14.9416512493241));
#70789=CARTESIAN_POINT('Ctrl Pts',(-20.664397467424,-18.0829218222117,-14.9409033130694));
#70790=CARTESIAN_POINT('Ctrl Pts',(-20.6670571477576,-18.0888538210115,
-14.9405151759685));
#70791=CARTESIAN_POINT('Ctrl Pts',(-20.6732798987867,-18.1029057179177,
-14.9395998383254));
#70792=CARTESIAN_POINT('Ctrl Pts',(-20.6768193795688,-18.1110359771549,
-14.9390734498376));
#70793=CARTESIAN_POINT('Ctrl Pts',(-20.6883951620446,-18.1380889539118,
-14.937332370114));
#70794=CARTESIAN_POINT('Ctrl Pts',(-20.6962070636656,-18.1571068476923,
-14.9361253045819));
#70795=CARTESIAN_POINT('Ctrl Pts',(-20.736185600108,-18.2586162775481,-14.9297670310457));
#70796=CARTESIAN_POINT('Ctrl Pts',(-20.7634324080283,-18.3429557947427,
-14.9247830122503));
#70797=CARTESIAN_POINT('Ctrl Pts',(-20.8290276887774,-18.6001176753881,
-14.9101344054699));
#70798=CARTESIAN_POINT('Ctrl Pts',(-20.851085988477,-18.7762442174503,-14.9008595449284));
#70799=CARTESIAN_POINT('Ctrl Pts',(-20.850999748114,-18.9530327076519,-14.890777192852));
#70800=CARTESIAN_POINT('Ctrl Pts',(-20.8509997467307,-18.9530355395134,
-14.8907770313492));
#70801=CARTESIAN_POINT('Ctrl Pts',(-20.8509866388438,-18.9798325789464,
-14.889248779021));
#70802=CARTESIAN_POINT('Ctrl Pts',(-20.8504647357704,-19.0066259838651,
-14.8877018299672));
#70803=CARTESIAN_POINT('Ctrl Pts',(-20.8488772347909,-19.0478815498525,
-14.8852810116848));
#70804=CARTESIAN_POINT('Ctrl Pts',(-20.8481713904245,-19.0623553181648,
-14.8844243242303));
#70805=CARTESIAN_POINT('Ctrl Pts',(-20.8470399810294,-19.081511077281,-14.883279390487));
#70806=CARTESIAN_POINT('Ctrl Pts',(-20.8467473096707,-19.086200913193,-14.8829981965203));
#70807=CARTESIAN_POINT('Ctrl Pts',(-20.8462061821127,-19.0944311785953,
-14.8825031124846));
#70808=CARTESIAN_POINT('Ctrl Pts',(-20.845964430651,-19.0979720508692,-14.8822895904033));
#70809=CARTESIAN_POINT('Ctrl Pts',(-20.845471825666,-19.1049296118924,-14.8818689752654));
#70810=CARTESIAN_POINT('Ctrl Pts',(-20.8452215797263,-19.1083463397607,
-14.881661915791));
#70811=CARTESIAN_POINT('Ctrl Pts',(-20.844666932587,-19.1156749680097,-14.8812166858999));
#70812=CARTESIAN_POINT('Ctrl Pts',(-20.8443599504657,-19.1195866174848,
-14.8809783745506));
#70813=CARTESIAN_POINT('Ctrl Pts',(-20.8435234725452,-19.1298783426118,
-14.8803496430295));
#70814=CARTESIAN_POINT('Ctrl Pts',(-20.8429759117084,-19.1362568516816,
-14.8799582295632));
#70815=CARTESIAN_POINT('Ctrl Pts',(-20.8405832034925,-19.1627202290814,
-14.8783273541142));
#70816=CARTESIAN_POINT('Ctrl Pts',(-20.8384800664517,-19.1827799588661,
-14.8770744599677));
#70817=CARTESIAN_POINT('Ctrl Pts',(-20.8355857381717,-19.2070383408862,
-14.8755415821871));
#70818=CARTESIAN_POINT('Ctrl Pts',(-20.835067953567,-19.2112694045152,-14.8752735671886));
#70819=CARTESIAN_POINT('Ctrl Pts',(-20.8313092268496,-19.2412328988615,
-14.873371027654));
#70820=CARTESIAN_POINT('Ctrl Pts',(-20.8276085505026,-19.2669044098143,
-14.8717174315256));
#70821=CARTESIAN_POINT('Ctrl Pts',(-20.8020054287801,-19.4240147384879,
-14.8614773343571));
#70822=CARTESIAN_POINT('Ctrl Pts',(-20.7682211192295,-19.5531157516609,
-14.8525677751688));
#70823=CARTESIAN_POINT('Ctrl Pts',(-20.7225805876025,-19.6781103542923,
-14.843838552956));
#70824=CARTESIAN_POINT('Origin',(-18.734,-18.952,0.));
#70825=CARTESIAN_POINT('',(-20.7225805863163,-19.6781103578147,-14.0426552896606));
#70826=CARTESIAN_POINT('',(-20.7225805821191,-19.6781103693095,-14.2664527148047));
#70827=CARTESIAN_POINT('',(-20.7225805821191,-19.6781103693095,0.));
#70828=CARTESIAN_POINT('',(-20.8484261850221,-18.9515327934241,-14.3109440134296));
#70829=CARTESIAN_POINT('Ctrl Pts',(-20.7225805821191,-19.6781103693095,
-14.2664527148047));
#70830=CARTESIAN_POINT('Ctrl Pts',(-20.7483493346654,-19.607538121474,-14.2709758300142));
#70831=CARTESIAN_POINT('Ctrl Pts',(-20.7703906773062,-19.5355010802264,
-14.2754989452236));
#70832=CARTESIAN_POINT('Ctrl Pts',(-20.788547932122,-19.4624133566172,-14.2800220604331));
#70833=CARTESIAN_POINT('Ctrl Pts',(-20.806681898482,-19.3894193751646,-14.2845393743048));
#70834=CARTESIAN_POINT('Ctrl Pts',(-20.8209415735944,-19.3153778114031,
-14.2890566881764));
#70835=CARTESIAN_POINT('Ctrl Pts',(-20.8312196579543,-19.2407190785,-14.2935740020481));
#70836=CARTESIAN_POINT('Ctrl Pts',(-20.8414842436756,-19.166158398038,-14.2980853831422));
#70837=CARTESIAN_POINT('Ctrl Pts',(-20.847777586069,-19.0909825928347,-14.3025967642363));
#70838=CARTESIAN_POINT('Ctrl Pts',(-20.8500434700713,-19.0156320105649,
-14.3071081453305));
#70839=CARTESIAN_POINT('Ctrl Pts',(-20.850685621504,-18.994277658663,-14.3083866705462));
#70840=CARTESIAN_POINT('Ctrl Pts',(-20.851004622492,-18.9729093192271,-14.3096651957618));
#70841=CARTESIAN_POINT('Ctrl Pts',(-20.850999949394,-18.9515371115436,-14.3109437209775));
#70842=CARTESIAN_POINT('Ctrl Pts',(-20.8476070208165,-18.9515314190757,
-14.3109441065097));
#70843=CARTESIAN_POINT('Ctrl Pts',(-20.8482398705352,-18.6260442197703,
-14.3304466040445));
#70844=CARTESIAN_POINT('Ctrl Pts',(-20.6243346302329,-17.5938833017488,
-14.3923410371397));
#70845=CARTESIAN_POINT('Ctrl Pts',(-19.0148744663066,-16.4645435790994,
-14.4966274057954));
#70846=CARTESIAN_POINT('Ctrl Pts',(-16.7944748199427,-17.3694160408942,
-14.6238032124768));
#70847=CARTESIAN_POINT('Ctrl Pts',(-16.3534691457724,-19.7262110589277,
-14.7509790191583));
#70848=CARTESIAN_POINT('Ctrl Pts',(-18.0964527779473,-21.3727154833541,
-14.8781548258396));
#70849=CARTESIAN_POINT('Ctrl Pts',(-20.0208838098492,-20.8979083957969,
-14.9832889543559));
#70850=CARTESIAN_POINT('Ctrl Pts',(-20.6031709075902,-19.9961147240441,
-15.0460311473117));
#70851=CARTESIAN_POINT('Ctrl Pts',(-20.7193262595591,-19.6769292106295,
-15.0663814047069));
#70852=CARTESIAN_POINT('Ctrl Pts',(-20.7225805876025,-19.6781103542923,
-14.843838552956));
#70853=CARTESIAN_POINT('Ctrl Pts',(-20.7076429479187,-19.7190197010936,
-14.8409815753642));
#70854=CARTESIAN_POINT('Ctrl Pts',(-20.6914352889252,-19.7594890121212,
-14.8381415685881));
#70855=CARTESIAN_POINT('Ctrl Pts',(-20.6503533962779,-19.8535323811849,
-14.8315248819409));
#70856=CARTESIAN_POINT('Ctrl Pts',(-20.624479739026,-19.9065985147269,-14.8277783969357));
#70857=CARTESIAN_POINT('Ctrl Pts',(-20.5792836655683,-19.9902275033178,
-14.8218610376395));
#70858=CARTESIAN_POINT('Ctrl Pts',(-20.5613390236455,-20.0214954410477,
-14.8196452307213));
#70859=CARTESIAN_POINT('Ctrl Pts',(-20.5368846514892,-20.0616923074862,
-14.8167904057333));
#70860=CARTESIAN_POINT('Ctrl Pts',(-20.5310922292495,-20.071048529154,-14.8161254489431));
#70861=CARTESIAN_POINT('Ctrl Pts',(-20.5215274852216,-20.0862321927493,
-14.8150454412858));
#70862=CARTESIAN_POINT('Ctrl Pts',(-20.5177990428995,-20.092086906261,-14.8146287798552));
#70863=CARTESIAN_POINT('Ctrl Pts',(-20.5105556221584,-20.1033386128491,
-14.8138275671119));
#70864=CARTESIAN_POINT('Ctrl Pts',(-20.5070446818932,-20.1087381023746,
-14.8134428716056));
#70865=CARTESIAN_POINT('Ctrl Pts',(-20.4989237545119,-20.1211034658168,
-14.8125613564739));
#70866=CARTESIAN_POINT('Ctrl Pts',(-20.4942970518485,-20.128058274632,-14.8120651696503));
#70867=CARTESIAN_POINT('Ctrl Pts',(-20.4818391206991,-20.1465466725458,
-14.8107449666183));
#70868=CARTESIAN_POINT('Ctrl Pts',(-20.4739348442708,-20.1580307194631,
-14.8099237119911));
#70869=CARTESIAN_POINT('Ctrl Pts',(-20.4094818015417,-20.2497212487156,
-14.8033548184419));
#70870=CARTESIAN_POINT('Ctrl Pts',(-20.3475282622321,-20.3259904575298,
-14.7978251132188));
#70871=CARTESIAN_POINT('Ctrl Pts',(-20.1871027224722,-20.4976021845072,
-14.7848692884694));
#70872=CARTESIAN_POINT('Ctrl Pts',(-20.0842495616095,-20.5882204381158,
-14.7775931152199));
#70873=CARTESIAN_POINT('Ctrl Pts',(-19.9317575763164,-20.6983394739842,
-14.7671707328954));
#70874=CARTESIAN_POINT('Ctrl Pts',(-19.8890588089683,-20.7268699132003,
-14.76428429342));
#70875=CARTESIAN_POINT('Ctrl Pts',(-19.8300417414095,-20.7632718679851,
-14.760278081994));
#70876=CARTESIAN_POINT('Ctrl Pts',(-19.8145955360426,-20.7725291874119,
-14.7592280529012));
#70877=CARTESIAN_POINT('Ctrl Pts',(-19.7915638375836,-20.7859363225787,
-14.7576572942295));
#70878=CARTESIAN_POINT('Ctrl Pts',(-19.7840676019868,-20.7902387580534,
-14.7571452683562));
#70879=CARTESIAN_POINT('Ctrl Pts',(-19.7704475716356,-20.7979454269309,
-14.7562131580613));
#70880=CARTESIAN_POINT('Ctrl Pts',(-19.7643327808252,-20.801365416998,-14.7557940299349));
#70881=CARTESIAN_POINT('Ctrl Pts',(-19.7546715390116,-20.8067061425825,
-14.7551306118184));
#70882=CARTESIAN_POINT('Ctrl Pts',(-19.7511363194201,-20.8086472397777,
-14.7548876027571));
#70883=CARTESIAN_POINT('Ctrl Pts',(-19.7475865136736,-20.8105831645117,
-14.7546433163214));
#70884=CARTESIAN_POINT('Ctrl Pts',(-19.747577419482,-20.8105881240403,-14.754642690486));
#70885=CARTESIAN_POINT('Ctrl Pts',(-19.7475591760445,-20.8105980729476,
-14.7546414350229));
#70886=CARTESIAN_POINT('Ctrl Pts',(-19.7475500259468,-20.8106030627899,
-14.7546408053366));
#70887=CARTESIAN_POINT('Ctrl Pts',(-19.7475316696383,-20.8106130728987,
-14.7546395420987));
#70888=CARTESIAN_POINT('Ctrl Pts',(-19.7475224644028,-20.8106180926325,
-14.7546389086143));
#70889=CARTESIAN_POINT('Ctrl Pts',(-19.7475039978208,-20.81062816252,-14.7546376377802));
#70890=CARTESIAN_POINT('Ctrl Pts',(-19.7474947359349,-20.8106332129669,
-14.7546370003935));
#70891=CARTESIAN_POINT('Ctrl Pts',(-19.7474761561388,-20.8106433442301,
-14.7546357217607));
#70892=CARTESIAN_POINT('Ctrl Pts',(-19.7474668377156,-20.8106484253251,
-14.7546350804794));
#70893=CARTESIAN_POINT('Ctrl Pts',(-19.7474481437399,-20.8106586184838,
-14.7546337939814));
#70894=CARTESIAN_POINT('Ctrl Pts',(-19.7474387687128,-20.81066373026,-14.7546331488008));
#70895=CARTESIAN_POINT('Ctrl Pts',(-19.7474199615284,-20.8106739847782,
-14.7546318545042));
#70896=CARTESIAN_POINT('Ctrl Pts',(-19.7474105287671,-20.8106791278484,
-14.7546312053465));
#70897=CARTESIAN_POINT('Ctrl Pts',(-19.7473916056544,-20.8106894452022,
-14.754629903064));
#70898=CARTESIAN_POINT('Ctrl Pts',(-19.7473821153389,-20.810694619465,-14.7546292499416));
#70899=CARTESIAN_POINT('Ctrl Pts',(-19.7473630763891,-20.8107049995977,
-14.7546279396793));
#70900=CARTESIAN_POINT('Ctrl Pts',(-19.7473535279432,-20.8107102053638,
-14.7546272825524));
#70901=CARTESIAN_POINT('Ctrl Pts',(-19.7473343726346,-20.8107206485529,
-14.7546259642743));
#70902=CARTESIAN_POINT('Ctrl Pts',(-19.7473247654062,-20.8107258861743,
-14.7546253030979));
#70903=CARTESIAN_POINT('Ctrl Pts',(-19.7473054912954,-20.8107363937449,
-14.7546239766356));
#70904=CARTESIAN_POINT('Ctrl Pts',(-19.7472958255505,-20.8107416630729,
-14.7546233114281));
#70905=CARTESIAN_POINT('Ctrl Pts',(-19.7472764350954,-20.810752233678,-14.7546219769507));
#70906=CARTESIAN_POINT('Ctrl Pts',(-19.7472667091036,-20.8107575356526,
-14.7546213075927));
#70907=CARTESIAN_POINT('Ctrl Pts',(-19.7472472344797,-20.8107681517453,
-14.7546199673145));
#70908=CARTESIAN_POINT('Ctrl Pts',(-19.7472374305908,-20.8107734959849,
-14.7546192925911));
#70909=CARTESIAN_POINT('Ctrl Pts',(-19.7472177802483,-20.8107842074636,
-14.7546179402112));
#70910=CARTESIAN_POINT('Ctrl Pts',(-19.7472079349286,-20.8107895740844,
-14.7546172626324));
#70911=CARTESIAN_POINT('Ctrl Pts',(-19.7471881820861,-20.8108003410291,
-14.7546159031897));
#70912=CARTESIAN_POINT('Ctrl Pts',(-19.7471782761647,-20.8108057404787,
-14.7546152214359));
#70913=CARTESIAN_POINT('Ctrl Pts',(-19.7471583681398,-20.8108165915978,
-14.7546138513045));
#70914=CARTESIAN_POINT('Ctrl Pts',(-19.7471484177377,-20.8108220150849,
-14.7546131664853));
#70915=CARTESIAN_POINT('Ctrl Pts',(-19.7441389748456,-20.8124622869553,
-14.7544060460706));
#70916=CARTESIAN_POINT('Ctrl Pts',(-19.7411355938517,-20.8140898379721,
-14.7541991424452));
#70917=CARTESIAN_POINT('Ctrl Pts',(-19.7340941498551,-20.8178836217641,
-14.753713597222));
#70918=CARTESIAN_POINT('Ctrl Pts',(-19.7300529967498,-20.820044010535,-14.7534345892217));
#70919=CARTESIAN_POINT('Ctrl Pts',(-19.717608152335,-20.8266451251454,-14.7525743807906));
#70920=CARTESIAN_POINT('Ctrl Pts',(-19.7091816775884,-20.8310423173854,
-14.7519905381892));
#70921=CARTESIAN_POINT('Ctrl Pts',(-19.5939549276201,-20.890187340136,-14.7439909203515));
#70922=CARTESIAN_POINT('Ctrl Pts',(-19.4827287343374,-20.9358072622843,
-14.736094938836));
#70923=CARTESIAN_POINT('Ctrl Pts',(-19.2644117655886,-21.0043641695455,
-14.7209775300448));
#70924=CARTESIAN_POINT('Ctrl Pts',(-19.1582022660974,-21.0289186894102,
-14.7137839202715));
#70925=CARTESIAN_POINT('Ctrl Pts',(-18.9765737644231,-21.0563876931189,
-14.7019827741361));
#70926=CARTESIAN_POINT('Ctrl Pts',(-18.9020306614998,-21.0636480343663,
-14.6972748127376));
#70927=CARTESIAN_POINT('Ctrl Pts',(-18.8084892403596,-21.0677724540655,
-14.6915390227631));
#70928=CARTESIAN_POINT('Ctrl Pts',(-18.7897158813092,-21.0683500420688,
-14.6903963324862));
#70929=CARTESIAN_POINT('Ctrl Pts',(-18.7623887108473,-21.0688269116208,
-14.6887448553477));
#70930=CARTESIAN_POINT('Ctrl Pts',(-18.7538396662056,-21.0689242980466,
-14.6882298932722));
#70931=CARTESIAN_POINT('Ctrl Pts',(-18.7388418088678,-21.0690042842168,
-14.6873293712608));
#70932=CARTESIAN_POINT('Ctrl Pts',(-18.7323932727385,-21.0690092116853,
-14.6869431170728));
#70933=CARTESIAN_POINT('Ctrl Pts',(-18.7198657866567,-21.0689615439237,
-14.6861945317473));
#70934=CARTESIAN_POINT('Ctrl Pts',(-18.7137868941591,-21.0689122291623,
-14.6858321017005));
#70935=CARTESIAN_POINT('Ctrl Pts',(-18.6992460283344,-21.0687316272221,
-14.6849670727568));
#70936=CARTESIAN_POINT('Ctrl Pts',(-18.6907844222653,-21.0685757811215,
-14.684465246086));
#70937=CARTESIAN_POINT('Ctrl Pts',(-18.6601984170295,-21.0678289520878,
-14.682656722482));
#70938=CARTESIAN_POINT('Ctrl Pts',(-18.6380821998677,-21.0669417623734,
-14.6813592826769));
#70939=CARTESIAN_POINT('Ctrl Pts',(-18.4309232207095,-21.0553752570998,
-14.669292435323));
#70940=CARTESIAN_POINT('Ctrl Pts',(-18.2480265114241,-21.0207867967459,
-14.6593770169785));
#70941=CARTESIAN_POINT('Ctrl Pts',(-17.995689099154,-20.937707355755,-14.6448953879912));
#70942=CARTESIAN_POINT('Ctrl Pts',(-17.9209152180251,-20.9082790729295,
-14.6404800235867));
#70943=CARTESIAN_POINT('Ctrl Pts',(-17.8152387635287,-20.8595817102325,
-14.6338245873714));
#70944=CARTESIAN_POINT('Ctrl Pts',(-17.7828712094407,-20.8436510949149,
-14.6317264791834));
#70945=CARTESIAN_POINT('Ctrl Pts',(-17.7443139683167,-20.8234343005845,
-14.6291356243559));
#70946=CARTESIAN_POINT('Ctrl Pts',(-17.7377178184286,-20.8199310998068,
-14.6286891004227));
#70947=CARTESIAN_POINT('Ctrl Pts',(-17.7274769485285,-20.8144225222623,
-14.6279904878432));
#70948=CARTESIAN_POINT('Ctrl Pts',(-17.723819293524,-20.8124411423512,-14.6277398984237));
#70949=CARTESIAN_POINT('Ctrl Pts',(-17.7170371875418,-20.8087413264565,
-14.6272732129449));
#70950=CARTESIAN_POINT('Ctrl Pts',(-17.7139112298574,-20.8070257722518,
-14.6270573006711));
#70951=CARTESIAN_POINT('Ctrl Pts',(-17.7068415732848,-20.803122606612,-14.6265671603556));
#70952=CARTESIAN_POINT('Ctrl Pts',(-17.7029005414877,-20.8009302972441,
-14.6262926350412));
#70953=CARTESIAN_POINT('Ctrl Pts',(-17.6927437972028,-20.7952377511309,
-14.6255818503118));
#70954=CARTESIAN_POINT('Ctrl Pts',(-17.6865387758885,-20.7917186925543,
-14.6251444250928));
#70955=CARTESIAN_POINT('Ctrl Pts',(-17.6485596117781,-20.7699251144456,
-14.6224480069914));
#70956=CARTESIAN_POINT('Ctrl Pts',(-17.6172487745305,-20.75086044076,-14.6201428557126));
#70957=CARTESIAN_POINT('Ctrl Pts',(-17.4431944831213,-20.6385858369582,
-14.6069248159007));
#70958=CARTESIAN_POINT('Ctrl Pts',(-17.3116252437888,-20.5292139370732,
-14.5954219872646));
#70959=CARTESIAN_POINT('Ctrl Pts',(-17.1290835939153,-20.3358495552604,
-14.5781406462631));
#70960=CARTESIAN_POINT('Ctrl Pts',(-17.0683335952191,-20.2620976862588,
-14.5720772490551));
#70961=CARTESIAN_POINT('Ctrl Pts',(-17.0003042799481,-20.1670909392671,
-14.5648995399914));
#70962=CARTESIAN_POINT('Ctrl Pts',(-16.9881112547638,-20.149505483256,-14.5635952934218));
#70963=CARTESIAN_POINT('Ctrl Pts',(-16.9711651700848,-20.1242557553682,
-14.5617562256899));
#70964=CARTESIAN_POINT('Ctrl Pts',(-16.9661915242067,-20.116741769833,-14.5612130911202));
#70965=CARTESIAN_POINT('Ctrl Pts',(-16.957698413396,-20.1037309880657,-14.5602796770699));
#70966=CARTESIAN_POINT('Ctrl Pts',(-16.9541561443926,-20.0982492951273,
-14.5598885463533));
#70967=CARTESIAN_POINT('Ctrl Pts',(-16.9474252612597,-20.0877267621261,
-14.559141777503));
#70968=CARTESIAN_POINT('Ctrl Pts',(-16.9442324952682,-20.0826886642404,
-14.5587859873076));
#70969=CARTESIAN_POINT('Ctrl Pts',(-16.9359919718277,-20.0695629814295,
-14.5578635619645));
#70970=CARTESIAN_POINT('Ctrl Pts',(-16.9309774411911,-20.0614546154661,
-14.5572981579801));
#70971=CARTESIAN_POINT('Ctrl Pts',(-16.9140973996719,-20.0337433043207,
-14.5553805635421));
#70972=CARTESIAN_POINT('Ctrl Pts',(-16.9024951897436,-20.0139812811232,
-14.554037989369));
#70973=CARTESIAN_POINT('Ctrl Pts',(-16.8043356504924,-19.840391151968,-14.5424490358628));
#70974=CARTESIAN_POINT('Ctrl Pts',(-16.7370108230236,-19.6764889356372,
-14.5329638207747));
#70975=CARTESIAN_POINT('Ctrl Pts',(-16.6682205241966,-19.4228393271697,
-14.5186615910465));
#70976=CARTESIAN_POINT('Ctrl Pts',(-16.6507495062445,-19.3382635647562,
-14.5139355675406));
#70977=CARTESIAN_POINT('Ctrl Pts',(-16.6331388704248,-19.2156064655233,
-14.5068593859828));
#70978=CARTESIAN_POINT('Ctrl Pts',(-16.6287843998222,-19.1782139193902,
-14.5046726174139));
#70979=CARTESIAN_POINT('Ctrl Pts',(-16.6247551286356,-19.1331967041538,
-14.5019834456781));
#70980=CARTESIAN_POINT('Ctrl Pts',(-16.6241214149201,-19.1256621008888,
-14.5015314594217));
#70981=CARTESIAN_POINT('Ctrl Pts',(-16.6232000776199,-19.113957278688,-14.500826145076));
#70982=CARTESIAN_POINT('Ctrl Pts',(-16.6228844118202,-19.1097892426324,
-14.5005743630948));
#70983=CARTESIAN_POINT('Ctrl Pts',(-16.6223224748363,-19.1020657577902,
-14.5001066060134));
#70984=CARTESIAN_POINT('Ctrl Pts',(-16.6220728369585,-19.0985106117853,
-14.4998908219755));
#70985=CARTESIAN_POINT('Ctrl Pts',(-16.621529449458,-19.0904820237861,-14.4994024513685));
#70986=CARTESIAN_POINT('Ctrl Pts',(-16.6212409332976,-19.0860082946337,
-14.499129576732));
#70987=CARTESIAN_POINT('Ctrl Pts',(-16.6204331128662,-19.0728306341277,
-14.4983236884368));
#70988=CARTESIAN_POINT('Ctrl Pts',(-16.6199533779791,-19.0641244953032,
-14.4977885384742));
#70989=CARTESIAN_POINT('Ctrl Pts',(-16.6169217648312,-19.0021391715391,
-14.4939602514148));
#70990=CARTESIAN_POINT('Ctrl Pts',(-16.6163308011492,-18.948787721568,-14.4905700676359));
#70991=CARTESIAN_POINT('Ctrl Pts',(-16.6182284094208,-18.8777415637757,
-14.4859767988122));
#70992=CARTESIAN_POINT('Ctrl Pts',(-16.6189249917261,-18.8600140040091,
-14.4848241015923));
#70993=CARTESIAN_POINT('Ctrl Pts',(-16.6223516703974,-18.7939759227892,
-14.480510044686));
#70994=CARTESIAN_POINT('Ctrl Pts',(-16.6265149429976,-18.7457555444233,
-14.4773202259516));
#70995=CARTESIAN_POINT('Ctrl Pts',(-16.6454646084781,-18.5891319441843,
-14.4668986555548));
#70996=CARTESIAN_POINT('Ctrl Pts',(-16.6669999515267,-18.4817154340415,
-14.4596659525143));
#70997=CARTESIAN_POINT('Ctrl Pts',(-16.7117227611718,-18.323414473137,-14.4490925059294));
#70998=CARTESIAN_POINT('Ctrl Pts',(-16.7287683875275,-18.2709919261779,
-14.445603384554));
#70999=CARTESIAN_POINT('Ctrl Pts',(-16.7597139762447,-18.1871075927867,
-14.4400458367904));
#71000=CARTESIAN_POINT('Ctrl Pts',(-16.7723674786205,-18.1552166131295,
-14.4379389720323));
#71001=CARTESIAN_POINT('Ctrl Pts',(-16.7900202330708,-18.113699047025,-14.4352024444129));
#71002=CARTESIAN_POINT('Ctrl Pts',(-16.7943255990543,-18.1037847872798,
-14.434549440251));
#71003=CARTESIAN_POINT('Ctrl Pts',(-16.8015027788911,-18.0875978523182,
-14.4334839409556));
#71004=CARTESIAN_POINT('Ctrl Pts',(-16.8043296188266,-18.0813055620455,
-14.4330699163808));
#71005=CARTESIAN_POINT('Ctrl Pts',(-16.8098619102645,-18.0691504652003,
-14.4322704012817));
#71006=CARTESIAN_POINT('Ctrl Pts',(-16.8125635249759,-18.0632860058831,
-14.4318847844145));
#71007=CARTESIAN_POINT('Ctrl Pts',(-16.8188645674854,-18.0497712285782,
-14.4309963640559));
#71008=CARTESIAN_POINT('Ctrl Pts',(-16.822483094604,-18.0421298969617,-14.4304942266299));
#71009=CARTESIAN_POINT('Ctrl Pts',(-16.8323404074004,-18.021632335304,-14.4291476168919));
#71010=CARTESIAN_POINT('Ctrl Pts',(-16.8386638134609,-18.0088171160672,
-14.4283060859858));
#71011=CARTESIAN_POINT('Ctrl Pts',(-16.8978737344223,-17.8918208441485,
-14.420624308031));
#71012=CARTESIAN_POINT('Ctrl Pts',(-16.9591729457351,-17.7921147917786,
-14.4141007390592));
#71013=CARTESIAN_POINT('Ctrl Pts',(-17.1248209892401,-17.5668178426426,
-14.3987920341743));
#71014=CARTESIAN_POINT('Ctrl Pts',(-17.2360388736691,-17.4472451057684,
-14.3901900912923));
#71015=CARTESIAN_POINT('Ctrl Pts',(-17.3845340351765,-17.3205329979835,
-14.3789809299058));
#71016=CARTESIAN_POINT('Ctrl Pts',(-17.4097099205386,-17.300031933106,-14.3770873619667));
#71017=CARTESIAN_POINT('Ctrl Pts',(-17.4410606641621,-17.2756798507381,
-14.3747237190424));
#71018=CARTESIAN_POINT('Ctrl Pts',(-17.4467983648085,-17.2712700050573,
-14.3742909078512));
#71019=CARTESIAN_POINT('Ctrl Pts',(-17.4558292253301,-17.2644024902162,
-14.3736091340303));
#71020=CARTESIAN_POINT('Ctrl Pts',(-17.4591071853729,-17.2619247961109,
-14.3733615557264));
#71021=CARTESIAN_POINT('Ctrl Pts',(-17.4652481537575,-17.2573110869204,
-14.3728974863215));
#71022=CARTESIAN_POINT('Ctrl Pts',(-17.4681093618142,-17.2551727692675,
-14.3726811603458));
#71023=CARTESIAN_POINT('Ctrl Pts',(-17.4746535600816,-17.250307741221,-14.3721861433191));
#71024=CARTESIAN_POINT('Ctrl Pts',(-17.4783399877556,-17.2475857510388,
-14.3719071300551));
#71025=CARTESIAN_POINT('Ctrl Pts',(-17.4897001517645,-17.2392544735096,
-14.3710468896221));
#71026=CARTESIAN_POINT('Ctrl Pts',(-17.4974027291289,-17.2336849727822,
-14.370463020003));
#71027=CARTESIAN_POINT('Ctrl Pts',(-17.6025137244998,-17.1587551529989,
-14.3624902741026));
#71028=CARTESIAN_POINT('Ctrl Pts',(-17.7055802435141,-17.0977253590708,
-14.3546245546615));
#71029=CARTESIAN_POINT('Ctrl Pts',(-17.9113747828314,-16.9983224336356,
-14.339526361252));
#71030=CARTESIAN_POINT('Ctrl Pts',(-18.0130398286374,-16.9585637235131,
-14.3323218107826));
#71031=CARTESIAN_POINT('Ctrl Pts',(-18.1891373989897,-16.9049412180369,
-14.3204940671805));
#71032=CARTESIAN_POINT('Ctrl Pts',(-18.2620726832091,-16.8869063779302,
-14.3157707365048));
#71033=CARTESIAN_POINT('Ctrl Pts',(-18.3542966735888,-16.8692450197401,
-14.3100183580194));
#71034=CARTESIAN_POINT('Ctrl Pts',(-18.3728205672688,-16.8659529302716,
-14.3088736998168));
#71035=CARTESIAN_POINT('Ctrl Pts',(-18.399828877072,-16.8615235342935,-14.307219920537));
#71036=CARTESIAN_POINT('Ctrl Pts',(-18.408279799198,-16.8601901264174,-14.3067046000093));
#71037=CARTESIAN_POINT('Ctrl Pts',(-18.4231151909209,-16.8579414455019,
-14.3058036645836));
#71038=CARTESIAN_POINT('Ctrl Pts',(-18.4294961488017,-16.8570040572316,
-14.3054173534682));
#71039=CARTESIAN_POINT('Ctrl Pts',(-18.4418980674715,-16.8552400246184,
-14.3046688127312));
#71040=CARTESIAN_POINT('Ctrl Pts',(-18.447918493792,-16.854410119604,-14.304306483472));
#71041=CARTESIAN_POINT('Ctrl Pts',(-18.4623244409392,-16.8524874614138,
-14.3034419416742));
#71042=CARTESIAN_POINT('Ctrl Pts',(-18.4707131409848,-16.8514189989209,
-14.3029404993663));
#71043=CARTESIAN_POINT('Ctrl Pts',(-18.5010374778185,-16.8477411199299,
-14.3011348233368));
#71044=CARTESIAN_POINT('Ctrl Pts',(-18.5230077067905,-16.8454247515293,
-14.2998398081182));
#71045=CARTESIAN_POINT('Ctrl Pts',(-18.730035253459,-16.8268688625312,-14.2877505853426));
#71046=CARTESIAN_POINT('Ctrl Pts',(-18.9164320929422,-16.8347086643427,
-14.2778149365771));
#71047=CARTESIAN_POINT('Ctrl Pts',(-19.2070661066051,-16.8856409444278,
-14.2617291744951));
#71048=CARTESIAN_POINT('Ctrl Pts',(-19.3130705856861,-16.912808455566,-14.2557044382252));
#71049=CARTESIAN_POINT('Ctrl Pts',(-19.4276556103934,-16.9518324946911,
-14.2485598568095));
#71050=CARTESIAN_POINT('Ctrl Pts',(-19.4387899194704,-16.9557286481411,
-14.2478587436266));
#71051=CARTESIAN_POINT('Ctrl Pts',(-19.4545994881612,-16.961409531765,-14.2468526484539));
#71052=CARTESIAN_POINT('Ctrl Pts',(-19.4593021097837,-16.9631181827622,
-14.2465520397536));
#71053=CARTESIAN_POINT('Ctrl Pts',(-19.4674061321594,-16.9660952631742,
-14.246031611518));
#71054=CARTESIAN_POINT('Ctrl Pts',(-19.4708104437233,-16.967355813172,-14.2458122610237));
#71055=CARTESIAN_POINT('Ctrl Pts',(-19.4774130277556,-16.9698199507624,
-14.2453853894602));
#71056=CARTESIAN_POINT('Ctrl Pts',(-19.4806116341742,-16.9710225279514,
-14.2451779346909));
#71057=CARTESIAN_POINT('Ctrl Pts',(-19.4892513653539,-16.9742946972862,
-14.244615827639));
#71058=CARTESIAN_POINT('Ctrl Pts',(-19.4946868407137,-16.9763789792127,
-14.2442603087065));
#71059=CARTESIAN_POINT('Ctrl Pts',(-19.5149313737947,-16.9842378586961,
-14.2429293226987));
#71060=CARTESIAN_POINT('Ctrl Pts',(-19.5296834171476,-16.9901566014415,
-14.241945734812));
#71061=CARTESIAN_POINT('Ctrl Pts',(-19.6585784742384,-17.0435641384826,
-14.233239633167));
#71062=CARTESIAN_POINT('Ctrl Pts',(-19.7684144681814,-17.1007966705077,
-14.2250589751229));
#71063=CARTESIAN_POINT('Ctrl Pts',(-20.0135263506943,-17.257173239253,-14.2058458527477));
#71064=CARTESIAN_POINT('Ctrl Pts',(-20.1433194170827,-17.3634582104785,
-14.1949293140074));
#71065=CARTESIAN_POINT('Ctrl Pts',(-20.2740377312084,-17.4992693764024,
-14.1833517784933));
#71066=CARTESIAN_POINT('Ctrl Pts',(-20.2885732311655,-17.5148345261482,
-14.1820538490488));
#71067=CARTESIAN_POINT('Ctrl Pts',(-20.3089101667041,-17.5372817067615,
-14.1802220646807));
#71068=CARTESIAN_POINT('Ctrl Pts',(-20.3149060430827,-17.5439850962232,
-14.1796799855965));
#71069=CARTESIAN_POINT('Ctrl Pts',(-20.3251770134136,-17.5556163612925,
-14.1787478162585));
#71070=CARTESIAN_POINT('Ctrl Pts',(-20.3294723460919,-17.5605261235653,
-14.1783568807515));
#71071=CARTESIAN_POINT('Ctrl Pts',(-20.3376538017579,-17.5699655929414,
-14.1776100974022));
#71072=CARTESIAN_POINT('Ctrl Pts',(-20.3415435918228,-17.5744920255406,
-14.1772540993608));
#71073=CARTESIAN_POINT('Ctrl Pts',(-20.3516099347434,-17.5863066360621,
-14.1763302980565));
#71074=CARTESIAN_POINT('Ctrl Pts',(-20.3577564321546,-17.5936203333132,
-14.1757637333954));
#71075=CARTESIAN_POINT('Ctrl Pts',(-20.3785534966147,-17.6187095625501,
-14.1738379040102));
#71076=CARTESIAN_POINT('Ctrl Pts',(-20.3929636857117,-17.6366828730015,
-14.1724883699118));
#71077=CARTESIAN_POINT('Ctrl Pts',(-20.514233751194,-17.793102936346,-14.1609878425405));
#71078=CARTESIAN_POINT('Ctrl Pts',(-20.6038500179196,-17.9440603936927,
-14.1515818059434));
#71079=CARTESIAN_POINT('Ctrl Pts',(-20.7088874074614,-18.184438461638,-14.1373097847421));
#71080=CARTESIAN_POINT('Ctrl Pts',(-20.7388925673333,-18.266628304272,-14.1325252852108));
#71081=CARTESIAN_POINT('Ctrl Pts',(-20.7745072694397,-18.386794187366,-14.1253702554482));
#71082=CARTESIAN_POINT('Ctrl Pts',(-20.7843049887495,-18.4234391443809,
-14.1231673023282));
#71083=CARTESIAN_POINT('Ctrl Pts',(-20.7948724745932,-18.4676952770427,
-14.1204601917538));
#71084=CARTESIAN_POINT('Ctrl Pts',(-20.7965927813452,-18.4750750209694,
-14.1200072372706));
#71085=CARTESIAN_POINT('Ctrl Pts',(-20.7992012880941,-18.4865430826915,
-14.1193007353718));
#71086=CARTESIAN_POINT('Ctrl Pts',(-20.8001170709358,-18.4906251516301,
-14.1190487424404));
#71087=CARTESIAN_POINT('Ctrl Pts',(-20.8017905239888,-18.4981894131817,
-14.118580793867));
#71088=CARTESIAN_POINT('Ctrl Pts',(-20.8025515038072,-18.5016708144893,
-14.1183650305685));
#71089=CARTESIAN_POINT('Ctrl Pts',(-20.8042489774775,-18.5095316647612,
-14.1178769641879));
#71090=CARTESIAN_POINT('Ctrl Pts',(-20.8051803614632,-18.5139121482261,
-14.1176043746306));
#71091=CARTESIAN_POINT('Ctrl Pts',(-20.807879766717,-18.5268090212333,-14.1168000903592));
#71092=CARTESIAN_POINT('Ctrl Pts',(-20.8096091841019,-18.5353332696965,
-14.1162662717741));
#71093=CARTESIAN_POINT('Ctrl Pts',(-20.8214936687642,-18.5958221781559,
-14.1124636819955));
#71094=CARTESIAN_POINT('Ctrl Pts',(-20.8297477350103,-18.6481367524029,
-14.1090992703783));
#71095=CARTESIAN_POINT('Ctrl Pts',(-20.8378088424033,-18.7155650890805,
-14.1047115704625));
#71096=CARTESIAN_POINT('Ctrl Pts',(-20.8394281570205,-18.7304478102423,
-14.1037399102944));
#71097=CARTESIAN_POINT('Ctrl Pts',(-20.8475637385171,-18.8133921847226,
-14.0983108221101));
#71098=CARTESIAN_POINT('Ctrl Pts',(-20.8509374103365,-18.8817197469213,
-14.0937882210587));
#71099=CARTESIAN_POINT('Ctrl Pts',(-20.8511442882195,-19.1108585921172,
-14.0786472789942));
#71100=CARTESIAN_POINT('Ctrl Pts',(-20.8329752262487,-19.2711508341196,
-14.0681492786479));
#71101=CARTESIAN_POINT('Ctrl Pts',(-20.7914795956747,-19.4510311537672,
-14.0567777760979));
#71102=CARTESIAN_POINT('Ctrl Pts',(-20.7857446847916,-19.4741093753488,
-14.0553254965786));
#71103=CARTESIAN_POINT('Ctrl Pts',(-20.7771304022459,-19.5064373723262,
-14.0532997977465));
#71104=CARTESIAN_POINT('Ctrl Pts',(-20.7745746985153,-19.515770826717,-14.0527159749718));
#71105=CARTESIAN_POINT('Ctrl Pts',(-20.7703333351151,-19.5308535536535,
-14.0517740932618));
#71106=CARTESIAN_POINT('Ctrl Pts',(-20.7686871312255,-19.5366136907826,
-14.0514147574334));
#71107=CARTESIAN_POINT('Ctrl Pts',(-20.7652024824747,-19.5486136004151,
-14.0506669103238));
#71108=CARTESIAN_POINT('Ctrl Pts',(-20.7633596820565,-19.5548520509312,
-14.0502785455249));
#71109=CARTESIAN_POINT('Ctrl Pts',(-20.7589304689817,-19.5695958416376,
-14.049361646217));
#71110=CARTESIAN_POINT('Ctrl Pts',(-20.7563191655654,-19.5780936224545,
-14.04883393154));
#71111=CARTESIAN_POINT('Ctrl Pts',(-20.7474528210905,-19.6063124414062,
-14.0470838497248));
#71112=CARTESIAN_POINT('Ctrl Pts',(-20.7409621030242,-19.6259586007358,
-14.0458692188294));
#71113=CARTESIAN_POINT('Ctrl Pts',(-20.7304048632613,-19.6564073564964,
-14.0439912770295));
#71114=CARTESIAN_POINT('Ctrl Pts',(-20.7265368266077,-19.6672754997887,
-14.0433218908956));
#71115=CARTESIAN_POINT('Ctrl Pts',(-20.7225805863163,-19.6781103578147,
-14.0426552896606));
#71116=CARTESIAN_POINT('Origin',(-18.734,-18.952,0.));
#71117=CARTESIAN_POINT('',(-20.7225805821191,-19.6781103693095,-13.2445592932782));
#71118=CARTESIAN_POINT('',(-20.7225805467356,-19.6781104662135,-13.4647889080502));
#71119=CARTESIAN_POINT('',(-20.7225805821191,-19.6781103693095,0.));
#71120=CARTESIAN_POINT('',(-20.8509991049198,-18.9539467328106,-13.5109437209775));
#71121=CARTESIAN_POINT('Ctrl Pts',(-20.7225805467356,-19.6781104662135,
-13.4647889080502));
#71122=CARTESIAN_POINT('Ctrl Pts',(-20.7382333305348,-19.635242579282,-13.4673503188061));
#71123=CARTESIAN_POINT('Ctrl Pts',(-20.7525027461134,-19.5918609102248,
-13.4699563619004));
#71124=CARTESIAN_POINT('Ctrl Pts',(-20.7697993275094,-19.5329117107744,
-13.4735579793603));
#71125=CARTESIAN_POINT('Ctrl Pts',(-20.7740668395333,-19.517742498761,-13.4744900743866));
#71126=CARTESIAN_POINT('Ctrl Pts',(-20.7796729213208,-19.4969265508334,
-13.4757781494082));
#71127=CARTESIAN_POINT('Ctrl Pts',(-20.7811583223091,-19.491319430789,-13.4761260033414));
#71128=CARTESIAN_POINT('Ctrl Pts',(-20.7834811071016,-19.4824034700739,
-13.476680645354));
#71129=CARTESIAN_POINT('Ctrl Pts',(-20.784333577585,-19.47909853887,-13.4768865675407));
#71130=CARTESIAN_POINT('Ctrl Pts',(-20.7860768719228,-19.4722717643364,
-13.4773126348401));
#71131=CARTESIAN_POINT('Ctrl Pts',(-20.7869666213465,-19.4687496956009,
-13.4775328428254));
#71132=CARTESIAN_POINT('Ctrl Pts',(-20.7890638347801,-19.4603569773869,
-13.4780584825616));
#71133=CARTESIAN_POINT('Ctrl Pts',(-20.7902630507495,-19.4554843060228,
-13.4783643854935));
#71134=CARTESIAN_POINT('Ctrl Pts',(-20.7927674028288,-19.4451503926449,
-13.4790146089627));
#71135=CARTESIAN_POINT('Ctrl Pts',(-20.7940681555771,-19.4396881395806,
-13.4793591675701));
#71136=CARTESIAN_POINT('Ctrl Pts',(-20.7975804740569,-19.424674048574,-13.4803085100425));
#71137=CARTESIAN_POINT('Ctrl Pts',(-20.7997474072569,-19.4151120495648,
-13.4809156168293));
#71138=CARTESIAN_POINT('Ctrl Pts',(-20.8343835369534,-19.2571922459627,
-13.4909794990141));
#71139=CARTESIAN_POINT('Ctrl Pts',(-20.8508585302458,-19.105796417632,-13.501135660806));
#71140=CARTESIAN_POINT('Ctrl Pts',(-20.850999092854,-18.9539598100794,-13.511142142957));
#71141=CARTESIAN_POINT('Ctrl Pts',(-20.8509991049198,-18.9539467328106,
-13.5109437209775));
#71142=CARTESIAN_POINT('Ctrl Pts',(-20.8510652701871,-18.8819944798437,
-13.5152699622426));
#71143=CARTESIAN_POINT('Ctrl Pts',(-20.84745892973,-18.8099473001284,-13.5195962035077));
#71144=CARTESIAN_POINT('Ctrl Pts',(-20.8401777557621,-18.7382144505981,
-13.5239224447729));
#71145=CARTESIAN_POINT('Ctrl Pts',(-20.8329012160598,-18.6665272570403,
-13.5282459325052));
#71146=CARTESIAN_POINT('Ctrl Pts',(-20.8219545300653,-18.59515448782,-13.5325694202375));
#71147=CARTESIAN_POINT('Ctrl Pts',(-20.8073873938027,-18.5245029646652,
-13.5368929079699));
#71148=CARTESIAN_POINT('Ctrl Pts',(-20.792824456527,-18.4538718068597,-13.541215149454));
#71149=CARTESIAN_POINT('Ctrl Pts',(-20.7746432396997,-18.3839619667449,
-13.545537390938));
#71150=CARTESIAN_POINT('Ctrl Pts',(-20.7529446959793,-18.3151708906015,
-13.5498596324221));
#71151=CARTESIAN_POINT('Ctrl Pts',(-20.7312448511874,-18.2463756896606,
-13.5541821330731));
#71152=CARTESIAN_POINT('Ctrl Pts',(-20.706027412668,-18.1786998565915,-13.5585046337241));
#71153=CARTESIAN_POINT('Ctrl Pts',(-20.67744287501,-18.1125246926962,-13.5628271343751));
#71154=CARTESIAN_POINT('Ctrl Pts',(-20.6488284904879,-18.0462804312647,
-13.5671541484134));
#71155=CARTESIAN_POINT('Ctrl Pts',(-20.6168401898347,-17.9815404195961,
-13.5714811624517));
#71156=CARTESIAN_POINT('Ctrl Pts',(-20.5816757716213,-17.9186640222254,
-13.57580817649));
#71157=CARTESIAN_POINT('Ctrl Pts',(-20.5464899011039,-17.8557492666601,
-13.5801378302541));
#71158=CARTESIAN_POINT('Ctrl Pts',(-20.5081243239348,-17.7947008039887,
-13.5844674840181));
#71159=CARTESIAN_POINT('Ctrl Pts',(-20.46682025899,-17.7358491252998,-13.5887971377822));
#71160=CARTESIAN_POINT('Ctrl Pts',(-20.4254474059601,-17.6768994346046,
-13.5931340021826));
#71161=CARTESIAN_POINT('Ctrl Pts',(-20.3811266092591,-17.6201542127691,
-13.597470866583));
#71162=CARTESIAN_POINT('Ctrl Pts',(-20.3341387764019,-17.5659102134945,
-13.6018077309834));
#71163=CARTESIAN_POINT('Ctrl Pts',(-20.3175654749946,-17.5467775552114,
-13.6033374069974));
#71164=CARTESIAN_POINT('Ctrl Pts',(-20.3006606978847,-17.5279557221356,
-13.6048670830114));
#71165=CARTESIAN_POINT('Ctrl Pts',(-20.2834377820478,-17.5094565657968,
-13.6063967590254));
#71166=CARTESIAN_POINT('Ctrl Pts',(-20.2340300954521,-17.4563877052551,
-13.6107849679563));
#71167=CARTESIAN_POINT('Ctrl Pts',(-20.1817963672775,-17.405756540934,-13.6151731768872));
#71168=CARTESIAN_POINT('Ctrl Pts',(-20.1270066890246,-17.3578791249304,
-13.6195613858181));
#71169=CARTESIAN_POINT('Ctrl Pts',(-20.0722983277386,-17.3100727669503,
-13.6239430819193));
#71170=CARTESIAN_POINT('Ctrl Pts',(-20.0150419071301,-17.2650123587827,
-13.6283247780206));
#71171=CARTESIAN_POINT('Ctrl Pts',(-19.9555455237308,-17.2229784462149,
-13.6327064741219));
#71172=CARTESIAN_POINT('Ctrl Pts',(-19.8961190533168,-17.1809939268396,
-13.6370830213815));
#71173=CARTESIAN_POINT('Ctrl Pts',(-19.8344582408823,-17.1420291152646,
-13.6414595686412));
#71174=CARTESIAN_POINT('Ctrl Pts',(-19.7709042257784,-17.1063243441593,
-13.6458361159008));
#71175=CARTESIAN_POINT('Ctrl Pts',(-19.7073905157072,-17.0706422165009,
-13.6502098876178));
#71176=CARTESIAN_POINT('Ctrl Pts',(-19.6419864047146,-17.0382162628698,
-13.6545836593348));
#71177=CARTESIAN_POINT('Ctrl Pts',(-19.5750607832521,-17.0092427431932,
-13.6589574310517));
#71178=CARTESIAN_POINT('Ctrl Pts',(-19.5081555274809,-16.980278040256,-13.6633298718153));
#71179=CARTESIAN_POINT('Ctrl Pts',(-19.4397301228477,-16.9547638770619,
-13.6677023125788));
#71180=CARTESIAN_POINT('Ctrl Pts',(-19.3701752330588,-16.9328491703583,
-13.6720747533424));
#71181=CARTESIAN_POINT('Ctrl Pts',(-19.3006185647437,-16.9109339032933,
-13.6764473059097));
#71182=CARTESIAN_POINT('Ctrl Pts',(-19.2299328146148,-16.8926184185036,
-13.6808198584771));
#71183=CARTESIAN_POINT('Ctrl Pts',(-19.1585240564096,-16.8780018501625,
-13.6851924110444));
#71184=CARTESIAN_POINT('Ctrl Pts',(-19.0870411875016,-16.8633701121954,
-13.6895695016118));
#71185=CARTESIAN_POINT('Ctrl Pts',(-19.0148342859533,-16.8524450521882,
-13.6939465921791));
#71186=CARTESIAN_POINT('Ctrl Pts',(-18.9423190546106,-16.8452745381787,
-13.6983236827464));
#71187=CARTESIAN_POINT('Ctrl Pts',(-18.8697642200086,-16.8381001080854,
-13.7027031638054));
#71188=CARTESIAN_POINT('Ctrl Pts',(-18.7969012025311,-16.8346843291133,
-13.7070826448643));
#71189=CARTESIAN_POINT('Ctrl Pts',(-18.7241475303631,-16.8350229267085,
-13.7114621259232));
#71190=CARTESIAN_POINT('Ctrl Pts',(-18.6512649027996,-16.8353621244656,
-13.715849369583));
#71191=CARTESIAN_POINT('Ctrl Pts',(-18.5784924896196,-16.839468960567,-13.7202366132427));
#71192=CARTESIAN_POINT('Ctrl Pts',(-18.5062439309009,-16.8472871518926,
-13.7246238569024));
#71193=CARTESIAN_POINT('Ctrl Pts',(-18.4571218728272,-16.8526027686348,
-13.7276067598372));
#71194=CARTESIAN_POINT('Ctrl Pts',(-18.4082418439352,-16.8596329436867,
-13.730589662772));
#71195=CARTESIAN_POINT('Ctrl Pts',(-18.3597305432932,-16.8683466282089,
-13.7335725657068));
#71196=CARTESIAN_POINT('Ctrl Pts',(-18.2883645862436,-16.8811655060194,
-13.7379607746377));
#71197=CARTESIAN_POINT('Ctrl Pts',(-18.217518663235,-16.8976801162965,-13.7423489835686));
#71198=CARTESIAN_POINT('Ctrl Pts',(-18.1476047194715,-16.9178344278368,
-13.7467371924995));
#71199=CARTESIAN_POINT('Ctrl Pts',(-18.0777945395923,-16.9379588270373,
-13.7511188886007));
#71200=CARTESIAN_POINT('Ctrl Pts',(-18.0089140527659,-16.9617120714412,
-13.755500584702));
#71201=CARTESIAN_POINT('Ctrl Pts',(-17.9413659204113,-16.9889869547365,
-13.7598822808033));
#71202=CARTESIAN_POINT('Ctrl Pts',(-17.873897162488,-17.0162297878734,-13.7642588280629));
#71203=CARTESIAN_POINT('Ctrl Pts',(-17.8077580939875,-17.0469858596163,
-13.7686353753226));
#71204=CARTESIAN_POINT('Ctrl Pts',(-17.7433354489119,-17.081098413273,-13.7730119225822));
#71205=CARTESIAN_POINT('Ctrl Pts',(-17.6789536597417,-17.115189333244,-13.7773856942992));
#71206=CARTESIAN_POINT('Ctrl Pts',(-17.6162865594632,-17.1526322864701,
-13.7817594660162));
#71207=CARTESIAN_POINT('Ctrl Pts',(-17.5556988450212,-17.1932233262362,
-13.7861332377332));
#71208=CARTESIAN_POINT('Ctrl Pts',(-17.4951295676243,-17.2338020140125,
-13.7905056784967));
#71209=CARTESIAN_POINT('Ctrl Pts',(-17.4366388203446,-17.2775266181314,
-13.7948781192603));
#71210=CARTESIAN_POINT('Ctrl Pts',(-17.3805632774546,-17.3241492580505,
-13.7992505600238));
#71211=CARTESIAN_POINT('Ctrl Pts',(-17.3244863007067,-17.3707730901158,
-13.8036231125912));
#71212=CARTESIAN_POINT('Ctrl Pts',(-17.2708250206033,-17.4202947951757,
-13.8079956651585));
#71213=CARTESIAN_POINT('Ctrl Pts',(-17.2198825933082,-17.4724265889274,
-13.8123682177259));
#71214=CARTESIAN_POINT('Ctrl Pts',(-17.1688872960406,-17.524612487021,-13.8167453082932));
#71215=CARTESIAN_POINT('Ctrl Pts',(-17.120616823207,-17.5794135364615,-13.8211223988605));
#71216=CARTESIAN_POINT('Ctrl Pts',(-17.0753364363177,-17.6365061070028,
-13.8254994894279));
#71217=CARTESIAN_POINT('Ctrl Pts',(-17.0300313201285,-17.693629857916,-13.8298789704868));
#71218=CARTESIAN_POINT('Ctrl Pts',(-16.9877198211676,-17.75304722842,-13.8342584515458));
#71219=CARTESIAN_POINT('Ctrl Pts',(-16.9486243452989,-17.8144048296514,
-13.8386379326047));
#71220=CARTESIAN_POINT('Ctrl Pts',(-16.9094595729617,-17.8758711868189,
-13.8430251762644));
#71221=CARTESIAN_POINT('Ctrl Pts',(-16.8735224451858,-17.9392842223086,
-13.8474124199242));
#71222=CARTESIAN_POINT('Ctrl Pts',(-16.8409895323028,-18.0042656652896,
-13.8517996635839));
#71223=CARTESIAN_POINT('Ctrl Pts',(-16.8188702864069,-18.0484467849189,
-13.8547825665187));
#71224=CARTESIAN_POINT('Ctrl Pts',(-16.7983237185202,-18.0933524542023,
-13.8577654694534));
#71225=CARTESIAN_POINT('Ctrl Pts',(-16.7793923012851,-18.1388593331259,
-13.8607483723882));
#71226=CARTESIAN_POINT('Ctrl Pts',(-16.7515419099038,-18.2058054245266,
-13.8651365813191));
#71227=CARTESIAN_POINT('Ctrl Pts',(-16.7270805292278,-18.2743146794849,
-13.86952479025));
#71228=CARTESIAN_POINT('Ctrl Pts',(-16.7061840240079,-18.3440103886485,
-13.8739129991809));
#71229=CARTESIAN_POINT('Ctrl Pts',(-16.6853185326665,-18.4136026578239,
-13.8782946952822));
#71230=CARTESIAN_POINT('Ctrl Pts',(-16.6680075510805,-18.4843774273511,
-13.8826763913834));
#71231=CARTESIAN_POINT('Ctrl Pts',(-16.6543788886961,-18.5559380939561,
-13.8870580874847));
#71232=CARTESIAN_POINT('Ctrl Pts',(-16.6407662410747,-18.6274146710828,
-13.8914346347443));
#71233=CARTESIAN_POINT('Ctrl Pts',(-16.6308274068039,-18.6996748392565,
-13.895811182004));
#71234=CARTESIAN_POINT('Ctrl Pts',(-16.6246399100932,-18.772308566959,-13.9001877292636));
#71235=CARTESIAN_POINT('Ctrl Pts',(-16.618456337403,-18.844896231407,-13.9045615009806));
#71236=CARTESIAN_POINT('Ctrl Pts',(-16.6160194227851,-18.917856505877,-13.9089352726976));
#71237=CARTESIAN_POINT('Ctrl Pts',(-16.6173550828665,-18.9907723454644,
-13.9133090444145));
#71238=CARTESIAN_POINT('Ctrl Pts',(-16.618690336502,-19.0636659965168,-13.9176814851781));
#71239=CARTESIAN_POINT('Ctrl Pts',(-16.6237958768595,-19.1365147575244,
-13.9220539259416));
#71240=CARTESIAN_POINT('Ctrl Pts',(-16.6326455110291,-19.2089013656677,
-13.9264263667052));
#71241=CARTESIAN_POINT('Ctrl Pts',(-16.6414953714849,-19.2812898247448,
-13.9307989192725));
#71242=CARTESIAN_POINT('Ctrl Pts',(-16.6540894553072,-19.3532156289256,
-13.9351714718399));
#71243=CARTESIAN_POINT('Ctrl Pts',(-16.6703498741219,-19.424268099667,-13.9395440244072));
#71244=CARTESIAN_POINT('Ctrl Pts',(-16.6866271686125,-19.4953943113425,
-13.9439211149746));
#71245=CARTESIAN_POINT('Ctrl Pts',(-16.7065782873148,-19.5656449087057,
-13.9482982055419));
#71246=CARTESIAN_POINT('Ctrl Pts',(-16.7300746894321,-19.6346216738906,
-13.9526752961092));
#71247=CARTESIAN_POINT('Ctrl Pts',(-16.7535839238067,-19.7036361098473,
-13.9570547771682));
#71248=CARTESIAN_POINT('Ctrl Pts',(-16.7806421175111,-19.7713748802477,
-13.9614342582271));
#71249=CARTESIAN_POINT('Ctrl Pts',(-16.8110725105123,-19.8374596942676,
-13.9658137392861));
#71250=CARTESIAN_POINT('Ctrl Pts',(-16.8415568411807,-19.9036616431767,
-13.9702009829458));
#71251=CARTESIAN_POINT('Ctrl Pts',(-16.8754250830335,-19.9682033538497,
-13.9745882266055));
#71252=CARTESIAN_POINT('Ctrl Pts',(-16.912454744336,-20.0307316077542,-13.9789754702652));
#71253=CARTESIAN_POINT('Ctrl Pts',(-16.9376313458521,-20.0732447952011,
-13.9819583732));
#71254=CARTESIAN_POINT('Ctrl Pts',(-16.9642684397431,-20.1148277943094,
-13.9849412761349));
#71255=CARTESIAN_POINT('Ctrl Pts',(-16.992285306212,-20.1553781306983,-13.9879241790697));
#71256=CARTESIAN_POINT('Ctrl Pts',(-17.033501486001,-20.2150325519721,-13.9923123880006));
#71257=CARTESIAN_POINT('Ctrl Pts',(-17.0778664461832,-20.2726834623514,
-13.9967005969315));
#71258=CARTESIAN_POINT('Ctrl Pts',(-17.1251586260628,-20.3279790817843,
-14.0010888058624));
#71259=CARTESIAN_POINT('Ctrl Pts',(-17.1723806165062,-20.3831926333497,
-14.0054705019636));
#71260=CARTESIAN_POINT('Ctrl Pts',(-17.2225208913247,-20.4360574697368,
-14.0098521980649));
#71261=CARTESIAN_POINT('Ctrl Pts',(-17.2753151507578,-20.4862514495973,
-14.0142338941662));
#71262=CARTESIAN_POINT('Ctrl Pts',(-17.3280473727347,-20.536386447537,-14.0186104414258));
#71263=CARTESIAN_POINT('Ctrl Pts',(-17.3834270362634,-20.583856492814,-14.0229869886854));
#71264=CARTESIAN_POINT('Ctrl Pts',(-17.4411513321102,-20.6283744575529,
-14.0273635359451));
#71265=CARTESIAN_POINT('Ctrl Pts',(-17.4988390200476,-20.6728641896455,
-14.031737307662));
#71266=CARTESIAN_POINT('Ctrl Pts',(-17.5588680090003,-20.7144052619587,
-14.036111079379));
#71267=CARTESIAN_POINT('Ctrl Pts',(-17.6209016583808,-20.7527501442134,
-14.040484851096));
#71268=CARTESIAN_POINT('Ctrl Pts',(-17.6829164307134,-20.7910833579916,
-14.0448572918595));
#71269=CARTESIAN_POINT('Ctrl Pts',(-17.7469342423156,-20.8262220591676,
-14.0492297326231));
#71270=CARTESIAN_POINT('Ctrl Pts',(-17.8125900634645,-20.8579624153833,
-14.0536021733866));
#71271=CARTESIAN_POINT('Ctrl Pts',(-17.8782475634398,-20.8897035832033,
-14.057974725954));
#71272=CARTESIAN_POINT('Ctrl Pts',(-17.9455427209576,-20.9180460253879,
-14.0623472785213));
#71273=CARTESIAN_POINT('Ctrl Pts',(-18.0140880608548,-20.9428329412274,
-14.0667198310886));
#71274=CARTESIAN_POINT('Ctrl Pts',(-18.0827045396913,-20.9676455818632,
-14.071096921656));
#71275=CARTESIAN_POINT('Ctrl Pts',(-18.1525733368264,-20.9888951643123,
-14.0754740122233));
#71276=CARTESIAN_POINT('Ctrl Pts',(-18.2232900373588,-21.0064742232647,
-14.0798511027906));
#71277=CARTESIAN_POINT('Ctrl Pts',(-18.2940453589062,-21.0240628827937,
-14.0842305838495));
#71278=CARTESIAN_POINT('Ctrl Pts',(-18.3656490319732,-21.0379769355906,
-14.0886100649085));
#71279=CARTESIAN_POINT('Ctrl Pts',(-18.4376872969889,-21.0481602472221,
-14.0929895459674));
#71280=CARTESIAN_POINT('Ctrl Pts',(-18.5098532493457,-21.0583616087051,
-14.0973767896272));
#71281=CARTESIAN_POINT('Ctrl Pts',(-18.5824548510274,-21.0648189809294,
-14.1017640332869));
#71282=CARTESIAN_POINT('Ctrl Pts',(-18.6550746705903,-21.0675282537413,
-14.1061512769466));
#71283=CARTESIAN_POINT('Ctrl Pts',(-18.7044491502641,-21.0693702981885,
-14.1091341798814));
#71284=CARTESIAN_POINT('Ctrl Pts',(-18.7538320255728,-21.069480806371,-14.1121170828162));
#71285=CARTESIAN_POINT('Ctrl Pts',(-18.8030934396838,-21.0678721834252,
-14.1150999857511));
#71286=CARTESIAN_POINT('Ctrl Pts',(-18.8755629038514,-21.0655057056244,
-14.119488194682));
#71287=CARTESIAN_POINT('Ctrl Pts',(-18.9480521075247,-21.0594071393707,
-14.1238764036129));
#71288=CARTESIAN_POINT('Ctrl Pts',(-19.020145332748,-21.0495723702763,-14.1282646125438));
#71289=CARTESIAN_POINT('Ctrl Pts',(-19.092131559672,-21.0397521976099,-14.132646308645));
#71290=CARTESIAN_POINT('Ctrl Pts',(-19.1637225008059,-21.0262068946333,
-14.1370280047463));
#71291=CARTESIAN_POINT('Ctrl Pts',(-19.2345042258083,-21.008984326617,-14.1414097008476));
#71292=CARTESIAN_POINT('Ctrl Pts',(-19.3052027766506,-20.9917819964888,
-14.1457862481073));
#71293=CARTESIAN_POINT('Ctrl Pts',(-19.3750935339407,-20.9709110986507,
-14.1501627953669));
#71294=CARTESIAN_POINT('Ctrl Pts',(-19.4437711636795,-20.9464708308745,
-14.1545393426265));
#71295=CARTESIAN_POINT('Ctrl Pts',(-19.5124052390636,-20.9220460627608,
-14.1589131143435));
#71296=CARTESIAN_POINT('Ctrl Pts',(-19.5798272600421,-20.8940565773994,
-14.1632868860605));
#71297=CARTESIAN_POINT('Ctrl Pts',(-19.6456468756575,-20.8626514528045,
-14.1676606577775));
#71298=CARTESIAN_POINT('Ctrl Pts',(-19.7114464621431,-20.8312558848944,
-14.172033098541));
#71299=CARTESIAN_POINT('Ctrl Pts',(-19.7756441762387,-20.7964469488634,
-14.1764055393046));
#71300=CARTESIAN_POINT('Ctrl Pts',(-19.8378710435228,-20.758421246352,-14.1807779800682));
#71301=CARTESIAN_POINT('Ctrl Pts',(-19.9000995019545,-20.7203945715193,
-14.1851505326355));
#71302=CARTESIAN_POINT('Ctrl Pts',(-19.9603566029539,-20.6791512201339,
-14.1895230852029));
#71303=CARTESIAN_POINT('Ctrl Pts',(-20.0183007689816,-20.6349321242383,
-14.1938956377702));
#71304=CARTESIAN_POINT('Ctrl Pts',(-20.0763050716505,-20.5906671360971,
-14.1982727283375));
#71305=CARTESIAN_POINT('Ctrl Pts',(-20.1319912623935,-20.5434205306327,
-14.2026498189049));
#71306=CARTESIAN_POINT('Ctrl Pts',(-20.185050077776,-20.493474187843,-14.2070269094722));
#71307=CARTESIAN_POINT('Ctrl Pts',(-20.2381378705468,-20.4435005675018,
-14.2114063905311));
#71308=CARTESIAN_POINT('Ctrl Pts',(-20.2885950971624,-20.3908246228575,
-14.2157858715901));
#71309=CARTESIAN_POINT('Ctrl Pts',(-20.3361505972396,-20.3357638757262,
-14.220165352649));
#71310=CARTESIAN_POINT('Ctrl Pts',(-20.3837903891216,-20.2806055337902,
-14.2245525963088));
#71311=CARTESIAN_POINT('Ctrl Pts',(-20.4285178872528,-20.2230543293395,
-14.2289398399685));
#71312=CARTESIAN_POINT('Ctrl Pts',(-20.4701036879215,-20.1634590314102,
-14.2333270836282));
#71313=CARTESIAN_POINT('Ctrl Pts',(-20.4983780251775,-20.1229399714081,
-14.236309986563));
#71314=CARTESIAN_POINT('Ctrl Pts',(-20.5252009588545,-20.0814766042671,
-14.2392928894977));
#71315=CARTESIAN_POINT('Ctrl Pts',(-20.5505126306684,-20.0391848336977,
-14.2422757924325));
#71316=CARTESIAN_POINT('Ctrl Pts',(-20.5890177730798,-19.9748488759396,
-14.2468135054349));
#71317=CARTESIAN_POINT('Ctrl Pts',(-20.6241652163778,-19.9083583182789,
-14.2513512184373));
#71318=CARTESIAN_POINT('Ctrl Pts',(-20.6557165770424,-19.8400846792511,
-14.2558889314397));
#71319=CARTESIAN_POINT('Ctrl Pts',(-20.6802004039359,-19.7871043980798,
-14.2594101925614));
#71320=CARTESIAN_POINT('Ctrl Pts',(-20.7025195175006,-19.7330511128152,
-14.262931453683));
#71321=CARTESIAN_POINT('Ctrl Pts',(-20.7225805821191,-19.6781103693095,
-14.2664527148047));
#71322=CARTESIAN_POINT('',(-20.8509999987353,-18.9520661441397,-13.2889079339059));
#71323=CARTESIAN_POINT('Ctrl Pts',(-20.7225805863163,-19.6781103578147,
-14.0426552896606));
#71324=CARTESIAN_POINT('Ctrl Pts',(-20.6958130594779,-19.7514179255168,
-14.0381451322549));
#71325=CARTESIAN_POINT('Ctrl Pts',(-20.6650078160421,-19.8232019799177,
-14.0337656063037));
#71326=CARTESIAN_POINT('Ctrl Pts',(-20.570357267885,-20.0139143494066,-14.0220205212262));
#71327=CARTESIAN_POINT('Ctrl Pts',(-20.4990150095605,-20.128686030151,-14.014842078084));
#71328=CARTESIAN_POINT('Ctrl Pts',(-20.3708542579152,-20.2967113021131,
-14.00314981442));
#71329=CARTESIAN_POINT('Ctrl Pts',(-20.3212057751213,-20.3549666842381,
-13.9988302312449));
#71330=CARTESIAN_POINT('Ctrl Pts',(-20.2619779473043,-20.4172858424494,
-13.9937348557344));
#71331=CARTESIAN_POINT('Ctrl Pts',(-20.2553888187653,-20.4241261026367,
-13.9931687258888));
#71332=CARTESIAN_POINT('Ctrl Pts',(-20.2455537548807,-20.4341994575187,
-13.9923243664036));
#71333=CARTESIAN_POINT('Ctrl Pts',(-20.2423428879629,-20.4374668347659,
-13.9920488096215));
#71334=CARTESIAN_POINT('Ctrl Pts',(-20.2366096482909,-20.443263223973,-13.9915569074305));
#71335=CARTESIAN_POINT('Ctrl Pts',(-20.2340914553369,-20.4457962992678,
-13.9913408910602));
#71336=CARTESIAN_POINT('Ctrl Pts',(-20.2286618086867,-20.4512304592593,
-13.9908751940785));
#71337=CARTESIAN_POINT('Ctrl Pts',(-20.2257483564714,-20.4541293994255,
-13.9906253579057));
#71338=CARTESIAN_POINT('Ctrl Pts',(-20.2176786545163,-20.4621122752175,
-13.989933542351));
#71339=CARTESIAN_POINT('Ctrl Pts',(-20.212504790597,-20.4671782120668,-13.9894901916504));
#71340=CARTESIAN_POINT('Ctrl Pts',(-20.1839451790823,-20.4948565043005,
-13.9870445508267));
#71341=CARTESIAN_POINT('Ctrl Pts',(-20.1600679645244,-20.5169527490522,
-13.98500593417));
#71342=CARTESIAN_POINT('Ctrl Pts',(-20.0137580935607,-20.6462202890972,
-13.9726000643451));
#71343=CARTESIAN_POINT('Ctrl Pts',(-19.8798138869347,-20.7395328337544,
-13.9616428011667));
#71344=CARTESIAN_POINT('Ctrl Pts',(-19.6336216829691,-20.8718996822781,
-13.9433847142914));
#71345=CARTESIAN_POINT('Ctrl Pts',(-19.5263234482218,-20.9186126517695,
-13.9359438713396));
#71346=CARTESIAN_POINT('Ctrl Pts',(-19.4021738934597,-20.9608396734241,
-13.9279368114988));
#71347=CARTESIAN_POINT('Ctrl Pts',(-19.388599174331,-20.9653040312148,-13.9270688353924));
#71348=CARTESIAN_POINT('Ctrl Pts',(-19.3669223587197,-20.9721905273076,
-13.9256945267389));
#71349=CARTESIAN_POINT('Ctrl Pts',(-19.3588493380864,-20.9747021003408,
-13.9251852661232));
#71350=CARTESIAN_POINT('Ctrl Pts',(-19.3445847676617,-20.9790463563296,
-13.9242898879908));
#71351=CARTESIAN_POINT('Ctrl Pts',(-19.3383995139578,-20.9808991887647,
-13.9239031143469));
#71352=CARTESIAN_POINT('Ctrl Pts',(-19.3255888931867,-20.9846729113781,
-13.9231050456488));
#71353=CARTESIAN_POINT('Ctrl Pts',(-19.3189624130423,-20.9865897768965,
-13.9226938859751));
#71354=CARTESIAN_POINT('Ctrl Pts',(-19.3019291080572,-20.9914269673407,
-13.9216411764047));
#71355=CARTESIAN_POINT('Ctrl Pts',(-19.2915089917432,-20.9943000655092,
-13.9210011678085));
#71356=CARTESIAN_POINT('Ctrl Pts',(-19.2479272897527,-21.0059582715653,
-13.9183405043392));
#71357=CARTESIAN_POINT('Ctrl Pts',(-19.2145755469596,-21.0140167750891,
-13.9163433781623));
#71358=CARTESIAN_POINT('Ctrl Pts',(-19.1271788951886,-21.0328978618357,
-13.9111993066022));
#71359=CARTESIAN_POINT('Ctrl Pts',(-19.0728803307786,-21.0424273060357,
-13.9080917500926));
#71360=CARTESIAN_POINT('Ctrl Pts',(-18.9099125740972,-21.0645104474783,
-13.8989473439218));
#71361=CARTESIAN_POINT('Ctrl Pts',(-18.8005787820791,-21.0707764803836,
-13.8930592236637));
#71362=CARTESIAN_POINT('Ctrl Pts',(-18.6455316024656,-21.0676449206137,
-13.8846160841683));
#71363=CARTESIAN_POINT('Ctrl Pts',(-18.599855691559,-21.0652404394081,-13.8821157478915));
#71364=CARTESIAN_POINT('Ctrl Pts',(-18.5315831001636,-21.0594240126794,
-13.8783162800304));
#71365=CARTESIAN_POINT('Ctrl Pts',(-18.5089045695325,-21.0571224586437,
-13.8770438075666));
#71366=CARTESIAN_POINT('Ctrl Pts',(-18.4852320985487,-21.0543331371715,
-13.8757007831837));
#71367=CARTESIAN_POINT('Ctrl Pts',(-18.4841960740489,-21.0542102861073,
-13.8756419760979));
#71368=CARTESIAN_POINT('Ctrl Pts',(-18.4647520122641,-21.0518900460502,
-13.8745377231388));
#71369=CARTESIAN_POINT('Ctrl Pts',(-18.4463740145589,-21.0494517730584,
-13.8734845244421));
#71370=CARTESIAN_POINT('Ctrl Pts',(-18.395068554122,-21.0419579355252,-13.8705119707729));
#71371=CARTESIAN_POINT('Ctrl Pts',(-18.3622264712923,-21.0363662975981,
-13.8685717292965));
#71372=CARTESIAN_POINT('Ctrl Pts',(-18.3227430090821,-21.0286811323164,
-13.8661790299478));
#71373=CARTESIAN_POINT('Ctrl Pts',(-18.3159605461909,-21.0273264441956,
-13.8657658562964));
#71374=CARTESIAN_POINT('Ctrl Pts',(-18.3048320049023,-21.0250469302752,
-13.8650842032775));
#71375=CARTESIAN_POINT('Ctrl Pts',(-18.3004819239325,-21.0241416023125,
-13.8648168120685));
#71376=CARTESIAN_POINT('Ctrl Pts',(-18.2926501571094,-21.0224859336363,
-13.864333666449));
#71377=CARTESIAN_POINT('Ctrl Pts',(-18.2891674908681,-21.021740496704,-13.8641181946151));
#71378=CARTESIAN_POINT('Ctrl Pts',(-18.2815707121067,-21.0200944069595,
-13.8636468100729));
#71379=CARTESIAN_POINT('Ctrl Pts',(-18.2774574516174,-21.0191902760618,
-13.863390704664));
#71380=CARTESIAN_POINT('Ctrl Pts',(-18.265824930441,-21.0165969333777,-13.8626640003407));
#71381=CARTESIAN_POINT('Ctrl Pts',(-18.2583122481092,-21.014878947389,-13.862191798882));
#71382=CARTESIAN_POINT('Ctrl Pts',(-18.2115906178136,-21.0039259414533,
-13.8592379839106));
#71383=CARTESIAN_POINT('Ctrl Pts',(-18.1726452438009,-20.9936150424382,
-13.8567004343362));
#71384=CARTESIAN_POINT('Ctrl Pts',(-17.9658344518386,-20.9324968498077,
-13.8429036509314));
#71385=CARTESIAN_POINT('Ctrl Pts',(-17.8044754330324,-20.862087847567,-13.8310594756206));
#71386=CARTESIAN_POINT('Ctrl Pts',(-17.6231896039867,-20.7545102229363,
-13.817408711854));
#71387=CARTESIAN_POINT('Ctrl Pts',(-17.5931950808407,-20.7356779892051,
-13.8151346568204));
#71388=CARTESIAN_POINT('Ctrl Pts',(-17.5108348252259,-20.6810397661047,
-13.8088525077503));
#71389=CARTESIAN_POINT('Ctrl Pts',(-17.4595822218534,-20.6436182244313,
-13.8048998612005));
#71390=CARTESIAN_POINT('Ctrl Pts',(-17.4003125151941,-20.5961178389879,
-13.8002730479109));
#71391=CARTESIAN_POINT('Ctrl Pts',(-17.3906115607842,-20.5882008701747,
-13.7995138155754));
#71392=CARTESIAN_POINT('Ctrl Pts',(-17.3748161558637,-20.5750750237738,
-13.7982742408212));
#71393=CARTESIAN_POINT('Ctrl Pts',(-17.3686801440415,-20.5699168546755,
-13.7977918571357));
#71394=CARTESIAN_POINT('Ctrl Pts',(-17.3577131987294,-20.5605907950322,
-13.7969281001716));
#71395=CARTESIAN_POINT('Ctrl Pts',(-17.3528715546427,-20.5564357026755,
-13.7965462090103));
#71396=CARTESIAN_POINT('Ctrl Pts',(-17.342612790318,-20.5475507973629,-13.7957357938495));
#71397=CARTESIAN_POINT('Ctrl Pts',(-17.3372008270287,-20.5428151327471,
-13.795307518859));
#71398=CARTESIAN_POINT('Ctrl Pts',(-17.3227223124671,-20.5300150574653,
-13.7941596766478));
#71399=CARTESIAN_POINT('Ctrl Pts',(-17.3137007039153,-20.5219000451298,
-13.7934422330006));
#71400=CARTESIAN_POINT('Ctrl Pts',(-17.2693543032314,-20.4813149060312,
-13.7899037184889));
#71401=CARTESIAN_POINT('Ctrl Pts',(-17.2350690976651,-20.4477265007838,
-13.7871307206324));
#71402=CARTESIAN_POINT('Ctrl Pts',(-17.0861946227446,-20.2916123914936,
-13.7748562278756));
#71403=CARTESIAN_POINT('Ctrl Pts',(-16.9852763364841,-20.1569029039112,
-13.7659337984802));
#71404=CARTESIAN_POINT('Ctrl Pts',(-16.8518811219019,-19.9262019060021,
-13.7513439704959));
#71405=CARTESIAN_POINT('Ctrl Pts',(-16.8084984036073,-19.837369583522,-13.7458494497216));
#71406=CARTESIAN_POINT('Ctrl Pts',(-16.7678421032428,-19.7368605735506,
-13.7394261789977));
#71407=CARTESIAN_POINT('Ctrl Pts',(-16.7642684258916,-19.7278482537088,
-13.7388484399939));
#71408=CARTESIAN_POINT('Ctrl Pts',(-16.7590835807036,-19.7145060504538,
-13.7379900563293));
#71409=CARTESIAN_POINT('Ctrl Pts',(-16.7574244231181,-19.7101947824483,
-13.7377122150107));
#71410=CARTESIAN_POINT('Ctrl Pts',(-16.7545060671554,-19.7025368449652,
-13.7372178024269));
#71411=CARTESIAN_POINT('Ctrl Pts',(-16.7532412227223,-19.6991923794091,
-13.7370015731437));
#71412=CARTESIAN_POINT('Ctrl Pts',(-16.7505494558862,-19.6920200182399,
-13.7365371924027));
#71413=CARTESIAN_POINT('Ctrl Pts',(-16.7491251598172,-19.688191249947,-13.736288894693));
#71414=CARTESIAN_POINT('Ctrl Pts',(-16.7452460607196,-19.677670434057,-13.7356055627893));
#71415=CARTESIAN_POINT('Ctrl Pts',(-16.7428139872269,-19.6709701447711,
-13.7351692110695));
#71416=CARTESIAN_POINT('Ctrl Pts',(-16.7300120784403,-19.6351380595596,
-13.7328299536195));
#71417=CARTESIAN_POINT('Ctrl Pts',(-16.7202482036132,-19.6057955854087,
-13.7308942755497));
#71418=CARTESIAN_POINT('Ctrl Pts',(-16.6926441574388,-19.516345496827,-13.7249549318184));
#71419=CARTESIAN_POINT('Ctrl Pts',(-16.6768287772441,-19.4556516428797,
-13.7208738366959));
#71420=CARTESIAN_POINT('Ctrl Pts',(-16.6356233923252,-19.2628039204623,
-13.7079148633303));
#71421=CARTESIAN_POINT('Ctrl Pts',(-16.62011557536,-19.1288652045959,-13.6989492342522));
#71422=CARTESIAN_POINT('Ctrl Pts',(-16.6166067523205,-18.9535302107213,
-13.6876558111758));
#71423=CARTESIAN_POINT('Ctrl Pts',(-16.6169711232901,-18.9126863708646,
-13.6850538712989));
#71424=CARTESIAN_POINT('Ctrl Pts',(-16.6203521445676,-18.8234178926193,
-13.6794348513671));
#71425=CARTESIAN_POINT('Ctrl Pts',(-16.6238520980651,-18.7750337559787,
-13.6764331910092));
#71426=CARTESIAN_POINT('Ctrl Pts',(-16.6303507814106,-18.7142867870322,
-13.672717270952));
#71427=CARTESIAN_POINT('Ctrl Pts',(-16.631802166116,-18.7017763311501,-13.6719547985169));
#71428=CARTESIAN_POINT('Ctrl Pts',(-16.6342793176457,-18.6819697761488,
-13.6707519229242));
#71429=CARTESIAN_POINT('Ctrl Pts',(-16.6352316620923,-18.6746649469813,
-13.6703092143439));
#71430=CARTESIAN_POINT('Ctrl Pts',(-16.6370774367705,-18.6610614634888,
-13.6694864484722));
#71431=CARTESIAN_POINT('Ctrl Pts',(-16.6379611641632,-18.6547615969657,
-13.6691060894844));
#71432=CARTESIAN_POINT('Ctrl Pts',(-16.639987347999,-18.6407759858801,-13.6682631452072));
#71433=CARTESIAN_POINT('Ctrl Pts',(-16.6411437520609,-18.6330923305548,
-13.6678010065479));
#71434=CARTESIAN_POINT('Ctrl Pts',(-16.6446277933629,-18.6107783101194,
-13.6664616348755));
#71435=CARTESIAN_POINT('Ctrl Pts',(-16.6470667570564,-18.5961656063579,
-13.6655879332183));
#71436=CARTESIAN_POINT('Ctrl Pts',(-16.6677249281885,-18.4799229437949,
-13.6586625321205));
#71437=CARTESIAN_POINT('Ctrl Pts',(-16.6932044991284,-18.3797175849504,
-13.6528538415446));
#71438=CARTESIAN_POINT('Ctrl Pts',(-16.7764326814558,-18.1303579151069,
-13.6383804516741));
#71439=CARTESIAN_POINT('Ctrl Pts',(-16.8439212937676,-17.9851700658453,
-13.6299536921691));
#71440=CARTESIAN_POINT('Ctrl Pts',(-16.9523809047564,-17.8074994601538,
-13.618198884059));
#71441=CARTESIAN_POINT('Ctrl Pts',(-16.9791052316602,-17.7669296862551,
-13.6154022716616));
#71442=CARTESIAN_POINT('Ctrl Pts',(-17.0116875206783,-17.7209886520113,
-13.6120585139978));
#71443=CARTESIAN_POINT('Ctrl Pts',(-17.0162112748365,-17.7146839098953,
-13.6115956410275));
#71444=CARTESIAN_POINT('Ctrl Pts',(-17.0234999390514,-17.7046427352062,
-13.6108517977022));
#71445=CARTESIAN_POINT('Ctrl Pts',(-17.0262427189144,-17.7008902236435,
-13.6105723151012));
#71446=CARTESIAN_POINT('Ctrl Pts',(-17.0311248243385,-17.694256777935,-13.610075542032));
#71447=CARTESIAN_POINT('Ctrl Pts',(-17.0332591429314,-17.691372214542,-13.609858600215));
#71448=CARTESIAN_POINT('Ctrl Pts',(-17.0378013193579,-17.6852659266808,
-13.6093973848977));
#71449=CARTESIAN_POINT('Ctrl Pts',(-17.0402109897701,-17.6820456839236,
-13.6091529891958));
#71450=CARTESIAN_POINT('Ctrl Pts',(-17.0467453190594,-17.6733649968834,
-13.608491066855));
#71451=CARTESIAN_POINT('Ctrl Pts',(-17.050887260276,-17.667917708255,-13.6080723543029));
#71452=CARTESIAN_POINT('Ctrl Pts',(-17.0716513221643,-17.6408828449773,
-13.6059779703024));
#71453=CARTESIAN_POINT('Ctrl Pts',(-17.0886618705169,-17.619598559898,-13.6042769863701));
#71454=CARTESIAN_POINT('Ctrl Pts',(-17.1391486009376,-17.5588689130347,
-13.599284761692));
#71455=CARTESIAN_POINT('Ctrl Pts',(-17.1736646918612,-17.5203163000448,
-13.5959403877277));
#71456=CARTESIAN_POINT('Ctrl Pts',(-17.3054203723514,-17.3835813132554,
-13.5835285051363));
#71457=CARTESIAN_POINT('Ctrl Pts',(-17.4108030784123,-17.2937084497809,
-13.5742897737105));
#71458=CARTESIAN_POINT('Ctrl Pts',(-17.6031704743741,-17.1597454553624,
-13.5591100729883));
#71459=CARTESIAN_POINT('Ctrl Pts',(-17.6858164728997,-17.1101890588021,
-13.5530293088708));
#71460=CARTESIAN_POINT('Ctrl Pts',(-17.7839415884109,-17.06010378842,-13.5463058347475));
#71461=CARTESIAN_POINT('Ctrl Pts',(-17.7963858895196,-17.0539056780228,
-13.5454617093154));
#71462=CARTESIAN_POINT('Ctrl Pts',(-17.8163935981916,-17.0441852620685,
-13.5441179456696));
#71463=CARTESIAN_POINT('Ctrl Pts',(-17.8239181787173,-17.0405843820378,
-13.5436155784605));
#71464=CARTESIAN_POINT('Ctrl Pts',(-17.8372882116439,-17.0342830172411,
-13.5427281878522));
#71465=CARTESIAN_POINT('Ctrl Pts',(-17.8431250340579,-17.0315645666108,
-13.5423425451855));
#71466=CARTESIAN_POINT('Ctrl Pts',(-17.8552841475793,-17.0259689259553,
-13.5415427900568));
#71467=CARTESIAN_POINT('Ctrl Pts',(-17.8616083869506,-17.0230961343992,
-13.5411288328822));
#71468=CARTESIAN_POINT('Ctrl Pts',(-17.878008453911,-17.0157435447766,-13.5400604892632));
#71469=CARTESIAN_POINT('Ctrl Pts',(-17.8881054288738,-17.0113112127731,
-13.5394077349168));
#71470=CARTESIAN_POINT('Ctrl Pts',(-17.9315449037819,-16.9926457462694,
-13.536620257447));
#71471=CARTESIAN_POINT('Ctrl Pts',(-17.9652165596594,-16.9791909556015,
-13.5345120219859));
#71472=CARTESIAN_POINT('Ctrl Pts',(-18.055007263207,-16.9459599898318,-13.5290129268166));
#71473=CARTESIAN_POINT('Ctrl Pts',(-18.1116438435915,-16.9276726411516,
-13.5256689800554));
#71474=CARTESIAN_POINT('Ctrl Pts',(-18.3313423076377,-16.8668286551017,
-13.5130362316837));
#71475=CARTESIAN_POINT('Ctrl Pts',(-18.4984768940598,-16.8414091189746,
-13.5041712361617));
#71476=CARTESIAN_POINT('Ctrl Pts',(-18.7205483698113,-16.8343609538018,
-13.4916799741708));
#71477=CARTESIAN_POINT('Ctrl Pts',(-18.7742935543018,-16.8347018474999,
-13.4885976398515));
#71478=CARTESIAN_POINT('Ctrl Pts',(-18.8366877340728,-16.8374739278206,
-13.4848914337852));
#71479=CARTESIAN_POINT('Ctrl Pts',(-18.8454103542768,-16.837915562786,-13.4843703969722));
#71480=CARTESIAN_POINT('Ctrl Pts',(-18.8586087614712,-16.8386657192304,
-13.4835772560194));
#71481=CARTESIAN_POINT('Ctrl Pts',(-18.8630868338411,-16.83893452203,-13.4833073242564));
#71482=CARTESIAN_POINT('Ctrl Pts',(-18.871121040528,-16.8394424212446,-13.4828214941084));
#71483=CARTESIAN_POINT('Ctrl Pts',(-18.8746774529178,-16.8396762659908,
-13.4826058928054));
#71484=CARTESIAN_POINT('Ctrl Pts',(-18.8824012148666,-16.840203719118,-13.482136458809));
#71485=CARTESIAN_POINT('Ctrl Pts',(-18.8865682360268,-16.8405006783851,
-13.481882445683));
#71486=CARTESIAN_POINT('Ctrl Pts',(-18.8982638989283,-16.8413689619674,
-13.4811674471303));
#71487=CARTESIAN_POINT('Ctrl Pts',(-18.9057903147636,-16.8419682251193,
-13.48070493855));
#71488=CARTESIAN_POINT('Ctrl Pts',(-18.9506294209084,-16.84577986564,-13.4779359039066));
#71489=CARTESIAN_POINT('Ctrl Pts',(-18.987852292974,-16.8499414435024,-13.4755810765705));
#71490=CARTESIAN_POINT('Ctrl Pts',(-19.1096723722018,-16.8668437378152,
-13.4677314366213));
#71491=CARTESIAN_POINT('Ctrl Pts',(-19.1936065901604,-16.8837238401075,
-13.4620980916345));
#71492=CARTESIAN_POINT('Ctrl Pts',(-19.4479091261381,-16.9511135519632,
-13.4447180654062));
#71493=CARTESIAN_POINT('Ctrl Pts',(-19.6131680269204,-17.0180143043342,
-13.4330524665178));
#71494=CARTESIAN_POINT('Ctrl Pts',(-19.7880620718266,-17.1159273293674,
-13.4207171625239));
#71495=CARTESIAN_POINT('Ctrl Pts',(-19.8077921083987,-17.1273958579983,
-13.4193242841738));
#71496=CARTESIAN_POINT('Ctrl Pts',(-19.8353271342834,-17.1440025762275,
-13.4173778475465));
#71497=CARTESIAN_POINT('Ctrl Pts',(-19.8432889032704,-17.1488765226628,
-13.4168147248669));
#71498=CARTESIAN_POINT('Ctrl Pts',(-19.8567579545737,-17.1572448329992,
-13.4158614725421));
#71499=CARTESIAN_POINT('Ctrl Pts',(-19.862281747963,-17.160712241786,-13.4154703583744));
#71500=CARTESIAN_POINT('Ctrl Pts',(-19.8732383562729,-17.1676607388309,
-13.4146941837743));
#71501=CARTESIAN_POINT('Ctrl Pts',(-19.8786714536052,-17.1711412475788,
-13.41430910749));
#71502=CARTESIAN_POINT('Ctrl Pts',(-19.8895652008054,-17.1781903658174,
-13.413536575524));
#71503=CARTESIAN_POINT('Ctrl Pts',(-19.8950254385381,-17.181759484095,-13.4131491443765));
#71504=CARTESIAN_POINT('Ctrl Pts',(-19.9145651278664,-17.1946610173911,
-13.4117618411988));
#71505=CARTESIAN_POINT('Ctrl Pts',(-19.9285495108308,-17.2041367869009,
-13.4107673469734));
#71506=CARTESIAN_POINT('Ctrl Pts',(-20.0547616540925,-17.2918800599656,
-13.4017728488539));
#71507=CARTESIAN_POINT('Ctrl Pts',(-20.1592737051247,-17.3806911619782,
-13.394216406992));
#71508=CARTESIAN_POINT('Ctrl Pts',(-20.3678976506755,-17.5960388531668,
-13.3778937736117));
#71509=CARTESIAN_POINT('Ctrl Pts',(-20.4673865506338,-17.7257835060041,
-13.3692248150557));
#71510=CARTESIAN_POINT('Ctrl Pts',(-20.5582171469079,-17.8777008255907,
-13.3588209721347));
#71511=CARTESIAN_POINT('Ctrl Pts',(-20.5653157397344,-17.8898467375748,
-13.3579873443408));
#71512=CARTESIAN_POINT('Ctrl Pts',(-20.575038350056,-17.9068696514844,-13.3568151589996));
#71513=CARTESIAN_POINT('Ctrl Pts',(-20.5777652552586,-17.9116878671795,
-13.3564829572085));
#71514=CARTESIAN_POINT('Ctrl Pts',(-20.5821176096883,-17.9194489826807,
-13.3559470820917));
#71515=CARTESIAN_POINT('Ctrl Pts',(-20.5837550245248,-17.9223851926633,
-13.3557441720481));
#71516=CARTESIAN_POINT('Ctrl Pts',(-20.5871657415607,-17.9285356818154,
-13.3553187414431));
#71517=CARTESIAN_POINT('Ctrl Pts',(-20.5889376786719,-17.931750675663,-13.3550961329588));
#71518=CARTESIAN_POINT('Ctrl Pts',(-20.5932122404427,-17.9395543646391,
-13.3545552800165));
#71519=CARTESIAN_POINT('Ctrl Pts',(-20.5957062415976,-17.9441477349192,
-13.3542364919918));
#71520=CARTESIAN_POINT('Ctrl Pts',(-20.6044137014452,-17.9603274548222,
-13.3531121965151));
#71521=CARTESIAN_POINT('Ctrl Pts',(-20.6105360659002,-17.9719621309205,
-13.3523012230678));
#71522=CARTESIAN_POINT('Ctrl Pts',(-20.6463529977379,-18.0415932943318,
-13.3474362625599));
#71523=CARTESIAN_POINT('Ctrl Pts',(-20.673462968082,-18.1008736150483,-13.3432483730028));
#71524=CARTESIAN_POINT('Ctrl Pts',(-20.7663306087012,-18.3315219542664,
-13.3270239402859));
#71525=CARTESIAN_POINT('Ctrl Pts',(-20.8124570528268,-18.5099651622943,
-13.3147003989581));
#71526=CARTESIAN_POINT('Ctrl Pts',(-20.8382409111785,-18.718416868344,-13.3013963293275));
#71527=CARTESIAN_POINT('Ctrl Pts',(-20.8409993885486,-18.7447693006873,
-13.2997318868771));
#71528=CARTESIAN_POINT('Ctrl Pts',(-20.8463154969658,-18.8067773330992,
-13.295856603968));
#71529=CARTESIAN_POINT('Ctrl Pts',(-20.848466290051,-18.8424603529987,-13.2936584702531));
#71530=CARTESIAN_POINT('Ctrl Pts',(-20.8501018468728,-18.8893377032315,
-13.2908108478712));
#71531=CARTESIAN_POINT('Ctrl Pts',(-20.8504028282094,-18.9004959613303,
-13.2901359888879));
#71532=CARTESIAN_POINT('Ctrl Pts',(-20.8507477576331,-18.9185925177508,
-13.2890461762796));
#71533=CARTESIAN_POINT('Ctrl Pts',(-20.8508458709918,-18.9255294585662,
-13.2886295333159));
#71534=CARTESIAN_POINT('Ctrl Pts',(-20.8509497984574,-18.9367926063628,
-13.2879548253289));
#71535=CARTESIAN_POINT('Ctrl Pts',(-20.8509764542885,-18.9411185282282,
-13.2876961097797));
#71536=CARTESIAN_POINT('Ctrl Pts',(-20.8509965706207,-18.947614789788,-13.2873082240935));
#71537=CARTESIAN_POINT('Ctrl Pts',(-20.8509999537562,-18.9497850671378,
-13.2871787442691));
#71538=CARTESIAN_POINT('Ctrl Pts',(-20.8509999995292,-18.9519553508202,
-13.2870493686989));
#71539=CARTESIAN_POINT('Ctrl Pts',(-20.8509999986719,-18.9520749873283,
-13.2890562789747));
#71540=CARTESIAN_POINT('Ctrl Pts',(-20.8509972774554,-19.0288988399363,
-13.2844612169094));
#71541=CARTESIAN_POINT('Ctrl Pts',(-20.846808461958,-19.1056371709782,-13.2798661548441));
#71542=CARTESIAN_POINT('Ctrl Pts',(-20.8384871131054,-19.181832527666,-13.2752710927788));
#71543=CARTESIAN_POINT('Ctrl Pts',(-20.8301538008358,-19.258137428713,-13.2706694244956));
#71544=CARTESIAN_POINT('Ctrl Pts',(-20.8176761741826,-19.3338973982161,
-13.2660677562124));
#71545=CARTESIAN_POINT('Ctrl Pts',(-20.8011589270257,-19.408665052766,-13.2614660879292));
#71546=CARTESIAN_POINT('Ctrl Pts',(-20.784602739877,-19.4836089746948,-13.256853571051));
#71547=CARTESIAN_POINT('Ctrl Pts',(-20.7639880126746,-19.5575555158826,
-13.2522410541727));
#71548=CARTESIAN_POINT('Ctrl Pts',(-20.7394693418677,-19.6300720602036,
-13.2476285372945));
#71549=CARTESIAN_POINT('Ctrl Pts',(-20.7340309672849,-19.6461566242721,
-13.2466054559557));
#71550=CARTESIAN_POINT('Ctrl Pts',(-20.728400713704,-19.6621709183055,-13.245582374617));
#71551=CARTESIAN_POINT('Ctrl Pts',(-20.7225805821191,-19.6781103693095,
-13.2445592932782));
#71552=CARTESIAN_POINT('Origin',(-18.734,-18.952,0.));
#71553=CARTESIAN_POINT('',(-20.7242504220745,-19.678735851896,-12.4443820803097));
#71554=CARTESIAN_POINT('',(-20.7225804971235,-19.678110602085,-12.6679319461521));
#71555=CARTESIAN_POINT('',(-20.7225805821191,-19.6781103693095,0.));
#71556=CARTESIAN_POINT('Ctrl Pts',(-20.7225804971235,-19.6781106020849,
-12.6679319461521));
#71557=CARTESIAN_POINT('Ctrl Pts',(-20.7627960942047,-19.5679731770063,
-12.6745736078838));
#71558=CARTESIAN_POINT('Ctrl Pts',(-20.7938156866259,-19.4546218238198,
-12.6809438939));
#71559=CARTESIAN_POINT('Ctrl Pts',(-20.8390879830612,-19.2112808287383,
-12.694385289415));
#71560=CARTESIAN_POINT('Ctrl Pts',(-20.8510398086386,-19.0814434490627,
-12.7014276962788));
#71561=CARTESIAN_POINT('Ctrl Pts',(-20.8509988957479,-18.948075646787,-12.709218677413));
#71562=CARTESIAN_POINT('Ctrl Pts',(-20.8509902918148,-18.9448007475233,
-12.7094103387302));
#71563=CARTESIAN_POINT('Ctrl Pts',(-20.850896614057,-18.925867051309,-12.7105205155376));
#71564=CARTESIAN_POINT('Ctrl Pts',(-20.8506454058121,-18.9102100571119,
-12.7114468464764));
#71565=CARTESIAN_POINT('Ctrl Pts',(-20.8500635609687,-18.8887743830472,
-12.7127281576504));
#71566=CARTESIAN_POINT('Ctrl Pts',(-20.8498828713514,-18.882991698817,-12.7130751213308));
#71567=CARTESIAN_POINT('Ctrl Pts',(-20.8495580067021,-18.873801856879,-12.7136286934075));
#71568=CARTESIAN_POINT('Ctrl Pts',(-20.8494292971625,-18.8703941323496,
-12.7138344418728));
#71569=CARTESIAN_POINT('Ctrl Pts',(-20.8491463981908,-18.8633550635714,
-12.7142604510224));
#71570=CARTESIAN_POINT('Ctrl Pts',(-20.8489910909365,-18.859723811226,-12.7144807759306));
#71571=CARTESIAN_POINT('Ctrl Pts',(-20.8485986130547,-18.8510693566604,
-12.7150071901784));
#71572=CARTESIAN_POINT('Ctrl Pts',(-20.8483528940849,-18.846046580164,-12.7153137543883));
#71573=CARTESIAN_POINT('Ctrl Pts',(-20.8474631299072,-18.8290964806147,
-12.716351735142));
#71574=CARTESIAN_POINT('Ctrl Pts',(-20.8467360486436,-18.8171740001958,
-12.7170875791991));
#71575=CARTESIAN_POINT('Ctrl Pts',(-20.8368861065989,-18.6754132077932,
-12.7259001726146));
#71576=CARTESIAN_POINT('Ctrl Pts',(-20.8159094459839,-18.5466897737048,
-12.7345169939419));
#71577=CARTESIAN_POINT('Ctrl Pts',(-20.742511607016,-18.2635785876856,-12.7538436953377));
#71578=CARTESIAN_POINT('Ctrl Pts',(-20.68382371734,-18.1116136822067,-12.7644503905451));
#71579=CARTESIAN_POINT('Ctrl Pts',(-20.5973010332701,-17.9468329361202,
-12.7759142878588));
#71580=CARTESIAN_POINT('Ctrl Pts',(-20.5859221280117,-17.9260194590116,
-12.7773628960543));
#71581=CARTESIAN_POINT('Ctrl Pts',(-20.5694163735905,-17.8969980170267,
-12.7793843750634));
#71582=CARTESIAN_POINT('Ctrl Pts',(-20.5645797181732,-17.8886278408834,
-12.7799675916828));
#71583=CARTESIAN_POINT('Ctrl Pts',(-20.5566540403871,-17.8751262304901,
-12.7809087582783));
#71584=CARTESIAN_POINT('Ctrl Pts',(-20.5536003185196,-17.8699743309944,
-12.7812679813822));
#71585=CARTESIAN_POINT('Ctrl Pts',(-20.5471835197496,-17.8592526114134,
-12.782015798378));
#71586=CARTESIAN_POINT('Ctrl Pts',(-20.5438165410143,-17.8536851904471,
-12.7824042448905));
#71587=CARTESIAN_POINT('Ctrl Pts',(-20.5357843190278,-17.8405408512395,
-12.7833217022563));
#71588=CARTESIAN_POINT('Ctrl Pts',(-20.5310968440375,-17.832977610371,-12.7838498904967));
#71589=CARTESIAN_POINT('Ctrl Pts',(-20.5153272651458,-17.8078880526529,
-12.7856031948381));
#71590=CARTESIAN_POINT('Ctrl Pts',(-20.5040351435845,-17.7904946796791,
-12.7868205349196));
#71591=CARTESIAN_POINT('Ctrl Pts',(-20.442391612741,-17.6985317796352,-12.7932716438279));
#71592=CARTESIAN_POINT('Ctrl Pts',(-20.3875775967268,-17.6270591357007,
-12.7983324571827));
#71593=CARTESIAN_POINT('Ctrl Pts',(-20.239226675372,-17.4572274408571,-12.8107698012182));
#71594=CARTESIAN_POINT('Ctrl Pts',(-20.1404888688135,-17.3639700355569,
-12.8179823280751));
#71595=CARTESIAN_POINT('Ctrl Pts',(-19.9740075103769,-17.234515345521,-12.8296580700672));
#71596=CARTESIAN_POINT('Ctrl Pts',(-19.9120725274929,-17.1914561278076,
-12.833918237911));
#71597=CARTESIAN_POINT('Ctrl Pts',(-19.8399118466703,-17.1468024930102,
-12.8389476021337));
#71598=CARTESIAN_POINT('Ctrl Pts',(-19.8318090219815,-17.1418634318041,
-12.8395132495199));
#71599=CARTESIAN_POINT('Ctrl Pts',(-19.8197472544567,-17.1346219792095,
-12.8403570256971));
#71600=CARTESIAN_POINT('Ctrl Pts',(-19.8158134764321,-17.1322776111949,
-12.8406324869893));
#71601=CARTESIAN_POINT('Ctrl Pts',(-19.8087980622483,-17.1281275037412,
-12.8411242847666));
#71602=CARTESIAN_POINT('Ctrl Pts',(-19.8057194325292,-17.126316781331,-12.8413402927544));
#71603=CARTESIAN_POINT('Ctrl Pts',(-19.7990873153699,-17.1224386012612,
-12.8418060471112));
#71604=CARTESIAN_POINT('Ctrl Pts',(-19.795532435717,-17.1203737312504,-12.8420559494402));
#71605=CARTESIAN_POINT('Ctrl Pts',(-19.7856953558016,-17.1146980697889,
-12.8427481304321));
#71606=CARTESIAN_POINT('Ctrl Pts',(-19.7794006661124,-17.1111091971637,
-12.8431917827522));
#71607=CARTESIAN_POINT('Ctrl Pts',(-19.7446834628047,-17.0915509136805,
-12.8456421382928));
#71608=CARTESIAN_POINT('Ctrl Pts',(-19.7159150516618,-17.0762083203526,
-12.8476853299662));
#71609=CARTESIAN_POINT('Ctrl Pts',(-19.5415619113382,-16.9883331863171,
-12.8600927436671));
#71610=CARTESIAN_POINT('Ctrl Pts',(-19.3883700340201,-16.9321130246887,
-12.871045822317));
#71611=CARTESIAN_POINT('Ctrl Pts',(-19.1167156872076,-16.8666084178378,
-12.8892985597815));
#71612=CARTESIAN_POINT('Ctrl Pts',(-19.001093166878,-16.8486696905022,-12.8967380863076));
#71613=CARTESIAN_POINT('Ctrl Pts',(-18.8703108069129,-16.8393446703619,
-12.904743920682));
#71614=CARTESIAN_POINT('Ctrl Pts',(-18.8560477180726,-16.8384727235829,
-12.9056118806448));
#71615=CARTESIAN_POINT('Ctrl Pts',(-18.833333140478,-16.8373148213725,-12.9069861686449));
#71616=CARTESIAN_POINT('Ctrl Pts',(-18.8248870704841,-16.8369349841761,
-12.9074954246141));
#71617=CARTESIAN_POINT('Ctrl Pts',(-18.8099870466371,-16.836354316576,-12.9083907973364));
#71618=CARTESIAN_POINT('Ctrl Pts',(-18.80353406734,-16.8361323992369,-12.9087775701918));
#71619=CARTESIAN_POINT('Ctrl Pts',(-18.7901850928668,-16.8357344639777,
-12.9095756399051));
#71620=CARTESIAN_POINT('Ctrl Pts',(-18.7832890427834,-16.835562621855,-12.9099868013696));
#71621=CARTESIAN_POINT('Ctrl Pts',(-18.7655855904696,-16.8352080450825,
-12.9110395209943));
#71622=CARTESIAN_POINT('Ctrl Pts',(-18.7547773213561,-16.8350743661137,
-12.9116795377962));
#71623=CARTESIAN_POINT('Ctrl Pts',(-18.7096623972587,-16.8348619304664,
-12.9143402810845));
#71624=CARTESIAN_POINT('Ctrl Pts',(-18.675356274072,-16.8355343058755,-12.9163374770723));
#71625=CARTESIAN_POINT('Ctrl Pts',(-18.586025601785,-16.8394590109449,-12.9214817691025));
#71626=CARTESIAN_POINT('Ctrl Pts',(-18.5310840017961,-16.8440266614322,
-12.9245894718428));
#71627=CARTESIAN_POINT('Ctrl Pts',(-18.3678441800644,-16.8640402229597,
-12.9337341331152));
#71628=CARTESIAN_POINT('Ctrl Pts',(-18.2604994115583,-16.8857366597852,
-12.9396223630923));
#71629=CARTESIAN_POINT('Ctrl Pts',(-18.1111156439335,-16.9281879776657,
-12.9480774751203));
#71630=CARTESIAN_POINT('Ctrl Pts',(-18.0673414866058,-16.9421825436189,
-12.9505897536701));
#71631=CARTESIAN_POINT('Ctrl Pts',(-18.0030660994603,-16.9650623657529,
-12.9543734436541));
#71632=CARTESIAN_POINT('Ctrl Pts',(-17.9821932981216,-16.9728658044634,
-12.9556173912177));
#71633=CARTESIAN_POINT('Ctrl Pts',(-17.9135904234385,-16.9997553035697,
-12.9597681002729));
#71634=CARTESIAN_POINT('Ctrl Pts',(-17.8664359112616,-17.020248758664,-12.962721747538));
#71635=CARTESIAN_POINT('Ctrl Pts',(-17.8129726159367,-17.045836415554,-12.9662396599061));
#71636=CARTESIAN_POINT('Ctrl Pts',(-17.8058862825645,-17.0492766948379,
-12.9667094508007));
#71637=CARTESIAN_POINT('Ctrl Pts',(-17.7946186733942,-17.0548248240846,
-12.9674623054615));
#71638=CARTESIAN_POINT('Ctrl Pts',(-17.7904248276733,-17.0569071742813,
-12.9677438240295));
#71639=CARTESIAN_POINT('Ctrl Pts',(-17.783025069199,-17.0606119934541,-12.9682429119953));
#71640=CARTESIAN_POINT('Ctrl Pts',(-17.7798163357228,-17.0622287320972,
-12.9684601214531));
#71641=CARTESIAN_POINT('Ctrl Pts',(-17.773041272701,-17.0656640411195,-12.9689204449763));
#71642=CARTESIAN_POINT('Ctrl Pts',(-17.7694760366275,-17.067484532087,-12.9691636739118));
#71643=CARTESIAN_POINT('Ctrl Pts',(-17.7599056496108,-17.0724056627488,
-12.9698192185863));
#71644=CARTESIAN_POINT('Ctrl Pts',(-17.7539102068058,-17.0755249347479,
-12.9702326821631));
#71645=CARTESIAN_POINT('Ctrl Pts',(-17.7247069458194,-17.0908967623459,
-12.9722599142832));
#71646=CARTESIAN_POINT('Ctrl Pts',(-17.7017145148158,-17.1035508497677,
-12.9738971246236));
#71647=CARTESIAN_POINT('Ctrl Pts',(-17.6365311652177,-17.1410205074514,
-12.9786448345478));
#71648=CARTESIAN_POINT('Ctrl Pts',(-17.5949591811586,-17.1668753695485,
-12.981802899346));
#71649=CARTESIAN_POINT('Ctrl Pts',(-17.4740684623494,-17.248003791619,-12.9913032927301));
#71650=CARTESIAN_POINT('Ctrl Pts',(-17.3975970787466,-17.3072940718698,
-12.9977324466284));
#71651=CARTESIAN_POINT('Ctrl Pts',(-17.2201704804253,-17.4654283083501,
-13.0133683538123));
#71652=CARTESIAN_POINT('Ctrl Pts',(-17.1245185358063,-17.5695536261855,
-13.0224360245941));
#71653=CARTESIAN_POINT('Ctrl Pts',(-17.0313564301591,-17.6938673115821,
-13.0319214934546));
#71654=CARTESIAN_POINT('Ctrl Pts',(-17.0229070028756,-17.7053830746888,
-13.0327890432953));
#71655=CARTESIAN_POINT('Ctrl Pts',(-17.009643570878,-17.7238488080858,-13.0341628067136));
#71656=CARTESIAN_POINT('Ctrl Pts',(-17.0047536494184,-17.7307434720371,
-13.0346719447464));
#71657=CARTESIAN_POINT('Ctrl Pts',(-16.9962016461544,-17.7429559287058,
-13.0355671802986));
#71658=CARTESIAN_POINT('Ctrl Pts',(-16.9925223775489,-17.7482614997871,
-13.0359539332874));
#71659=CARTESIAN_POINT('Ctrl Pts',(-16.9849620115875,-17.75927089851,-13.0367520292356));
#71660=CARTESIAN_POINT('Ctrl Pts',(-16.9810844044168,-17.7649770385774,
-13.0371632364698));
#71661=CARTESIAN_POINT('Ctrl Pts',(-16.9712013629442,-17.7796745876409,
-13.0382162124839));
#71662=CARTESIAN_POINT('Ctrl Pts',(-16.9652367467791,-17.7886933044593,
-13.0388564384312));
#71663=CARTESIAN_POINT('Ctrl Pts',(-16.9406197290176,-17.8265421970063,
-13.0415192153238));
#71664=CARTESIAN_POINT('Ctrl Pts',(-16.9226004333516,-17.8557792787245,
-13.0435181898367));
#71665=CARTESIAN_POINT('Ctrl Pts',(-16.8775013031238,-17.933105482106,-13.0486680993282));
#71666=CARTESIAN_POINT('Ctrl Pts',(-16.8515757658105,-17.9818386215875,
-13.0517795280847));
#71667=CARTESIAN_POINT('Ctrl Pts',(-16.7800131128559,-18.130054830611,-13.0609306890882));
#71668=CARTESIAN_POINT('Ctrl Pts',(-16.7401514618464,-18.2321198014625,
-13.0668217145879));
#71669=CARTESIAN_POINT('Ctrl Pts',(-16.6935607463832,-18.3855290571819,
-13.075550953093));
#71670=CARTESIAN_POINT('Ctrl Pts',(-16.6805271426218,-18.4347664445024,
-13.0783364533726));
#71671=CARTESIAN_POINT('Ctrl Pts',(-16.6658114747131,-18.4997477630116,
-13.082043323072));
#71672=CARTESIAN_POINT('Ctrl Pts',(-16.6625120047518,-18.5151094757731,
-13.082921877604));
#71673=CARTESIAN_POINT('Ctrl Pts',(-16.6488821168603,-18.5821965500195,
-13.0867737710449));
#71674=CARTESIAN_POINT('Ctrl Pts',(-16.6403167696737,-18.6342568320332,
-13.0898017226383));
#71675=CARTESIAN_POINT('Ctrl Pts',(-16.6326149766286,-18.695201364635,-13.093447320796));
#71676=CARTESIAN_POINT('Ctrl Pts',(-16.6315783129447,-18.7038315098328,
-13.0939659067662));
#71677=CARTESIAN_POINT('Ctrl Pts',(-16.6300882632132,-18.7169160805514,
-13.0947560408225));
#71678=CARTESIAN_POINT('Ctrl Pts',(-16.6295957989882,-18.7213660838256,
-13.0950254410843));
#71679=CARTESIAN_POINT('Ctrl Pts',(-16.6287367226327,-18.7293607579082,
-13.0955107063885));
#71680=CARTESIAN_POINT('Ctrl Pts',(-16.6283649412955,-18.7329048188489,
-13.0957262773786));
#71681=CARTESIAN_POINT('Ctrl Pts',(-16.6275760434057,-18.740612617913,-13.0961961048509));
#71682=CARTESIAN_POINT('Ctrl Pts',(-16.6271623284955,-18.7447766049649,
-13.0964505442747));
#71683=CARTESIAN_POINT('Ctrl Pts',(-16.6260337078267,-18.7564888772883,
-13.0971679225));
#71684=CARTESIAN_POINT('Ctrl Pts',(-16.6253470129127,-18.7640397273437,
-13.0976324004455));
#71685=CARTESIAN_POINT('Ctrl Pts',(-16.6214621617039,-18.8094612311245,
-13.1004377094568));
#71686=CARTESIAN_POINT('Ctrl Pts',(-16.6192439523349,-18.8474062032782,
-13.1028282950644));
#71687=CARTESIAN_POINT('Ctrl Pts',(-16.6152879487766,-18.973068866035,-13.1108564905582));
#71688=CARTESIAN_POINT('Ctrl Pts',(-16.6179805347711,-19.0608317096103,
-13.1166390871901));
#71689=CARTESIAN_POINT('Ctrl Pts',(-16.6422708687808,-19.3218393588444,
-13.1339594423221));
#71690=CARTESIAN_POINT('Ctrl Pts',(-16.6798383271981,-19.4928833380346,
-13.145406598618));
#71691=CARTESIAN_POINT('Ctrl Pts',(-16.7456646104199,-19.67914744913,-13.1575672761188));
#71692=CARTESIAN_POINT('Ctrl Pts',(-16.7537054664638,-19.7007687631953,
-13.158975435354));
#71693=CARTESIAN_POINT('Ctrl Pts',(-16.7655761013795,-19.7311583401141,
-13.1609504653947));
#71694=CARTESIAN_POINT('Ctrl Pts',(-16.7691141698648,-19.7400380973349,
-13.1615270559426));
#71695=CARTESIAN_POINT('Ctrl Pts',(-16.7749592022607,-19.7544236924032,
-13.1624604132948));
#71696=CARTESIAN_POINT('Ctrl Pts',(-16.7772294963945,-19.7599441977579,
-13.1628184123042));
#71697=CARTESIAN_POINT('Ctrl Pts',(-16.7820294182413,-19.77147690137,-13.1635659507681));
#71698=CARTESIAN_POINT('Ctrl Pts',(-16.7845635475733,-19.7774871672829,
-13.1639553328692));
#71699=CARTESIAN_POINT('Ctrl Pts',(-16.7906560133211,-19.7917523156977,
-13.1648790958912));
#71700=CARTESIAN_POINT('Ctrl Pts',(-16.7942392469403,-19.7999964781566,
-13.1654126227249));
#71701=CARTESIAN_POINT('Ctrl Pts',(-16.8064770449228,-19.8276692399912,
-13.1672025492852));
#71702=CARTESIAN_POINT('Ctrl Pts',(-16.8153720304585,-19.8469905715973,
-13.1684507132827));
#71703=CARTESIAN_POINT('Ctrl Pts',(-16.8912568177799,-20.0054915855231,
-13.1786847429151));
#71704=CARTESIAN_POINT('Ctrl Pts',(-16.9730038171536,-20.1370936072568,
-13.1871021016205));
#71705=CARTESIAN_POINT('Ctrl Pts',(-17.1527707598866,-20.3662522671283,
-13.2029188009421));
#71706=CARTESIAN_POINT('Ctrl Pts',(-17.2474062788223,-20.4654147187232,
-13.2103043431566));
#71707=CARTESIAN_POINT('Ctrl Pts',(-17.3627250384739,-20.564928057284,-13.2192364843212));
#71708=CARTESIAN_POINT('Ctrl Pts',(-17.3746370055784,-20.5749800231576,
-13.220158591548));
#71709=CARTESIAN_POINT('Ctrl Pts',(-17.3911125432161,-20.5885743563221,
-13.2214349466975));
#71710=CARTESIAN_POINT('Ctrl Pts',(-17.3955815638066,-20.592231213347,-13.2217812578595));
#71711=CARTESIAN_POINT('Ctrl Pts',(-17.4027117868424,-20.5980171044354,
-13.2223340458817));
#71712=CARTESIAN_POINT('Ctrl Pts',(-17.405363303654,-20.60015810629,-13.2225396671707));
#71713=CARTESIAN_POINT('Ctrl Pts',(-17.4108543852708,-20.6045700901351,
-13.2229656352164));
#71714=CARTESIAN_POINT('Ctrl Pts',(-17.4136946266629,-20.6068401557086,
-13.2231860471924));
#71715=CARTESIAN_POINT('Ctrl Pts',(-17.4204832407508,-20.6122373601705,
-13.2237130354384));
#71716=CARTESIAN_POINT('Ctrl Pts',(-17.4244369408101,-20.61535773715,-13.2240200893119));
#71717=CARTESIAN_POINT('Ctrl Pts',(-17.4378410712935,-20.6258592605778,
-13.2250614320295));
#71718=CARTESIAN_POINT('Ctrl Pts',(-17.447342866729,-20.6331740536974,-13.2258001867073));
#71719=CARTESIAN_POINT('Ctrl Pts',(-17.5586170524809,-20.7173406948873,
-13.2344532828878));
#71720=CARTESIAN_POINT('Ctrl Pts',(-17.6670612857956,-20.7849178593191,
-13.242886595689));
#71721=CARTESIAN_POINT('Ctrl Pts',(-17.9282980499113,-20.9166318025306,
-13.2622203688515));
#71722=CARTESIAN_POINT('Ctrl Pts',(-18.0838969379994,-20.9734646777314,
-13.2730158444569));
#71723=CARTESIAN_POINT('Ctrl Pts',(-18.2675087243459,-21.0170985742589,
-13.2846392240358));
#71724=CARTESIAN_POINT('Ctrl Pts',(-18.2905652612627,-21.0221719578198,
-13.286080842425));
#71725=CARTESIAN_POINT('Ctrl Pts',(-18.323158548674,-21.0287742742223,-13.2880942884745));
#71726=CARTESIAN_POINT('Ctrl Pts',(-18.3326276132522,-21.0306250975529,
-13.2886763525564));
#71727=CARTESIAN_POINT('Ctrl Pts',(-18.347991065657,-21.0335191393526,-13.2896161597697));
#71728=CARTESIAN_POINT('Ctrl Pts',(-18.3538777260398,-21.0346021902578,
-13.2899751688801));
#71729=CARTESIAN_POINT('Ctrl Pts',(-18.3661754505193,-21.0368108950247,
-13.2907229307289));
#71730=CARTESIAN_POINT('Ctrl Pts',(-18.3725872800356,-21.0379319774436,
-13.2911115343753));
#71731=CARTESIAN_POINT('Ctrl Pts',(-18.3877913579037,-21.0405181406197,
-13.292030061354));
#71732=CARTESIAN_POINT('Ctrl Pts',(-18.3965879341658,-21.041957307959,-13.2925591567417));
#71733=CARTESIAN_POINT('Ctrl Pts',(-18.4253810101607,-21.0464814836454,
-13.2942835669587));
#71734=CARTESIAN_POINT('Ctrl Pts',(-18.4454130618968,-21.0493354493858,
-13.2954715701017));
#71735=CARTESIAN_POINT('Ctrl Pts',(-18.4930790423714,-21.0554305453066,
-13.2982725966207));
#71736=CARTESIAN_POINT('Ctrl Pts',(-18.5207423175308,-21.0584150179696,
-13.2998776609134));
#71737=CARTESIAN_POINT('Ctrl Pts',(-18.7171650100066,-21.0756968227674,
-13.3111483189815));
#71738=CARTESIAN_POINT('Ctrl Pts',(-18.8870389590356,-21.0702429782238,
-13.3201754913812));
#71739=CARTESIAN_POINT('Ctrl Pts',(-19.1572101688511,-21.0288698788889,
-13.3351123390378));
#71740=CARTESIAN_POINT('Ctrl Pts',(-19.2586540326935,-21.0055889673471,
-13.3408766595485));
#71741=CARTESIAN_POINT('Ctrl Pts',(-19.3672203705736,-20.972102674751,-13.3476076668997));
#71742=CARTESIAN_POINT('Ctrl Pts',(-19.376457946993,-20.96918383707,-13.3481849790797));
#71743=CARTESIAN_POINT('Ctrl Pts',(-19.3900688505813,-20.964780164466,-13.3490428475197));
#71744=CARTESIAN_POINT('Ctrl Pts',(-19.394458024889,-20.9633442081365,-13.349320605287));
#71745=CARTESIAN_POINT('Ctrl Pts',(-19.4022370962683,-20.9607710093327,
-13.3498149256466));
#71746=CARTESIAN_POINT('Ctrl Pts',(-19.4056288476265,-20.9596395282995,
-13.3500311467298));
#71747=CARTESIAN_POINT('Ctrl Pts',(-19.4128905108622,-20.9571965913209,
-13.3504955737299));
#71748=CARTESIAN_POINT('Ctrl Pts',(-19.4167594388522,-20.9558825423636,
-13.3507439262314));
#71749=CARTESIAN_POINT('Ctrl Pts',(-19.4273710673343,-20.9522440926401,
-13.3514275598349));
#71750=CARTESIAN_POINT('Ctrl Pts',(-19.4341057912877,-20.9498968303757,
-13.3518641603594));
#71751=CARTESIAN_POINT('Ctrl Pts',(-19.4695225158455,-20.9373519286973,
-13.3541740836137));
#71752=CARTESIAN_POINT('Ctrl Pts',(-19.4979923761602,-20.9265711124939,
-13.3560791089139));
#71753=CARTESIAN_POINT('Ctrl Pts',(-19.6765789912471,-20.8545046253558,
-13.3682925365836));
#71754=CARTESIAN_POINT('Ctrl Pts',(-19.8194665385398,-20.7767576930581,
-13.3792085257959));
#71755=CARTESIAN_POINT('Ctrl Pts',(-20.0499070462781,-20.6146438519663,
-13.3976307853898));
#71756=CARTESIAN_POINT('Ctrl Pts',(-20.1417395844055,-20.5376460977423,
-13.4052584023651));
#71757=CARTESIAN_POINT('Ctrl Pts',(-20.2377288059876,-20.4422132330214,
-13.4135235941648));
#71758=CARTESIAN_POINT('Ctrl Pts',(-20.248746231174,-20.4310130756201,-13.414477400804));
#71759=CARTESIAN_POINT('Ctrl Pts',(-20.2652268079093,-20.413881815592,-13.4159123286463));
#71760=CARTESIAN_POINT('Ctrl Pts',(-20.2707822499913,-20.4080406240678,
-13.4163974664898));
#71761=CARTESIAN_POINT('Ctrl Pts',(-20.2806777374817,-20.3975164263434,
-13.4172642559059));
#71762=CARTESIAN_POINT('Ctrl Pts',(-20.285030193926,-20.3928452732211,-13.4176464401603));
#71763=CARTESIAN_POINT('Ctrl Pts',(-20.2942209517347,-20.3828916427895,
-13.418455499241));
#71764=CARTESIAN_POINT('Ctrl Pts',(-20.2990537165217,-20.3776041449064,
-13.4188821352738));
#71765=CARTESIAN_POINT('Ctrl Pts',(-20.3088371006349,-20.3667904970008,
-13.4197483457089));
#71766=CARTESIAN_POINT('Ctrl Pts',(-20.3137856956804,-20.3612626447143,
-13.4201878318702));
#71767=CARTESIAN_POINT('Ctrl Pts',(-20.3355743450282,-20.3366645339933,
-13.4221290260871));
#71768=CARTESIAN_POINT('Ctrl Pts',(-20.352099346437,-20.3173171212203,-13.4236176279517));
#71769=CARTESIAN_POINT('Ctrl Pts',(-20.4222713864287,-20.232095851272,-13.4300187482448));
#71770=CARTESIAN_POINT('Ctrl Pts',(-20.4722775149361,-20.1633212406356,
-13.4347859723443));
#71771=CARTESIAN_POINT('Ctrl Pts',(-20.5551898505232,-20.0335375724555,
-13.443273618919));
#71772=CARTESIAN_POINT('Ctrl Pts',(-20.5894925668684,-19.9735692243239,
-13.4470187497232));
#71773=CARTESIAN_POINT('Ctrl Pts',(-20.6594230944977,-19.8361307617998,
-13.4553933615768));
#71774=CARTESIAN_POINT('Ctrl Pts',(-20.6934048684955,-19.7580131654387,
-13.4600146201655));
#71775=CARTESIAN_POINT('Ctrl Pts',(-20.7225805467356,-19.6781104662135,
-13.4647889080502));
#71776=CARTESIAN_POINT('',(-20.8509991540683,-18.9538925310889,-12.4890563034253));
#71777=CARTESIAN_POINT('Ctrl Pts',(-20.7225805821191,-19.6781103693095,
-13.2445592932782));
#71778=CARTESIAN_POINT('Ctrl Pts',(-20.6962607934143,-19.7501917262988,
-13.2399327166672));
#71779=CARTESIAN_POINT('Ctrl Pts',(-20.6660544015046,-19.8207403796103,
-13.2353061400562));
#71780=CARTESIAN_POINT('Ctrl Pts',(-20.632174183212,-19.8893493319929,-13.2306795634452));
#71781=CARTESIAN_POINT('Ctrl Pts',(-20.6214444202636,-19.9110775802836,
-13.2292143405865));
#71782=CARTESIAN_POINT('Ctrl Pts',(-20.6103465168557,-19.9326114901367,
-13.2277491177279));
#71783=CARTESIAN_POINT('Ctrl Pts',(-20.5988881380091,-19.953938737006,-13.2262838948692));
#71784=CARTESIAN_POINT('Ctrl Pts',(-20.5645713376047,-20.017811897754,-13.2218956859383));
#71785=CARTESIAN_POINT('Ctrl Pts',(-20.526902233303,-20.0800446523181,-13.2175074770074));
#71786=CARTESIAN_POINT('Ctrl Pts',(-20.4860618340581,-20.1402627359456,
-13.2131192680765));
#71787=CARTESIAN_POINT('Ctrl Pts',(-20.4452820487372,-20.2003914459526,
-13.2087375719752));
#71788=CARTESIAN_POINT('Ctrl Pts',(-20.4013405804882,-20.2585110248676,
-13.2043558758739));
#71789=CARTESIAN_POINT('Ctrl Pts',(-20.3544642120277,-20.3142719029391,
-13.1999741797727));
#71790=CARTESIAN_POINT('Ctrl Pts',(-20.3076429270307,-20.3699672575413,
-13.195597632513));
#71791=CARTESIAN_POINT('Ctrl Pts',(-20.2578939016345,-20.4233090498181,
-13.1912210852534));
#71792=CARTESIAN_POINT('Ctrl Pts',(-20.2054860875596,-20.4739782173601,
-13.1868445379937));
#71793=CARTESIAN_POINT('Ctrl Pts',(-20.1531115097586,-20.5246152512524,
-13.1824707662767));
#71794=CARTESIAN_POINT('Ctrl Pts',(-20.0980818347927,-20.5725826889237,
-13.1780969945598));
#71795=CARTESIAN_POINT('Ctrl Pts',(-20.040704044844,-20.6175970518671,-13.1737232228428));
#71796=CARTESIAN_POINT('Ctrl Pts',(-19.9833437151495,-20.6625977167886,
-13.1693507820792));
#71797=CARTESIAN_POINT('Ctrl Pts',(-19.9236370683463,-20.7046467934755,
-13.1649783413157));
#71798=CARTESIAN_POINT('Ctrl Pts',(-19.8619241653156,-20.743501068182,-13.1606059005521));
#71799=CARTESIAN_POINT('Ctrl Pts',(-19.8002096842791,-20.7823563363966,
-13.1562333479848));
#71800=CARTESIAN_POINT('Ctrl Pts',(-19.7364892544385,-20.8180163851247,
-13.1518607954174));
#71801=CARTESIAN_POINT('Ctrl Pts',(-19.671130479885,-20.8502822402558,-13.1474882428501));
#71802=CARTESIAN_POINT('Ctrl Pts',(-19.60570387353,-20.8825815821084,-13.1431111522827));
#71803=CARTESIAN_POINT('Ctrl Pts',(-19.538635961093,-20.9114794832209,-13.1387340617154));
#71804=CARTESIAN_POINT('Ctrl Pts',(-19.4703166749595,-20.9368241116473,
-13.1343569711481));
#71805=CARTESIAN_POINT('Ctrl Pts',(-19.4019600771282,-20.9621825817159,
-13.1299774900891));
#71806=CARTESIAN_POINT('Ctrl Pts',(-19.3323512055625,-20.9839837711616,
-13.1255980090302));
#71807=CARTESIAN_POINT('Ctrl Pts',(-19.2618949953259,-21.0021258190438,
-13.1212185279712));
#71808=CARTESIAN_POINT('Ctrl Pts',(-19.1913139019297,-21.020300023584,-13.1168312843115));
#71809=CARTESIAN_POINT('Ctrl Pts',(-19.1198829437752,-21.0348020386143,
-13.1124440406518));
#71810=CARTESIAN_POINT('Ctrl Pts',(-19.048016498307,-21.0455812950041,-13.1080567969921));
#71811=CARTESIAN_POINT('Ctrl Pts',(-18.9991542404236,-21.0529101506624,
-13.1050738940573));
#71812=CARTESIAN_POINT('Ctrl Pts',(-18.9500908178362,-21.0585191746184,
-13.1020909911225));
#71813=CARTESIAN_POINT('Ctrl Pts',(-18.900956661124,-21.0624062341896,-13.0991080881877));
#71814=CARTESIAN_POINT('Ctrl Pts',(-18.8286744078926,-21.0681245662636,
-13.0947198792568));
#71815=CARTESIAN_POINT('Ctrl Pts',(-18.7559569381437,-21.0701362205188,
-13.0903316703259));
#71816=CARTESIAN_POINT('Ctrl Pts',(-18.6832169260197,-21.0683908144285,
-13.085943461395));
#71817=CARTESIAN_POINT('Ctrl Pts',(-18.6105848721342,-21.0666479988102,
-13.0815617652938));
#71818=CARTESIAN_POINT('Ctrl Pts',(-18.5379308205422,-21.0611592036425,
-13.0771800691925));
#71819=CARTESIAN_POINT('Ctrl Pts',(-18.4656714572673,-21.0519259018249,
-13.0727983730912));
#71820=CARTESIAN_POINT('Ctrl Pts',(-18.3934970044949,-21.0427034498716,
-13.0684218258316));
#71821=CARTESIAN_POINT('Ctrl Pts',(-18.3217167948298,-21.0297452929197,
-13.064045278572));
#71822=CARTESIAN_POINT('Ctrl Pts',(-18.2507446877307,-21.0131048743729,
-13.0596687313123));
#71823=CARTESIAN_POINT('Ctrl Pts',(-18.1798175901105,-20.9964750089376,
-13.0552949595953));
#71824=CARTESIAN_POINT('Ctrl Pts',(-18.1096980467018,-20.9761676251632,
-13.0509211878784));
#71825=CARTESIAN_POINT('Ctrl Pts',(-18.0407905817005,-20.9522874049448,
-13.0465474161614));
#71826=CARTESIAN_POINT('Ctrl Pts',(-17.9719040854722,-20.9284144515577,
-13.0421749753979));
#71827=CARTESIAN_POINT('Ctrl Pts',(-17.9042293909008,-20.9009709780647,
-13.0378025346343));
#71828=CARTESIAN_POINT('Ctrl Pts',(-17.8381550707622,-20.8701112748636,
-13.0334300938708));
#71829=CARTESIAN_POINT('Ctrl Pts',(-17.7720790610959,-20.8392507825765,
-13.0290575413034));
#71830=CARTESIAN_POINT('Ctrl Pts',(-17.7076039433215,-20.8049740930874,
-13.0246849887361));
#71831=CARTESIAN_POINT('Ctrl Pts',(-17.6450960002999,-20.7674826023504,
-13.0203124361687));
#71832=CARTESIAN_POINT('Ctrl Pts',(-17.5825231841773,-20.7299522015302,
-13.0159353456014));
#71833=CARTESIAN_POINT('Ctrl Pts',(-17.5219220335751,-20.6892005866782,
-13.0115582550341));
#71834=CARTESIAN_POINT('Ctrl Pts',(-17.4636312781366,-20.6454734454698,
-13.0071811644667));
#71835=CARTESIAN_POINT('Ctrl Pts',(-17.4053086879532,-20.6017224232466,
-13.0028016834078));
#71836=CARTESIAN_POINT('Ctrl Pts',(-17.3492993758005,-20.5549929484573,
-12.9984222023489));
#71837=CARTESIAN_POINT('Ctrl Pts',(-17.2959081742796,-20.5055703720129,
-12.9940427212899));
#71838=CARTESIAN_POINT('Ctrl Pts',(-17.2424223372125,-20.4560601943835,
-12.9896554776302));
#71839=CARTESIAN_POINT('Ctrl Pts',(-17.1915642147118,-20.4038477284533,
-12.9852682339705));
#71840=CARTESIAN_POINT('Ctrl Pts',(-17.1436006220654,-20.3492540279653,
-12.9808809903108));
#71841=CARTESIAN_POINT('Ctrl Pts',(-17.1109900008266,-20.3121355722699,
-12.9778980873759));
#71842=CARTESIAN_POINT('Ctrl Pts',(-17.0797165992413,-20.2739170566122,
-12.9749151844411));
#71843=CARTESIAN_POINT('Ctrl Pts',(-17.0498528101568,-20.2347069980877,
-12.9719322815063));
#71844=CARTESIAN_POINT('Ctrl Pts',(-17.0059195850955,-20.1770242867296,
-12.9675440725754));
#71845=CARTESIAN_POINT('Ctrl Pts',(-16.9648675150388,-20.1169692727541,
-12.9631558636445));
#71846=CARTESIAN_POINT('Ctrl Pts',(-16.926962336405,-20.0548616787018,-12.9587676547136));
#71847=CARTESIAN_POINT('Ctrl Pts',(-16.889113415341,-19.9928462626167,-12.9543859586124));
#71848=CARTESIAN_POINT('Ctrl Pts',(-16.8544023633226,-19.9287847222598,
-12.9500042625111));
#71849=CARTESIAN_POINT('Ctrl Pts',(-16.8230534861162,-19.8630282218873,
-12.9456225664098));
#71850=CARTESIAN_POINT('Ctrl Pts',(-16.7917414463352,-19.7973489906359,
-12.9412460191502));
#71851=CARTESIAN_POINT('Ctrl Pts',(-16.7637839395866,-19.7299791891848,
-12.9368694718905));
#71852=CARTESIAN_POINT('Ctrl Pts',(-16.739360042701,-19.661295735745,-12.9324929246309));
#71853=CARTESIAN_POINT('Ctrl Pts',(-16.7149516350957,-19.5926558403531,
-12.9281191529139));
#71854=CARTESIAN_POINT('Ctrl Pts',(-16.6940725522121,-19.5227043993277,
-12.9237453811969));
#71855=CARTESIAN_POINT('Ctrl Pts',(-16.6768537344171,-19.4518382158243,
-12.91937160948));
#71856=CARTESIAN_POINT('Ctrl Pts',(-16.6596401563663,-19.3809935971386,
-12.9149991687164));
#71857=CARTESIAN_POINT('Ctrl Pts',(-16.6460847459306,-19.3092352570616,
-12.9106267279528));
#71858=CARTESIAN_POINT('Ctrl Pts',(-16.6362680963764,-19.2369734382706,
-12.9062542871893));
#71859=CARTESIAN_POINT('Ctrl Pts',(-16.6264511958094,-19.164709771737,-12.9018817346219));
#71860=CARTESIAN_POINT('Ctrl Pts',(-16.620373308882,-19.0919430791857,-12.8975091820546));
#71861=CARTESIAN_POINT('Ctrl Pts',(-16.6180633554341,-19.0190903583474,
-12.8931366294872));
#71862=CARTESIAN_POINT('Ctrl Pts',(-16.6157510046294,-18.9461620282075,
-12.8887595389199));
#71863=CARTESIAN_POINT('Ctrl Pts',(-16.6172144102078,-18.8731479746871,
-12.8843824483526));
#71864=CARTESIAN_POINT('Ctrl Pts',(-16.6224303356468,-18.8004660018901,
-12.8800053577853));
#71865=CARTESIAN_POINT('Ctrl Pts',(-16.6276491096962,-18.7277443347702,
-12.8756258767263));
#71866=CARTESIAN_POINT('Ctrl Pts',(-16.6366244245267,-18.6553555885067,
-12.8712463956674));
#71867=CARTESIAN_POINT('Ctrl Pts',(-16.6492813452851,-18.5837105341124,
-12.8668669146084));
#71868=CARTESIAN_POINT('Ctrl Pts',(-16.6619607003506,-18.5119384893401,
-12.8624796709487));
#71869=CARTESIAN_POINT('Ctrl Pts',(-16.6783345842871,-18.4409132392692,
-12.858092427289));
#71870=CARTESIAN_POINT('Ctrl Pts',(-16.6982774637591,-18.3710329136339,
-12.8537051836292));
#71871=CARTESIAN_POINT('Ctrl Pts',(-16.7118367001087,-18.3235210258541,
-12.8507222806944));
#71872=CARTESIAN_POINT('Ctrl Pts',(-16.7270447244344,-18.27653808659,-12.8477393777596));
#71873=CARTESIAN_POINT('Ctrl Pts',(-16.7438494759073,-18.2302037050153,
-12.8447564748248));
#71874=CARTESIAN_POINT('Ctrl Pts',(-16.7685712862064,-18.1620402577033,
-12.8403682658939));
#71875=CARTESIAN_POINT('Ctrl Pts',(-16.7968473421401,-18.0950153233851,
-12.835980056963));
#71876=CARTESIAN_POINT('Ctrl Pts',(-16.8285526457323,-18.0295254040819,
-12.8315918480321));
#71877=CARTESIAN_POINT('Ctrl Pts',(-16.8602108933972,-17.9641326826773,
-12.8272101519309));
#71878=CARTESIAN_POINT('Ctrl Pts',(-16.8952880767684,-17.9002708843009,
-12.8228284558296));
#71879=CARTESIAN_POINT('Ctrl Pts',(-16.9336103347364,-17.8383186931567,
-12.8184467597283));
#71880=CARTESIAN_POINT('Ctrl Pts',(-16.9718875610016,-17.7764393007675,
-12.8140702124687));
#71881=CARTESIAN_POINT('Ctrl Pts',(-17.0134020343727,-17.7164654662072,
-12.8096936652091));
#71882=CARTESIAN_POINT('Ctrl Pts',(-17.057933757175,-17.6587517834296,-12.8053171179494));
#71883=CARTESIAN_POINT('Ctrl Pts',(-17.1024372386059,-17.6010747018308,
-12.8009433462325));
#71884=CARTESIAN_POINT('Ctrl Pts',(-17.149953878891,-17.5456553090191,-12.7965695745155));
#71885=CARTESIAN_POINT('Ctrl Pts',(-17.2002209049089,-17.4928184871437,
-12.7921958027985));
#71886=CARTESIAN_POINT('Ctrl Pts',(-17.250472634502,-17.4399977436907,-12.787823362035));
#71887=CARTESIAN_POINT('Ctrl Pts',(-17.3034727559331,-17.3897583602254,
-12.7834509212714));
#71888=CARTESIAN_POINT('Ctrl Pts',(-17.3589199436392,-17.3423901595111,
-12.7790784805079));
#71889=CARTESIAN_POINT('Ctrl Pts',(-17.4143685491361,-17.2950207475866,
-12.7747059279405));
#71890=CARTESIAN_POINT('Ctrl Pts',(-17.4722639770754,-17.2505229759786,
-12.7703333753732));
#71891=CARTESIAN_POINT('Ctrl Pts',(-17.5322712521177,-17.2091468746583,
-12.7659608228059));
#71892=CARTESIAN_POINT('Ctrl Pts',(-17.5923408049735,-17.1677278316595,
-12.7615837322385));
#71893=CARTESIAN_POINT('Ctrl Pts',(-17.6545261829435,-17.1294372018124,
-12.7572066416712));
#71894=CARTESIAN_POINT('Ctrl Pts',(-17.7184635014064,-17.0944815963161,
-12.7528295511039));
#71895=CARTESIAN_POINT('Ctrl Pts',(-17.782435738412,-17.0595069002663,-12.7484500700449));
#71896=CARTESIAN_POINT('Ctrl Pts',(-17.8481613859395,-17.0278710642731,
-12.744070588986));
#71897=CARTESIAN_POINT('Ctrl Pts',(-17.9152544897584,-16.9997334225421,
-12.7396911079271));
#71898=CARTESIAN_POINT('Ctrl Pts',(-17.9824665156535,-16.97154590703,-12.7353038642674));
#71899=CARTESIAN_POINT('Ctrl Pts',(-18.0510503837931,-16.9468691314342,
-12.7309166206076));
#71900=CARTESIAN_POINT('Ctrl Pts',(-18.1206033812626,-16.9258130421598,
-12.7265293769479));
#71901=CARTESIAN_POINT('Ctrl Pts',(-18.1678927174312,-16.9114969304131,
-12.7235464740131));
#71902=CARTESIAN_POINT('Ctrl Pts',(-18.2156297492658,-16.8988534982272,
-12.7205635710783));
#71903=CARTESIAN_POINT('Ctrl Pts',(-18.2636857248404,-16.887903712861,-12.7175806681434));
#71904=CARTESIAN_POINT('Ctrl Pts',(-18.3343818439591,-16.8717952618032,
-12.7131924592126));
#71905=CARTESIAN_POINT('Ctrl Pts',(-18.4060444995739,-16.8592916243426,
-12.7088042502817));
#71906=CARTESIAN_POINT('Ctrl Pts',(-18.4782726371994,-16.8505023159863,
-12.7044160413508));
#71907=CARTESIAN_POINT('Ctrl Pts',(-18.5503935762929,-16.8417260524208,
-12.7000343452495));
#71908=CARTESIAN_POINT('Ctrl Pts',(-18.623077856446,-16.8366532323251,-12.6956526491482));
#71909=CARTESIAN_POINT('Ctrl Pts',(-18.6959129564504,-16.8353426405973,
-12.691270953047));
#71910=CARTESIAN_POINT('Ctrl Pts',(-18.768662469416,-16.8340335889191,-12.6868944057873));
#71911=CARTESIAN_POINT('Ctrl Pts',(-18.8415619702677,-16.8364779920626,
-12.6825178585277));
#71912=CARTESIAN_POINT('Ctrl Pts',(-18.9141942210373,-16.8426828017805,
-12.6781413112681));
#71913=CARTESIAN_POINT('Ctrl Pts',(-18.9867804094891,-16.8488836764982,
-12.6737675395511));
#71914=CARTESIAN_POINT('Ctrl Pts',(-19.0590992046967,-16.8588401850895,
-12.6693937678341));
#71915=CARTESIAN_POINT('Ctrl Pts',(-19.1307351980795,-16.8725072294896,
-12.6650199961172));
#71916=CARTESIAN_POINT('Ctrl Pts',(-19.202349392389,-16.8861701149623,-12.6606475553536));
#71917=CARTESIAN_POINT('Ctrl Pts',(-19.2732807238323,-16.9035412042303,
-12.6562751145901));
#71918=CARTESIAN_POINT('Ctrl Pts',(-19.3431223955191,-16.9245240057458,
-12.6519026738265));
#71919=CARTESIAN_POINT('Ctrl Pts',(-19.4129658530651,-16.9455073437939,
-12.6475301212592));
#71920=CARTESIAN_POINT('Ctrl Pts',(-19.4817191341323,-16.9701024367362,
-12.6431575686918));
#71921=CARTESIAN_POINT('Ctrl Pts',(-19.5489906872852,-16.9981629598049,
-12.6387850161245));
#71922=CARTESIAN_POINT('Ctrl Pts',(-19.6163320573932,-17.0262526051427,
-12.6344079255571));
#71923=CARTESIAN_POINT('Ctrl Pts',(-19.6821881831272,-17.0578146752691,
-12.6300308349898));
#71924=CARTESIAN_POINT('Ctrl Pts',(-19.746188373322,-17.0926550355268,-12.6256537444225));
#71925=CARTESIAN_POINT('Ctrl Pts',(-19.8102235163959,-17.1275144233983,
-12.6212742633636));
#71926=CARTESIAN_POINT('Ctrl Pts',(-19.8724002944077,-17.1656554136576,
-12.6168947823046));
#71927=CARTESIAN_POINT('Ctrl Pts',(-19.932375822801,-17.2068397244591,-12.6125153012457));
#71928=CARTESIAN_POINT('Ctrl Pts',(-19.9924576574157,-17.248097034175,-12.608128057586));
#71929=CARTESIAN_POINT('Ctrl Pts',(-20.0503300675354,-17.29240814305,-12.6037408139262));
#71930=CARTESIAN_POINT('Ctrl Pts',(-20.1056826247701,-17.3394939451575,
-12.5993535702665));
#71931=CARTESIAN_POINT('Ctrl Pts',(-20.1433170299302,-17.3715077534137,
-12.5963706673317));
#71932=CARTESIAN_POINT('Ctrl Pts',(-20.1797873054597,-17.4048033925969,
-12.5933877643969));
#71933=CARTESIAN_POINT('Ctrl Pts',(-20.2150061302366,-17.4392839518926,
-12.590404861462));
#71934=CARTESIAN_POINT('Ctrl Pts',(-20.2660558507877,-17.4892635559152,
-12.5860811407752));
#71935=CARTESIAN_POINT('Ctrl Pts',(-20.3146860821101,-17.5419415318573,
-12.5817574200883));
#71936=CARTESIAN_POINT('Ctrl Pts',(-20.3605919747976,-17.5970507214202,
-12.5774336994015));
#71937=CARTESIAN_POINT('Ctrl Pts',(-20.4064369112149,-17.652086734089,-12.5731157199795));
#71938=CARTESIAN_POINT('Ctrl Pts',(-20.4495643625502,-17.7095471849218,
-12.5687977405574));
#71939=CARTESIAN_POINT('Ctrl Pts',(-20.4897052944034,-17.7691272599286,
-12.5644797611354));
#71940=CARTESIAN_POINT('Ctrl Pts',(-20.5298070691322,-17.8286492150986,
-12.5601659938641));
#71941=CARTESIAN_POINT('Ctrl Pts',(-20.5669278234433,-17.8902862851976,
-12.5558522265929));
#71942=CARTESIAN_POINT('Ctrl Pts',(-20.6008391323988,-17.9537011200325,
-12.5515384593216));
#71943=CARTESIAN_POINT('Ctrl Pts',(-20.6347293023105,-18.0170764244271,
-12.5472273810918));
#71944=CARTESIAN_POINT('Ctrl Pts',(-20.6654137615195,-18.0822268576,-12.542916302862));
#71945=CARTESIAN_POINT('Ctrl Pts',(-20.6927087374024,-18.1487882707383,
-12.5386052246321));
#71946=CARTESIAN_POINT('Ctrl Pts',(-20.720007692024,-18.2153593864121,-12.5342935179843));
#71947=CARTESIAN_POINT('Ctrl Pts',(-20.7439159714601,-18.2833414390349,
-12.5299818113365));
#71948=CARTESIAN_POINT('Ctrl Pts',(-20.7642975065945,-18.3523492393767,
-12.5256701046887));
#71949=CARTESIAN_POINT('Ctrl Pts',(-20.7846795217661,-18.4213586650285,
-12.5213582964892));
#71950=CARTESIAN_POINT('Ctrl Pts',(-20.8015344966334,-18.4913934058167,
-12.5170464882897));
#71951=CARTESIAN_POINT('Ctrl Pts',(-20.8147766394152,-18.5620543924287,
-12.5127346800901));
#71952=CARTESIAN_POINT('Ctrl Pts',(-20.828033543779,-18.6327941478605,-12.5084180653339));
#71953=CARTESIAN_POINT('Ctrl Pts',(-20.8376694934189,-18.7041610510436,
-12.5041014505776));
#71954=CARTESIAN_POINT('Ctrl Pts',(-20.8436502754155,-18.7757481477,-12.4997848358213));
#71955=CARTESIAN_POINT('Ctrl Pts',(-20.8486051622908,-18.8350557709941,
-12.496208658356));
#71956=CARTESIAN_POINT('Ctrl Pts',(-20.8510522363742,-18.8945142745419,
-12.4926324808906));
#71957=CARTESIAN_POINT('Ctrl Pts',(-20.8509991540683,-18.9538925310889,
-12.4890563034253));
#71958=CARTESIAN_POINT('Ctrl Pts',(-20.8516473850063,-18.9538935158916,
-12.4890562790225));
#71959=CARTESIAN_POINT('Ctrl Pts',(-20.8529700926033,-19.0968822287437,
-12.4804472042752));
#71960=CARTESIAN_POINT('Ctrl Pts',(-20.8300641645468,-19.3437931350663,
-12.4655558047043));
#71961=CARTESIAN_POINT('Ctrl Pts',(-20.7608946003787,-19.5811887556435,
-12.4506644051334));
#71962=CARTESIAN_POINT('Ctrl Pts',(-20.7242504220745,-19.678735851896,-12.4443820803097));
#71963=CARTESIAN_POINT('Origin',(-18.734,-18.952,0.));
#71964=CARTESIAN_POINT('',(-20.7225805826898,-19.6781103677465,-11.642549326843));
#71965=CARTESIAN_POINT('',(-20.7225805820713,-19.6781103694405,-11.8674650853572));
#71966=CARTESIAN_POINT('',(-20.7225805821191,-19.6781103693095,0.));
#71967=CARTESIAN_POINT('',(-20.8509993992253,-18.9504051082612,-11.9120635502395));
#71968=CARTESIAN_POINT('Ctrl Pts',(-20.7225805820713,-19.6781103694405,
-11.8674650853572));
#71969=CARTESIAN_POINT('Ctrl Pts',(-20.7358715470792,-19.6417107309776,
-11.8699797732346));
#71970=CARTESIAN_POINT('Ctrl Pts',(-20.7481612630639,-19.604951226548,-11.8724727008059));
#71971=CARTESIAN_POINT('Ctrl Pts',(-20.7623062774745,-19.5584322024437,
-11.8755658152096));
#71972=CARTESIAN_POINT('Ctrl Pts',(-20.7651109560046,-19.5489712391965,
-11.8761917407254));
#71973=CARTESIAN_POINT('Ctrl Pts',(-20.783378893993,-19.4857290083341,-11.8803546635274));
#71974=CARTESIAN_POINT('Ctrl Pts',(-20.7967716263503,-19.4313690076842,
-11.8838304877392));
#71975=CARTESIAN_POINT('Ctrl Pts',(-20.8104073115161,-19.3647545756929,
-11.887969560528));
#71976=CARTESIAN_POINT('Ctrl Pts',(-20.8127188708028,-19.3529507807812,
-11.8886984932715));
#71977=CARTESIAN_POINT('Ctrl Pts',(-20.8163752184754,-19.3333978114117,
-11.8898986987927));
#71978=CARTESIAN_POINT('Ctrl Pts',(-20.8177776237672,-19.3256598163581,
-11.8903717987834));
#71979=CARTESIAN_POINT('Ctrl Pts',(-20.8202374523177,-19.3116426489251,
-11.8912254707796));
#71980=CARTESIAN_POINT('Ctrl Pts',(-20.8213097198868,-19.3053662080856,
-11.8916065107796));
#71981=CARTESIAN_POINT('Ctrl Pts',(-20.8233364632863,-19.2931716236168,
-11.8923445323753));
#71982=CARTESIAN_POINT('Ctrl Pts',(-20.8242941503961,-19.2872540820544,
-11.892701612527));
#71983=CARTESIAN_POINT('Ctrl Pts',(-20.8263396796084,-19.2742651871561,
-11.8934831274235));
#71984=CARTESIAN_POINT('Ctrl Pts',(-20.827416838552,-19.2671922075359,-11.8939072211355));
#71985=CARTESIAN_POINT('Ctrl Pts',(-20.8299772097504,-19.2497876328722,
-11.894947251902));
#71986=CARTESIAN_POINT('Ctrl Pts',(-20.8314199210973,-19.2394502017417,
-11.8955619130377));
#71987=CARTESIAN_POINT('Ctrl Pts',(-20.8449846075371,-19.1367106455658,
-11.9016414582525));
#71988=CARTESIAN_POINT('Ctrl Pts',(-20.8510696177588,-19.0436105526441,
-11.9069088192729));
#71989=CARTESIAN_POINT('Ctrl Pts',(-20.8509993992253,-18.9504051082612,
-11.9120635502395));
#71990=CARTESIAN_POINT('Ctrl Pts',(-20.8509994011072,-18.9504076081963,
-11.9120634119805));
#71991=CARTESIAN_POINT('Ctrl Pts',(-20.8509185676265,-18.8429438358049,
-11.9180067026759));
#71992=CARTESIAN_POINT('Ctrl Pts',(-20.8426553590784,-18.7356392271031,
-11.9237827343211));
#71993=CARTESIAN_POINT('Ctrl Pts',(-20.8144662881294,-18.5528019122291,
-11.9338768813632));
#71994=CARTESIAN_POINT('Ctrl Pts',(-20.7984544823587,-18.476894838746,-11.9381478592865));
#71995=CARTESIAN_POINT('Ctrl Pts',(-20.7691437057061,-18.3679398005603,
-11.9446066414929));
#71996=CARTESIAN_POINT('Ctrl Pts',(-20.7591179340521,-18.334073432349,-11.9466619632899));
#71997=CARTESIAN_POINT('Ctrl Pts',(-20.7459662609387,-18.2934137430804,
-11.9492053394917));
#71998=CARTESIAN_POINT('Ctrl Pts',(-20.7436448499687,-18.2863637132412,
-11.9496491277717));
#71999=CARTESIAN_POINT('Ctrl Pts',(-20.7399678682761,-18.2753914484512,
-11.9503443826599));
#72000=CARTESIAN_POINT('Ctrl Pts',(-20.7386377313515,-18.2714606653927,
-11.950594373282));
#72001=CARTESIAN_POINT('Ctrl Pts',(-20.7361428095416,-18.2641585262246,
-11.9510605279638));
#72002=CARTESIAN_POINT('Ctrl Pts',(-20.7349810585352,-18.2607861939944,
-11.9512765119146));
#72003=CARTESIAN_POINT('Ctrl Pts',(-20.7323265932119,-18.2531435839721,
-11.9517675738904));
#72004=CARTESIAN_POINT('Ctrl Pts',(-20.7308287180436,-18.2488751652235,
-11.9520429539471));
#72005=CARTESIAN_POINT('Ctrl Pts',(-20.7263403321082,-18.2362148587465,
-11.9528630037925));
#72006=CARTESIAN_POINT('Ctrl Pts',(-20.723310560138,-18.2278371341262,-11.9534099211958));
#72007=CARTESIAN_POINT('Ctrl Pts',(-20.70003653577,-18.1647297046504,-11.9575606454482));
#72008=CARTESIAN_POINT('Ctrl Pts',(-20.6775917875363,-18.1108437544836,
-11.9612804744289));
#72009=CARTESIAN_POINT('Ctrl Pts',(-20.6438613574187,-18.0384453847687,
-11.966458491192));
#72010=CARTESIAN_POINT('Ctrl Pts',(-20.6344729737546,-18.0190718803266,
-11.9678624389679));
#72011=CARTESIAN_POINT('Ctrl Pts',(-20.5649713374984,-17.8810553648092,
-11.9779817419938));
#72012=CARTESIAN_POINT('Ctrl Pts',(-20.4940849116522,-17.7681574140124,
-11.9868646309309));
#72013=CARTESIAN_POINT('Ctrl Pts',(-20.3732623415019,-17.6108137189589,
-11.9997138529784));
#72014=CARTESIAN_POINT('Ctrl Pts',(-20.3310694303964,-17.5608378175314,
-12.0038810957337));
#72015=CARTESIAN_POINT('Ctrl Pts',(-20.2691983534546,-17.4940862824816,
-12.0095592717183));
#72016=CARTESIAN_POINT('Ctrl Pts',(-20.2514281028702,-17.4755995006899,
-12.0111449690918));
#72017=CARTESIAN_POINT('Ctrl Pts',(-20.2199337027648,-17.4440046845269,
-12.0138788298085));
#72018=CARTESIAN_POINT('Ctrl Pts',(-20.2063613374684,-17.4307501950048,
-12.0150333647132));
#72019=CARTESIAN_POINT('Ctrl Pts',(-20.1863980443352,-17.4117719526879,
-12.0166981609527));
#72020=CARTESIAN_POINT('Ctrl Pts',(-20.1801478896024,-17.4059020724114,
-12.0172147447383));
#72021=CARTESIAN_POINT('Ctrl Pts',(-20.1691113632873,-17.3956625130229,
-12.0181189044961));
#72022=CARTESIAN_POINT('Ctrl Pts',(-20.1643402989295,-17.3912765686663,
-12.0185071748868));
#72023=CARTESIAN_POINT('Ctrl Pts',(-20.1550953315577,-17.3828558537133,
-12.0192545811365));
#72024=CARTESIAN_POINT('Ctrl Pts',(-20.1506242038972,-17.3788181416987,
-12.0196138398409));
#72025=CARTESIAN_POINT('Ctrl Pts',(-20.1387915016344,-17.3682238110123,
-12.0205588518216));
#72026=CARTESIAN_POINT('Ctrl Pts',(-20.1314012045182,-17.3616993811009,
-12.0211432503674));
#72027=CARTESIAN_POINT('Ctrl Pts',(-20.1052286970545,-17.3389166334173,
-12.0231927943456));
#72028=CARTESIAN_POINT('Ctrl Pts',(-20.0862057148745,-17.3229371196022,
-12.0246464249312));
#72029=CARTESIAN_POINT('Ctrl Pts',(-19.9417783239518,-17.2058899267861,
-12.0354289966536));
#72030=CARTESIAN_POINT('Ctrl Pts',(-19.8054879199467,-17.1190926754184,
-12.0441454916573));
#72031=CARTESIAN_POINT('Ctrl Pts',(-19.543790477347,-16.9916877723254,-12.0599582577842));
#72032=CARTESIAN_POINT('Ctrl Pts',(-19.4219457147379,-16.9456835890036,
-12.0670290975834));
#72033=CARTESIAN_POINT('Ctrl Pts',(-19.2852115225785,-16.9079852652148,
-12.0753993043172));
#72034=CARTESIAN_POINT('Ctrl Pts',(-19.2737227985241,-16.904921675954,-12.0761059186987));
#72035=CARTESIAN_POINT('Ctrl Pts',(-19.2573483935927,-16.9007026898369,
-12.077118546535));
#72036=CARTESIAN_POINT('Ctrl Pts',(-19.252483228653,-16.8994675797488,-12.0774201088643));
#72037=CARTESIAN_POINT('Ctrl Pts',(-19.2440893407327,-16.8973683875234,
-12.0779416567103));
#72038=CARTESIAN_POINT('Ctrl Pts',(-19.2405626645072,-16.8964960556362,
-12.0781611676606));
#72039=CARTESIAN_POINT('Ctrl Pts',(-19.2337187710189,-16.8948218850486,
-12.0785879224804));
#72040=CARTESIAN_POINT('Ctrl Pts',(-19.2304018533018,-16.8940189878427,
-12.0787950981116));
#72041=CARTESIAN_POINT('Ctrl Pts',(-19.221443932642,-16.8918735388113,-12.0793555220617));
#72042=CARTESIAN_POINT('Ctrl Pts',(-19.2157993800231,-16.8905461491583,
-12.0797096280388));
#72043=CARTESIAN_POINT('Ctrl Pts',(-19.1948080548063,-16.8857006901206,
-12.0810299257304));
#72044=CARTESIAN_POINT('Ctrl Pts',(-19.1794280713751,-16.8823307749749,
-12.0820040751469));
#72045=CARTESIAN_POINT('Ctrl Pts',(-19.0338793528071,-16.8521369622244,
-12.091277707838));
#72046=CARTESIAN_POINT('Ctrl Pts',(-18.9015049597613,-16.8374578893284,
-12.1001050363254));
#72047=CARTESIAN_POINT('Ctrl Pts',(-18.6105816054926,-16.8326966396408,
-12.1193232908383));
#72048=CARTESIAN_POINT('Ctrl Pts',(-18.4527006870236,-16.8478214602303,
-12.1296096473111));
#72049=CARTESIAN_POINT('Ctrl Pts',(-18.2771319967909,-16.8847764096748,
-12.1406290920443));
#72050=CARTESIAN_POINT('Ctrl Pts',(-18.2563771364257,-16.889472861555,-12.1419259562897));
#72051=CARTESIAN_POINT('Ctrl Pts',(-18.2269580599202,-16.8965977763712,
-12.1437565121233));
#72052=CARTESIAN_POINT('Ctrl Pts',(-18.2182335895534,-16.8987696564558,
-12.1442984128683));
#72053=CARTESIAN_POINT('Ctrl Pts',(-18.2032036125933,-16.9026130812662,
-12.1452303719699));
#72054=CARTESIAN_POINT('Ctrl Pts',(-18.196891560507,-16.904258299183,-12.1456212745695));
#72055=CARTESIAN_POINT('Ctrl Pts',(-18.1848184377886,-16.9074647869958,
-12.1463680607121));
#72056=CARTESIAN_POINT('Ctrl Pts',(-18.179056178119,-16.9090212969375,-12.1467240941382));
#72057=CARTESIAN_POINT('Ctrl Pts',(-18.1640851621782,-16.9131333031989,
-12.1476481293907));
#72058=CARTESIAN_POINT('Ctrl Pts',(-18.1548869244608,-16.9157268405281,
-12.1482148913496));
#72059=CARTESIAN_POINT('Ctrl Pts',(-18.1235594148199,-16.9247893967345,
-12.1501421194037));
#72060=CARTESIAN_POINT('Ctrl Pts',(-18.1015179135435,-16.9315577192699,
-12.151492835393));
#72061=CARTESIAN_POINT('Ctrl Pts',(-17.9135613355801,-16.9926512524357,
-12.1629764456236));
#72062=CARTESIAN_POINT('Ctrl Pts',(-17.7548460951913,-17.0669452295633,
-12.1723674309809));
#72063=CARTESIAN_POINT('Ctrl Pts',(-17.5328552153039,-17.206542941225,-12.1866338937454));
#72064=CARTESIAN_POINT('Ctrl Pts',(-17.4616422455476,-17.2577531318441,
-12.1914296539073));
#72065=CARTESIAN_POINT('Ctrl Pts',(-17.3644107249343,-17.3372687796213,
-12.1985998549312));
#72066=CARTESIAN_POINT('Ctrl Pts',(-17.3356625658025,-17.362099464542,-12.2008059067099));
#72067=CARTESIAN_POINT('Ctrl Pts',(-17.3019982132014,-17.3927959238269,
-12.2035164515418));
#72068=CARTESIAN_POINT('Ctrl Pts',(-17.2964241144743,-17.3979337086322,
-12.2039695904049));
#72069=CARTESIAN_POINT('Ctrl Pts',(-17.287816433903,-17.40595355793,-12.2046763184344));
#72070=CARTESIAN_POINT('Ctrl Pts',(-17.2847635348026,-17.4088149251846,
-12.2049283515191));
#72071=CARTESIAN_POINT('Ctrl Pts',(-17.2791263015234,-17.4141299726935,
-12.2053963366021));
#72072=CARTESIAN_POINT('Ctrl Pts',(-17.2765396723192,-17.416581134653,-12.2056120960131));
#72073=CARTESIAN_POINT('Ctrl Pts',(-17.2707169491088,-17.4221268805651,
-12.2061001047623));
#72074=CARTESIAN_POINT('Ctrl Pts',(-17.2674844956563,-17.4252251890792,
-12.206372640274));
#72075=CARTESIAN_POINT('Ctrl Pts',(-17.2580046488534,-17.4343695087406,
-12.2071766206417));
#72076=CARTESIAN_POINT('Ctrl Pts',(-17.2517847304922,-17.4404436915919,
-12.2077101870163));
#72077=CARTESIAN_POINT('Ctrl Pts',(-17.2080430168751,-17.483690103548,-12.2115044535058));
#72078=CARTESIAN_POINT('Ctrl Pts',(-17.1718896218182,-17.5222137140302,
-12.2148603229745));
#72079=CARTESIAN_POINT('Ctrl Pts',(-17.1270154340751,-17.5737652377432,
-12.2192759565411));
#72080=CARTESIAN_POINT('Ctrl Pts',(-17.1169426633622,-17.5855974209795,
-12.2202846082135));
#72081=CARTESIAN_POINT('Ctrl Pts',(-17.0206797985266,-17.7012298272086,
-12.2300877104767));
#72082=CARTESIAN_POINT('Ctrl Pts',(-16.9444672921623,-17.8129357490622,
-12.2391142900666));
#72083=CARTESIAN_POINT('Ctrl Pts',(-16.8324364319377,-18.0164623445212,
-12.254226853012));
#72084=CARTESIAN_POINT('Ctrl Pts',(-16.7914098361147,-18.1049328999886,
-12.2604206720449));
#72085=CARTESIAN_POINT('Ctrl Pts',(-16.7488927238891,-18.2161291225741,
-12.2677349921378));
#72086=CARTESIAN_POINT('Ctrl Pts',(-16.7414776561936,-18.2364501346267,
-12.2690536179719));
#72087=CARTESIAN_POINT('Ctrl Pts',(-16.7314035750793,-18.2654299315242,
-12.270909249224));
#72088=CARTESIAN_POINT('Ctrl Pts',(-16.7284868551709,-18.2739971018309,
-12.2714547729041));
#72089=CARTESIAN_POINT('Ctrl Pts',(-16.7235591097719,-18.2887812458655,
-12.2723910073258));
#72090=CARTESIAN_POINT('Ctrl Pts',(-16.721521782423,-18.294989258687,-12.2727825828778));
#72091=CARTESIAN_POINT('Ctrl Pts',(-16.7176820909712,-18.306874763982,-12.2735293320088));
#72092=CARTESIAN_POINT('Ctrl Pts',(-16.7158748880513,-18.3125506165016,
-12.2738846618351));
#72093=CARTESIAN_POINT('Ctrl Pts',(-16.7112508296161,-18.3272881934851,
-12.2748040273872));
#72094=CARTESIAN_POINT('Ctrl Pts',(-16.7084708834987,-18.336361428961,-12.2753668484514));
#72095=CARTESIAN_POINT('Ctrl Pts',(-16.6992635842597,-18.3671499602183,
-12.2772661542599));
#72096=CARTESIAN_POINT('Ctrl Pts',(-16.6931235535876,-18.3889500560984,
-12.2785932742696));
#72097=CARTESIAN_POINT('Ctrl Pts',(-16.6413731965901,-18.5846716186548,
-12.2903612435084));
#72098=CARTESIAN_POINT('Ctrl Pts',(-16.6177427928168,-18.7636413725187,
-12.3000071994611));
#72099=CARTESIAN_POINT('Ctrl Pts',(-16.6166782209977,-19.0274760084611,
-12.3143734482994));
#72100=CARTESIAN_POINT('Ctrl Pts',(-16.6213412674197,-19.1114333725433,
-12.3189820059042));
#72101=CARTESIAN_POINT('Ctrl Pts',(-16.6352307957032,-19.231696336893,-12.3258994678031));
#72102=CARTESIAN_POINT('Ctrl Pts',(-16.6404478918399,-19.2683880641553,
-12.3280532474319));
#72103=CARTESIAN_POINT('Ctrl Pts',(-16.6478796142739,-19.3123434444918,
-12.3307058467947));
#72104=CARTESIAN_POINT('Ctrl Pts',(-16.6491740493474,-19.3197586346467,
-12.3311558322912));
#72105=CARTESIAN_POINT('Ctrl Pts',(-16.6512474400778,-19.3312732327306,
-12.3318586922956));
#72106=CARTESIAN_POINT('Ctrl Pts',(-16.6519990317559,-19.3353775925498,
-12.3321100379411));
#72107=CARTESIAN_POINT('Ctrl Pts',(-16.6534151877111,-19.3429840731354,
-12.3325774007549));
#72108=CARTESIAN_POINT('Ctrl Pts',(-16.6540764648268,-19.3464867473232,
-12.3327932295165));
#72109=CARTESIAN_POINT('Ctrl Pts',(-16.6555911984728,-19.3544003457163,
-12.3332822376755));
#72110=CARTESIAN_POINT('Ctrl Pts',(-16.6564498471733,-19.3588102089762,
-12.3335557084669));
#72111=CARTESIAN_POINT('Ctrl Pts',(-16.6590249476465,-19.3718146562835,
-12.3343649558944));
#72112=CARTESIAN_POINT('Ctrl Pts',(-16.6607807173933,-19.3804012297473,
-12.3349028949872));
#72113=CARTESIAN_POINT('Ctrl Pts',(-16.6738381177958,-19.4422975436483,
-12.3388054876417));
#72114=CARTESIAN_POINT('Ctrl Pts',(-16.6871401814529,-19.4951596902494,
-12.3422714146459));
#72115=CARTESIAN_POINT('Ctrl Pts',(-16.710915326641,-19.5762756100903,-12.3477384364724));
#72116=CARTESIAN_POINT('Ctrl Pts',(-16.7199782499035,-19.6049225969443,
-12.3496987075554));
#72117=CARTESIAN_POINT('Ctrl Pts',(-16.7713467167216,-19.7560315446476,
-12.3601667422174));
#72118=CARTESIAN_POINT('Ctrl Pts',(-16.8242222547657,-19.8746197759884,
-12.3688106848789));
#72119=CARTESIAN_POINT('Ctrl Pts',(-16.9306835106997,-20.064426003423,-12.3828999435972));
#72120=CARTESIAN_POINT('Ctrl Pts',(-16.9785109570755,-20.1384668492301,
-12.3884748073271));
#72121=CARTESIAN_POINT('Ctrl Pts',(-17.0429913087979,-20.2258126884641,
-12.395137564478));
#72122=CARTESIAN_POINT('Ctrl Pts',(-17.0554044716555,-20.2421264502442,
-12.3963862245251));
#72123=CARTESIAN_POINT('Ctrl Pts',(-17.0735177871782,-20.2652274214933,
-12.3981610621399));
#72124=CARTESIAN_POINT('Ctrl Pts',(-17.0790263540612,-20.2721627455101,
-12.3986947835348));
#72125=CARTESIAN_POINT('Ctrl Pts',(-17.0886523388242,-20.2841269877132,
-12.399617127077));
#72126=CARTESIAN_POINT('Ctrl Pts',(-17.0927496603199,-20.289171851892,-12.4000065473993));
#72127=CARTESIAN_POINT('Ctrl Pts',(-17.1006731547311,-20.2988364399503,
-12.4007535785642));
#72128=CARTESIAN_POINT('Ctrl Pts',(-17.1044958522927,-20.303458920278,-12.401111324537));
#72129=CARTESIAN_POINT('Ctrl Pts',(-17.1145631269963,-20.3155276504802,
-12.4020465765252));
#72130=CARTESIAN_POINT('Ctrl Pts',(-17.1208394665978,-20.322947313913,-12.4026227815959));
#72131=CARTESIAN_POINT('Ctrl Pts',(-17.1428074041226,-20.3485572741231,
-12.4046161848513));
#72132=CARTESIAN_POINT('Ctrl Pts',(-17.1587577246184,-20.3665239270639,
-12.4060226930004));
#72133=CARTESIAN_POINT('Ctrl Pts',(-17.2748110920692,-20.4928498207702,
-12.4159804993574));
#72134=CARTESIAN_POINT('Ctrl Pts',(-17.3856945483354,-20.5907585268992,
-12.4240270587059));
#72135=CARTESIAN_POINT('Ctrl Pts',(-17.5439647497482,-20.7034829403172,
-12.4345796710768));
#72136=CARTESIAN_POINT('Ctrl Pts',(-17.5829479229916,-20.7293450426015,
-12.437116717034));
#72137=CARTESIAN_POINT('Ctrl Pts',(-17.6835103683468,-20.791362828888,-12.4435797683822));
#72138=CARTESIAN_POINT('Ctrl Pts',(-17.7461173731449,-20.8257316904768,
-12.4475293662063));
#72139=CARTESIAN_POINT('Ctrl Pts',(-17.8405408809355,-20.8715173157519,
-12.453547773292));
#72140=CARTESIAN_POINT('Ctrl Pts',(-17.8710889920245,-20.8854425849454,
-12.4555040949869));
#72141=CARTESIAN_POINT('Ctrl Pts',(-17.9086757220346,-20.9015082160251,
-12.4579375170801));
#72142=CARTESIAN_POINT('Ctrl Pts',(-17.9154129368002,-20.9043467070598,
-12.4583747109307));
#72143=CARTESIAN_POINT('Ctrl Pts',(-17.9259745501669,-20.9087321970095,
-12.4590618686022));
#72144=CARTESIAN_POINT('Ctrl Pts',(-17.9297890722405,-20.9103030412569,
-12.4593104118072));
#72145=CARTESIAN_POINT('Ctrl Pts',(-17.9369129639894,-20.9132123802894,
-12.4597753047112));
#72146=CARTESIAN_POINT('Ctrl Pts',(-17.9402211361437,-20.9145536574145,
-12.4599914832567));
#72147=CARTESIAN_POINT('Ctrl Pts',(-17.9477613383806,-20.9175886002641,
-12.4604848699888));
#72148=CARTESIAN_POINT('Ctrl Pts',(-17.9519954391431,-20.9192769617962,
-12.4607623921135));
#72149=CARTESIAN_POINT('Ctrl Pts',(-17.9630180965906,-20.9236310749426,
-12.4614860178304));
#72150=CARTESIAN_POINT('Ctrl Pts',(-17.9698149686861,-20.9262754178315,
-12.4619333569158));
#72151=CARTESIAN_POINT('Ctrl Pts',(-18.013180324473,-20.9428893497819,-12.4647940349285));
#72152=CARTESIAN_POINT('Ctrl Pts',(-18.0501142289988,-20.9558765461593,
-12.4672600161436));
#72153=CARTESIAN_POINT('Ctrl Pts',(-18.0991349441146,-20.9716008646714,
-12.4705524317999));
#72154=CARTESIAN_POINT('Ctrl Pts',(-18.1109183866702,-20.9752673041789,
-12.4713453165844));
#72155=CARTESIAN_POINT('Ctrl Pts',(-18.1458489787212,-20.98580193884,-12.4736987858701));
#72156=CARTESIAN_POINT('Ctrl Pts',(-18.1690819341408,-20.9923772854732,
-12.4752680532311));
#72157=CARTESIAN_POINT('Ctrl Pts',(-18.3317800649155,-21.0354320037361,
-12.4862637836891));
#72158=CARTESIAN_POINT('Ctrl Pts',(-18.4745550414503,-21.0579827035799,
-12.4959109169794));
#72159=CARTESIAN_POINT('Ctrl Pts',(-18.6802311550212,-21.0692194916129,
-12.509219179147));
#72160=CARTESIAN_POINT('Ctrl Pts',(-18.7420711558458,-21.0698870251877,
-12.5131507704253));
#72161=CARTESIAN_POINT('Ctrl Pts',(-18.8410951838317,-21.066617660406,-12.5193243928189));
#72162=CARTESIAN_POINT('Ctrl Pts',(-18.8782965839875,-21.0644052643062,
-12.5216163397455));
#72163=CARTESIAN_POINT('Ctrl Pts',(-18.9265161375305,-21.060257698663,-12.5245534348725));
#72164=CARTESIAN_POINT('Ctrl Pts',(-18.9376025876477,-21.0592159312481,
-12.525226415348));
#72165=CARTESIAN_POINT('Ctrl Pts',(-18.955614489402,-21.0573799178003,-12.5263161660786));
#72166=CARTESIAN_POINT('Ctrl Pts',(-18.9625450384991,-21.056638863885,-12.5267346022133));
#72167=CARTESIAN_POINT('Ctrl Pts',(-18.9758627008476,-21.0551483039326,
-12.5275370260485));
#72168=CARTESIAN_POINT('Ctrl Pts',(-18.9822502964348,-21.054403897001,-12.5279211696673));
#72169=CARTESIAN_POINT('Ctrl Pts',(-18.9968632835753,-21.0526333810973,
-12.5287983629214));
#72170=CARTESIAN_POINT('Ctrl Pts',(-19.005086272362,-21.051588041391,-12.5292908006172));
#72171=CARTESIAN_POINT('Ctrl Pts',(-19.0269054778989,-21.0486839738374,
-12.5305944562841));
#72172=CARTESIAN_POINT('Ctrl Pts',(-19.0404902626894,-21.0467412816943,
-12.5314030225098));
#72173=CARTESIAN_POINT('Ctrl Pts',(-19.1432878596563,-21.0310192693119,
-12.5374998570467));
#72174=CARTESIAN_POINT('Ctrl Pts',(-19.2315619172785,-21.011677809125,-12.542605636556));
#72175=CARTESIAN_POINT('Ctrl Pts',(-19.4524106042043,-20.9482546123032,
-12.5553256081018));
#72176=CARTESIAN_POINT('Ctrl Pts',(-19.5823413261859,-20.8965980082631,
-12.5627450703409));
#72177=CARTESIAN_POINT('Ctrl Pts',(-19.755360329122,-20.8071466963016,-12.5735038081901));
#72178=CARTESIAN_POINT('Ctrl Pts',(-19.8034593137398,-20.7798408335541,
-12.5766019163904));
#72179=CARTESIAN_POINT('Ctrl Pts',(-19.8746319555107,-20.7356645080236,
-12.5814338042496));
#72180=CARTESIAN_POINT('Ctrl Pts',(-19.8985260649091,-20.720157006408,-12.5831004506625));
#72181=CARTESIAN_POINT('Ctrl Pts',(-19.9278456863197,-20.7002762054967,
-12.5852110717727));
#72182=CARTESIAN_POINT('Ctrl Pts',(-19.9335733760471,-20.6963511475277,
-12.5856265638801));
#72183=CARTESIAN_POINT('Ctrl Pts',(-19.9426064176098,-20.6900954760322,
-12.5862870463402));
#72184=CARTESIAN_POINT('Ctrl Pts',(-19.9459246361934,-20.6877834058569,
-12.5865307918188));
#72185=CARTESIAN_POINT('Ctrl Pts',(-19.9521703936436,-20.6834048437636,
-12.5869917470716));
#72186=CARTESIAN_POINT('Ctrl Pts',(-19.955099318139,-20.6813404220923,-12.5872088162025));
#72187=CARTESIAN_POINT('Ctrl Pts',(-19.9617838667649,-20.6766034395958,
-12.5877062847042));
#72188=CARTESIAN_POINT('Ctrl Pts',(-19.9655360083536,-20.6739260456115,
-12.5879870134862));
#72189=CARTESIAN_POINT('Ctrl Pts',(-19.975474541165,-20.6667851638483,-12.5887345014587));
#72190=CARTESIAN_POINT('Ctrl Pts',(-19.9816455357087,-20.6623005021688,
-12.5892026657452));
#72191=CARTESIAN_POINT('Ctrl Pts',(-20.024702482516,-20.6306525913797,-12.5924967979107));
#72192=CARTESIAN_POINT('Ctrl Pts',(-20.0607196961468,-20.6023337784195,
-12.5953948294594));
#72193=CARTESIAN_POINT('Ctrl Pts',(-20.1245701968741,-20.5486893202651,
-12.6007562756045));
#72194=CARTESIAN_POINT('Ctrl Pts',(-20.1527030036379,-20.5237454690348,
-12.6032036500081));
#72195=CARTESIAN_POINT('Ctrl Pts',(-20.2758195357236,-20.4085850850627,
-12.6142537724694));
#72196=CARTESIAN_POINT('Ctrl Pts',(-20.36297939067,-20.3104098869636,-12.6229969641755));
#72197=CARTESIAN_POINT('Ctrl Pts',(-20.4927973386742,-20.1335789387884,
-12.6372014210681));
#72198=CARTESIAN_POINT('Ctrl Pts',(-20.5405828621735,-20.059139852871,-12.642796817856));
#72199=CARTESIAN_POINT('Ctrl Pts',(-20.5935715959742,-19.9639803495881,
-12.6494813230252));
#72200=CARTESIAN_POINT('Ctrl Pts',(-20.6033012857515,-19.9458931020195,
-12.6507323760418));
#72201=CARTESIAN_POINT('Ctrl Pts',(-20.6168513921819,-19.9198006994783,
-12.6525099853627));
#72202=CARTESIAN_POINT('Ctrl Pts',(-20.6208868722838,-19.9119091070977,
-12.6530441178926));
#72203=CARTESIAN_POINT('Ctrl Pts',(-20.6277957976667,-19.8981864137335,
-12.6539669434635));
#72204=CARTESIAN_POINT('Ctrl Pts',(-20.6306921440056,-19.8923670374509,
-12.654356436983));
#72205=CARTESIAN_POINT('Ctrl Pts',(-20.6362088784293,-19.8811535629588,
-12.6551034501763));
#72206=CARTESIAN_POINT('Ctrl Pts',(-20.6388332360704,-19.8757614977014,
-12.6554611057355));
#72207=CARTESIAN_POINT('Ctrl Pts',(-20.6456466878072,-19.8616099253851,
-12.6563957702967));
#72208=CARTESIAN_POINT('Ctrl Pts',(-20.6497985236599,-19.8528325576252,
-12.6569714815719));
#72209=CARTESIAN_POINT('Ctrl Pts',(-20.6639911323003,-19.8222861155732,
-12.6589614563516));
#72210=CARTESIAN_POINT('Ctrl Pts',(-20.6737226580472,-19.8003747830157,
-12.6603650794084));
#72211=CARTESIAN_POINT('Ctrl Pts',(-20.6971018432278,-19.7452280013232,
-12.6638422537416));
#72212=CARTESIAN_POINT('Ctrl Pts',(-20.7102719135608,-19.7118198044429,
-12.6658991664758));
#72213=CARTESIAN_POINT('Ctrl Pts',(-20.7225804971235,-19.6781106020849,
-12.6679319461521));
#72214=CARTESIAN_POINT('',(-20.8538228987003,-18.9509225630713,-11.6890562790225));
#72215=CARTESIAN_POINT('Ctrl Pts',(-20.7242504220745,-19.678735851896,-12.4443820803097));
#72216=CARTESIAN_POINT('Ctrl Pts',(-20.5136266400376,-20.2394180472743,
-12.4082724695729));
#72217=CARTESIAN_POINT('Ctrl Pts',(-19.519709855093,-21.2712729544138,-12.3297709232754));
#72218=CARTESIAN_POINT('Ctrl Pts',(-17.2597753208662,-20.9751143311526,
-12.2088774414178));
#72219=CARTESIAN_POINT('Ctrl Pts',(-16.2349111543522,-18.8074837620172,
-12.0817016347362));
#72220=CARTESIAN_POINT('Ctrl Pts',(-17.5028058927726,-16.7724378715414,
-11.9545258280549));
#72221=CARTESIAN_POINT('Ctrl Pts',(-19.9002448080497,-16.7370049550442,
-11.8273500213734));
#72222=CARTESIAN_POINT('Ctrl Pts',(-20.8239162058793,-18.1263146561008,
-11.7388601716959));
#72223=CARTESIAN_POINT('Ctrl Pts',(-20.8542040030872,-18.8895339278279,
-11.692762257579));
#72224=CARTESIAN_POINT('Ctrl Pts',(-20.8538228987003,-18.9509225630713,
-11.6890562790225));
#72225=CARTESIAN_POINT('Ctrl Pts',(-20.8509997772495,-18.951028853519,-11.6906773230242));
#72226=CARTESIAN_POINT('Ctrl Pts',(-20.8510794080773,-19.1246158951622,
-11.6795115293442));
#72227=CARTESIAN_POINT('Ctrl Pts',(-20.8298099013721,-19.2975644957165,
-11.6678002294521));
#72228=CARTESIAN_POINT('Ctrl Pts',(-20.7727929299519,-19.5253756648775,
-11.6526342526004));
#72229=CARTESIAN_POINT('Ctrl Pts',(-20.7553607601819,-19.5840902169118,
-11.6487420158878));
#72230=CARTESIAN_POINT('Ctrl Pts',(-20.7312404359986,-19.6540563010343,
-11.6441315496009));
#72231=CARTESIAN_POINT('Ctrl Pts',(-20.7269648807203,-19.6661031986997,
-11.6433386668622));
#72232=CARTESIAN_POINT('Ctrl Pts',(-20.7225805826898,-19.6781103677465,
-11.642549326843));
#72233=CARTESIAN_POINT('Origin',(-18.734,-18.952,0.));
#72234=CARTESIAN_POINT('',(-20.7225805823871,-19.6781103685755,-10.8441190550425));
#72235=CARTESIAN_POINT('',(-20.7225805818558,-19.6781103700305,-11.0644159698366));
#72236=CARTESIAN_POINT('',(-20.7225805821191,-19.6781103693095,0.));
#72237=CARTESIAN_POINT('Ctrl Pts',(-20.7225805818558,-19.6781103700305,
-11.0644159698366));
#72238=CARTESIAN_POINT('Ctrl Pts',(-20.7579844873321,-19.5811505663178,
-11.0708124775531));
#72239=CARTESIAN_POINT('Ctrl Pts',(-20.7862468792086,-19.4817385396693,
-11.0775607479106));
#72240=CARTESIAN_POINT('Ctrl Pts',(-20.8362075101163,-19.2401187738218,
-11.0938352048317));
#72241=CARTESIAN_POINT('Ctrl Pts',(-20.850904768817,-19.0969559230897,-11.1033538061458));
#72242=CARTESIAN_POINT('Ctrl Pts',(-20.8510404642511,-18.8914033906172,
-11.1164064283306));
#72243=CARTESIAN_POINT('Ctrl Pts',(-20.8483582573918,-18.8294329440592,
-11.1202674706854));
#72244=CARTESIAN_POINT('Ctrl Pts',(-20.8418780036,-18.7552932863852,-11.1248002585708));
#72245=CARTESIAN_POINT('Ctrl Pts',(-20.8406878626443,-18.7429319035788,
-11.1255531701033));
#72246=CARTESIAN_POINT('Ctrl Pts',(-20.8385539133076,-18.7226409458399,
-11.1267845412211));
#72247=CARTESIAN_POINT('Ctrl Pts',(-20.8376739010565,-18.7147050980675,
-11.1272649965875));
#72248=CARTESIAN_POINT('Ctrl Pts',(-20.8360103029312,-18.7004401585787,
-11.1281266408321));
#72249=CARTESIAN_POINT('Ctrl Pts',(-20.8352429789031,-18.6941093013817,
-11.128508337234));
#72250=CARTESIAN_POINT('Ctrl Pts',(-20.8335469916613,-18.6806267574853,
-11.1293197527859));
#72251=CARTESIAN_POINT('Ctrl Pts',(-20.8326103660227,-18.673476140081,-11.1297492155852));
#72252=CARTESIAN_POINT('Ctrl Pts',(-20.829987445343,-18.6542163531508,-11.1309036536396));
#72253=CARTESIAN_POINT('Ctrl Pts',(-20.8282327463475,-18.6421166591405,
-11.1316264622143));
#72254=CARTESIAN_POINT('Ctrl Pts',(-20.8189028629222,-18.581484427413,-11.1352369958233));
#72255=CARTESIAN_POINT('Ctrl Pts',(-20.8097446721144,-18.5332084702202,
-11.1380742019443));
#72256=CARTESIAN_POINT('Ctrl Pts',(-20.77842894594,-18.3946544175901,-11.1461498406355));
#72257=CARTESIAN_POINT('Ctrl Pts',(-20.7519967217578,-18.3054591454402,
-11.1512604423142));
#72258=CARTESIAN_POINT('Ctrl Pts',(-20.662349994649,-18.0628319145366,-11.1653489677555));
#72259=CARTESIAN_POINT('Ctrl Pts',(-20.5868669751842,-17.9146859160175,
-11.1741494194995));
#72260=CARTESIAN_POINT('Ctrl Pts',(-20.4871421882956,-17.7652493966157,
-11.18471080089));
#72261=CARTESIAN_POINT('Ctrl Pts',(-20.4792655345325,-17.7536958993347,
-11.18553946098));
#72262=CARTESIAN_POINT('Ctrl Pts',(-20.4681194465743,-17.737689808394,-11.1867057626787));
#72263=CARTESIAN_POINT('Ctrl Pts',(-20.4649459669798,-17.733170416235,-11.1870371320656));
#72264=CARTESIAN_POINT('Ctrl Pts',(-20.4598136868389,-17.7259219425457,
-11.1875720124777));
#72265=CARTESIAN_POINT('Ctrl Pts',(-20.4578659848135,-17.7231849810935,
-11.1877747655506));
#72266=CARTESIAN_POINT('Ctrl Pts',(-20.453774816735,-17.7174648349837,-11.1882001881634));
#72267=CARTESIAN_POINT('Ctrl Pts',(-20.4516300983818,-17.7144825906876,
-11.1884229470425));
#72268=CARTESIAN_POINT('Ctrl Pts',(-20.4464076162279,-17.7072604265331,
-11.1889647147434));
#72269=CARTESIAN_POINT('Ctrl Pts',(-20.4433218642617,-17.7030263361959,
-11.1892842714886));
#72270=CARTESIAN_POINT('Ctrl Pts',(-20.4323912721032,-17.6881443887543,
-11.1904141674171));
#72271=CARTESIAN_POINT('Ctrl Pts',(-20.4244625858972,-17.6775588893136,
-11.1912300439275));
#72272=CARTESIAN_POINT('Ctrl Pts',(-20.3764348900314,-17.6146744062217,
-11.1961467917197));
#72273=CARTESIAN_POINT('Ctrl Pts',(-20.3340141529888,-17.564201330716,-11.2003845261687));
#72274=CARTESIAN_POINT('Ctrl Pts',(-20.2240817521247,-17.4451520266549,
-11.2109621644093));
#72275=CARTESIAN_POINT('Ctrl Pts',(-20.1541137412452,-17.3790374347441,
-11.2173578349685));
#72276=CARTESIAN_POINT('Ctrl Pts',(-19.9712621129894,-17.2284345051613,
-11.2329413739918));
#72277=CARTESIAN_POINT('Ctrl Pts',(-19.8539618884946,-17.1500027207405,
-11.2419899121193));
#72278=CARTESIAN_POINT('Ctrl Pts',(-19.7171140998958,-17.0770653795885,
-11.2514585608735));
#72279=CARTESIAN_POINT('Ctrl Pts',(-19.7044367136208,-17.0704724916167,
-11.2523264913288));
#72280=CARTESIAN_POINT('Ctrl Pts',(-19.6841535537,-17.0601837564007,-11.2537007415871));
#72281=CARTESIAN_POINT('Ctrl Pts',(-19.676590880354,-17.0564043388244,-11.2542099890717));
#72282=CARTESIAN_POINT('Ctrl Pts',(-19.6632128771048,-17.0498185896777,
-11.2551053519251));
#72283=CARTESIAN_POINT('Ctrl Pts',(-19.6574070065859,-17.0469933883648,
-11.2554921233506));
#72284=CARTESIAN_POINT('Ctrl Pts',(-19.6453717582343,-17.041204850674,-11.2562901949485));
#72285=CARTESIAN_POINT('Ctrl Pts',(-19.6391406328896,-17.038245308087,-11.2567013597033));
#72286=CARTESIAN_POINT('Ctrl Pts',(-19.6231088304744,-17.0307266402043,
-11.2577540977608));
#72287=CARTESIAN_POINT('Ctrl Pts',(-19.6132874240169,-17.0262119877792,
-11.2583941295991));
#72288=CARTESIAN_POINT('Ctrl Pts',(-19.5721500402048,-17.0076824878413,
-11.2610550190411));
#72289=CARTESIAN_POINT('Ctrl Pts',(-19.5405292519066,-16.9943542607359,
-11.2630523428465));
#72290=CARTESIAN_POINT('Ctrl Pts',(-19.4573061818126,-16.96163456475,-11.2681970385183));
#72291=CARTESIAN_POINT('Ctrl Pts',(-19.4052450622355,-16.9434788747606,
-11.2713050089752));
#72292=CARTESIAN_POINT('Ctrl Pts',(-19.2479505595839,-16.8954247313737,
-11.2804501372988));
#72293=CARTESIAN_POINT('Ctrl Pts',(-19.1410481911417,-16.8716251140253,
-11.2863385681661));
#72294=CARTESIAN_POINT('Ctrl Pts',(-18.9869106877308,-16.8496507161838,
-11.294815342171));
#72295=CARTESIAN_POINT('Ctrl Pts',(-18.9408341897008,-16.8446187586796,
-11.2973492262774));
#72296=CARTESIAN_POINT('Ctrl Pts',(-18.8732968578577,-16.8394794261704,
-11.3011064623954));
#72297=CARTESIAN_POINT('Ctrl Pts',(-18.8519396268359,-16.8381795272402,
-11.3023009260558));
#72298=CARTESIAN_POINT('Ctrl Pts',(-18.7787678745559,-16.8348383223842,
-11.3064254654049));
#72299=CARTESIAN_POINT('Ctrl Pts',(-18.7269038955648,-16.8343771739595,
-11.3094040309555));
#72300=CARTESIAN_POINT('Ctrl Pts',(-18.6664282352558,-16.8360609722037,
-11.3129946951207));
#72301=CARTESIAN_POINT('Ctrl Pts',(-18.6577780991352,-16.8363549142684,
-11.3135110982405));
#72302=CARTESIAN_POINT('Ctrl Pts',(-18.6446645621392,-16.8368810545605,
-11.3142985533844));
#72303=CARTESIAN_POINT('Ctrl Pts',(-18.6401995732535,-16.8370743623204,
-11.3145674793427));
#72304=CARTESIAN_POINT('Ctrl Pts',(-18.6321760289926,-16.8374471927784,
-11.3150522420014));
#72305=CARTESIAN_POINT('Ctrl Pts',(-18.628617288541,-16.8376215619198,-11.3152677873554));
#72306=CARTESIAN_POINT('Ctrl Pts',(-18.6208737562566,-16.8380205735515,
-11.315737972356));
#72307=CARTESIAN_POINT('Ctrl Pts',(-18.6166892399142,-16.8382486552726,
-11.3159927972084));
#72308=CARTESIAN_POINT('Ctrl Pts',(-18.6049071606807,-16.838925944523,-11.3167123292818));
#72309=CARTESIAN_POINT('Ctrl Pts',(-18.597311393328,-16.8394036954825,-11.3171785901851));
#72310=CARTESIAN_POINT('Ctrl Pts',(-18.551291574423,-16.8425474286557,-11.3200172816168));
#72311=CARTESIAN_POINT('Ctrl Pts',(-18.512946147429,-16.8462205047304,-11.32244082374));
#72312=CARTESIAN_POINT('Ctrl Pts',(-18.3856261185697,-16.8619320178184,
-11.3306360958104));
#72313=CARTESIAN_POINT('Ctrl Pts',(-18.297322067007,-16.8785827890315,-11.3365589563103));
#72314=CARTESIAN_POINT('Ctrl Pts',(-18.0441406902274,-16.9432172183882,
-11.3538259097801));
#72315=CARTESIAN_POINT('Ctrl Pts',(-17.883673604404,-17.0057006591603,-11.3650719540722));
#72316=CARTESIAN_POINT('Ctrl Pts',(-17.7119985427835,-17.097884859132,-11.3770690553889));
#72317=CARTESIAN_POINT('Ctrl Pts',(-17.6916899067312,-17.1092250079467,
-11.3784891185983));
#72318=CARTESIAN_POINT('Ctrl Pts',(-17.6632766092955,-17.1257107591034,
-11.3804778074892));
#72319=CARTESIAN_POINT('Ctrl Pts',(-17.6550142981273,-17.130579996073,-11.381056335434));
#72320=CARTESIAN_POINT('Ctrl Pts',(-17.6416585665028,-17.1385737150611,
-11.3819919745945));
#72321=CARTESIAN_POINT('Ctrl Pts',(-17.6365448535094,-17.141663870763,-11.3823503299366));
#72322=CARTESIAN_POINT('Ctrl Pts',(-17.6258802996449,-17.1481701272996,
-11.3830979400449));
#72323=CARTESIAN_POINT('Ctrl Pts',(-17.6203320074089,-17.1515903011523,
-11.3834870404065));
#72324=CARTESIAN_POINT('Ctrl Pts',(-17.6071925293078,-17.1597739433391,
-11.3844089199815));
#72325=CARTESIAN_POINT('Ctrl Pts',(-17.5996155826525,-17.1645601236342,
-11.3849408545199));
#72326=CARTESIAN_POINT('Ctrl Pts',(-17.5742946242304,-17.1807806392733,
-11.3867198010634));
#72327=CARTESIAN_POINT('Ctrl Pts',(-17.5566909265376,-17.1924324464752,
-11.3879587166515));
#72328=CARTESIAN_POINT('Ctrl Pts',(-17.4624627602254,-17.2568489618403,
-11.3946071354624));
#72329=CARTESIAN_POINT('Ctrl Pts',(-17.3892011751445,-17.3143605354946,
-11.3998310507177));
#72330=CARTESIAN_POINT('Ctrl Pts',(-17.2048037462984,-17.4798624873552,
-11.4134760685261));
#72331=CARTESIAN_POINT('Ctrl Pts',(-17.1013405781946,-17.595516747048,-11.4216583478927));
#72332=CARTESIAN_POINT('Ctrl Pts',(-16.9802309195438,-17.7650459394442,
-11.433372371975));
#72333=CARTESIAN_POINT('Ctrl Pts',(-16.9507247510517,-17.8098554024099,
-11.436449435185));
#72334=CARTESIAN_POINT('Ctrl Pts',(-16.9184277827835,-17.8632103356466,
-11.4401504167748));
#72335=CARTESIAN_POINT('Ctrl Pts',(-16.9139476690044,-17.8707160800193,
-11.4406718866123));
#72336=CARTESIAN_POINT('Ctrl Pts',(-16.9072380496975,-17.8821168676759,
-11.4414655587312));
#72337=CARTESIAN_POINT('Ctrl Pts',(-16.9049741730571,-17.8859917151222,
-11.4417355842843));
#72338=CARTESIAN_POINT('Ctrl Pts',(-16.9009344145529,-17.8929569113979,
-11.4422215142728));
#72339=CARTESIAN_POINT('Ctrl Pts',(-16.8991540024281,-17.8960445705582,
-11.4424371210916));
#72340=CARTESIAN_POINT('Ctrl Pts',(-16.895304288382,-17.9027600262537,-11.4429064864137));
#72341=CARTESIAN_POINT('Ctrl Pts',(-16.8932379489929,-17.906389406468,-11.4431604249098));
#72342=CARTESIAN_POINT('Ctrl Pts',(-16.8874688996558,-17.9165924383327,
-11.4438750071541));
#72343=CARTESIAN_POINT('Ctrl Pts',(-16.8837906155752,-17.9231797274809,
-11.4443371712664));
#72344=CARTESIAN_POINT('Ctrl Pts',(-16.8621105825172,-17.962497909465,-11.4470999244142));
#72345=CARTESIAN_POINT('Ctrl Pts',(-16.8449436796381,-17.9956788191202,
-11.4494485653246));
#72346=CARTESIAN_POINT('Ctrl Pts',(-16.7915437151275,-18.1059466968339,
-11.4572675946221));
#72347=CARTESIAN_POINT('Ctrl Pts',(-16.7590845511968,-18.1847648905646,
-11.4628754206623));
#72348=CARTESIAN_POINT('Ctrl Pts',(-16.6736958740607,-18.4337796735083,
-11.4802659812416));
#72349=CARTESIAN_POINT('Ctrl Pts',(-16.6374055860073,-18.6088939673275,
-11.4919694303881));
#72350=CARTESIAN_POINT('Ctrl Pts',(-16.6216971068866,-18.8092250006362,
-11.5043355398657));
#72351=CARTESIAN_POINT('Ctrl Pts',(-16.6202826718643,-18.8319694491984,
-11.5057263784402));
#72352=CARTESIAN_POINT('Ctrl Pts',(-16.6187986224762,-18.8642354321953,
-11.5076815417981));
#72353=CARTESIAN_POINT('Ctrl Pts',(-16.6184256124905,-18.8737408000677,
-11.5082553233971));
#72354=CARTESIAN_POINT('Ctrl Pts',(-16.6179230993141,-18.8892060477199,
-11.5091853748408));
#72355=CARTESIAN_POINT('Ctrl Pts',(-16.6177546806795,-18.8951644508896,
-11.5095428596705));
#72356=CARTESIAN_POINT('Ctrl Pts',(-16.6174544999128,-18.9076515434461,
-11.5102903092406));
#72357=CARTESIAN_POINT('Ctrl Pts',(-16.6173277742421,-18.9141802998865,
-11.5106801123024));
#72358=CARTESIAN_POINT('Ctrl Pts',(-16.6170977999836,-18.92973785894,-11.5116066667348));
#72359=CARTESIAN_POINT('Ctrl Pts',(-16.6170221024747,-18.9387669884501,
-11.5121425500491));
#72360=CARTESIAN_POINT('Ctrl Pts',(-16.616961468523,-18.9693033990417,-11.513948816493));
#72361=CARTESIAN_POINT('Ctrl Pts',(-16.6172465045199,-18.9908103195865,
-11.5152107542175));
#72362=CARTESIAN_POINT('Ctrl Pts',(-16.6229840477437,-19.1921284540706,
-11.5269368435748));
#72363=CARTESIAN_POINT('Ctrl Pts',(-16.6510054389155,-19.3705577992118,
-11.5365998245621));
#72364=CARTESIAN_POINT('Ctrl Pts',(-16.7347789666902,-19.6585463785539,
-11.5529241017152));
#72365=CARTESIAN_POINT('Ctrl Pts',(-16.7780349048173,-19.7707091566606,
-11.5595103938139));
#72366=CARTESIAN_POINT('Ctrl Pts',(-16.8347118640321,-19.8871385202989,
-11.5671846549436));
#72367=CARTESIAN_POINT('Ctrl Pts',(-16.8389326008756,-19.8956625565929,
-11.5677516144617));
#72368=CARTESIAN_POINT('Ctrl Pts',(-16.8452721866534,-19.9082516709598,
-11.5685969769487));
#72369=CARTESIAN_POINT('Ctrl Pts',(-16.84734709472,-19.9123389116424,-11.5688726978324));
#72370=CARTESIAN_POINT('Ctrl Pts',(-16.8510625607891,-19.9195992766697,
-11.5693647795511));
#72371=CARTESIAN_POINT('Ctrl Pts',(-16.8526978919293,-19.922775019319,-11.5695808104175));
#72372=CARTESIAN_POINT('Ctrl Pts',(-16.8562312901945,-19.9295942664112,
-11.5700464092219));
#72373=CARTESIAN_POINT('Ctrl Pts',(-16.8581318996417,-19.9332363357724,
-11.5702961320384));
#72374=CARTESIAN_POINT('Ctrl Pts',(-16.8634079138655,-19.9432752191973,
-11.5709873215845));
#72375=CARTESIAN_POINT('Ctrl Pts',(-16.8668054815038,-19.9496602325058,
-11.5714301556311));
#72376=CARTESIAN_POINT('Ctrl Pts',(-16.8856059253174,-19.9845592700827,
-11.5738677463297));
#72377=CARTESIAN_POINT('Ctrl Pts',(-16.9016284040048,-20.012732468425,-11.5758985539128));
#72378=CARTESIAN_POINT('Ctrl Pts',(-17.0020051347757,-20.1801654887417,
-11.5883018036747));
#72379=CARTESIAN_POINT('Ctrl Pts',(-17.1015465148793,-20.3096789800685,
-11.5992662296815));
#72380=CARTESIAN_POINT('Ctrl Pts',(-17.2963442641619,-20.5103622226945,
-11.6175348600792));
#72381=CARTESIAN_POINT('Ctrl Pts',(-17.3845566913055,-20.5873462648025,
-11.6249792661696));
#72382=CARTESIAN_POINT('Ctrl Pts',(-17.4901846040866,-20.6651305013763,
-11.6329888615444));
#72383=CARTESIAN_POINT('Ctrl Pts',(-17.5017669852199,-20.6734803707338,
-11.6338561231333));
#72384=CARTESIAN_POINT('Ctrl Pts',(-17.5203382624236,-20.686585140214,-11.6352295178388));
#72385=CARTESIAN_POINT('Ctrl Pts',(-17.5272725358787,-20.691416353976,-11.6357385729682));
#72386=CARTESIAN_POINT('Ctrl Pts',(-17.539554898624,-20.6998648637377,-11.6366337121068));
#72387=CARTESIAN_POINT('Ctrl Pts',(-17.5448909187911,-20.7034994366282,
-11.6370204511408));
#72388=CARTESIAN_POINT('Ctrl Pts',(-17.5559635325566,-20.7109675049447,
-11.6378185655833));
#72389=CARTESIAN_POINT('Ctrl Pts',(-17.5617024134304,-20.7147974847763,
-11.6382298050335));
#72390=CARTESIAN_POINT('Ctrl Pts',(-17.5764847992254,-20.7245587498564,
-11.6392829614986));
#72391=CARTESIAN_POINT('Ctrl Pts',(-17.5855552873038,-20.7304489619235,
-11.639923334643));
#72392=CARTESIAN_POINT('Ctrl Pts',(-17.6236297688466,-20.7547610822365,
-11.6425875437171));
#72393=CARTESIAN_POINT('Ctrl Pts',(-17.6530358950941,-20.772545624605,-11.6445877708354));
#72394=CARTESIAN_POINT('Ctrl Pts',(-17.7307999031055,-20.8170277141788,
-11.6497416379285));
#72395=CARTESIAN_POINT('Ctrl Pts',(-17.7797933692674,-20.8425631869656,
-11.65285569201));
#72396=CARTESIAN_POINT('Ctrl Pts',(-18.0003559669081,-20.9467593781062,
-11.6664180841387));
#72397=CARTESIAN_POINT('Ctrl Pts',(-18.1809676349705,-21.0041792710223,
-11.6762656388817));
#72398=CARTESIAN_POINT('Ctrl Pts',(-18.4073602201613,-21.0440548965402,
-11.6893368017394));
#72399=CARTESIAN_POINT('Ctrl Pts',(-18.4481422604152,-21.0500162262898,
-11.6917225301682));
#72400=CARTESIAN_POINT('Ctrl Pts',(-18.4964149175663,-21.055638995056,-11.6946101484542));
#72401=CARTESIAN_POINT('Ctrl Pts',(-18.5037650309882,-21.0564561169903,
-11.6950515590223));
#72402=CARTESIAN_POINT('Ctrl Pts',(-18.5156829041899,-21.0577178602441,
-11.695770313428));
#72403=CARTESIAN_POINT('Ctrl Pts',(-18.5202481653399,-21.0581861773223,
-11.6960463585453));
#72404=CARTESIAN_POINT('Ctrl Pts',(-18.5283700476443,-21.0589926641191,
-11.6965387953529));
#72405=CARTESIAN_POINT('Ctrl Pts',(-18.5319260380648,-21.0593366787582,
-11.6967548552368));
#72406=CARTESIAN_POINT('Ctrl Pts',(-18.5395694361031,-21.0600565939946,
-11.6972202617655));
#72407=CARTESIAN_POINT('Ctrl Pts',(-18.5436570107701,-21.0604296036271,
-11.6974697619459));
#72408=CARTESIAN_POINT('Ctrl Pts',(-18.5549340111549,-21.0614256203844,
-11.6981597224047));
#72409=CARTESIAN_POINT('Ctrl Pts',(-18.5621254989973,-21.0620237507538,
-11.6986015421587));
#72410=CARTESIAN_POINT('Ctrl Pts',(-18.6013929219655,-21.0650876251846,
-11.7010234222429));
#72411=CARTESIAN_POINT('Ctrl Pts',(-18.6335169706994,-21.0668585884061,
-11.703038998777));
#72412=CARTESIAN_POINT('Ctrl Pts',(-18.8285955317185,-21.0731586812053,
-11.7154371960103));
#72413=CARTESIAN_POINT('Ctrl Pts',(-18.9915820964966,-21.0595848288149,
-11.7264156691741));
#72414=CARTESIAN_POINT('Ctrl Pts',(-19.2659917298223,-21.0043979204939,
-11.7446994764501));
#72415=CARTESIAN_POINT('Ctrl Pts',(-19.3784964379381,-20.9718971723678,
-11.7521456795152));
#72416=CARTESIAN_POINT('Ctrl Pts',(-19.5011222370866,-20.9251743462991,
-11.7601584202365));
#72417=CARTESIAN_POINT('Ctrl Pts',(-19.5144346470234,-20.9199469771841,
-11.7610271329673));
#72418=CARTESIAN_POINT('Ctrl Pts',(-19.5355343766359,-20.9114139890556,
-11.7624023837635));
#72419=CARTESIAN_POINT('Ctrl Pts',(-19.5433564412223,-20.9081959747764,
-11.762911856147));
#72420=CARTESIAN_POINT('Ctrl Pts',(-19.5571159429487,-20.902438627853,-11.7638074806225));
#72421=CARTESIAN_POINT('Ctrl Pts',(-19.5630614014326,-20.8999188614121,
-11.7641942899779));
#72422=CARTESIAN_POINT('Ctrl Pts',(-19.5744705594249,-20.8950218064413,
-11.7649362382588));
#72423=CARTESIAN_POINT('Ctrl Pts',(-19.5799359258969,-20.8926485802329,
-11.7652915109602));
#72424=CARTESIAN_POINT('Ctrl Pts',(-19.5943402722727,-20.8863213676107,
-11.7662275147921));
#72425=CARTESIAN_POINT('Ctrl Pts',(-19.6032620811115,-20.8823284633698,
-11.7668069104198));
#72426=CARTESIAN_POINT('Ctrl Pts',(-19.6363021087377,-20.8672660674517,
-11.768951572079));
#72427=CARTESIAN_POINT('Ctrl Pts',(-19.6602398224105,-20.8558048977944,
-11.7705033494632));
#72428=CARTESIAN_POINT('Ctrl Pts',(-19.7190620055048,-20.8262691787175,
-11.7743162838781));
#72429=CARTESIAN_POINT('Ctrl Pts',(-19.7536713989744,-20.8076676992583,
-11.7765593758584));
#72430=CARTESIAN_POINT('Ctrl Pts',(-19.8816292581679,-20.7342327264881,
-11.7848832307175));
#72431=CARTESIAN_POINT('Ctrl Pts',(-19.9712475386277,-20.6732283674483,
-11.7907667202882));
#72432=CARTESIAN_POINT('Ctrl Pts',(-20.1621981724831,-20.5205947240546,
-11.8040419224601));
#72433=CARTESIAN_POINT('Ctrl Pts',(-20.2601175449013,-20.4254973343465,
-11.8113990711624));
#72434=CARTESIAN_POINT('Ctrl Pts',(-20.3583114625171,-20.3097720358783,
-11.8202987225759));
#72435=CARTESIAN_POINT('Ctrl Pts',(-20.3682777801224,-20.2977595379688,
-11.8212221183077));
#72436=CARTESIAN_POINT('Ctrl Pts',(-20.3817499136355,-20.2811510848299,
-11.8224999853794));
#72437=CARTESIAN_POINT('Ctrl Pts',(-20.3853713640904,-20.2766490102178,
-11.8228464956567));
#72438=CARTESIAN_POINT('Ctrl Pts',(-20.391099894762,-20.269467478861,-11.8233995229171));
#72439=CARTESIAN_POINT('Ctrl Pts',(-20.3932190424407,-20.2667976224114,
-11.8236051829998));
#72440=CARTESIAN_POINT('Ctrl Pts',(-20.3975850636709,-20.2612696259498,
-11.824031163451));
#72441=CARTESIAN_POINT('Ctrl Pts',(-20.3998310193153,-20.2584108204592,
-11.8242515487345));
#72442=CARTESIAN_POINT('Ctrl Pts',(-20.4051694706375,-20.2515795261911,
-11.8247783612546));
#72443=CARTESIAN_POINT('Ctrl Pts',(-20.408255171997,-20.2476017761356,-11.8250852652578));
#72444=CARTESIAN_POINT('Ctrl Pts',(-20.418634009445,-20.2341235137528,-11.8261255781667));
#72445=CARTESIAN_POINT('Ctrl Pts',(-20.4258605442536,-20.2245723295287,
-11.8268634411502));
#72446=CARTESIAN_POINT('Ctrl Pts',(-20.5082067674954,-20.1137955701971,
-11.8354239296354));
#72447=CARTESIAN_POINT('Ctrl Pts',(-20.5742144263623,-20.0061265644406,
-11.8437541602859));
#72448=CARTESIAN_POINT('Ctrl Pts',(-20.6639559109624,-19.8253310612981,
-11.8570928881668));
#72449=CARTESIAN_POINT('Ctrl Pts',(-20.6939932569247,-19.7556568638507,
-11.862096629707));
#72450=CARTESIAN_POINT('Ctrl Pts',(-20.7210162224442,-19.6823839466691,
-11.8671696830208));
#72451=CARTESIAN_POINT('Ctrl Pts',(-20.7218001284805,-19.6802477784641,
-11.8673174213476));
#72452=CARTESIAN_POINT('Ctrl Pts',(-20.7225805820713,-19.6781103694405,
-11.8674650853572));
#72453=CARTESIAN_POINT('Ctrl Pts',(-20.7225805826898,-19.6781103677465,
-11.642549326843));
#72454=CARTESIAN_POINT('Ctrl Pts',(-20.7142737541329,-19.7008600745484,
-11.6410537824784));
#72455=CARTESIAN_POINT('Ctrl Pts',(-20.7055765608164,-19.7234671650752,
-11.6395709790409));
#72456=CARTESIAN_POINT('Ctrl Pts',(-20.6923270196944,-19.7562186672103,
-11.6374269988322));
#72457=CARTESIAN_POINT('Ctrl Pts',(-20.6880803544136,-19.7664828768096,
-11.6367556865579));
#72458=CARTESIAN_POINT('Ctrl Pts',(-20.6810401204349,-19.7831271056101,
-11.6356679616845));
#72459=CARTESIAN_POINT('Ctrl Pts',(-20.6782955490836,-19.7895275015664,
-11.6352498947636));
#72460=CARTESIAN_POINT('Ctrl Pts',(-20.6729551092705,-19.8018137818539,
-11.6344477271332));
#72461=CARTESIAN_POINT('Ctrl Pts',(-20.670363901434,-19.8077015964858,-11.6340634729269));
#72462=CARTESIAN_POINT('Ctrl Pts',(-20.6643671010903,-19.8211609627361,
-11.6331854006886));
#72463=CARTESIAN_POINT('Ctrl Pts',(-20.6609437117122,-19.8287245057633,
-11.6326921988427));
#72464=CARTESIAN_POINT('Ctrl Pts',(-20.6517254935704,-19.8487761465608,
-11.6313851760237));
#72465=CARTESIAN_POINT('Ctrl Pts',(-20.645853133331,-19.8612283187725,-11.6305740289688));
#72466=CARTESIAN_POINT('Ctrl Pts',(-20.5998122863577,-19.9564380024344,
-11.6243741118654));
#72467=CARTESIAN_POINT('Ctrl Pts',(-20.554407193293,-20.0365606683844,-11.6191752932871));
#72468=CARTESIAN_POINT('Ctrl Pts',(-20.4267062017835,-20.2311580598958,
-11.6063012206764));
#72469=CARTESIAN_POINT('Ctrl Pts',(-20.3379453853446,-20.3408328134021,
-11.5988194733751));
#72470=CARTESIAN_POINT('Ctrl Pts',(-20.201614149999,-20.4786360478685,-11.5880939164555));
#72471=CARTESIAN_POINT('Ctrl Pts',(-20.162862190324,-20.5149654463813,-11.5851129140871));
#72472=CARTESIAN_POINT('Ctrl Pts',(-20.1088879984315,-20.5618792481894,
-11.5809842414364));
#72473=CARTESIAN_POINT('Ctrl Pts',(-20.0948309131645,-20.5737790789704,
-11.5799109528858));
#72474=CARTESIAN_POINT('Ctrl Pts',(-20.0738433234799,-20.5910808464022,
-11.578308355089));
#72475=CARTESIAN_POINT('Ctrl Pts',(-20.0670312092362,-20.5966257756623,
-11.5777881635711));
#72476=CARTESIAN_POINT('Ctrl Pts',(-20.0546983476196,-20.6065375246519,
-11.5768459455248));
#72477=CARTESIAN_POINT('Ctrl Pts',(-20.0491899118001,-20.6109195395256,
-11.5764249479618));
#72478=CARTESIAN_POINT('Ctrl Pts',(-20.0404619766761,-20.6177919047249,
-11.5757574586586));
#72479=CARTESIAN_POINT('Ctrl Pts',(-20.0372569157665,-20.6203006255508,
-11.5755122528289));
#72480=CARTESIAN_POINT('Ctrl Pts',(-20.0340353601645,-20.622807308597,-11.5752656712314));
#72481=CARTESIAN_POINT('Ctrl Pts',(-20.0340260484216,-20.6228145539121,
-11.5752649584989));
#72482=CARTESIAN_POINT('Ctrl Pts',(-20.0340073890624,-20.6228290722044,
-11.5752635302861));
#72483=CARTESIAN_POINT('Ctrl Pts',(-20.0339980418306,-20.6228363448815,
-11.5752628148353));
#72484=CARTESIAN_POINT('Ctrl Pts',(-20.0339793113038,-20.6228509180425,
-11.5752613811714));
#72485=CARTESIAN_POINT('Ctrl Pts',(-20.0339699277046,-20.6228582187622,
-11.575260662935));
#72486=CARTESIAN_POINT('Ctrl Pts',(-20.0339511244705,-20.6228728479841,
-11.5752592237021));
#72487=CARTESIAN_POINT('Ctrl Pts',(-20.0339417043797,-20.62288017684,-11.5752585026707));
#72488=CARTESIAN_POINT('Ctrl Pts',(-20.0339228272802,-20.6228948630179,
-11.5752570577801));
#72489=CARTESIAN_POINT('Ctrl Pts',(-20.0339133707563,-20.6229022199615,
-11.575256333958));
#72490=CARTESIAN_POINT('Ctrl Pts',(-20.0338936955076,-20.6229175265545,
-11.5752548279714));
#72491=CARTESIAN_POINT('Ctrl Pts',(-20.0338834764892,-20.6229254764106,
-11.5752540457842));
#72492=CARTESIAN_POINT('Ctrl Pts',(-20.0338628599782,-20.6229415146626,
-11.5752524677467));
#72493=CARTESIAN_POINT('Ctrl Pts',(-20.0338524628754,-20.62294960275,-11.5752516719262));
#72494=CARTESIAN_POINT('Ctrl Pts',(-20.0338314864396,-20.6229659203706,
-11.5752500663343));
#72495=CARTESIAN_POINT('Ctrl Pts',(-20.0338209071046,-20.6229741498998,
-11.5752492565628));
#72496=CARTESIAN_POINT('Ctrl Pts',(-20.0337995625962,-20.6229907531943,
-11.5752476227927));
#72497=CARTESIAN_POINT('Ctrl Pts',(-20.0337887971895,-20.6229991271353,
-11.5752467987762));
#72498=CARTESIAN_POINT('Ctrl Pts',(-20.0337670763489,-20.6230160224941,
-11.5752451361955));
#72499=CARTESIAN_POINT('Ctrl Pts',(-20.0337561210846,-20.6230245437742,
-11.5752442976441));
#72500=CARTESIAN_POINT('Ctrl Pts',(-20.0337340164851,-20.6230417369387,
-11.5752426056839));
#72501=CARTESIAN_POINT('Ctrl Pts',(-20.0337228670254,-20.6230504089137,
-11.5752417522654));
#72502=CARTESIAN_POINT('Ctrl Pts',(-20.0337003696859,-20.6230679068323,
-11.575240030238));
#72503=CARTESIAN_POINT('Ctrl Pts',(-20.0336890220284,-20.6230767325965,
-11.575239161646));
#72504=CARTESIAN_POINT('Ctrl Pts',(-20.0336661241077,-20.6230945413294,
-11.575237408951));
#72505=CARTESIAN_POINT('Ctrl Pts',(-20.0336545736747,-20.6231035244235,
-11.5752365248348));
#72506=CARTESIAN_POINT('Ctrl Pts',(-20.0336312657286,-20.6231216512757,
-11.5752347407489));
#72507=CARTESIAN_POINT('Ctrl Pts',(-20.0336195082778,-20.6231307949786,
-11.5752338407838));
#72508=CARTESIAN_POINT('Ctrl Pts',(-20.0335957815171,-20.6231492467439,
-11.5752320246338));
#72509=CARTESIAN_POINT('Ctrl Pts',(-20.0335838124631,-20.6231585546003,
-11.5752311084686));
#72510=CARTESIAN_POINT('Ctrl Pts',(-20.0335596577322,-20.6231773383556,
-11.5752292595536));
#72511=CARTESIAN_POINT('Ctrl Pts',(-20.0335474723098,-20.6231868140491,
-11.5752283268232));
#72512=CARTESIAN_POINT('Ctrl Pts',(-20.0335228807438,-20.6232059366429,
-11.5752264444642));
#72513=CARTESIAN_POINT('Ctrl Pts',(-20.0335104737562,-20.6232155841916,
-11.5752254947708));
#72514=CARTESIAN_POINT('Ctrl Pts',(-20.0334854335946,-20.623235054722,-11.5752235780672));
#72515=CARTESIAN_POINT('Ctrl Pts',(-20.0334728008742,-20.6232448773427,
-11.5752226110916));
#72516=CARTESIAN_POINT('Ctrl Pts',(-20.0334473043917,-20.6232647017677,
-11.5752206594516));
#72517=CARTESIAN_POINT('Ctrl Pts',(-20.0334344400561,-20.6232747040094,
-11.5752196747433));
#72518=CARTESIAN_POINT('Ctrl Pts',(-20.0334084750853,-20.6232948917387,
-11.5752176872353));
#72519=CARTESIAN_POINT('Ctrl Pts',(-20.0333953743993,-20.623305077257,-11.5752166844316));
#72520=CARTESIAN_POINT('Ctrl Pts',(-20.0333689309668,-20.6233256359919,
-11.5752146602917));
#72521=CARTESIAN_POINT('Ctrl Pts',(-20.0333555884457,-20.6233360090241,
-11.5752136389726));
#72522=CARTESIAN_POINT('Ctrl Pts',(-20.0333286557826,-20.6233569470817,
-11.575211577376));
#72523=CARTESIAN_POINT('Ctrl Pts',(-20.0333150657324,-20.6233675120263,
-11.5752105371055));
#72524=CARTESIAN_POINT('Ctrl Pts',(-20.0332876321185,-20.6233888384608,
-11.5752084371547));
#72525=CARTESIAN_POINT('Ctrl Pts',(-20.033273788974,-20.6233995996148,-11.5752073775064));
#72526=CARTESIAN_POINT('Ctrl Pts',(-20.0304283522789,-20.6256114812766,
-11.5749895680261));
#72527=CARTESIAN_POINT('Ctrl Pts',(-20.0275912314192,-20.627805355082,-11.5747723018109));
#72528=CARTESIAN_POINT('Ctrl Pts',(-20.0210760000583,-20.6328170151961,
-11.5742731672189));
#72529=CARTESIAN_POINT('Ctrl Pts',(-20.0173942073726,-20.6356299403492,
-11.5739909614331));
#72530=CARTESIAN_POINT('Ctrl Pts',(-20.0075614602168,-20.6430912598743,
-11.5732369807269));
#72531=CARTESIAN_POINT('Ctrl Pts',(-20.0013943626232,-20.6477181274058,
-11.5727637624762));
#72532=CARTESIAN_POINT('Ctrl Pts',(-19.9571208653912,-20.6805579018551,
-11.5693650709828));
#72533=CARTESIAN_POINT('Ctrl Pts',(-19.9181043615528,-20.7075150744474,
-11.5663624340112));
#72534=CARTESIAN_POINT('Ctrl Pts',(-19.8739262935959,-20.7358954797653,
-11.5629826349602));
#72535=CARTESIAN_POINT('Ctrl Pts',(-19.8696232086967,-20.7386378941255,
-11.5626536342788));
#72536=CARTESIAN_POINT('Ctrl Pts',(-19.7361460573059,-20.8230276627825,
-11.5524555510168));
#72537=CARTESIAN_POINT('Ctrl Pts',(-19.598519616211,-20.8904659096128,-11.5421895606764));
#72538=CARTESIAN_POINT('Ctrl Pts',(-19.3645534466935,-20.9751928737638,
-11.5260136986025));
#72539=CARTESIAN_POINT('Ctrl Pts',(-19.2721512865808,-21.0017084126554,
-11.5199118666605));
#72540=CARTESIAN_POINT('Ctrl Pts',(-19.1572683192196,-21.0263658600964,
-11.5126938616489));
#72541=CARTESIAN_POINT('Ctrl Pts',(-19.136212364857,-21.0305511921553,-11.5113853579743));
#72542=CARTESIAN_POINT('Ctrl Pts',(-19.1062208018131,-21.0360398455086,
-11.5095413842829));
#72543=CARTESIAN_POINT('Ctrl Pts',(-19.0973354384946,-21.0376072895067,
-11.508997540457));
#72544=CARTESIAN_POINT('Ctrl Pts',(-19.0820037345527,-21.0402109624818,
-11.5080632895427));
#72545=CARTESIAN_POINT('Ctrl Pts',(-19.0755621749183,-21.041274253237,-11.507672027193));
#72546=CARTESIAN_POINT('Ctrl Pts',(-19.0632287999549,-21.0432515257891,
-11.5069252660748));
#72547=CARTESIAN_POINT('Ctrl Pts',(-19.0573378504017,-21.0441704477533,
-11.5065696139974));
#72548=CARTESIAN_POINT('Ctrl Pts',(-19.0420304387359,-21.0464920348363,
-11.5056481048649));
#72549=CARTESIAN_POINT('Ctrl Pts',(-19.032608189996,-21.0478560991988,-11.5050834740262));
#72550=CARTESIAN_POINT('Ctrl Pts',(-19.0005573329577,-21.0522755922057,
-11.5031713655264));
#72551=CARTESIAN_POINT('Ctrl Pts',(-18.9778881304877,-21.0550285339199,
-11.5018334283228));
#72552=CARTESIAN_POINT('Ctrl Pts',(-18.7786169280041,-21.0759623889595,
-11.4901885369016));
#72553=CARTESIAN_POINT('Ctrl Pts',(-18.6004266435321,-21.0722291514489,
-11.4806531542528));
#72554=CARTESIAN_POINT('Ctrl Pts',(-18.340121870918,-21.0337954209121,-11.4663313288045));
#72555=CARTESIAN_POINT('Ctrl Pts',(-18.2563064398102,-21.0161750665568,
-11.4616421432142));
#72556=CARTESIAN_POINT('Ctrl Pts',(-18.1376708697272,-20.9836209664239,
-11.4546156891845));
#72557=CARTESIAN_POINT('Ctrl Pts',(-18.10181905066,-20.9727520979914,-11.4524391971222));
#72558=CARTESIAN_POINT('Ctrl Pts',(-18.0591116052589,-20.9585571681657,
-11.449761417048));
#72559=CARTESIAN_POINT('Ctrl Pts',(-18.0519591543124,-20.9561372945469,
-11.4493100501105));
#72560=CARTESIAN_POINT('Ctrl Pts',(-18.040869774355,-20.9523192104497,-11.448605495434));
#72561=CARTESIAN_POINT('Ctrl Pts',(-18.0369236978897,-20.9509474934926,
-11.4483538484556));
#72562=CARTESIAN_POINT('Ctrl Pts',(-18.0296186535031,-20.9483838864436,
-11.447886213624));
#72563=CARTESIAN_POINT('Ctrl Pts',(-18.0262586256018,-20.9471951908831,
-11.4476704160123));
#72564=CARTESIAN_POINT('Ctrl Pts',(-18.0186762294424,-20.9444911612744,
-11.4471818493433));
#72565=CARTESIAN_POINT('Ctrl Pts',(-18.0144556903384,-20.9429708963362,
-11.4469087911941));
#72566=CARTESIAN_POINT('Ctrl Pts',(-18.0020330502059,-20.938451523183,-11.4461018695659));
#72567=CARTESIAN_POINT('Ctrl Pts',(-17.9938447554281,-20.9354151046728,
-11.4455658617546));
#72568=CARTESIAN_POINT('Ctrl Pts',(-17.9354277464974,-20.9133405459597,
-11.4417134634449));
#72569=CARTESIAN_POINT('Ctrl Pts',(-17.8859251258482,-20.8924490031394,
-11.43829865909));
#72570=CARTESIAN_POINT('Ctrl Pts',(-17.8358135390154,-20.8690166105104,
-11.4347225586648));
#72571=CARTESIAN_POINT('Ctrl Pts',(-17.8343526425792,-20.8683314525241,
-11.4346181983414));
#72572=CARTESIAN_POINT('Ctrl Pts',(-17.6830300437104,-20.7971502314567,
-11.4237973728122));
#72573=CARTESIAN_POINT('Ctrl Pts',(-17.5419538727101,-20.7093133261423,
-11.4126524078956));
#72574=CARTESIAN_POINT('Ctrl Pts',(-17.3481817952745,-20.5544933967912,
-11.3966456620601));
#72575=CARTESIAN_POINT('Ctrl Pts',(-17.2868650396811,-20.4993462430798,
-11.391443369791));
#72576=CARTESIAN_POINT('Ctrl Pts',(-17.2150028042942,-20.4266958213404,
-11.385176868305));
#72577=CARTESIAN_POINT('Ctrl Pts',(-17.2012901825571,-20.4124385996125,
-11.3839725379746));
#72578=CARTESIAN_POINT('Ctrl Pts',(-17.1818158989105,-20.3916144394611,
-11.3822491564036));
#72579=CARTESIAN_POINT('Ctrl Pts',(-17.1758922131555,-20.3852010836314,
-11.3817231495992));
#72580=CARTESIAN_POINT('Ctrl Pts',(-17.1656427958268,-20.373965765426,-11.3808098228625));
#72581=CARTESIAN_POINT('Ctrl Pts',(-17.1612992410656,-20.3691602881184,
-11.3804217477678));
#72582=CARTESIAN_POINT('Ctrl Pts',(-17.1529554953507,-20.3598436080819,
-11.379674258925));
#72583=CARTESIAN_POINT('Ctrl Pts',(-17.1489523912764,-20.3553351095643,
-11.3793147245042));
#72584=CARTESIAN_POINT('Ctrl Pts',(-17.1395029388477,-20.3446006410547,
-11.3784638251503));
#72585=CARTESIAN_POINT('Ctrl Pts',(-17.1340736870449,-20.3383597006392,
-11.377973175));
#72586=CARTESIAN_POINT('Ctrl Pts',(-17.1150155147745,-20.3161912115734,
-11.3762444284302));
#72587=CARTESIAN_POINT('Ctrl Pts',(-17.1015864451089,-20.300092896419,-11.375014545015));
#72588=CARTESIAN_POINT('Ctrl Pts',(-16.9654659817686,-20.131899091542,-11.3624152173509));
#72589=CARTESIAN_POINT('Ctrl Pts',(-16.8641601627928,-19.9637204788182,
-11.3520147333967));
#72590=CARTESIAN_POINT('Ctrl Pts',(-16.7583034625296,-19.7160524409148,
-11.337297523916));
#72591=CARTESIAN_POINT('Ctrl Pts',(-16.7328340676586,-19.6466122475292,
-11.3332149170402));
#72592=CARTESIAN_POINT('Ctrl Pts',(-16.7009389175957,-19.5432092254425,
-11.3270137967667));
#72593=CARTESIAN_POINT('Ctrl Pts',(-16.6916268484878,-19.5101911135058,
-11.3250158591472));
#72594=CARTESIAN_POINT('Ctrl Pts',(-16.6812968559391,-19.4698348678679,
-11.3225361986492));
#72595=CARTESIAN_POINT('Ctrl Pts',(-16.6795093329084,-19.4626968212548,
-11.3220961864667));
#72596=CARTESIAN_POINT('Ctrl Pts',(-16.6767753509654,-19.4515326297265,
-11.3214055676379));
#72597=CARTESIAN_POINT('Ctrl Pts',(-16.6758033953377,-19.447512704823,-11.3211564051586));
#72598=CARTESIAN_POINT('Ctrl Pts',(-16.6740147574145,-19.4400189899952,
-11.320690976177));
#72599=CARTESIAN_POINT('Ctrl Pts',(-16.6731950765745,-19.4365459743117,
-11.3204748846718));
#72600=CARTESIAN_POINT('Ctrl Pts',(-16.671351758678,-19.428646487416,-11.319982509782));
#72601=CARTESIAN_POINT('Ctrl Pts',(-16.6703335920687,-19.4242188023378,
-11.3197059176251));
#72602=CARTESIAN_POINT('Ctrl Pts',(-16.6677291094246,-19.4127234265138,
-11.3189862838825));
#72603=CARTESIAN_POINT('Ctrl Pts',(-16.6661648165223,-19.4056508784201,
-11.3185420286667));
#72604=CARTESIAN_POINT('Ctrl Pts',(-16.6565182475577,-19.3609496466262,
-11.3157253143244));
#72605=CARTESIAN_POINT('Ctrl Pts',(-16.6494276171593,-19.3231169608967,
-11.3133019564691));
#72606=CARTESIAN_POINT('Ctrl Pts',(-16.6413177492058,-19.2722194751253,
-11.310007672671));
#72607=CARTESIAN_POINT('Ctrl Pts',(-16.639382415205,-19.2593055087793,-11.3091689049927));
#72608=CARTESIAN_POINT('Ctrl Pts',(-16.6342012907033,-19.2224073602757,
-11.3067654610224));
#72609=CARTESIAN_POINT('Ctrl Pts',(-16.6312472119723,-19.1983846788938,
-11.3051924166487));
#72610=CARTESIAN_POINT('Ctrl Pts',(-16.6239679875808,-19.1294520813687,
-11.3006636405915));
#72611=CARTESIAN_POINT('Ctrl Pts',(-16.6206657341887,-19.0844478517381,
-11.2976890347353));
#72612=CARTESIAN_POINT('Ctrl Pts',(-16.6142908378506,-18.9301203174101,
-11.2874858142536));
#72613=CARTESIAN_POINT('Ctrl Pts',(-16.6182489877911,-18.8206730275438,
-11.2802556413919));
#72614=CARTESIAN_POINT('Ctrl Pts',(-16.6368877453668,-18.6573127939604,
-11.2696875091259));
#72615=CARTESIAN_POINT('Ctrl Pts',(-16.6452611316731,-18.6028709162452,
-11.2662011542191));
#72616=CARTESIAN_POINT('Ctrl Pts',(-16.6622778449022,-18.5151571175473,
-11.2606474969773));
#72617=CARTESIAN_POINT('Ctrl Pts',(-16.6696241816054,-18.48166279303,-11.2585418233322));
#72618=CARTESIAN_POINT('Ctrl Pts',(-16.6803520144997,-18.4378640974134,
-11.2558065930408));
#72619=CARTESIAN_POINT('Ctrl Pts',(-16.6830032099105,-18.4273878113292,
-11.255153722763));
#72620=CARTESIAN_POINT('Ctrl Pts',(-16.6874778822416,-18.410258551145,-11.2540883859295));
#72621=CARTESIAN_POINT('Ctrl Pts',(-16.689253840375,-18.4035934716542,-11.2536743908326));
#72622=CARTESIAN_POINT('Ctrl Pts',(-16.6927553212726,-18.3907060898778,
-11.2528748939722));
#72623=CARTESIAN_POINT('Ctrl Pts',(-16.694476797333,-18.3844827763128,-11.2524892660685));
#72624=CARTESIAN_POINT('Ctrl Pts',(-16.6985183630847,-18.3701280152444,
-11.2516007649937));
#72625=CARTESIAN_POINT('Ctrl Pts',(-16.7008587623885,-18.3620023627581,
-11.2510985582762));
#72626=CARTESIAN_POINT('Ctrl Pts',(-16.7072862069991,-18.3401793436074,
-11.2497516399945));
#72627=CARTESIAN_POINT('Ctrl Pts',(-16.7114634404168,-18.3265088374717,
-11.2489098719704));
#72628=CARTESIAN_POINT('Ctrl Pts',(-16.7511464134438,-18.2011971691311,
-11.2412094359633));
#72629=CARTESIAN_POINT('Ctrl Pts',(-16.7957251604953,-18.0926344336082,
-11.2346692916207));
#72630=CARTESIAN_POINT('Ctrl Pts',(-16.9236328374399,-17.8424536776135,
-11.2192886908296));
#72631=CARTESIAN_POINT('Ctrl Pts',(-17.0148679750468,-17.7057676535107,
-11.2106344587158));
#72632=CARTESIAN_POINT('Ctrl Pts',(-17.1411812576398,-17.5571540339218,
-11.1994200459266));
#72633=CARTESIAN_POINT('Ctrl Pts',(-17.1619566971105,-17.5337805407049,
-11.1975944553612));
#72634=CARTESIAN_POINT('Ctrl Pts',(-17.1881102377196,-17.5056373174185,
-11.1953064843154));
#72635=CARTESIAN_POINT('Ctrl Pts',(-17.1930060659735,-17.5004222863873,
-11.1948786100337));
#72636=CARTESIAN_POINT('Ctrl Pts',(-17.200743040498,-17.4922641233642,-11.1942029030577));
#72637=CARTESIAN_POINT('Ctrl Pts',(-17.2035665008124,-17.4893041883865,
-11.1939564142953));
#72638=CARTESIAN_POINT('Ctrl Pts',(-17.2088734410351,-17.4837729199301,
-11.1934932566674));
#72639=CARTESIAN_POINT('Ctrl Pts',(-17.2113548610946,-17.4811996873116,
-11.1932767460596));
#72640=CARTESIAN_POINT('Ctrl Pts',(-17.2170517747477,-17.4753218557642,
-11.1927798054227));
#72641=CARTESIAN_POINT('Ctrl Pts',(-17.2202715451111,-17.4720214786387,
-11.192499043489));
#72642=CARTESIAN_POINT('Ctrl Pts',(-17.2302634605219,-17.461846132948,-11.1916281338745));
#72643=CARTESIAN_POINT('Ctrl Pts',(-17.2370717411971,-17.4550070449214,
-11.1910352497287));
#72644=CARTESIAN_POINT('Ctrl Pts',(-17.307521700781,-17.3851994474055,-11.1849080563275));
#72645=CARTESIAN_POINT('Ctrl Pts',(-17.3750433680705,-17.3262886361878,
-11.1791036289618));
#72646=CARTESIAN_POINT('Ctrl Pts',(-17.4930927077582,-17.235798732497,-11.1693288862232));
#72647=CARTESIAN_POINT('Ctrl Pts',(-17.54159556474,-17.2017516551551,-11.1654055534536));
#72648=CARTESIAN_POINT('Ctrl Pts',(-17.7187164040156,-17.0882035412027,
-11.1515189926062));
#72649=CARTESIAN_POINT('Ctrl Pts',(-17.8543634099491,-17.0204738700821,
-11.1417108762248));
#72650=CARTESIAN_POINT('Ctrl Pts',(-18.0159927270331,-16.9603661461655,
-11.131120101357));
#72651=CARTESIAN_POINT('Ctrl Pts',(-18.0360051205492,-16.9532646369299,
-11.1298259899217));
#72652=CARTESIAN_POINT('Ctrl Pts',(-18.0646315724498,-16.9435887865455,
-11.1279986095254));
#72653=CARTESIAN_POINT('Ctrl Pts',(-18.0731599095603,-16.9407665294933,
-11.1274571701216));
#72654=CARTESIAN_POINT('Ctrl Pts',(-18.0879102482788,-16.9359891958493,
-11.1265257547475));
#72655=CARTESIAN_POINT('Ctrl Pts',(-18.0941237452958,-16.9340084465304,
-11.1261349371457));
#72656=CARTESIAN_POINT('Ctrl Pts',(-18.1060429328967,-16.9302694130194,
-11.1253881432459));
#72657=CARTESIAN_POINT('Ctrl Pts',(-18.1117470936753,-16.9285064946601,
-11.1250320178821));
#72658=CARTESIAN_POINT('Ctrl Pts',(-18.1266094453857,-16.9239819499955,
-11.1241073753115));
#72659=CARTESIAN_POINT('Ctrl Pts',(-18.1357790966937,-16.9212582014469,
-11.1235401012597));
#72660=CARTESIAN_POINT('Ctrl Pts',(-18.1671627411517,-16.9121670380822,
-11.1216092456665));
#72661=CARTESIAN_POINT('Ctrl Pts',(-18.1894628661008,-16.9061010870061,
-11.1202554648303));
#72662=CARTESIAN_POINT('Ctrl Pts',(-18.3803334569641,-16.8575236264456,
-11.1088120330079));
#72663=CARTESIAN_POINT('Ctrl Pts',(-18.5534464133171,-16.8355599523234,
-11.099457032121));
#72664=CARTESIAN_POINT('Ctrl Pts',(-18.815462624508,-16.8347320222064,-11.0852040104298));
#72665=CARTESIAN_POINT('Ctrl Pts',(-18.9035392322254,-16.8399597932138,
-11.0803815958537));
#72666=CARTESIAN_POINT('Ctrl Pts',(-19.028856184673,-16.8552879573845,-11.0731754996182));
#72667=CARTESIAN_POINT('Ctrl Pts',(-19.0665522244061,-16.8609356371533,
-11.0709621361512));
#72668=CARTESIAN_POINT('Ctrl Pts',(-19.1115438729607,-16.8689236202211,
-11.068243488057));
#72669=CARTESIAN_POINT('Ctrl Pts',(-19.1190078669846,-16.8702902415531,
-11.0677899153578));
#72670=CARTESIAN_POINT('Ctrl Pts',(-19.1305775019918,-16.8724729369049,
-11.0670826552624));
#72671=CARTESIAN_POINT('Ctrl Pts',(-19.1346884285145,-16.8732611265988,
-11.066830527709));
#72672=CARTESIAN_POINT('Ctrl Pts',(-19.1422946906124,-16.8747428796379,
-11.0663624566346));
#72673=CARTESIAN_POINT('Ctrl Pts',(-19.145790622846,-16.8754330781707,-11.0661467062739));
#72674=CARTESIAN_POINT('Ctrl Pts',(-19.1536733537035,-16.8770100466767,
-11.0656588326937));
#72675=CARTESIAN_POINT('Ctrl Pts',(-19.1580590667994,-16.8779018978805,
-11.0653864240091));
#72676=CARTESIAN_POINT('Ctrl Pts',(-19.1693179224785,-16.8802286309406,
-11.0646846693478));
#72677=CARTESIAN_POINT('Ctrl Pts',(-19.176186751448,-16.8816837987949,-11.0642542054727));
#72678=CARTESIAN_POINT('Ctrl Pts',(-19.2171490559425,-16.8905748495753,
-11.0616736947725));
#72679=CARTESIAN_POINT('Ctrl Pts',(-19.251059575373,-16.8988181446468,-11.0594818296684));
#72680=CARTESIAN_POINT('Ctrl Pts',(-19.3010310369819,-16.9122820858429,
-11.0561842401516));
#72681=CARTESIAN_POINT('Ctrl Pts',(-19.3172601511958,-16.9168634114519,
-11.0551025635541));
#72682=CARTESIAN_POINT('Ctrl Pts',(-19.3343465824947,-16.9219079110824,
-11.0539535345151));
#72683=CARTESIAN_POINT('Ctrl Pts',(-19.3352605937441,-16.9221784297616,
-11.0538920380399));
#72684=CARTESIAN_POINT('Ctrl Pts',(-19.3406451319327,-16.9237760403013,
-11.053529574103));
#72685=CARTESIAN_POINT('Ctrl Pts',(-19.3451114216255,-16.9251172760521,
-11.0532281848643));
#72686=CARTESIAN_POINT('Ctrl Pts',(-19.3733200192054,-16.9336900866297,
-11.0513201154294));
#72687=CARTESIAN_POINT('Ctrl Pts',(-19.3969374990588,-16.9413237942379,
-11.0497023113939));
#72688=CARTESIAN_POINT('Ctrl Pts',(-19.4575335737938,-16.9620935078351,
-11.0455070938697));
#72689=CARTESIAN_POINT('Ctrl Pts',(-19.4942909164965,-16.9758455796272,
-11.0429191744637));
#72690=CARTESIAN_POINT('Ctrl Pts',(-19.6319039644652,-17.0317389395767,
-11.0331074510814));
#72691=CARTESIAN_POINT('Ctrl Pts',(-19.7298347048603,-17.0806500117974,
-11.0258811083959));
#72692=CARTESIAN_POINT('Ctrl Pts',(-19.8707066089787,-17.1652119787485,
-11.0153210185736));
#72693=CARTESIAN_POINT('Ctrl Pts',(-19.9167399781432,-17.1953439982526,
-11.0118388494714));
#72694=CARTESIAN_POINT('Ctrl Pts',(-19.9894591958985,-17.2470998201683,
-11.0062910797199));
#72695=CARTESIAN_POINT('Ctrl Pts',(-20.0168825433592,-17.2676380997185,
-11.0041872091145));
#72696=CARTESIAN_POINT('Ctrl Pts',(-20.0522837211303,-17.2955176627458,
-11.0014539428101));
#72697=CARTESIAN_POINT('Ctrl Pts',(-20.0607195885365,-17.3022664326622,
-11.0008012753337));
#72698=CARTESIAN_POINT('Ctrl Pts',(-20.0744558861512,-17.3134291034181,
-10.9997361845875));
#72699=CARTESIAN_POINT('Ctrl Pts',(-20.0797869824924,-17.3178047958252,
-10.9993222341393));
#72700=CARTESIAN_POINT('Ctrl Pts',(-20.0900678100271,-17.3263275882316,
-10.9985227648716));
#72701=CARTESIAN_POINT('Ctrl Pts',(-20.0950201309793,-17.3304714309419,
-10.9981371202192));
#72702=CARTESIAN_POINT('Ctrl Pts',(-20.1064149699957,-17.3400950147911,
-10.9972484967315));
#72703=CARTESIAN_POINT('Ctrl Pts',(-20.1128437920656,-17.3455908580134,
-10.9967461849391));
#72704=CARTESIAN_POINT('Ctrl Pts',(-20.1300532705622,-17.3604822473122,
-10.995398798728));
#72705=CARTESIAN_POINT('Ctrl Pts',(-20.1407720675095,-17.369948845206,-10.9945566710879));
#72706=CARTESIAN_POINT('Ctrl Pts',(-20.2387839507698,-17.4582945132311,
-10.9868265981097));
#72707=CARTESIAN_POINT('Ctrl Pts',(-20.3194606300363,-17.5442177894591,
-10.9802601224696));
#72708=CARTESIAN_POINT('Ctrl Pts',(-20.4942609928979,-17.7645918866182,
-10.9648656021939));
#72709=CARTESIAN_POINT('Ctrl Pts',(-20.5807193416625,-17.9041106389875,
-10.9562205072344));
#72710=CARTESIAN_POINT('Ctrl Pts',(-20.6634192119356,-18.0802252846467,
-10.9450299844428));
#72711=CARTESIAN_POINT('Ctrl Pts',(-20.6759748602771,-18.1085647248755,
-10.9432200940925));
#72712=CARTESIAN_POINT('Ctrl Pts',(-20.690648753618,-18.143751561138,-10.9409496141373));
#72713=CARTESIAN_POINT('Ctrl Pts',(-20.6933610185081,-18.1503490286847,
-10.9405229093265));
#72714=CARTESIAN_POINT('Ctrl Pts',(-20.6975744493935,-18.1607471457256,
-10.9398486397909));
#72715=CARTESIAN_POINT('Ctrl Pts',(-20.6990980709941,-18.1645387194061,
-10.9396024095043));
#72716=CARTESIAN_POINT('Ctrl Pts',(-20.7019342811252,-18.1716561977018,
-10.9391394652371));
#72717=CARTESIAN_POINT('Ctrl Pts',(-20.703249424435,-18.1749810244938,-10.9389229078748));
#72718=CARTESIAN_POINT('Ctrl Pts',(-20.7062437525257,-18.1826074448077,
-10.9384254974222));
#72719=CARTESIAN_POINT('Ctrl Pts',(-20.7079172852275,-18.1869111989385,
-10.9381443100713));
#72720=CARTESIAN_POINT('Ctrl Pts',(-20.7130574314315,-18.2002590231849,
-10.937270793411));
#72721=CARTESIAN_POINT('Ctrl Pts',(-20.7164760103375,-18.2093212852235,
-10.9366757044127));
#72722=CARTESIAN_POINT('Ctrl Pts',(-20.7565245106005,-18.3177322788394,
-10.9295352707546));
#72723=CARTESIAN_POINT('Ctrl Pts',(-20.7857089113694,-18.4196597363177,
-10.9226145016515));
#72724=CARTESIAN_POINT('Ctrl Pts',(-20.8362075107609,-18.6638812322754,
-10.9061648035184));
#72725=CARTESIAN_POINT('Ctrl Pts',(-20.8509047688548,-18.8070440802342,
-10.8966462024059));
#72726=CARTESIAN_POINT('Ctrl Pts',(-20.8510404642358,-19.0125966095008,
-10.8835935804314));
#72727=CARTESIAN_POINT('Ctrl Pts',(-20.8483582573966,-19.074567055652,-10.8797325381029));
#72728=CARTESIAN_POINT('Ctrl Pts',(-20.8418780036544,-19.1487067130386,
-10.875199750235));
#72729=CARTESIAN_POINT('Ctrl Pts',(-20.8406878626907,-19.16106809596,-10.8744468386955));
#72730=CARTESIAN_POINT('Ctrl Pts',(-20.8385539133339,-19.1813590539228,
-10.8732154675641));
#72731=CARTESIAN_POINT('Ctrl Pts',(-20.8376739010711,-19.1892949018066,
-10.872735012191));
#72732=CARTESIAN_POINT('Ctrl Pts',(-20.8360103029197,-19.2035598415205,
-10.8718733679328));
#72733=CARTESIAN_POINT('Ctrl Pts',(-20.8352429788777,-19.2098906988285,
-10.8714916715242));
#72734=CARTESIAN_POINT('Ctrl Pts',(-20.8335469916007,-19.2233732429876,
-10.8706802559566));
#72735=CARTESIAN_POINT('Ctrl Pts',(-20.8326103659402,-19.2305238605445,
-10.8702507931481));
#72736=CARTESIAN_POINT('Ctrl Pts',(-20.8299874451884,-19.2497836479508,
-10.8690963550652));
#72737=CARTESIAN_POINT('Ctrl Pts',(-20.8282327461388,-19.2618833422834,
-10.8683735464714));
#72738=CARTESIAN_POINT('Ctrl Pts',(-20.8189028622638,-19.3225155765967,
-10.8647630127091));
#72739=CARTESIAN_POINT('Ctrl Pts',(-20.8097446709085,-19.3707915360266,
-10.8619258064585));
#72740=CARTESIAN_POINT('Ctrl Pts',(-20.7790242589775,-19.5067116634044,
-10.8540036864043));
#72741=CARTESIAN_POINT('Ctrl Pts',(-20.7535279435943,-19.5933555926682,
-10.8490364150279));
#72742=CARTESIAN_POINT('Ctrl Pts',(-20.7225805823871,-19.6781103685755,
-10.8441190550425));
#72743=CARTESIAN_POINT('Origin',(-18.734,-18.952,0.));
#72744=CARTESIAN_POINT('',(-20.722580582123,-19.6781103692989,-10.0464611886058));
#72745=CARTESIAN_POINT('',(-20.7219729237028,-19.6778789621695,-10.2662522608197));
#72746=CARTESIAN_POINT('',(-20.7225805821191,-19.6781103693095,0.));
#72747=CARTESIAN_POINT('',(-20.8538228835136,-18.9530774369207,-10.3109437209775));
#72748=CARTESIAN_POINT('Ctrl Pts',(-20.7219729237027,-19.6778789621698,
-10.2662522608197));
#72749=CARTESIAN_POINT('Ctrl Pts',(-20.787539735307,-19.5036327148231,-10.2774434356492));
#72750=CARTESIAN_POINT('Ctrl Pts',(-20.8444160839083,-19.2611105174517,
-10.2923405890351));
#72751=CARTESIAN_POINT('Ctrl Pts',(-20.8542039878978,-19.0144660717244,
-10.307237742421));
#72752=CARTESIAN_POINT('Ctrl Pts',(-20.8538228835136,-18.9530774369207,
-10.3109437209775));
#72753=CARTESIAN_POINT('Ctrl Pts',(-20.8509997772493,-18.9529711470399,
-10.3093226856846));
#72754=CARTESIAN_POINT('Ctrl Pts',(-20.8510794193682,-18.7793595916912,
-10.3204900561849));
#72755=CARTESIAN_POINT('Ctrl Pts',(-20.8298038944403,-18.6063867465604,
-10.3322030597167));
#72756=CARTESIAN_POINT('Ctrl Pts',(-20.7727769716693,-18.3785693060707,
-10.3473694074294));
#72757=CARTESIAN_POINT('Ctrl Pts',(-20.7553480080759,-18.3198705581746,
-10.3512605836352));
#72758=CARTESIAN_POINT('Ctrl Pts',(-20.7233403127886,-18.2270290779853,
-10.3573784312497));
#72759=CARTESIAN_POINT('Ctrl Pts',(-20.7103668064488,-18.1923736213319,
-10.3596539082093));
#72760=CARTESIAN_POINT('Ctrl Pts',(-20.6923256027683,-18.1477778926987,
-10.3625732349727));
#72761=CARTESIAN_POINT('Ctrl Pts',(-20.6880792039238,-18.1375143730626,
-10.363244502009));
#72762=CARTESIAN_POINT('Ctrl Pts',(-20.6810393040183,-18.1208709831831,
-10.3643321719418));
#72763=CARTESIAN_POINT('Ctrl Pts',(-20.6782947910262,-18.1144707399865,
-10.364750228847));
#72764=CARTESIAN_POINT('Ctrl Pts',(-20.6729543848587,-18.1021845649081,
-10.3655523895481));
#72765=CARTESIAN_POINT('Ctrl Pts',(-20.6703631503778,-18.0962967035517,
-10.3659366467752));
#72766=CARTESIAN_POINT('Ctrl Pts',(-20.6643661714385,-18.082836969157,-10.366814742967));
#72767=CARTESIAN_POINT('Ctrl Pts',(-20.6609426267439,-18.0752731062338,
-10.3673079656299));
#72768=CARTESIAN_POINT('Ctrl Pts',(-20.6517237262486,-18.055220055506,-10.3686150802324));
#72769=CARTESIAN_POINT('Ctrl Pts',(-20.6458508213901,-18.0427668015452,
-10.3694262976481));
#72770=CARTESIAN_POINT('Ctrl Pts',(-20.5997890217786,-17.9475145479618,
-10.3756289861628));
#72771=CARTESIAN_POINT('Ctrl Pts',(-20.5543581860886,-17.8673531545177,
-10.3808303029813));
#72772=CARTESIAN_POINT('Ctrl Pts',(-20.4266263404313,-17.6727378440846,
-10.3937058489615));
#72773=CARTESIAN_POINT('Ctrl Pts',(-20.3378682033472,-17.5630795093536,
-10.4011868368574));
#72774=CARTESIAN_POINT('Ctrl Pts',(-20.2015575085882,-17.425310348179,-10.4119104618055));
#72775=CARTESIAN_POINT('Ctrl Pts',(-20.162822177308,-17.3889988003595,-10.414890161463));
#72776=CARTESIAN_POINT('Ctrl Pts',(-20.1088699145807,-17.3421053719128,
-10.4190171484939));
#72777=CARTESIAN_POINT('Ctrl Pts',(-20.0948169897376,-17.3302093016445,
-10.4200901189935));
#72778=CARTESIAN_POINT('Ctrl Pts',(-20.0738350991701,-17.3129124410464,
-10.4216922816779));
#72779=CARTESIAN_POINT('Ctrl Pts',(-20.0670244445388,-17.3073687515419,
-10.4222123618597));
#72780=CARTESIAN_POINT('Ctrl Pts',(-20.054694019646,-17.2974590259749,-10.423154393972));
#72781=CARTESIAN_POINT('Ctrl Pts',(-20.0491865537469,-17.2930778035314,
-10.4235753175168));
#72782=CARTESIAN_POINT('Ctrl Pts',(-20.040459814539,-17.2862064002273,-10.4242427154831));
#72783=CARTESIAN_POINT('Ctrl Pts',(-20.0372549728867,-17.2836978573849,
-10.4244879045828));
#72784=CARTESIAN_POINT('Ctrl Pts',(-20.0340336348583,-17.2811913489641,
-10.4247344695675));
#72785=CARTESIAN_POINT('Ctrl Pts',(-20.0340243211539,-17.2811841021382,
-10.4247351824503));
#72786=CARTESIAN_POINT('Ctrl Pts',(-20.0340056579227,-17.2811695808643,
-10.4247366109597));
#72787=CARTESIAN_POINT('Ctrl Pts',(-20.033996308311,-17.2811623063511,-10.4247373265928));
#72788=CARTESIAN_POINT('Ctrl Pts',(-20.0339775732599,-17.2811477297012,
-10.4247387606032));
#72789=CARTESIAN_POINT('Ctrl Pts',(-20.0339681873699,-17.2811404272149,
-10.4247394790151));
#72790=CARTESIAN_POINT('Ctrl Pts',(-20.0339493787154,-17.2811257938074,
-10.4247409186631));
#72791=CARTESIAN_POINT('Ctrl Pts',(-20.0339399567985,-17.2811184635465,
-10.4247416398344));
#72792=CARTESIAN_POINT('Ctrl Pts',(-20.03392107619,-17.2811037746705,-10.4247430849939));
#72793=CARTESIAN_POINT('Ctrl Pts',(-20.0339116170876,-17.2810964157366,
-10.4247438090134));
#72794=CARTESIAN_POINT('Ctrl Pts',(-20.033891928788,-17.2810810990237,-10.4247453159992));
#72795=CARTESIAN_POINT('Ctrl Pts',(-20.0338816997124,-17.2810731413611,
-10.4247460989564));
#72796=CARTESIAN_POINT('Ctrl Pts',(-20.0338610630875,-17.2810570874973,
-10.4247476785337));
#72797=CARTESIAN_POINT('Ctrl Pts',(-20.0338506553949,-17.28104899119,-10.424748475165));
#72798=CARTESIAN_POINT('Ctrl Pts',(-20.0338296579193,-17.2810326572391,
-10.4247500823675));
#72799=CARTESIAN_POINT('Ctrl Pts',(-20.0338190678582,-17.2810244193848,
-10.4247508929602));
#72800=CARTESIAN_POINT('Ctrl Pts',(-20.0337977012581,-17.2810077989438,
-10.4247525284215));
#72801=CARTESIAN_POINT('Ctrl Pts',(-20.0337869252412,-17.280999416769,-10.4247533532503));
#72802=CARTESIAN_POINT('Ctrl Pts',(-20.0337651829476,-17.2809825047624,
-10.4247550174734));
#72803=CARTESIAN_POINT('Ctrl Pts',(-20.0337542164602,-17.2809739747727,
-10.424755856884));
#72804=CARTESIAN_POINT('Ctrl Pts',(-20.0337320891588,-17.2809567639912,
-10.4247575505822));
#72805=CARTESIAN_POINT('Ctrl Pts',(-20.0337209284337,-17.2809480832747,
-10.4247584048631));
#72806=CARTESIAN_POINT('Ctrl Pts',(-20.0336984085359,-17.280930567853,-10.4247601286175));
#72807=CARTESIAN_POINT('Ctrl Pts',(-20.0336870491494,-17.2809217329879,
-10.4247609981075));
#72808=CARTESIAN_POINT('Ctrl Pts',(-20.0336641275913,-17.2809039059147,
-10.4247627526122));
#72809=CARTESIAN_POINT('Ctrl Pts',(-20.0336525653564,-17.2808949136643,
-10.4247636376319));
#72810=CARTESIAN_POINT('Ctrl Pts',(-20.0336292333611,-17.2808767681539,
-10.424765423559));
#72811=CARTESIAN_POINT('Ctrl Pts',(-20.0336174638869,-17.2808676151237,
-10.4247663244446));
#72812=CARTESIAN_POINT('Ctrl Pts',(-20.0335937128453,-17.2808491445224,
-10.4247681424534));
#72813=CARTESIAN_POINT('Ctrl Pts',(-20.0335817313709,-17.2808398270312,
-10.4247690595696));
#72814=CARTESIAN_POINT('Ctrl Pts',(-20.0308946390714,-17.2787502341517,
-10.4249747421063));
#72815=CARTESIAN_POINT('Ctrl Pts',(-20.0282145952773,-17.2766764298895,
-10.4251799677509));
#72816=CARTESIAN_POINT('Ctrl Pts',(-20.0219399979129,-17.2718452196714,
-10.4256606326095));
#72817=CARTESIAN_POINT('Ctrl Pts',(-20.0183415796849,-17.2690929229766,
-10.4259364266806));
#72818=CARTESIAN_POINT('Ctrl Pts',(-20.0073758593416,-17.2607613038662,
-10.4267772194265));
#72819=CARTESIAN_POINT('Ctrl Pts',(-19.999980946506,-17.2552187405541,-10.4273446934099));
#72820=CARTESIAN_POINT('Ctrl Pts',(-19.9401409584356,-17.2109769932916,
-10.4319388993246));
#72821=CARTESIAN_POINT('Ctrl Pts',(-19.8859754012468,-17.174673903762,-10.4361100043851));
#72822=CARTESIAN_POINT('Ctrl Pts',(-19.7079132361217,-17.0668940801398,
-10.4496551322327));
#72823=CARTESIAN_POINT('Ctrl Pts',(-19.5784113480963,-17.0054378217447,
-10.4592335235597));
#72824=CARTESIAN_POINT('Ctrl Pts',(-19.3473606168183,-16.9232236623335,
-10.4751490732572));
#72825=CARTESIAN_POINT('Ctrl Pts',(-19.2486572182595,-16.8959654732595,
-10.4816192969437));
#72826=CARTESIAN_POINT('Ctrl Pts',(-19.1338549727237,-16.873052269362,-10.4887581511366));
#72827=CARTESIAN_POINT('Ctrl Pts',(-19.1193234232712,-16.8703099311315,
-10.4896550406672));
#72828=CARTESIAN_POINT('Ctrl Pts',(-19.097119593072,-16.8663601826252,-10.4910154555303));
#72829=CARTESIAN_POINT('Ctrl Pts',(-19.0894676473943,-16.8650423960097,
-10.4914824805236));
#72830=CARTESIAN_POINT('Ctrl Pts',(-19.0755338120865,-16.8627216270455,
-10.492329684243));
#72831=CARTESIAN_POINT('Ctrl Pts',(-19.0692543488453,-16.8617048085398,
-10.4927102982376));
#72832=CARTESIAN_POINT('Ctrl Pts',(-19.0556888634034,-16.8595708836126,
-10.4935300100819));
#72833=CARTESIAN_POINT('Ctrl Pts',(-19.04840138055,-16.8584634930436,-10.4939687954227));
#72834=CARTESIAN_POINT('Ctrl Pts',(-19.0286282160052,-16.8555643791738,
-10.4951551855948));
#72835=CARTESIAN_POINT('Ctrl Pts',(-19.016131939635,-16.8538461264881,-10.495900462443));
#72836=CARTESIAN_POINT('Ctrl Pts',(-18.955303979036,-16.8460354798875,-10.4995072602386));
#72837=CARTESIAN_POINT('Ctrl Pts',(-18.906784966137,-16.8415005559573,-10.5023194526611));
#72838=CARTESIAN_POINT('Ctrl Pts',(-18.8174408792678,-16.8362520116136,
-10.5074055673432));
#72839=CARTESIAN_POINT('Ctrl Pts',(-18.7766700749188,-16.8350372132828,
-10.5096915279946));
#72840=CARTESIAN_POINT('Ctrl Pts',(-18.6015149717955,-16.8348810016189,
-10.5194116910763));
#72841=CARTESIAN_POINT('Ctrl Pts',(-18.4674400710306,-16.8475546496889,
-10.5265773662841));
#72842=CARTESIAN_POINT('Ctrl Pts',(-18.2739305793158,-16.8846462265019,
-10.5374062461092));
#72843=CARTESIAN_POINT('Ctrl Pts',(-18.2129475501003,-16.8991681280966,
-10.5408963489381));
#72844=CARTESIAN_POINT('Ctrl Pts',(-18.122979145102,-16.9248596307359,-10.5462782755912));
#72845=CARTESIAN_POINT('Ctrl Pts',(-18.0934463843998,-16.9339971752689,
-10.5480834842668));
#72846=CARTESIAN_POINT('Ctrl Pts',(-18.0573649175315,-16.9460327110222,
-10.5503487474621));
#72847=CARTESIAN_POINT('Ctrl Pts',(-18.0506153222674,-16.9483220872038,
-10.5507751013617));
#72848=CARTESIAN_POINT('Ctrl Pts',(-18.0400157032895,-16.9519771294003,
-10.551448939555));
#72849=CARTESIAN_POINT('Ctrl Pts',(-18.0361577805577,-16.9533199547908,
-10.5516950922531));
#72850=CARTESIAN_POINT('Ctrl Pts',(-18.0289301690009,-16.9558591433505,
-10.552157972696));
#72851=CARTESIAN_POINT('Ctrl Pts',(-18.0255596165151,-16.9570528807664,
-10.5523745443152));
#72852=CARTESIAN_POINT('Ctrl Pts',(-18.0178412860028,-16.9598084833635,
-10.5528720968145));
#72853=CARTESIAN_POINT('Ctrl Pts',(-18.013495597809,-16.9613760405134,-10.5531534126666));
#72854=CARTESIAN_POINT('Ctrl Pts',(-18.0000447644388,-16.9662777804661,
-10.5540277177136));
#72855=CARTESIAN_POINT('Ctrl Pts',(-17.9909575203233,-16.9696602495671,
-10.5546234736399));
#72856=CARTESIAN_POINT('Ctrl Pts',(-17.8885299935141,-17.0085892236044,
-10.5613935871788));
#72857=CARTESIAN_POINT('Ctrl Pts',(-17.7978047603853,-17.0506324095215,
-10.567902760316));
#72858=CARTESIAN_POINT('Ctrl Pts',(-17.6933381517651,-17.1083374168986,
-10.5757659955355));
#72859=CARTESIAN_POINT('Ctrl Pts',(-17.6764101759332,-17.1179954858049,
-10.5770525672602));
#72860=CARTESIAN_POINT('Ctrl Pts',(-17.565739975038,-17.1831789414606,-10.5855376920495));
#72861=CARTESIAN_POINT('Ctrl Pts',(-17.4762631147445,-17.2456410613889,
-10.5927393033561));
#72862=CARTESIAN_POINT('Ctrl Pts',(-17.333975943132,-17.3622679320992,-10.6045598990233));
#72863=CARTESIAN_POINT('Ctrl Pts',(-17.2785272354868,-17.4128714857016,
-10.6092790984574));
#72864=CARTESIAN_POINT('Ctrl Pts',(-17.2126800076809,-17.4797133151403,
-10.615027018531));
#72865=CARTESIAN_POINT('Ctrl Pts',(-17.1996621532909,-17.4932848086699,
-10.6161711480857));
#72866=CARTESIAN_POINT('Ctrl Pts',(-17.1809881198082,-17.5132796428476,
-10.6178243089738));
#72867=CARTESIAN_POINT('Ctrl Pts',(-17.1751876009825,-17.5195663805517,
-10.6183395332425));
#72868=CARTESIAN_POINT('Ctrl Pts',(-17.1650808492612,-17.530654408848,-10.6192403576289));
#72869=CARTESIAN_POINT('Ctrl Pts',(-17.1607581863951,-17.5354405101109,
-10.6196266534362));
#72870=CARTESIAN_POINT('Ctrl Pts',(-17.1524043866532,-17.5447753360454,
-10.6203752060694));
#72871=CARTESIAN_POINT('Ctrl Pts',(-17.1483708394203,-17.5493218097851,
-10.6207375623374));
#72872=CARTESIAN_POINT('Ctrl Pts',(-17.1387709985879,-17.5602367399885,
-10.6216022347255));
#72873=CARTESIAN_POINT('Ctrl Pts',(-17.1332231541187,-17.5666213399545,
-10.6221037800799));
#72874=CARTESIAN_POINT('Ctrl Pts',(-17.1133174192485,-17.5898085889461,
-10.6239102185812));
#72875=CARTESIAN_POINT('Ctrl Pts',(-17.099184289931,-17.6068029451931,-10.6252058828932));
#72876=CARTESIAN_POINT('Ctrl Pts',(-16.9688591091537,-17.7686005169474,
-10.637289142984));
#72877=CARTESIAN_POINT('Ctrl Pts',(-16.8719253322914,-17.9278707889274,
-10.6472193997445));
#72878=CARTESIAN_POINT('Ctrl Pts',(-16.7646839404573,-18.1710399562158,
-10.6617076839513));
#72879=CARTESIAN_POINT('Ctrl Pts',(-16.7365514954819,-18.246095048847,-10.6661125560944));
#72880=CARTESIAN_POINT('Ctrl Pts',(-16.7020314371913,-18.3569453537787,
-10.6727537259724));
#72881=CARTESIAN_POINT('Ctrl Pts',(-16.6922024433507,-18.3915995524339,
-10.6748487593431));
#72882=CARTESIAN_POINT('Ctrl Pts',(-16.6814095747168,-18.4337169889009,
-10.6774362028975));
#72883=CARTESIAN_POINT('Ctrl Pts',(-16.679594672032,-18.4409584378852,-10.6778825324453));
#72884=CARTESIAN_POINT('Ctrl Pts',(-16.6768283685089,-18.4522488847521,
-10.678580906465));
#72885=CARTESIAN_POINT('Ctrl Pts',(-16.6758505138807,-18.4562914256275,
-10.6788314533667));
#72886=CARTESIAN_POINT('Ctrl Pts',(-16.6740564191552,-18.463805203277,-10.6792981009882));
#72887=CARTESIAN_POINT('Ctrl Pts',(-16.6732370343696,-18.4672756301861,
-10.679514018183));
#72888=CARTESIAN_POINT('Ctrl Pts',(-16.6714010003066,-18.475140782277,-10.6800042231805));
#72889=CARTESIAN_POINT('Ctrl Pts',(-16.670389631716,-18.4795366743295,-10.6802788085906));
#72890=CARTESIAN_POINT('Ctrl Pts',(-16.6678144193574,-18.4908958046621,
-10.6809898501807));
#72891=CARTESIAN_POINT('Ctrl Pts',(-16.6662717386905,-18.4978637135345,
-10.6814274735406));
#72892=CARTESIAN_POINT('Ctrl Pts',(-16.6570111496377,-18.5407170673958,
-10.6841272778506));
#72893=CARTESIAN_POINT('Ctrl Pts',(-16.6501929059821,-18.5767881192622,
-10.6864357473103));
#72894=CARTESIAN_POINT('Ctrl Pts',(-16.616998226469,-18.7814180918168,-10.6996659054849));
#72895=CARTESIAN_POINT('Ctrl Pts',(-16.6101361683581,-18.9525036638496,
-10.7111777637828));
#72896=CARTESIAN_POINT('Ctrl Pts',(-16.6315580065215,-19.2175250193883,
-10.7284557937702));
#72897=CARTESIAN_POINT('Ctrl Pts',(-16.6456362937023,-19.3118710039997,
-10.7345086108143));
#72898=CARTESIAN_POINT('Ctrl Pts',(-16.6705999748074,-19.4258421294952,
-10.7416752218674));
#72899=CARTESIAN_POINT('Ctrl Pts',(-16.6754903028518,-19.446655341638,-10.7429782936529));
#72900=CARTESIAN_POINT('Ctrl Pts',(-16.6828881243915,-19.4761280468211,
-10.7448160072132));
#72901=CARTESIAN_POINT('Ctrl Pts',(-16.685136805431,-19.4848505884275,-10.7453589457638));
#72902=CARTESIAN_POINT('Ctrl Pts',(-16.689110543327,-19.4998674089627,-10.7462921285862));
#72903=CARTESIAN_POINT('Ctrl Pts',(-16.6908091466947,-19.5061684998858,
-10.7466832229823));
#72904=CARTESIAN_POINT('Ctrl Pts',(-16.6941161130725,-19.518214015266,-10.7474299942396));
#72905=CARTESIAN_POINT('Ctrl Pts',(-16.6957196698045,-19.5239596837978,
-10.7477858228173));
#72906=CARTESIAN_POINT('Ctrl Pts',(-16.6999500459863,-19.538873701343,-10.7487085025316));
#72907=CARTESIAN_POINT('Ctrl Pts',(-16.7026145921048,-19.548031279268,-10.7492741211305));
#72908=CARTESIAN_POINT('Ctrl Pts',(-16.7118975924196,-19.5791498444912,
-10.7511932387757));
#72909=CARTESIAN_POINT('Ctrl Pts',(-16.7188111594146,-19.6010216263463,
-10.7525371004372));
#72910=CARTESIAN_POINT('Ctrl Pts',(-16.7819128938809,-19.7899118602451,
-10.7641101260313));
#72911=CARTESIAN_POINT('Ctrl Pts',(-16.85839321266,-19.9494197709131,-10.7735810672016));
#72912=CARTESIAN_POINT('Ctrl Pts',(-17.0005664995918,-20.1703504946566,
-10.7878777857968));
#72913=CARTESIAN_POINT('Ctrl Pts',(-17.0517807733767,-20.2401404179923,
-10.7926143204675));
#72914=CARTESIAN_POINT('Ctrl Pts',(-17.1312328492206,-20.3355632306599,
-10.7997046831101));
#72915=CARTESIAN_POINT('Ctrl Pts',(-17.1561189047737,-20.3638783966051,
-10.8018943724424));
#72916=CARTESIAN_POINT('Ctrl Pts',(-17.1868891626435,-20.3970585714183,
-10.8045867817025));
#72917=CARTESIAN_POINT('Ctrl Pts',(-17.192062284342,-20.4025772282142,-10.8050389433295));
#72918=CARTESIAN_POINT('Ctrl Pts',(-17.2001402234296,-20.4111026912632,
-10.8057444727771));
#72919=CARTESIAN_POINT('Ctrl Pts',(-17.2030246197794,-20.4141288801937,
-10.8059962929739));
#72920=CARTESIAN_POINT('Ctrl Pts',(-17.2083844745054,-20.4197189683043,
-10.8064640846992));
#72921=CARTESIAN_POINT('Ctrl Pts',(-17.2108574504169,-20.4222851677875,
-10.8066798649331));
#72922=CARTESIAN_POINT('Ctrl Pts',(-17.216455278627,-20.4280647373772,-10.8071681802184));
#72923=CARTESIAN_POINT('Ctrl Pts',(-17.219583845293,-20.4312744166662,-10.807441003048));
#72924=CARTESIAN_POINT('Ctrl Pts',(-17.2288257878519,-20.4406959231759,
-10.8082465997509));
#72925=CARTESIAN_POINT('Ctrl Pts',(-17.2349672719974,-20.4468798730914,
-10.8087815076653));
#72926=CARTESIAN_POINT('Ctrl Pts',(-17.2789207686384,-20.4905940675539,
-10.8126055245112));
#72927=CARTESIAN_POINT('Ctrl Pts',(-17.3180962975981,-20.5267199583551,
-10.8159914478675));
#72928=CARTESIAN_POINT('Ctrl Pts',(-17.3723156933874,-20.5730585810309,
-10.8206007893428));
#72929=CARTESIAN_POINT('Ctrl Pts',(-17.3861921526224,-20.584614178082,-10.821774126052));
#72930=CARTESIAN_POINT('Ctrl Pts',(-17.4376053551246,-20.6263262087608,
-10.8260938079698));
#72931=CARTESIAN_POINT('Ctrl Pts',(-17.4760193957113,-20.6553766160652,
-10.8292679942957));
#72932=CARTESIAN_POINT('Ctrl Pts',(-17.6048294285987,-20.7460531032254,
-10.8396736914859));
#72933=CARTESIAN_POINT('Ctrl Pts',(-17.6990215663492,-20.8019934660045,
-10.8469061992004));
#72934=CARTESIAN_POINT('Ctrl Pts',(-17.8465280207515,-20.8747891520258,
-10.857479235492));
#72935=CARTESIAN_POINT('Ctrl Pts',(-17.8968715958033,-20.8972355880089,
-10.8609681432704));
#72936=CARTESIAN_POINT('Ctrl Pts',(-17.9798872212718,-20.9304285466725,
-10.8665253906586));
#72937=CARTESIAN_POINT('Ctrl Pts',(-18.0120433432207,-20.9423880022128,
-10.8686321634593));
#72938=CARTESIAN_POINT('Ctrl Pts',(-18.0546963311517,-20.9570816302145,
-10.8713685909166));
#72939=CARTESIAN_POINT('Ctrl Pts',(-18.0649421710351,-20.9605236982969,
-10.8720215847374));
#72940=CARTESIAN_POINT('Ctrl Pts',(-18.0817695475518,-20.9660337680627,
-10.8730870714796));
#72941=CARTESIAN_POINT('Ctrl Pts',(-18.0883355333232,-20.9681483031316,
-10.8735010937725));
#72942=CARTESIAN_POINT('Ctrl Pts',(-18.1010673092143,-20.9721799173819,
-10.8743006074492));
#72943=CARTESIAN_POINT('Ctrl Pts',(-18.10723175743,-20.9741009522746,-10.8746862251603));
#72944=CARTESIAN_POINT('Ctrl Pts',(-18.1214882355998,-20.9784722600781,
-10.8755746517272));
#72945=CARTESIAN_POINT('Ctrl Pts',(-18.1295863827775,-20.980902330048,-10.8760767944877));
#72946=CARTESIAN_POINT('Ctrl Pts',(-18.1514104520049,-20.9873089753633,
-10.8774234279941));
#72947=CARTESIAN_POINT('Ctrl Pts',(-18.165162588493,-20.9911952385216,-10.8782649771697));
#72948=CARTESIAN_POINT('Ctrl Pts',(-18.2917245321447,-21.0255808407728,
-10.8859481709596));
#72949=CARTESIAN_POINT('Ctrl Pts',(-18.40684581723,-21.0468318545523,-10.8924729976926));
#72950=CARTESIAN_POINT('Ctrl Pts',(-18.6851915739438,-21.074693681077,-10.9077869288836));
#72951=CARTESIAN_POINT('Ctrl Pts',(-18.848546917264,-21.0721598589193,-10.9163926288912));
#72952=CARTESIAN_POINT('Ctrl Pts',(-19.0420772806209,-21.0467137523404,
-10.9276020963078));
#72953=CARTESIAN_POINT('Ctrl Pts',(-19.0740756661868,-21.0417573060092,
-10.9294907074751));
#72954=CARTESIAN_POINT('Ctrl Pts',(-19.1130639760767,-21.0347990264385,
-10.9318488356548));
#72955=CARTESIAN_POINT('Ctrl Pts',(-19.1201754921969,-21.0334921975084,
-10.9322812936415));
#72956=CARTESIAN_POINT('Ctrl Pts',(-19.1313162829863,-21.0313858816296,
-10.932962633488));
#72957=CARTESIAN_POINT('Ctrl Pts',(-19.1353502400238,-21.0306110404835,
-10.9332101339289));
#72958=CARTESIAN_POINT('Ctrl Pts',(-19.1428880004036,-21.0291404295187,
-10.9336741375203));
#72959=CARTESIAN_POINT('Ctrl Pts',(-19.1463923064997,-21.0284475302056,
-10.9338904760341));
#72960=CARTESIAN_POINT('Ctrl Pts',(-19.1543899819773,-21.0268451220722,
-10.9343856275422));
#72961=CARTESIAN_POINT('Ctrl Pts',(-19.1588821457535,-21.0259298876386,
-10.9346647634294));
#72962=CARTESIAN_POINT('Ctrl Pts',(-19.1705975386467,-21.0235033306079,
-10.935395332013));
#72963=CARTESIAN_POINT('Ctrl Pts',(-19.1778158289252,-21.021968832088,-10.9358480386525));
#72964=CARTESIAN_POINT('Ctrl Pts',(-19.2250032895863,-21.0116793339687,
-10.9388236899474));
#72965=CARTESIAN_POINT('Ctrl Pts',(-19.2647167027151,-21.0018054699887,
-10.9414041654556));
#72966=CARTESIAN_POINT('Ctrl Pts',(-19.3142212966261,-20.9879622664121,
-10.9446963827874));
#72967=CARTESIAN_POINT('Ctrl Pts',(-19.324305351243,-20.9850614080953,-10.9453709994192));
#72968=CARTESIAN_POINT('Ctrl Pts',(-19.3350136213566,-20.9818945985568,
-10.9460913570241));
#72969=CARTESIAN_POINT('Ctrl Pts',(-19.3356598796412,-20.9817031417266,
-10.9461348470336));
#72970=CARTESIAN_POINT('Ctrl Pts',(-19.3407296351053,-20.9801985705268,
-10.9464761375737));
#72971=CARTESIAN_POINT('Ctrl Pts',(-19.3451488947369,-20.9788713130255,
-10.9467743596194));
#72972=CARTESIAN_POINT('Ctrl Pts',(-19.3733140799957,-20.9703118395231,
-10.9486794861855));
#72973=CARTESIAN_POINT('Ctrl Pts',(-19.3969350472084,-20.9626770591781,
-10.9502975271165));
#72974=CARTESIAN_POINT('Ctrl Pts',(-19.457534237769,-20.9419062439879,-10.9544929616215));
#72975=CARTESIAN_POINT('Ctrl Pts',(-19.4942912559967,-20.9281542829556,
-10.9570808584803));
#72976=CARTESIAN_POINT('Ctrl Pts',(-19.6319039834722,-20.8722610513795,
-10.9668925590682));
#72977=CARTESIAN_POINT('Ctrl Pts',(-19.7298347209471,-20.8233499794817,
-10.9741189015601));
#72978=CARTESIAN_POINT('Ctrl Pts',(-19.8707066194332,-20.7387880145052,
-10.9846789909834));
#72979=CARTESIAN_POINT('Ctrl Pts',(-19.9167399858445,-20.708655996465,-10.9881611598825));
#72980=CARTESIAN_POINT('Ctrl Pts',(-19.9894591996748,-20.6569001770201,
-10.9937089293397));
#72981=CARTESIAN_POINT('Ctrl Pts',(-20.0168825458729,-20.6363618983359,
-10.9958127998496));
#72982=CARTESIAN_POINT('Ctrl Pts',(-20.0522837221869,-20.6084823364114,
-10.9985460660424));
#72983=CARTESIAN_POINT('Ctrl Pts',(-20.0607195893577,-20.6017335666755,
-10.9991987335007));
#72984=CARTESIAN_POINT('Ctrl Pts',(-20.0744558866247,-20.5905708961939,
-11.0002638242202));
#72985=CARTESIAN_POINT('Ctrl Pts',(-20.0797869828508,-20.5861952038791,
-11.0006777746594));
#72986=CARTESIAN_POINT('Ctrl Pts',(-20.0900678101864,-20.5776724116351,
-11.0014772439116));
#72987=CARTESIAN_POINT('Ctrl Pts',(-20.0950201310551,-20.573528568994,-11.0018628885576));
#72988=CARTESIAN_POINT('Ctrl Pts',(-20.1064149699122,-20.5639049852794,
-11.0027515120329));
#72989=CARTESIAN_POINT('Ctrl Pts',(-20.1128437919051,-20.5584091421238,
-11.0032538238192));
#72990=CARTESIAN_POINT('Ctrl Pts',(-20.1300532702657,-20.5435177529472,
-11.0046012100195));
#72991=CARTESIAN_POINT('Ctrl Pts',(-20.1407720671548,-20.5340511551088,
-11.0054433376549));
#72992=CARTESIAN_POINT('Ctrl Pts',(-20.2387839559125,-20.4457054821749,
-11.0131734110647));
#72993=CARTESIAN_POINT('Ctrl Pts',(-20.3194606398749,-20.3597822000834,
-11.0197398870946));
#72994=CARTESIAN_POINT('Ctrl Pts',(-20.4942610015816,-20.1394080997281,
-11.0351344074215));
#72995=CARTESIAN_POINT('Ctrl Pts',(-20.5807193464566,-19.9998893516795,
-11.0437795021006));
#72996=CARTESIAN_POINT('Ctrl Pts',(-20.66341921337,-19.8237747121326,-11.0549700245056));
#72997=CARTESIAN_POINT('Ctrl Pts',(-20.675974861148,-19.7954352730716,-11.0567799147819));
#72998=CARTESIAN_POINT('Ctrl Pts',(-20.690648753905,-19.7602484381654,-11.0590503946498));
#72999=CARTESIAN_POINT('Ctrl Pts',(-20.6933610187251,-19.7536509707836,
-11.05947709945));
#73000=CARTESIAN_POINT('Ctrl Pts',(-20.6975744495108,-19.743252853983,-11.0601513689701));
#73001=CARTESIAN_POINT('Ctrl Pts',(-20.6990980710783,-19.7394612803831,
-11.0603975992514));
#73002=CARTESIAN_POINT('Ctrl Pts',(-20.7019342811529,-19.7323438022282,
-11.0608605435095));
#73003=CARTESIAN_POINT('Ctrl Pts',(-20.7032494244389,-19.7290189754961,
-11.0610771008679));
#73004=CARTESIAN_POINT('Ctrl Pts',(-20.7062437524804,-19.7213925553081,
-11.0615745113123));
#73005=CARTESIAN_POINT('Ctrl Pts',(-20.7079172851563,-19.7170888012446,
-11.0618556986588));
#73006=CARTESIAN_POINT('Ctrl Pts',(-20.7130574312923,-19.70374097718,-11.0627292153072));
#73007=CARTESIAN_POINT('Ctrl Pts',(-20.7164760101577,-19.6946787152548,
-11.0633243042981));
#73008=CARTESIAN_POINT('Ctrl Pts',(-20.7207530624095,-19.6831007664952,
-11.0640868798659));
#73009=CARTESIAN_POINT('Ctrl Pts',(-20.7216691884613,-19.6806063806669,
-11.0642513062267));
#73010=CARTESIAN_POINT('Ctrl Pts',(-20.7225805818558,-19.6781103700305,
-11.0644159698366));
#73011=CARTESIAN_POINT('',(-20.8509993992249,-18.9535948922217,-10.0879364584982));
#73012=CARTESIAN_POINT('Ctrl Pts',(-20.7225805823871,-19.6781103685755,
-10.8441190550425));
#73013=CARTESIAN_POINT('Ctrl Pts',(-20.721654332156,-19.68064706727,-10.8439718791398));
#73014=CARTESIAN_POINT('Ctrl Pts',(-20.7207231989508,-19.6831820734091,
-10.8438247431562));
#73015=CARTESIAN_POINT('Ctrl Pts',(-20.66234998667,-19.8411681008426,-10.834651040078));
#73016=CARTESIAN_POINT('Ctrl Pts',(-20.5868669710953,-19.9893140896377,
-10.8258505888223));
#73017=CARTESIAN_POINT('Ctrl Pts',(-20.4871421897505,-20.1387506012441,
-10.8152892080054));
#73018=CARTESIAN_POINT('Ctrl Pts',(-20.4792655355707,-20.1503040991621,
-10.8144605478709));
#73019=CARTESIAN_POINT('Ctrl Pts',(-20.4681194470797,-20.1663101908851,
-10.8132942461161));
#73020=CARTESIAN_POINT('Ctrl Pts',(-20.464945967379,-20.1708295831989,-10.812962876718));
#73021=CARTESIAN_POINT('Ctrl Pts',(-20.4598136870831,-20.1780780571108,
-10.8124279962897));
#73022=CARTESIAN_POINT('Ctrl Pts',(-20.4578659850139,-20.1808150186255,
-10.8122252432122));
#73023=CARTESIAN_POINT('Ctrl Pts',(-20.4537748168611,-20.1865351648408,
-10.8117998205916));
#73024=CARTESIAN_POINT('Ctrl Pts',(-20.4516300984774,-20.1895174091799,
-10.8115770617094));
#73025=CARTESIAN_POINT('Ctrl Pts',(-20.4464076162739,-20.1967395734038,
-10.8110352940034));
#73026=CARTESIAN_POINT('Ctrl Pts',(-20.4433218642905,-20.2009736637648,
-10.8107157372564));
#73027=CARTESIAN_POINT('Ctrl Pts',(-20.4323912722236,-20.2158556110821,
-10.8095858413374));
#73028=CARTESIAN_POINT('Ctrl Pts',(-20.4244625861269,-20.2264411103798,
-10.8087699648383));
#73029=CARTESIAN_POINT('Ctrl Pts',(-20.3764348919687,-20.2893255912705,
-10.8038532172211));
#73030=CARTESIAN_POINT('Ctrl Pts',(-20.3340141567129,-20.3397986648666,
-10.7996154829477));
#73031=CARTESIAN_POINT('Ctrl Pts',(-20.2240817568495,-20.4588479687894,
-10.7890378447767));
#73032=CARTESIAN_POINT('Ctrl Pts',(-20.1541137448145,-20.5249625621451,
-10.7826421740993));
#73033=CARTESIAN_POINT('Ctrl Pts',(-19.9712621148261,-20.6755654935763,
-10.7670586349167));
#73034=CARTESIAN_POINT('Ctrl Pts',(-19.8539618898259,-20.7539972784858,
-10.7580100967457));
#73035=CARTESIAN_POINT('Ctrl Pts',(-19.7171141005304,-20.8269346200798,
-10.7485414479407));
#73036=CARTESIAN_POINT('Ctrl Pts',(-19.7044367141368,-20.8335275081182,
-10.747673517477));
#73037=CARTESIAN_POINT('Ctrl Pts',(-19.6841535539931,-20.8438162434527,
-10.7462992672034));
#73038=CARTESIAN_POINT('Ctrl Pts',(-19.6765908805431,-20.8475956610821,
-10.7457900197118));
#73039=CARTESIAN_POINT('Ctrl Pts',(-19.6632128770887,-20.8541814103305,
-10.7448946568446));
#73040=CARTESIAN_POINT('Ctrl Pts',(-19.65740700647,-20.8570066116918,-10.7445078854125));
#73041=CARTESIAN_POINT('Ctrl Pts',(-19.6453717578922,-20.8627951494897,
-10.7437098137997));
#73042=CARTESIAN_POINT('Ctrl Pts',(-19.6391406324191,-20.865754692136,-10.7432986490364));
#73043=CARTESIAN_POINT('Ctrl Pts',(-19.6231088296308,-20.8732733601876,
-10.7422459109548));
#73044=CARTESIAN_POINT('Ctrl Pts',(-19.6132874229279,-20.8777880127195,
-10.7416058791007));
#73045=CARTESIAN_POINT('Ctrl Pts',(-19.5721500376953,-20.896317513263,-10.7389449895684));
#73046=CARTESIAN_POINT('Ctrl Pts',(-19.5405292481989,-20.909645740814,-10.7369476656899));
#73047=CARTESIAN_POINT('Ctrl Pts',(-19.457306174465,-20.9423654379907,-10.731802969803));
#73048=CARTESIAN_POINT('Ctrl Pts',(-19.4052450524024,-20.9605211285955,
-10.7286949992077));
#73049=CARTESIAN_POINT('Ctrl Pts',(-19.2479505448434,-21.0085752724312,
-10.7195498706312));
#73050=CARTESIAN_POINT('Ctrl Pts',(-19.1410481739847,-21.0323748894513,
-10.7136614396477));
#73051=CARTESIAN_POINT('Ctrl Pts',(-18.9869104505298,-21.0543493171957,
-10.7051846535349));
#73052=CARTESIAN_POINT('Ctrl Pts',(-18.9408337330223,-21.0593812909741,
-10.7026507573554));
#73053=CARTESIAN_POINT('Ctrl Pts',(-18.8732966600446,-21.0645205820013,
-10.6988935352125));
#73054=CARTESIAN_POINT('Ctrl Pts',(-18.8519399092396,-21.0658204521351,
-10.6976990983847));
#73055=CARTESIAN_POINT('Ctrl Pts',(-18.7787684009524,-21.0691616723124,
-10.6935745735534));
#73056=CARTESIAN_POINT('Ctrl Pts',(-18.7269041839199,-21.0696228328302,
-10.6905959948421));
#73057=CARTESIAN_POINT('Ctrl Pts',(-18.6664282755531,-21.0679390291251,
-10.687005316025));
#73058=CARTESIAN_POINT('Ctrl Pts',(-18.657778129181,-21.0676450868561,-10.6864889123011));
#73059=CARTESIAN_POINT('Ctrl Pts',(-18.6446645796776,-21.067118946185,-10.6857014564131));
#73060=CARTESIAN_POINT('Ctrl Pts',(-18.6401995885298,-21.066925638362,-10.6854325303205));
#73061=CARTESIAN_POINT('Ctrl Pts',(-18.6321760418079,-21.066552807839,-10.6849477675161));
#73062=CARTESIAN_POINT('Ctrl Pts',(-18.6286173011567,-21.0663784387093,
-10.6847322221513));
#73063=CARTESIAN_POINT('Ctrl Pts',(-18.6208737703034,-21.065979427197,-10.6842620372403));
#73064=CARTESIAN_POINT('Ctrl Pts',(-18.6166892555886,-21.065751345594,-10.6840072124888));
#73065=CARTESIAN_POINT('Ctrl Pts',(-18.6049071857032,-21.0650740569778,
-10.6832876809919));
#73066=CARTESIAN_POINT('Ctrl Pts',(-18.5973114260672,-21.064596306608,-10.6828214205683));
#73067=CARTESIAN_POINT('Ctrl Pts',(-18.5512917547967,-21.0614525844054,
-10.6799827382927));
#73068=CARTESIAN_POINT('Ctrl Pts',(-18.5129464670905,-21.0577795262608,
-10.6775592052215));
#73069=CARTESIAN_POINT('Ctrl Pts',(-18.3856271384966,-21.0420681277534,
-10.6693639794191));
#73070=CARTESIAN_POINT('Ctrl Pts',(-18.2973236371973,-21.0254175170392,
-10.6634411578528));
#73071=CARTESIAN_POINT('Ctrl Pts',(-18.0441419775274,-20.9607832913705,
-10.6461741899727));
#73072=CARTESIAN_POINT('Ctrl Pts',(-17.8836741157218,-20.8982996341513,
-10.6349280904655));
#73073=CARTESIAN_POINT('Ctrl Pts',(-17.7119984076849,-20.806115065783,-10.6229309439354));
#73074=CARTESIAN_POINT('Ctrl Pts',(-17.6916898153342,-20.7947749397357,
-10.6215108837775));
#73075=CARTESIAN_POINT('Ctrl Pts',(-17.663276567896,-20.7782892165825,-10.619522198383));
#73076=CARTESIAN_POINT('Ctrl Pts',(-17.6550142637645,-20.7734199835285,
-10.6189436709301));
#73077=CARTESIAN_POINT('Ctrl Pts',(-17.6416585403609,-20.7654262691874,
-10.6180080323445));
#73078=CARTESIAN_POINT('Ctrl Pts',(-17.6365448286014,-20.7623361141328,
-10.6176496770886));
#73079=CARTESIAN_POINT('Ctrl Pts',(-17.6258802748347,-20.7558298574641,
-10.6169020669863));
#73080=CARTESIAN_POINT('Ctrl Pts',(-17.6203319814758,-20.7524096828114,
-10.6165129665454));
#73081=CARTESIAN_POINT('Ctrl Pts',(-17.6071924962542,-20.7442260359152,
-10.6155910864694));
#73082=CARTESIAN_POINT('Ctrl Pts',(-17.5996155436419,-20.739439851644,-10.6150591515117));
#73083=CARTESIAN_POINT('Ctrl Pts',(-17.5742945447087,-20.7232193091537,
-10.6132802021167));
#73084=CARTESIAN_POINT('Ctrl Pts',(-17.5566908130909,-20.7115674781159,
-10.6120412841322));
#73085=CARTESIAN_POINT('Ctrl Pts',(-17.462462336009,-20.6471507386989,-10.6053928432974));
#73086=CARTESIAN_POINT('Ctrl Pts',(-17.3892005001075,-20.5896389295884,
-10.6001689098512));
#73087=CARTESIAN_POINT('Ctrl Pts',(-17.2048003946038,-20.4241343864209,
-10.5865236892977));
#73088=CARTESIAN_POINT('Ctrl Pts',(-17.1013352948134,-20.3084772792071,
-10.578341240394));
#73089=CARTESIAN_POINT('Ctrl Pts',(-16.9802264995808,-20.138947380487,-10.5666271778609));
#73090=CARTESIAN_POINT('Ctrl Pts',(-16.9507222853145,-20.094140592561,-10.5635502962915));
#73091=CARTESIAN_POINT('Ctrl Pts',(-16.9184272112633,-20.0407887090463,
-10.5598495256133));
#73092=CARTESIAN_POINT('Ctrl Pts',(-16.9139472470223,-20.0332832073824,
-10.5593280725652));
#73093=CARTESIAN_POINT('Ctrl Pts',(-16.9072378062841,-20.0218827164531,
-10.5585344210374));
#73094=CARTESIAN_POINT('Ctrl Pts',(-16.904973961376,-20.0180079214236,-10.5582643991173));
#73095=CARTESIAN_POINT('Ctrl Pts',(-16.9009342368253,-20.011042780965,-10.5577784729938));
#73096=CARTESIAN_POINT('Ctrl Pts',(-16.8991538272415,-20.0079551250207,
-10.5575628663861));
#73097=CARTESIAN_POINT('Ctrl Pts',(-16.8953040930042,-20.0012396315514,
-10.5570934983962));
#73098=CARTESIAN_POINT('Ctrl Pts',(-16.8932377311395,-19.9976102101956,
-10.5568395570042));
#73099=CARTESIAN_POINT('Ctrl Pts',(-16.8874685550356,-19.9874069486464,
-10.5561249586191));
#73100=CARTESIAN_POINT('Ctrl Pts',(-16.8837901684364,-19.9808194699733,
-10.5556627811539));
#73101=CARTESIAN_POINT('Ctrl Pts',(-16.8621082588388,-19.9414978349402,
-10.5528997849538));
#73102=CARTESIAN_POINT('Ctrl Pts',(-16.8449397535161,-19.9083135704699,
-10.5505509047069));
#73103=CARTESIAN_POINT('Ctrl Pts',(-16.7915325222157,-19.7980290572225,
-10.5427306927185));
#73104=CARTESIAN_POINT('Ctrl Pts',(-16.7590691122222,-19.7191969686125,
-10.5371218810942));
#73105=CARTESIAN_POINT('Ctrl Pts',(-16.6736890748013,-19.4701861005766,
-10.5197317279115));
#73106=CARTESIAN_POINT('Ctrl Pts',(-16.6374050927338,-19.2950921422355,
-10.5080297421229));
#73107=CARTESIAN_POINT('Ctrl Pts',(-16.6216974500578,-19.0947803478442,
-10.4956647963491));
#73108=CARTESIAN_POINT('Ctrl Pts',(-16.6202828609828,-19.0720342040855,
-10.4942738524237));
#73109=CARTESIAN_POINT('Ctrl Pts',(-16.6187986907307,-19.0397662431442,
-10.4923185681888));
#73110=CARTESIAN_POINT('Ctrl Pts',(-16.6184256628598,-19.0302605956026,
-10.4917447694746));
#73111=CARTESIAN_POINT('Ctrl Pts',(-16.6179231307851,-19.0147950176111,
-10.4908146978918));
#73112=CARTESIAN_POINT('Ctrl Pts',(-16.6177547077915,-19.0088365639154,
-10.4904572099336));
#73113=CARTESIAN_POINT('Ctrl Pts',(-16.6174545212065,-18.9963494661293,
-10.4897097598633));
#73114=CARTESIAN_POINT('Ctrl Pts',(-16.6173277932303,-18.9898207550052,
-10.4893199594034));
#73115=CARTESIAN_POINT('Ctrl Pts',(-16.6170978152185,-18.9742634891722,
-10.4883934221738));
#73116=CARTESIAN_POINT('Ctrl Pts',(-16.6170221135093,-18.9652346075889,
-10.4878575533742));
#73117=CARTESIAN_POINT('Ctrl Pts',(-16.6169614563799,-18.9346999186841,
-10.4860513879421));
#73118=CARTESIAN_POINT('Ctrl Pts',(-16.6172464316565,-18.9131944715482,
-10.4847895354095));
#73119=CARTESIAN_POINT('Ctrl Pts',(-16.6229818787195,-18.7119289702551,
-10.4730664950018));
#73120=CARTESIAN_POINT('Ctrl Pts',(-16.650988260201,-18.5335497020633,-10.4634059639935));
#73121=CARTESIAN_POINT('Ctrl Pts',(-16.7347415328079,-18.2455500022279,
-10.4470815795015));
#73122=CARTESIAN_POINT('Ctrl Pts',(-16.7780138208059,-18.1333329819364,
-10.440492433379));
#73123=CARTESIAN_POINT('Ctrl Pts',(-16.8347150170204,-18.016855095654,-10.432814929758));
#73124=CARTESIAN_POINT('Ctrl Pts',(-16.8389349183148,-18.0083328090676,
-10.4322480843172));
#73125=CARTESIAN_POINT('Ctrl Pts',(-16.8452734803941,-17.9957457755526,
-10.4314028597307));
#73126=CARTESIAN_POINT('Ctrl Pts',(-16.8473482214746,-17.9916588765876,
-10.4311271614003));
#73127=CARTESIAN_POINT('Ctrl Pts',(-16.8510635049801,-17.9843988860813,
-10.4306351043593));
#73128=CARTESIAN_POINT('Ctrl Pts',(-16.8526988225738,-17.9812231772852,
-10.4304190754897));
#73129=CARTESIAN_POINT('Ctrl Pts',(-16.8562323263675,-17.9744037422464,
-10.4299534632163));
#73130=CARTESIAN_POINT('Ctrl Pts',(-16.8581330563605,-17.970761451832,-10.4297037248402));
#73131=CARTESIAN_POINT('Ctrl Pts',(-16.8634097332128,-17.9607213392477,
-10.4290124493867));
#73132=CARTESIAN_POINT('Ctrl Pts',(-16.8668078519805,-17.9543353226877,
-10.4285695444434));
#73133=CARTESIAN_POINT('Ctrl Pts',(-16.8856168563481,-17.9194206384387,
-10.4261308510631));
#73134=CARTESIAN_POINT('Ctrl Pts',(-16.9016480041505,-17.8912331639775,
-10.4240989740089));
#73135=CARTESIAN_POINT('Ctrl Pts',(-17.0020305028812,-17.7238006088581,
-10.41169536643));
#73136=CARTESIAN_POINT('Ctrl Pts',(-17.1015653443001,-17.5943000723529,
-10.4007319227682));
#73137=CARTESIAN_POINT('Ctrl Pts',(-17.2963461628739,-17.3936369333862,
-10.3824650355408));
#73138=CARTESIAN_POINT('Ctrl Pts',(-17.3845492722723,-17.3166607229697,
-10.3750213987216));
#73139=CARTESIAN_POINT('Ctrl Pts',(-17.4901699542042,-17.2388801006792,
-10.3670122466832));
#73140=CARTESIAN_POINT('Ctrl Pts',(-17.5017556359537,-17.2305277187122,
-10.3661447298444));
#73141=CARTESIAN_POINT('Ctrl Pts',(-17.5203312227918,-17.2174197794686,
-10.3647710086347));
#73142=CARTESIAN_POINT('Ctrl Pts',(-17.5272664644299,-17.2125878522914,
-10.3642618800883));
#73143=CARTESIAN_POINT('Ctrl Pts',(-17.5395499552708,-17.2041385137033,
-10.3633666555635));
#73144=CARTESIAN_POINT('Ctrl Pts',(-17.5448861281116,-17.2005038150918,
-10.3629799041664));
#73145=CARTESIAN_POINT('Ctrl Pts',(-17.555958479747,-17.1930358810124,-10.3621818060875));
#73146=CARTESIAN_POINT('Ctrl Pts',(-17.5616969421382,-17.1892061556762,
-10.3617705951576));
#73147=CARTESIAN_POINT('Ctrl Pts',(-17.5764770268571,-17.1794463392741,
-10.3607175984647));
#73148=CARTESIAN_POINT('Ctrl Pts',(-17.5855456163395,-17.1735572967557,
-10.3600773556533));
#73149=CARTESIAN_POINT('Ctrl Pts',(-17.6236016868468,-17.1492565847232,
-10.357414414779));
#73150=CARTESIAN_POINT('Ctrl Pts',(-17.6529908205066,-17.131481506216,-10.3554152968543));
#73151=CARTESIAN_POINT('Ctrl Pts',(-17.7306991380011,-17.0870277633216,
-10.3502649343218));
#73152=CARTESIAN_POINT('Ctrl Pts',(-17.7796527953812,-17.061509025676,-10.3471532050509));
#73153=CARTESIAN_POINT('Ctrl Pts',(-18.0001640608131,-16.9573114816709,
-10.3335928911971));
#73154=CARTESIAN_POINT('Ctrl Pts',(-18.1807674339952,-16.8998749470545,
-10.3237454457231));
#73155=CARTESIAN_POINT('Ctrl Pts',(-18.4072158569911,-16.8599663968284,
-10.3106716474144));
#73156=CARTESIAN_POINT('Ctrl Pts',(-18.4480604320674,-16.8539936769848,
-10.3082823569198));
#73157=CARTESIAN_POINT('Ctrl Pts',(-18.4963994698329,-16.8483627376973,
-10.3053907873153));
#73158=CARTESIAN_POINT('Ctrl Pts',(-18.5037529616296,-16.8475451915094,
-10.3049491761383));
#73159=CARTESIAN_POINT('Ctrl Pts',(-18.5156752363866,-16.8462829325157,
-10.304230158663));
#73160=CARTESIAN_POINT('Ctrl Pts',(-18.5202415175733,-16.8458144951164,
-10.3039540526395));
#73161=CARTESIAN_POINT('Ctrl Pts',(-18.5283645190566,-16.8450078752761,
-10.3034615490718));
#73162=CARTESIAN_POINT('Ctrl Pts',(-18.5319206080349,-16.8446638417687,
-10.3032454836792));
#73163=CARTESIAN_POINT('Ctrl Pts',(-18.5395634333902,-16.8439439609681,
-10.3027801130099));
#73164=CARTESIAN_POINT('Ctrl Pts',(-18.5436503363709,-16.8435710002399,
-10.3025306544487));
#73165=CARTESIAN_POINT('Ctrl Pts',(-18.5549236141006,-16.8425752726991,
-10.3018409237011));
#73166=CARTESIAN_POINT('Ctrl Pts',(-18.562112048801,-16.8419773553544,-10.3013992935025));
#73167=CARTESIAN_POINT('Ctrl Pts',(-18.6013323208737,-16.8389168513302,
-10.2989803359217));
#73168=CARTESIAN_POINT('Ctrl Pts',(-18.633412144967,-16.8371470665829,-10.2969675913487));
#73169=CARTESIAN_POINT('Ctrl Pts',(-18.8284837672567,-16.8308334396913,
-10.2845703249421));
#73170=CARTESIAN_POINT('Ctrl Pts',(-18.9915088627262,-16.8444033070309,
-10.2735892285581));
#73171=CARTESIAN_POINT('Ctrl Pts',(-19.2659681080618,-16.8995952760549,
-10.2553020994591));
#73172=CARTESIAN_POINT('Ctrl Pts',(-19.3784846450023,-16.9320983726147,
-10.2478551001261));
#73173=CARTESIAN_POINT('Ctrl Pts',(-19.5011217458905,-16.9788254618589,
-10.2398416205954));
#73174=CARTESIAN_POINT('Ctrl Pts',(-19.5144342696115,-16.9840528722652,
-10.2389729004162));
#73175=CARTESIAN_POINT('Ctrl Pts',(-19.5355341451213,-16.9925859160875,
-10.237597640089));
#73176=CARTESIAN_POINT('Ctrl Pts',(-19.543356242556,-16.9958039428756,-10.2370881655599));
#73177=CARTESIAN_POINT('Ctrl Pts',(-19.5571157825931,-17.0015613044551,
-10.2361925385826));
#73178=CARTESIAN_POINT('Ctrl Pts',(-19.5630612466798,-17.0040810727035,
-10.2358057288595));
#73179=CARTESIAN_POINT('Ctrl Pts',(-19.5744704106973,-17.0089781292245,
-10.2350637801813));
#73180=CARTESIAN_POINT('Ctrl Pts',(-19.5799357776103,-17.0113513551275,
-10.2347085074487));
#73181=CARTESIAN_POINT('Ctrl Pts',(-19.594340085058,-17.0176785493396,-10.2337725061402));
#73182=CARTESIAN_POINT('Ctrl Pts',(-19.6032618547738,-17.0216714349256,
-10.2331931130482));
#73183=CARTESIAN_POINT('Ctrl Pts',(-19.6363015689364,-17.0367336824467,
-10.231048471716));
#73184=CARTESIAN_POINT('Ctrl Pts',(-19.6602390128667,-17.0481947125768,
-10.2294967117845));
#73185=CARTESIAN_POINT('Ctrl Pts',(-19.7190604166622,-17.0777299985423,
-10.2256838278797));
#73186=CARTESIAN_POINT('Ctrl Pts',(-19.7536693107868,-17.0963311657396,
-10.2234407683219));
#73187=CARTESIAN_POINT('Ctrl Pts',(-19.8816272910708,-17.1697659698881,
-10.2151169071897));
#73188=CARTESIAN_POINT('Ctrl Pts',(-19.9712461359685,-17.2307705860135,
-10.209233383477));
#73189=CARTESIAN_POINT('Ctrl Pts',(-20.1621976467807,-17.3834047618063,
-10.1959581259965));
#73190=CARTESIAN_POINT('Ctrl Pts',(-20.260117338126,-17.4785024137405,-10.1886009569423));
#73191=CARTESIAN_POINT('Ctrl Pts',(-20.3583115020396,-17.5942280116429,
-10.1797012825132));
#73192=CARTESIAN_POINT('Ctrl Pts',(-20.3682778060191,-17.6062404937221,
-10.1787778879968));
#73193=CARTESIAN_POINT('Ctrl Pts',(-20.3817499242634,-17.6228489283591,
-10.1775000223475));
#73194=CARTESIAN_POINT('Ctrl Pts',(-20.3853713727367,-17.6273510005747,
-10.1771535122544));
#73195=CARTESIAN_POINT('Ctrl Pts',(-20.3910999010786,-17.6345325290855,
-10.1766004852127));
#73196=CARTESIAN_POINT('Ctrl Pts',(-20.3932190483917,-17.6372023851,-10.1763948251634));
#73197=CARTESIAN_POINT('Ctrl Pts',(-20.3975850695391,-17.6427303815051,
-10.1759688447163));
#73198=CARTESIAN_POINT('Ctrl Pts',(-20.3998310254622,-17.6455891873776,
-10.1757484594032));
#73199=CARTESIAN_POINT('Ctrl Pts',(-20.4051694785284,-17.6524204839468,
-10.1752216467053));
#73200=CARTESIAN_POINT('Ctrl Pts',(-20.4082551813425,-17.6563982359319,
-10.174914742553));
#73201=CARTESIAN_POINT('Ctrl Pts',(-20.4186340286359,-17.669876511333,-10.1738744286385));
#73202=CARTESIAN_POINT('Ctrl Pts',(-20.4258605716586,-17.6794277067749,
-10.1731365647873));
#73203=CARTESIAN_POINT('Ctrl Pts',(-20.5082076495465,-17.7902056223147,
-10.1645759869468));
#73204=CARTESIAN_POINT('Ctrl Pts',(-20.5742159455847,-17.8978759174788,
-10.1562456568966));
#73205=CARTESIAN_POINT('Ctrl Pts',(-20.6639570531766,-18.0786715880011,
-10.1429069302171));
#73206=CARTESIAN_POINT('Ctrl Pts',(-20.6939937560356,-18.1483444894198,
-10.1379032853588));
#73207=CARTESIAN_POINT('Ctrl Pts',(-20.7344247282807,-18.257973289476,-10.1303131310646));
#73208=CARTESIAN_POINT('Ctrl Pts',(-20.7474992285013,-18.2968715254224,
-10.1276720761972));
#73209=CARTESIAN_POINT('Ctrl Pts',(-20.7623062613021,-18.3455677444204,
-10.1244341970915));
#73210=CARTESIAN_POINT('Ctrl Pts',(-20.7651109235248,-18.3550286512658,
-10.1238082752894));
#73211=CARTESIAN_POINT('Ctrl Pts',(-20.7833788644753,-18.4182708730031,
-10.1196453528436));
#73212=CARTESIAN_POINT('Ctrl Pts',(-20.7967716114792,-18.4726309223956,
-10.1161695253994));
#73213=CARTESIAN_POINT('Ctrl Pts',(-20.8104073081852,-18.5392454074478,
-10.112030449285));
#73214=CARTESIAN_POINT('Ctrl Pts',(-20.8127188682339,-18.5510492057949,
-10.1113015163257));
#73215=CARTESIAN_POINT('Ctrl Pts',(-20.8163752168606,-18.5706021797478,
-10.1101013105191));
#73216=CARTESIAN_POINT('Ctrl Pts',(-20.8177776223906,-18.5783401759405,
-10.1096282104574));
#73217=CARTESIAN_POINT('Ctrl Pts',(-20.8202374512184,-18.5923573446946,
-10.1087745383789));
#73218=CARTESIAN_POINT('Ctrl Pts',(-20.8213097188383,-18.5986337857175,
-10.1083934983669));
#73219=CARTESIAN_POINT('Ctrl Pts',(-20.8233364623021,-18.6108283703562,
-10.1076554767596));
#73220=CARTESIAN_POINT('Ctrl Pts',(-20.8242941494265,-18.6167459119008,
-10.1072983966081));
#73221=CARTESIAN_POINT('Ctrl Pts',(-20.8263396785846,-18.6297348062099,
-10.1065168817455));
#73222=CARTESIAN_POINT('Ctrl Pts',(-20.8274168374647,-18.6368077852555,
-10.106092788067));
#73223=CARTESIAN_POINT('Ctrl Pts',(-20.8299772084217,-18.6542123578294,
-10.1050527574227));
#73224=CARTESIAN_POINT('Ctrl Pts',(-20.8314199196078,-18.6645497874455,
-10.104438096375));
#73225=CARTESIAN_POINT('Ctrl Pts',(-20.8449846070162,-18.7672893463057,
-10.0983585509772));
#73226=CARTESIAN_POINT('Ctrl Pts',(-20.851069617783,-18.8603894435261,-10.093091189706));
#73227=CARTESIAN_POINT('Ctrl Pts',(-20.8509993992249,-18.9535948922217,
-10.0879364584982));
#73228=CARTESIAN_POINT('Ctrl Pts',(-20.8509994011068,-18.9535923923061,
-10.0879365967561));
#73229=CARTESIAN_POINT('Ctrl Pts',(-20.850883505645,-19.1076691373228,-10.0794153726715));
#73230=CARTESIAN_POINT('Ctrl Pts',(-20.8339479021024,-19.2612691803274,
-10.0712643188475));
#73231=CARTESIAN_POINT('Ctrl Pts',(-20.7877757711039,-19.4688406968946,
-10.0593982033839));
#73232=CARTESIAN_POINT('Ctrl Pts',(-20.7726928098578,-19.5254541017574,
-10.0560661702904));
#73233=CARTESIAN_POINT('Ctrl Pts',(-20.7515883197402,-19.5932339086432,
-10.0518806465533));
#73234=CARTESIAN_POINT('Ctrl Pts',(-20.7477880301854,-19.6050706748842,
-10.0511423048045));
#73235=CARTESIAN_POINT('Ctrl Pts',(-20.7422787371043,-19.621725042868,-10.0500920839653));
#73236=CARTESIAN_POINT('Ctrl Pts',(-20.7406561150653,-19.6265712368428,
-10.0497851180081));
#73237=CARTESIAN_POINT('Ctrl Pts',(-20.7378448456755,-19.6348675940094,
-10.0492571927926));
#73238=CARTESIAN_POINT('Ctrl Pts',(-20.7366647828737,-19.6383206857942,
-10.0490367396442));
#73239=CARTESIAN_POINT('Ctrl Pts',(-20.7343716263545,-19.644974632166,-10.048610516056));
#73240=CARTESIAN_POINT('Ctrl Pts',(-20.7332597708327,-19.6481758777097,
-10.0484048244984));
#73241=CARTESIAN_POINT('Ctrl Pts',(-20.7302650144133,-19.6567320147411,
-10.0478533928633));
#73242=CARTESIAN_POINT('Ctrl Pts',(-20.7283682704733,-19.6620819814589,
-10.047506842636));
#73243=CARTESIAN_POINT('Ctrl Pts',(-20.7251697799558,-19.6709897494137,
-10.0469269837388));
#73244=CARTESIAN_POINT('Ctrl Pts',(-20.7238799494575,-19.6745518239872,
-10.0466943454164));
#73245=CARTESIAN_POINT('Ctrl Pts',(-20.722580582123,-19.6781103692989,-10.0464611886058));
#73246=CARTESIAN_POINT('Origin',(-18.734,-18.952,0.));
#73247=CARTESIAN_POINT('',(-20.7225807271506,-19.6781099721152,-9.24346982890923));
#73248=CARTESIAN_POINT('',(-20.7225805821191,-19.6781103693095,-9.46634969989166));
#73249=CARTESIAN_POINT('',(-20.7225805821191,-19.6781103693095,0.));
#73250=CARTESIAN_POINT('',(-20.8516083971888,-18.9501065433296,-9.51094371951038));
#73251=CARTESIAN_POINT('Ctrl Pts',(-20.7225805821191,-19.6781103693095,
-9.46634969989166));
#73252=CARTESIAN_POINT('Ctrl Pts',(-20.7472616655809,-19.610516894003,-9.47066128466945));
#73253=CARTESIAN_POINT('Ctrl Pts',(-20.7684942812802,-19.5416581924624,
-9.47497286944723));
#73254=CARTESIAN_POINT('Ctrl Pts',(-20.7861613956308,-19.4719255776385,
-9.47928445422502));
#73255=CARTESIAN_POINT('Ctrl Pts',(-20.8038310616679,-19.4021828912336,
-9.48359666173114));
#73256=CARTESIAN_POINT('Ctrl Pts',(-20.8179340943008,-19.3315665265442,
-9.48790886923727));
#73257=CARTESIAN_POINT('Ctrl Pts',(-20.8284043739734,-19.2604790402619,
-9.4922210767434));
#73258=CARTESIAN_POINT('Ctrl Pts',(-20.8388856820424,-19.1893166771852,
-9.49653782631863));
#73259=CARTESIAN_POINT('Ctrl Pts',(-20.8457265470577,-19.1176826969835,
-9.50085457589386));
#73260=CARTESIAN_POINT('Ctrl Pts',(-20.8489127383039,-19.045984622997,-9.50517132546909));
#73261=CARTESIAN_POINT('Ctrl Pts',(-20.8503329332884,-19.014026326333,-9.50709544917115));
#73262=CARTESIAN_POINT('Ctrl Pts',(-20.8510277144304,-18.9820552992082,
-9.50901957287322));
#73263=CARTESIAN_POINT('Ctrl Pts',(-20.8509991540683,-18.9501074689014,
-9.51094369657528));
#73264=CARTESIAN_POINT('Ctrl Pts',(-20.8516473698352,-18.9501064841217,
-9.51094372097751));
#73265=CARTESIAN_POINT('Ctrl Pts',(-20.8529700774227,-18.8071177722941,
-9.51955279572482));
#73266=CARTESIAN_POINT('Ctrl Pts',(-20.7745204018912,-17.9614816365997,
-9.57055380603263));
#73267=CARTESIAN_POINT('Ctrl Pts',(-19.6371491233128,-16.6173369466333,
-9.66394675190085));
#73268=CARTESIAN_POINT('Ctrl Pts',(-17.2597753314279,-16.928885683341,-9.79112255858232));
#73269=CARTESIAN_POINT('Ctrl Pts',(-16.2349111722559,-19.0965162369476,
-9.91829836526373));
#73270=CARTESIAN_POINT('Ctrl Pts',(-17.5028059015931,-21.1315621128438,
-10.0454741719452));
#73271=CARTESIAN_POINT('Ctrl Pts',(-19.6892757596572,-21.1638770149718,
-10.1614588037971));
#73272=CARTESIAN_POINT('Ctrl Pts',(-20.5391740279707,-20.1636738456026,
-10.2350515000887));
#73273=CARTESIAN_POINT('Ctrl Pts',(-20.7219729237027,-19.6778789621698,
-10.2662522608197));
#73274=CARTESIAN_POINT('Ctrl Pts',(-20.722580582123,-19.6781103692989,-10.0464611886058));
#73275=CARTESIAN_POINT('Ctrl Pts',(-20.7187550915236,-19.6885871461701,
-10.0457747474716));
#73276=CARTESIAN_POINT('Ctrl Pts',(-20.7148469372165,-19.6990333320199,
-10.0450838126525));
#73277=CARTESIAN_POINT('Ctrl Pts',(-20.6549184747011,-19.8554400803251,
-10.0346460290459));
#73278=CARTESIAN_POINT('Ctrl Pts',(-20.5829848665573,-19.9947754284463,
-10.0241696945664));
#73279=CARTESIAN_POINT('Ctrl Pts',(-20.459226806328,-20.1807298986069,-10.0094649923507));
#73280=CARTESIAN_POINT('Ctrl Pts',(-20.4194453519409,-20.2347547271001,
-10.005087012774));
#73281=CARTESIAN_POINT('Ctrl Pts',(-20.3438774955942,-20.3277799833174,
-9.99739792145197));
#73282=CARTESIAN_POINT('Ctrl Pts',(-20.3090674751063,-20.3674996609403,
-9.99406021181886));
#73283=CARTESIAN_POINT('Ctrl Pts',(-20.2576202360407,-20.4219521561615,
-9.98940797716126));
#73284=CARTESIAN_POINT('Ctrl Pts',(-20.2421828076885,-20.4377868761848,
-9.98804521972032));
#73285=CARTESIAN_POINT('Ctrl Pts',(-20.2145560326903,-20.4652502938927,
-9.98566350175101));
#73286=CARTESIAN_POINT('Ctrl Pts',(-20.2024709059035,-20.4769806038585,
-9.98464012615214));
#73287=CARTESIAN_POINT('Ctrl Pts',(-20.1843140782033,-20.4941883431244,
-9.98312940303068));
#73288=CARTESIAN_POINT('Ctrl Pts',(-20.178348770264,-20.4997766130378,-9.98263726626117));
#73289=CARTESIAN_POINT('Ctrl Pts',(-20.1676419638449,-20.5096908908263,
-9.98176135675834));
#73290=CARTESIAN_POINT('Ctrl Pts',(-20.1629129020684,-20.5140301250517,
-9.9813770202822));
#73291=CARTESIAN_POINT('Ctrl Pts',(-20.1536163277823,-20.5224828119447,
-9.98062639583515));
#73292=CARTESIAN_POINT('Ctrl Pts',(-20.1490504928204,-20.5265980073383,
-9.98026003600057));
#73293=CARTESIAN_POINT('Ctrl Pts',(-20.1366409690211,-20.5376851646344,
-9.97927044418196));
#73294=CARTESIAN_POINT('Ctrl Pts',(-20.1287631901906,-20.5446188428548,
-9.9786488209032));
#73295=CARTESIAN_POINT('Ctrl Pts',(-20.0989372486999,-20.5704792951196,
-9.97631954289845));
#73296=CARTESIAN_POINT('Ctrl Pts',(-20.0766521460087,-20.5890138229301,
-9.97462805555531));
#73297=CARTESIAN_POINT('Ctrl Pts',(-20.0515903372689,-20.6090015525466,
-9.97277604555553));
#73298=CARTESIAN_POINT('Ctrl Pts',(-20.0491838352121,-20.6109122706577,
-9.97259871195944));
#73299=CARTESIAN_POINT('Ctrl Pts',(-19.9172692520436,-20.7151825471311,
-9.96290520055451));
#73300=CARTESIAN_POINT('Ctrl Pts',(-19.7762389490106,-20.8020491981962,
-9.95403301223472));
#73301=CARTESIAN_POINT('Ctrl Pts',(-19.548204367267,-20.9080733234487,-9.94034793969889));
#73302=CARTESIAN_POINT('Ctrl Pts',(-19.4677210862196,-20.9396625988341,
-9.93561679888838));
#73303=CARTESIAN_POINT('Ctrl Pts',(-19.3497026771053,-20.9778375961337,
-9.92853371290306));
#73304=CARTESIAN_POINT('Ctrl Pts',(-19.3135640507415,-20.9884706894498,
-9.92634552173695));
#73305=CARTESIAN_POINT('Ctrl Pts',(-19.2698540958267,-21.000073871433,-9.92365477310876));
#73306=CARTESIAN_POINT('Ctrl Pts',(-19.2625343092727,-21.0019750424996,
-9.92320270139751));
#73307=CARTESIAN_POINT('Ctrl Pts',(-19.2511529735457,-21.0048661127848,
-9.92249728223481));
#73308=CARTESIAN_POINT('Ctrl Pts',(-19.2470983289707,-21.0058832924928,
-9.92224548162995));
#73309=CARTESIAN_POINT('Ctrl Pts',(-19.2395813512201,-21.0077454120221,
-9.92177770766564));
#73310=CARTESIAN_POINT('Ctrl Pts',(-19.2361198871982,-21.0085936205404,
-9.92156192548175));
#73311=CARTESIAN_POINT('Ctrl Pts',(-19.2282997756501,-21.0104889666802,
-9.92107358183766));
#73312=CARTESIAN_POINT('Ctrl Pts',(-19.223939959272,-21.0115309974859,-9.92080073245111));
#73313=CARTESIAN_POINT('Ctrl Pts',(-19.2110917941654,-21.014558705917,-9.9199949862861));
#73314=CARTESIAN_POINT('Ctrl Pts',(-19.2025945720958,-21.0165057801839,
-9.91945995430702));
#73315=CARTESIAN_POINT('Ctrl Pts',(-19.1420507203019,-21.0299859190133,
-9.91563371873206));
#73316=CARTESIAN_POINT('Ctrl Pts',(-19.0896011856568,-21.0396009274838,
-9.91224557989896));
#73317=CARTESIAN_POINT('Ctrl Pts',(-19.0096867213254,-21.0511519920042,
-9.90702723502794));
#73318=CARTESIAN_POINT('Ctrl Pts',(-18.9824504918898,-21.0545495291893,
-9.90523891355756));
#73319=CARTESIAN_POINT('Ctrl Pts',(-18.8184280549174,-21.0717787395807,
-9.89443653042584));
#73320=CARTESIAN_POINT('Ctrl Pts',(-18.6806127534488,-21.072788622229,-9.88525203852045));
#73321=CARTESIAN_POINT('Ctrl Pts',(-18.4818913021121,-21.0548500095181,
-9.87235864899197));
#73322=CARTESIAN_POINT('Ctrl Pts',(-18.4203814790917,-21.0465599832269,
-9.86841236794707));
#73323=CARTESIAN_POINT('Ctrl Pts',(-18.3225554016999,-21.0289683844883,
-9.86221849707654));
#73324=CARTESIAN_POINT('Ctrl Pts',(-18.2859707463055,-21.0213850280445,
-9.85992058481192));
#73325=CARTESIAN_POINT('Ctrl Pts',(-18.2387546380831,-21.0102869682285,
-9.85697705777438));
#73326=CARTESIAN_POINT('Ctrl Pts',(-18.227925411775,-21.0076511695017,-9.85630345965948));
#73327=CARTESIAN_POINT('Ctrl Pts',(-18.2103561707791,-21.003227620575,-9.85521295884289));
#73328=CARTESIAN_POINT('Ctrl Pts',(-18.2036033899213,-21.0014919002323,
-9.85479438597461));
#73329=CARTESIAN_POINT('Ctrl Pts',(-18.1906396387028,-20.9980913623198,
-9.85399186669419));
#73330=CARTESIAN_POINT('Ctrl Pts',(-18.1844274467638,-20.9964315482125,
-9.85360776346931));
#73331=CARTESIAN_POINT('Ctrl Pts',(-18.1702292296614,-20.9925685841567,
-9.85273089308057));
#73332=CARTESIAN_POINT('Ctrl Pts',(-18.1622483489522,-20.990346800875,-9.85223873629566));
#73333=CARTESIAN_POINT('Ctrl Pts',(-18.1410984204317,-20.9843249185812,
-9.85093631775104));
#73334=CARTESIAN_POINT('Ctrl Pts',(-18.1279527498485,-20.9804436402094,
-9.85012869961266));
#73335=CARTESIAN_POINT('Ctrl Pts',(-18.0291373443934,-20.9502218699535,
-9.84407038492819));
#73336=CARTESIAN_POINT('Ctrl Pts',(-17.9451747108148,-20.9185908271117,
-9.83899942898672));
#73337=CARTESIAN_POINT('Ctrl Pts',(-17.7339771197533,-20.823315479201,-9.82616914553694));
#73338=CARTESIAN_POINT('Ctrl Pts',(-17.6107065797325,-20.7520214298508,
-9.81861982055679));
#73339=CARTESIAN_POINT('Ctrl Pts',(-17.4517594198323,-20.6373657814144,
-9.80778302533903));
#73340=CARTESIAN_POINT('Ctrl Pts',(-17.4092366908299,-20.6041501435285,
-9.80475710136688));
#73341=CARTESIAN_POINT('Ctrl Pts',(-17.3466253420211,-20.5512703503387,
-9.80002727420146));
#73342=CARTESIAN_POINT('Ctrl Pts',(-17.3255811193627,-20.5327688572244,
-9.79838718134557));
#73343=CARTESIAN_POINT('Ctrl Pts',(-17.2998160340355,-20.5091939672304,
-9.79630625488515));
#73344=CARTESIAN_POINT('Ctrl Pts',(-17.2947435572111,-20.5045068723515,
-9.79589295518321));
#73345=CARTESIAN_POINT('Ctrl Pts',(-17.2867432949987,-20.4970415268961,
-9.79523516940728));
#73346=CARTESIAN_POINT('Ctrl Pts',(-17.2838003127209,-20.4942795325081,
-9.79499191100239));
#73347=CARTESIAN_POINT('Ctrl Pts',(-17.2782580721514,-20.4890482403505,
-9.79453133156171));
#73348=CARTESIAN_POINT('Ctrl Pts',(-17.2756571816422,-20.4865807496129,
-9.79431414798781));
#73349=CARTESIAN_POINT('Ctrl Pts',(-17.2697164939023,-20.4809160181113,
-9.79381570512716));
#73350=CARTESIAN_POINT('Ctrl Pts',(-17.266380897832,-20.4777144381185,-9.79353411174673));
#73351=CARTESIAN_POINT('Ctrl Pts',(-17.257535353891,-20.4691684387349,-9.79278282535843));
#73352=CARTESIAN_POINT('Ctrl Pts',(-17.2520439997879,-20.4638049914073,
-9.79231170494516));
#73353=CARTESIAN_POINT('Ctrl Pts',(-17.2132882755112,-20.425537927177,-9.78895388474047));
#73354=CARTESIAN_POINT('Ctrl Pts',(-17.1810961794957,-20.3915718693035,
-9.78599202321496));
#73355=CARTESIAN_POINT('Ctrl Pts',(-17.125316260505,-20.3286685569773,-9.78058303947507));
#73356=CARTESIAN_POINT('Ctrl Pts',(-17.1013166005308,-20.3001188335241,
-9.77815421222783));
#73357=CARTESIAN_POINT('Ctrl Pts',(-17.0034145093029,-20.1772048310218,
-9.76785133107912));
#73358=CARTESIAN_POINT('Ctrl Pts',(-16.9368360057211,-20.0772807742351,
-9.75986013238943));
#73359=CARTESIAN_POINT('Ctrl Pts',(-16.832227970176,-19.8870934150451,-9.7457418953503));
#73360=CARTESIAN_POINT('Ctrl Pts',(-16.7913005351884,-19.7987938478536,
-9.73956111761863));
#73361=CARTESIAN_POINT('Ctrl Pts',(-16.7488668865826,-19.6878004950989,
-9.73226044158712));
#73362=CARTESIAN_POINT('Ctrl Pts',(-16.741460351778,-19.667500979143,-9.73094324512345));
#73363=CARTESIAN_POINT('Ctrl Pts',(-16.7313955261904,-19.6385465398602,
-9.72908925942552));
#73364=CARTESIAN_POINT('Ctrl Pts',(-16.7284801478685,-19.6299830061242,
-9.72854397239901));
#73365=CARTESIAN_POINT('Ctrl Pts',(-16.7235539724407,-19.6152031739237,
-9.72760801752366));
#73366=CARTESIAN_POINT('Ctrl Pts',(-16.7215169142161,-19.6089958223235,
-9.72721648621118));
#73367=CARTESIAN_POINT('Ctrl Pts',(-16.7176772865902,-19.5971102270746,
-9.72646973591365));
#73368=CARTESIAN_POINT('Ctrl Pts',(-16.7158698908773,-19.5914336192741,
-9.72611436109393));
#73369=CARTESIAN_POINT('Ctrl Pts',(-16.7112444253581,-19.5766911355542,
-9.72519469576326));
#73370=CARTESIAN_POINT('Ctrl Pts',(-16.7084633142987,-19.5676137335427,
-9.72463162152827));
#73371=CARTESIAN_POINT('Ctrl Pts',(-16.6992477313659,-19.5367958958989,
-9.7227305302328));
#73372=CARTESIAN_POINT('Ctrl Pts',(-16.6931013323144,-19.5149704444151,
-9.721401902303));
#73373=CARTESIAN_POINT('Ctrl Pts',(-16.6414326919542,-19.3195173403618,
-9.70965054102293));
#73374=CARTESIAN_POINT('Ctrl Pts',(-16.6178134052955,-19.1408589724949,
-9.70001951991667));
#73375=CARTESIAN_POINT('Ctrl Pts',(-16.6166486753162,-18.8771219636983,
-9.68565936986543));
#73376=CARTESIAN_POINT('Ctrl Pts',(-16.6213037377898,-18.7929540282656,
-9.68103996703634));
#73377=CARTESIAN_POINT('Ctrl Pts',(-16.6352132691489,-18.6724279936042,
-9.6741078324025));
#73378=CARTESIAN_POINT('Ctrl Pts',(-16.6404363192971,-18.6356821462556,
-9.67195098004826));
#73379=CARTESIAN_POINT('Ctrl Pts',(-16.6478772898762,-18.5916699458051,
-9.66929497372547));
#73380=CARTESIAN_POINT('Ctrl Pts',(-16.6491722301562,-18.5842516133608,
-9.66884480030381));
#73381=CARTESIAN_POINT('Ctrl Pts',(-16.6512462681675,-18.5727331951739,
-9.66814170974775));
#73382=CARTESIAN_POINT('Ctrl Pts',(-16.651997972521,-18.5686281523267,-9.66789032309219));
#73383=CARTESIAN_POINT('Ctrl Pts',(-16.6534142251776,-18.5610210495021,
-9.66742292332395));
#73384=CARTESIAN_POINT('Ctrl Pts',(-16.6540754819808,-18.5575184353135,
-9.66720709886792));
#73385=CARTESIAN_POINT('Ctrl Pts',(-16.6555900121567,-18.549605791886,-9.66671815109773));
#73386=CARTESIAN_POINT('Ctrl Pts',(-16.6564484722836,-18.5451968226364,
-9.66644473670408));
#73387=CARTESIAN_POINT('Ctrl Pts',(-16.6590225197354,-18.5321974328358,
-9.66563580735149));
#73388=CARTESIAN_POINT('Ctrl Pts',(-16.6607773790297,-18.5236150133232,
-9.66509813241869));
#73389=CARTESIAN_POINT('Ctrl Pts',(-16.6738110976748,-18.4618279479156,
-9.66120246731753));
#73390=CARTESIAN_POINT('Ctrl Pts',(-16.6870823566694,-18.4090690423848,
-9.65774360085324));
#73391=CARTESIAN_POINT('Ctrl Pts',(-16.7108441930768,-18.3279498005957,
-9.65227698936044));
#73392=CARTESIAN_POINT('Ctrl Pts',(-16.7199369000747,-18.2992000357889,
-9.65030978437348));
#73393=CARTESIAN_POINT('Ctrl Pts',(-16.7713401227965,-18.1479835772066,
-9.63983436637738));
#73394=CARTESIAN_POINT('Ctrl Pts',(-16.824217386032,-18.0293894530551,-9.63119000482233));
#73395=CARTESIAN_POINT('Ctrl Pts',(-16.9306818126656,-17.8395766510796,
-9.61710026501743));
#73396=CARTESIAN_POINT('Ctrl Pts',(-16.978509845372,-17.7655347035796,-9.61152531949231));
#73397=CARTESIAN_POINT('Ctrl Pts',(-17.0429909979033,-17.6781877217658,
-9.60486247567757));
#73398=CARTESIAN_POINT('Ctrl Pts',(-17.0554042510384,-17.6618738343458,
-9.60361380607884));
#73399=CARTESIAN_POINT('Ctrl Pts',(-17.0735176763853,-17.6387727184145,
-9.60183895739354));
#73400=CARTESIAN_POINT('Ctrl Pts',(-17.079026259512,-17.6318373728369,-9.60130523435084));
#73401=CARTESIAN_POINT('Ctrl Pts',(-17.0886522634915,-17.619873105309,-9.6003828888715));
#73402=CARTESIAN_POINT('Ctrl Pts',(-17.0927495877286,-17.6148282371837,
-9.59999346825073));
#73403=CARTESIAN_POINT('Ctrl Pts',(-17.1006730807913,-17.6051636497448,
-9.59924643714513));
#73404=CARTESIAN_POINT('Ctrl Pts',(-17.1044957741889,-17.6005411739219,
-9.59888869152701));
#73405=CARTESIAN_POINT('Ctrl Pts',(-17.114563022773,-17.5884724735427,-9.59795344186742));
#73406=CARTESIAN_POINT('Ctrl Pts',(-17.120839340106,-17.5810528351643,-9.59737723875789));
#73407=CARTESIAN_POINT('Ctrl Pts',(-17.1428071232989,-17.5554430492663,
-9.59538384914218));
#73408=CARTESIAN_POINT('Ctrl Pts',(-17.1587573069793,-17.5374765414124,
-9.59397735247406));
#73409=CARTESIAN_POINT('Ctrl Pts',(-17.2748615069997,-17.4110952165873,
-9.58401517828428));
#73410=CARTESIAN_POINT('Ctrl Pts',(-17.3858071246414,-17.3131420658155,
-9.5759648193249));
#73411=CARTESIAN_POINT('Ctrl Pts',(-17.5440876299469,-17.2004356420584,
-9.56541234292053));
#73412=CARTESIAN_POINT('Ctrl Pts',(-17.5830075365717,-17.174618387826,-9.56287946376296));
#73413=CARTESIAN_POINT('Ctrl Pts',(-17.6835054484938,-17.1126399076543,
-9.55642055143619));
#73414=CARTESIAN_POINT('Ctrl Pts',(-17.7461140354447,-17.0782699973492,
-9.55247085455544));
#73415=CARTESIAN_POINT('Ctrl Pts',(-17.8405396986962,-17.0324832248759,
-9.54645231114514));
#73416=CARTESIAN_POINT('Ctrl Pts',(-17.871088305706,-17.0185577117792,-9.54449595810553));
#73417=CARTESIAN_POINT('Ctrl Pts',(-17.908675575444,-17.0024918458974,-9.54206250117054));
#73418=CARTESIAN_POINT('Ctrl Pts',(-17.9154128236215,-16.9996533402576,
-9.54162530516594));
#73419=CARTESIAN_POINT('Ctrl Pts',(-17.925974477908,-16.9952678328126,-9.54093814484613));
#73420=CARTESIAN_POINT('Ctrl Pts',(-17.9297890073633,-16.9936969853691,
-9.54068960116459));
#73421=CARTESIAN_POINT('Ctrl Pts',(-17.9369129055815,-16.9907876434509,
-9.5402247078457));
#73422=CARTESIAN_POINT('Ctrl Pts',(-17.9402210768033,-16.9894463665882,
-9.54000852936465));
#73423=CARTESIAN_POINT('Ctrl Pts',(-17.9477612673617,-16.9864114281703,
-9.5395151434047));
#73424=CARTESIAN_POINT('Ctrl Pts',(-17.9519953573566,-16.9847230707411,
-9.53923762199125));
#73425=CARTESIAN_POINT('Ctrl Pts',(-17.963017968391,-16.9803689753294,-9.53851399933805));
#73426=CARTESIAN_POINT('Ctrl Pts',(-17.9698148047226,-16.977724645775,-9.53806666262228));
#73427=CARTESIAN_POINT('Ctrl Pts',(-18.013179568873,-16.9611109354619,-9.53520602376663));
#73428=CARTESIAN_POINT('Ctrl Pts',(-18.0501129063736,-16.94812391682,-9.53274008093113));
#73429=CARTESIAN_POINT('Ctrl Pts',(-18.09913364696,-16.932399539207,-9.52944766422414));
#73430=CARTESIAN_POINT('Ctrl Pts',(-18.110917694779,-16.9287329050173,-9.52865473877205));
#73431=CARTESIAN_POINT('Ctrl Pts',(-18.1458489420505,-16.9181980711818,
-9.52630122535594));
#73432=CARTESIAN_POINT('Ctrl Pts',(-18.169081944689,-16.9116227110253,-9.52473195480415));
#73433=CARTESIAN_POINT('Ctrl Pts',(-18.3317801037737,-16.868567990221,-9.51373622242815));
#73434=CARTESIAN_POINT('Ctrl Pts',(-18.4745550596188,-16.8460172956255,
-9.50408909060972));
#73435=CARTESIAN_POINT('Ctrl Pts',(-18.6802311525133,-16.8347805084393,
-9.4907808297797));
#73436=CARTESIAN_POINT('Ctrl Pts',(-18.7420711537337,-16.8341129747927,
-9.48684923847594));
#73437=CARTESIAN_POINT('Ctrl Pts',(-18.841095182424,-16.8373823395173,-9.48067561603798));
#73438=CARTESIAN_POINT('Ctrl Pts',(-18.8782965828865,-16.8395947356132,
-9.47838366909235));
#73439=CARTESIAN_POINT('Ctrl Pts',(-18.9265161368928,-16.8437423012779,
-9.47544657393694));
#73440=CARTESIAN_POINT('Ctrl Pts',(-18.9376025871686,-16.8447840687048,
-9.47477359345177));
#73441=CARTESIAN_POINT('Ctrl Pts',(-18.9556144891969,-16.8466200821777,
-9.47368384270458));
#73442=CARTESIAN_POINT('Ctrl Pts',(-18.9625450384104,-16.8473611361049,
-9.47326540656282));
#73443=CARTESIAN_POINT('Ctrl Pts',(-18.975862700996,-16.8488516960841,-9.47246298271339));
#73444=CARTESIAN_POINT('Ctrl Pts',(-18.9822502967018,-16.8495961030302,
-9.47207883908743));
#73445=CARTESIAN_POINT('Ctrl Pts',(-18.9968632841322,-16.8513666189717,
-9.47120164581598));
#73446=CARTESIAN_POINT('Ctrl Pts',(-19.0050862730904,-16.8524119587024,
-9.47070920810994));
#73447=CARTESIAN_POINT('Ctrl Pts',(-19.0269054791241,-16.8553160263316,
-9.46940555241348));
#73448=CARTESIAN_POINT('Ctrl Pts',(-19.0404902642397,-16.8572587185303,
-9.46859698616855));
#73449=CARTESIAN_POINT('Ctrl Pts',(-19.1432878681387,-16.8729807320672,
-9.4625001512217));
#73450=CARTESIAN_POINT('Ctrl Pts',(-19.2315619322145,-16.8923221941895,
-9.45739437134887));
#73451=CARTESIAN_POINT('Ctrl Pts',(-19.4524106249719,-16.9557453951669,
-9.44467439946604));
#73452=CARTESIAN_POINT('Ctrl Pts',(-19.5823413464641,-17.0074020005798,
-9.43725493722378));
#73453=CARTESIAN_POINT('Ctrl Pts',(-19.7553603436323,-17.0968533118509,
-9.426496199625));
#73454=CARTESIAN_POINT('Ctrl Pts',(-19.8034593232911,-17.1241591722003,
-9.42339809171695));
#73455=CARTESIAN_POINT('Ctrl Pts',(-19.8746319587823,-17.1683354940968,
-9.41856620426507));
#73456=CARTESIAN_POINT('Ctrl Pts',(-19.8985260666795,-17.1838429947864,
-9.41689955795282));
#73457=CARTESIAN_POINT('Ctrl Pts',(-19.9278456865798,-17.2037237946812,
-9.41478893695049));
#73458=CARTESIAN_POINT('Ctrl Pts',(-19.9335733762604,-17.2076488526192,
-9.4143734448464));
#73459=CARTESIAN_POINT('Ctrl Pts',(-19.942606417804,-17.2139045241028,-9.41371296238759));
#73460=CARTESIAN_POINT('Ctrl Pts',(-19.9459246364139,-17.2162165942969,
-9.41346921690699));
#73461=CARTESIAN_POINT('Ctrl Pts',(-19.9521703939516,-17.2205951564529,
-9.4130082616476));
#73462=CARTESIAN_POINT('Ctrl Pts',(-19.9550993185081,-17.2226595781681,
-9.41279119251213));
#73463=CARTESIAN_POINT('Ctrl Pts',(-19.9617838673207,-17.2273965607995,
-9.4122937239963));
#73464=CARTESIAN_POINT('Ctrl Pts',(-19.9655360090366,-17.2300739548765,
-9.41201299520463));
#73465=CARTESIAN_POINT('Ctrl Pts',(-19.9754745422914,-17.2372148369655,
-9.41126550719833));
#73466=CARTESIAN_POINT('Ctrl Pts',(-19.9816455371486,-17.2416994988799,
-9.41079734288748));
#73467=CARTESIAN_POINT('Ctrl Pts',(-20.0247024892636,-17.2733474136382,
-9.40750321031105));
#73468=CARTESIAN_POINT('Ctrl Pts',(-20.0607197076459,-17.3016662306517,
-9.40460517835694));
#73469=CARTESIAN_POINT('Ctrl Pts',(-20.1245701891533,-17.3553106737324,
-9.39924373375802));
#73470=CARTESIAN_POINT('Ctrl Pts',(-20.1527029732708,-17.3802545042879,
-9.39679636136647));
#73471=CARTESIAN_POINT('Ctrl Pts',(-20.2758195000087,-17.4954148755112,
-9.38574623983081));
#73472=CARTESIAN_POINT('Ctrl Pts',(-20.3629793690467,-17.5935900853675,
-9.37700304687893));
#73473=CARTESIAN_POINT('Ctrl Pts',(-20.4927973318511,-17.7704210507134,
-9.36279858849358));
#73474=CARTESIAN_POINT('Ctrl Pts',(-20.5405828581872,-17.8448601402593,
-9.35720319140505));
#73475=CARTESIAN_POINT('Ctrl Pts',(-20.5935715947112,-17.9400196480767,
-9.3505186859072));
#73476=CARTESIAN_POINT('Ctrl Pts',(-20.603301284846,-17.9581068962629,-9.3492676328467));
#73477=CARTESIAN_POINT('Ctrl Pts',(-20.6168513917212,-17.9841992996234,
-9.34749002346898));
#73478=CARTESIAN_POINT('Ctrl Pts',(-20.6208868719261,-17.9920908921971,
-9.34695589092577));
#73479=CARTESIAN_POINT('Ctrl Pts',(-20.627795797468,-18.0058135858679,-9.34603306533409));
#73480=CARTESIAN_POINT('Ctrl Pts',(-20.6306921438653,-18.0116329622653,
-9.34564357180678));
#73481=CARTESIAN_POINT('Ctrl Pts',(-20.6362088783901,-18.0228464369602,
-9.34489655859997));
#73482=CARTESIAN_POINT('Ctrl Pts',(-20.6388332360733,-18.0282385023041,
-9.34453890303502));
#73483=CARTESIAN_POINT('Ctrl Pts',(-20.6456466878981,-18.0423900748048,
-9.34360423846161));
#73484=CARTESIAN_POINT('Ctrl Pts',(-20.6497985237955,-18.0511674426622,
-9.34302852718004));
#73485=CARTESIAN_POINT('Ctrl Pts',(-20.6639911324903,-18.0817138848473,
-9.34103855239193));
#73486=CARTESIAN_POINT('Ctrl Pts',(-20.6737226582474,-18.1036252174408,
-9.33963492933289));
#73487=CARTESIAN_POINT('Ctrl Pts',(-20.7429144525703,-18.2668347027014,
-9.32934406891176));
#73488=CARTESIAN_POINT('Ctrl Pts',(-20.7872440731791,-18.4140553991742,
-9.32100723458071));
#73489=CARTESIAN_POINT('Ctrl Pts',(-20.839087984038,-18.6927191816881,-9.30561471876861));
#73490=CARTESIAN_POINT('Ctrl Pts',(-20.8510398086686,-18.8225565564254,
-9.29857231214665));
#73491=CARTESIAN_POINT('Ctrl Pts',(-20.850998895741,-18.9559243732588,-9.29078133015851));
#73492=CARTESIAN_POINT('Ctrl Pts',(-20.8509902917105,-18.9591992920498,
-9.29058966769631));
#73493=CARTESIAN_POINT('Ctrl Pts',(-20.8508966134014,-18.9781329928378,
-9.28947949059534));
#73494=CARTESIAN_POINT('Ctrl Pts',(-20.8506454051252,-18.9937899720814,
-9.2885531605265));
#73495=CARTESIAN_POINT('Ctrl Pts',(-20.8500635606029,-19.0152256289942,
-9.28727185036972));
#73496=CARTESIAN_POINT('Ctrl Pts',(-20.8498828710246,-19.0210083110181,
-9.28692488681997));
#73497=CARTESIAN_POINT('Ctrl Pts',(-20.849558006434,-19.0301981503566,-9.28637131489791));
#73498=CARTESIAN_POINT('Ctrl Pts',(-20.8494292968978,-19.0336058744959,
-9.28616556645554));
#73499=CARTESIAN_POINT('Ctrl Pts',(-20.849146397906,-19.0406449432384,-9.2857395573068));
#73500=CARTESIAN_POINT('Ctrl Pts',(-20.8489910906245,-19.0442761959381,
-9.2855192323764));
#73501=CARTESIAN_POINT('Ctrl Pts',(-20.8485986126162,-19.0529306526134,
-9.28499281799852));
#73502=CARTESIAN_POINT('Ctrl Pts',(-20.8483528935365,-19.0579534308632,
-9.28468625368016));
#73503=CARTESIAN_POINT('Ctrl Pts',(-20.8474631286402,-19.0749035421436,
-9.28364827220232));
#73504=CARTESIAN_POINT('Ctrl Pts',(-20.8467360466117,-19.0868260325307,
-9.28291242752136));
#73505=CARTESIAN_POINT('Ctrl Pts',(-20.8368860011543,-19.2285882718191,
-9.2740997440102));
#73506=CARTESIAN_POINT('Ctrl Pts',(-20.8159089736642,-19.3573131149155,
-9.26548282185087));
#73507=CARTESIAN_POINT('Ctrl Pts',(-20.7661583380872,-19.5492103473173,
-9.25238287201765));
#73508=CARTESIAN_POINT('Ctrl Pts',(-20.7459070626398,-19.6142266721053,
-9.24789438225943));
#73509=CARTESIAN_POINT('Ctrl Pts',(-20.7225807271506,-19.6781099721152,
-9.24346982890923));
#73510=CARTESIAN_POINT('Origin',(-18.734,-18.952,0.));
#73511=CARTESIAN_POINT('',(-20.7225805821191,-19.6781103693095,-8.44448865465826));
#73512=CARTESIAN_POINT('',(-20.7225804318258,-19.6781107809139,-8.66553671816755));
#73513=CARTESIAN_POINT('',(-20.7225805821191,-19.6781103693095,0.));
#73514=CARTESIAN_POINT('',(-20.8509999986719,-18.9519250126714,-8.71094372102528));
#73515=CARTESIAN_POINT('Ctrl Pts',(-20.7225804318258,-19.6781107809139,
-8.66553671816755));
#73516=CARTESIAN_POINT('Ctrl Pts',(-20.756070039132,-19.5863936772582,-8.67195993448919));
#73517=CARTESIAN_POINT('Ctrl Pts',(-20.7832013384852,-19.4923954521791,
-8.67845479377976));
#73518=CARTESIAN_POINT('Ctrl Pts',(-20.8168871681233,-19.3356413520089,
-8.68892803045935));
#73519=CARTESIAN_POINT('Ctrl Pts',(-20.8273110801215,-19.2739462484318,
-8.69296405635655));
#73520=CARTESIAN_POINT('Ctrl Pts',(-20.8382409136492,-19.1855831091221,
-8.69860368086808));
#73521=CARTESIAN_POINT('Ctrl Pts',(-20.840999390498,-19.1592306791796,-8.70026812315789));
#73522=CARTESIAN_POINT('Ctrl Pts',(-20.8463154977908,-19.0972226537623,
-8.70414340561251));
#73523=CARTESIAN_POINT('Ctrl Pts',(-20.8484662904148,-19.0615396384699,
-8.70634153903778));
#73524=CARTESIAN_POINT('Ctrl Pts',(-20.8501018469652,-19.0146622935275,
-8.70918916109573));
#73525=CARTESIAN_POINT('Ctrl Pts',(-20.8504028282684,-19.0035040360996,
-8.70986402003792));
#73526=CARTESIAN_POINT('Ctrl Pts',(-20.8507477576586,-18.9854074805868,
-8.71095383259111));
#73527=CARTESIAN_POINT('Ctrl Pts',(-20.8508458710089,-18.9784705400062,
-8.71137047554056));
#73528=CARTESIAN_POINT('Ctrl Pts',(-20.8509497984663,-18.9672073924015,
-8.71204518351584));
#73529=CARTESIAN_POINT('Ctrl Pts',(-20.8509764542952,-18.96288147049,-8.71230389906779));
#73530=CARTESIAN_POINT('Ctrl Pts',(-20.8509965706215,-18.9563852094995,
-8.71269178471987));
#73531=CARTESIAN_POINT('Ctrl Pts',(-20.8509999537557,-18.954214932766,-8.71282126450749));
#73532=CARTESIAN_POINT('Ctrl Pts',(-20.8509999995291,-18.9520446497005,
-8.71295064004092));
#73533=CARTESIAN_POINT('Ctrl Pts',(-20.8509999986719,-18.9519250126714,
-8.71094372102528));
#73534=CARTESIAN_POINT('Ctrl Pts',(-20.8509972790728,-18.8751468230116,
-8.71553605185446));
#73535=CARTESIAN_POINT('Ctrl Pts',(-20.8468134450973,-18.79845405233,-8.72012838268364));
#73536=CARTESIAN_POINT('Ctrl Pts',(-20.8385019469856,-18.7223033410474,
-8.72472071351282));
#73537=CARTESIAN_POINT('Ctrl Pts',(-20.8301661890791,-18.6459303592906,
-8.72932644854445));
#73538=CARTESIAN_POINT('Ctrl Pts',(-20.817678733725,-18.5701030045679,-8.73393218357608));
#73539=CARTESIAN_POINT('Ctrl Pts',(-20.8011445449259,-18.4952698494918,
-8.73853791860771));
#73540=CARTESIAN_POINT('Ctrl Pts',(-20.7845848825983,-18.4203214021249,
-8.74315074950135));
#73541=CARTESIAN_POINT('Ctrl Pts',(-20.7639661648778,-18.3463705997999,
-8.74776358039499));
#73542=CARTESIAN_POINT('Ctrl Pts',(-20.7394430352797,-18.2738501402727,
-8.75237641128863));
#73543=CARTESIAN_POINT('Ctrl Pts',(-20.714852135364,-18.2011292685364,-8.75700198986252));
#73544=CARTESIAN_POINT('Ctrl Pts',(-20.6863354068384,-18.1298470190297,
-8.76162756843642));
#73545=CARTESIAN_POINT('Ctrl Pts',(-20.6540955877916,-18.0604160534513,
-8.76625314701031));
#73546=CARTESIAN_POINT('Ctrl Pts',(-20.6367568977577,-18.023075831747,-8.76874079971715));
#73547=CARTESIAN_POINT('Ctrl Pts',(-20.6183421527928,-17.9862706239728,
-8.771228452424));
#73548=CARTESIAN_POINT('Ctrl Pts',(-20.598888138009,-17.950061262994,-8.77371610513084));
#73549=CARTESIAN_POINT('Ctrl Pts',(-20.5645713376047,-17.886188102246,-8.77810431406174));
#73550=CARTESIAN_POINT('Ctrl Pts',(-20.526902233303,-17.8239553476819,-8.78249252299264));
#73551=CARTESIAN_POINT('Ctrl Pts',(-20.4860618340582,-17.7637372640545,
-8.78688073192354));
#73552=CARTESIAN_POINT('Ctrl Pts',(-20.4452820487373,-17.7036085540475,
-8.79126242802481));
#73553=CARTESIAN_POINT('Ctrl Pts',(-20.4013405804883,-17.6454889751325,
-8.79564412412608));
#73554=CARTESIAN_POINT('Ctrl Pts',(-20.3544642120278,-17.589728097061,-8.80002582022735));
#73555=CARTESIAN_POINT('Ctrl Pts',(-20.3076429270308,-17.5340327424588,
-8.80440236748699));
#73556=CARTESIAN_POINT('Ctrl Pts',(-20.2578939016347,-17.4806909501821,
-8.80877891474663));
#73557=CARTESIAN_POINT('Ctrl Pts',(-20.2054860875598,-17.4300217826401,
-8.81315546200628));
#73558=CARTESIAN_POINT('Ctrl Pts',(-20.1531115097589,-17.3793847487478,
-8.81752923372325));
#73559=CARTESIAN_POINT('Ctrl Pts',(-20.0980818347929,-17.3314173110765,
-8.82190300544023));
#73560=CARTESIAN_POINT('Ctrl Pts',(-20.0407040448442,-17.2864029481331,
-8.82627677715721));
#73561=CARTESIAN_POINT('Ctrl Pts',(-19.9833437151498,-17.2414022832115,
-8.83064921792076));
#73562=CARTESIAN_POINT('Ctrl Pts',(-19.9236370683466,-17.1993532065247,
-8.83502165868432));
#73563=CARTESIAN_POINT('Ctrl Pts',(-19.8619241653159,-17.1604989318182,
-8.83939409944787));
#73564=CARTESIAN_POINT('Ctrl Pts',(-19.8002096842795,-17.1216436636036,
-8.84376665201522));
#73565=CARTESIAN_POINT('Ctrl Pts',(-19.7364892544389,-17.0859836148755,
-8.84813920458256));
#73566=CARTESIAN_POINT('Ctrl Pts',(-19.6711304798855,-17.0537177597445,
-8.8525117571499));
#73567=CARTESIAN_POINT('Ctrl Pts',(-19.6057038735305,-17.0214184178919,
-8.85688884771723));
#73568=CARTESIAN_POINT('Ctrl Pts',(-19.5386359610935,-16.9925205167793,
-8.86126593828456));
#73569=CARTESIAN_POINT('Ctrl Pts',(-19.4703166749601,-16.9671758883529,
-8.86564302885189));
#73570=CARTESIAN_POINT('Ctrl Pts',(-19.4019600771288,-16.9418174182843,
-8.87002250991083));
#73571=CARTESIAN_POINT('Ctrl Pts',(-19.3323512055631,-16.9200162288386,
-8.87440199096978));
#73572=CARTESIAN_POINT('Ctrl Pts',(-19.2618949953266,-16.9018741809564,
-8.87878147202872));
#73573=CARTESIAN_POINT('Ctrl Pts',(-19.1913139019304,-16.8836999764162,
-8.88316871568844));
#73574=CARTESIAN_POINT('Ctrl Pts',(-19.1198829437759,-16.8691979613858,
-8.88755595934816));
#73575=CARTESIAN_POINT('Ctrl Pts',(-19.0480164983078,-16.858418704996,-8.89194320300788));
#73576=CARTESIAN_POINT('Ctrl Pts',(-18.9991542404241,-16.8510898493377,
-8.89492610594268));
#73577=CARTESIAN_POINT('Ctrl Pts',(-18.9500908178364,-16.8454808253817,
-8.89790900887748));
#73578=CARTESIAN_POINT('Ctrl Pts',(-18.900956661124,-16.8415937658104,-8.90089191181227));
#73579=CARTESIAN_POINT('Ctrl Pts',(-18.8286744078926,-16.8358754337365,
-8.90528012074316));
#73580=CARTESIAN_POINT('Ctrl Pts',(-18.7559569381437,-16.8338637794812,
-8.90966832967406));
#73581=CARTESIAN_POINT('Ctrl Pts',(-18.6832169260197,-16.8356091855716,
-8.91405653860495));
#73582=CARTESIAN_POINT('Ctrl Pts',(-18.6105848721342,-16.8373520011899,
-8.91843823470622));
#73583=CARTESIAN_POINT('Ctrl Pts',(-18.5379308205421,-16.8428407963575,
-8.92281993080749));
#73584=CARTESIAN_POINT('Ctrl Pts',(-18.4656714572672,-16.8520740981752,
-8.92720162690876));
#73585=CARTESIAN_POINT('Ctrl Pts',(-18.3934970044949,-16.8612965501284,
-8.9315781741684));
#73586=CARTESIAN_POINT('Ctrl Pts',(-18.3217167948298,-16.8742547070803,
-8.93595472142803));
#73587=CARTESIAN_POINT('Ctrl Pts',(-18.2507446877308,-16.8908951256271,
-8.94033126868767));
#73588=CARTESIAN_POINT('Ctrl Pts',(-18.1798175901105,-16.9075249910624,
-8.94470504040464));
#73589=CARTESIAN_POINT('Ctrl Pts',(-18.1096980467019,-16.9278323748368,
-8.94907881212161));
#73590=CARTESIAN_POINT('Ctrl Pts',(-18.0407905817006,-16.9517125950552,
-8.95345258383859));
#73591=CARTESIAN_POINT('Ctrl Pts',(-17.9719040854723,-16.9755855484423,
-8.95782502460214));
#73592=CARTESIAN_POINT('Ctrl Pts',(-17.9042293909009,-17.0030290219352,
-8.96219746536569));
#73593=CARTESIAN_POINT('Ctrl Pts',(-17.8381550707623,-17.0338887251363,
-8.96656990612925));
#73594=CARTESIAN_POINT('Ctrl Pts',(-17.7720790610961,-17.0647492174235,
-8.97094245869659));
#73595=CARTESIAN_POINT('Ctrl Pts',(-17.7076039433217,-17.0990259069124,
-8.97531501126393));
#73596=CARTESIAN_POINT('Ctrl Pts',(-17.6450960003002,-17.1365173976494,
-8.97968756383127));
#73597=CARTESIAN_POINT('Ctrl Pts',(-17.5825231841776,-17.1740477984696,
-8.98406465439859));
#73598=CARTESIAN_POINT('Ctrl Pts',(-17.5219220335754,-17.2147994133216,
-8.98844174496592));
#73599=CARTESIAN_POINT('Ctrl Pts',(-17.463631278137,-17.25852655453,-8.99281883553324));
#73600=CARTESIAN_POINT('Ctrl Pts',(-17.4053086879535,-17.3022775767532,
-8.99719831659219));
#73601=CARTESIAN_POINT('Ctrl Pts',(-17.3492993758008,-17.3490070515425,
-9.00157779765112));
#73602=CARTESIAN_POINT('Ctrl Pts',(-17.2959081742799,-17.3984296279868,
-9.00595727871007));
#73603=CARTESIAN_POINT('Ctrl Pts',(-17.2424223372128,-17.4479398056162,
-9.01034452236979));
#73604=CARTESIAN_POINT('Ctrl Pts',(-17.1915642147122,-17.5001522715464,
-9.01473176602951));
#73605=CARTESIAN_POINT('Ctrl Pts',(-17.1436006220657,-17.5547459720344,
-9.01911900968923));
#73606=CARTESIAN_POINT('Ctrl Pts',(-17.1109900008268,-17.5918644277299,
-9.02210191262405));
#73607=CARTESIAN_POINT('Ctrl Pts',(-17.0797165992414,-17.6300829433876,
-9.02508481555887));
#73608=CARTESIAN_POINT('Ctrl Pts',(-17.0498528101568,-17.6692930019123,
-9.0280677184937));
#73609=CARTESIAN_POINT('Ctrl Pts',(-17.0059195850955,-17.7269757132704,
-9.03245592742459));
#73610=CARTESIAN_POINT('Ctrl Pts',(-16.9648675150388,-17.7870307272458,
-9.03684413635549));
#73611=CARTESIAN_POINT('Ctrl Pts',(-16.926962336405,-17.8491383212981,-9.04123234528639));
#73612=CARTESIAN_POINT('Ctrl Pts',(-16.8891134153411,-17.9111537373832,
-9.04561404138765));
#73613=CARTESIAN_POINT('Ctrl Pts',(-16.8544023633227,-17.9752152777401,
-9.04999573748892));
#73614=CARTESIAN_POINT('Ctrl Pts',(-16.8230534861162,-18.0409717781125,
-9.05437743359019));
#73615=CARTESIAN_POINT('Ctrl Pts',(-16.7917414463353,-18.106651009364,-9.05875398084983));
#73616=CARTESIAN_POINT('Ctrl Pts',(-16.7637839395867,-18.174020810815,-9.06313052810946));
#73617=CARTESIAN_POINT('Ctrl Pts',(-16.739360042701,-18.2427042642548,-9.0675070753691));
#73618=CARTESIAN_POINT('Ctrl Pts',(-16.7149516350958,-18.3113441596467,
-9.07188084708608));
#73619=CARTESIAN_POINT('Ctrl Pts',(-16.6940725522121,-18.3812956006721,
-9.07625461880305));
#73620=CARTESIAN_POINT('Ctrl Pts',(-16.6768537344172,-18.4521617841754,
-9.08062839052003));
#73621=CARTESIAN_POINT('Ctrl Pts',(-16.6596401563663,-18.5230064028611,
-9.08500083128358));
#73622=CARTESIAN_POINT('Ctrl Pts',(-16.6460847459307,-18.5947647429381,
-9.08937327204712));
#73623=CARTESIAN_POINT('Ctrl Pts',(-16.6362680963765,-18.667026561729,-9.09374571281068));
#73624=CARTESIAN_POINT('Ctrl Pts',(-16.6264511958094,-18.7392902282626,
-9.09811826537802));
#73625=CARTESIAN_POINT('Ctrl Pts',(-16.620373308882,-18.8120569208139,-9.10249081794537));
#73626=CARTESIAN_POINT('Ctrl Pts',(-16.6180633554341,-18.8849096416521,
-9.10686337051271));
#73627=CARTESIAN_POINT('Ctrl Pts',(-16.6157510046294,-18.957837971792,-9.11124046108004));
#73628=CARTESIAN_POINT('Ctrl Pts',(-16.6172144102078,-19.0308520253124,
-9.11561755164736));
#73629=CARTESIAN_POINT('Ctrl Pts',(-16.6224303356467,-19.1035339981093,
-9.11999464221469));
#73630=CARTESIAN_POINT('Ctrl Pts',(-16.6276491096961,-19.1762556652293,
-9.12437412327363));
#73631=CARTESIAN_POINT('Ctrl Pts',(-16.6366244245266,-19.2486444114927,
-9.12875360433257));
#73632=CARTESIAN_POINT('Ctrl Pts',(-16.649281345285,-19.320289465887,-9.13313308539151));
#73633=CARTESIAN_POINT('Ctrl Pts',(-16.6619607003505,-19.3920615106593,
-9.13752032905123));
#73634=CARTESIAN_POINT('Ctrl Pts',(-16.6783345842869,-19.4630867607301,
-9.14190757271095));
#73635=CARTESIAN_POINT('Ctrl Pts',(-16.6982774637589,-19.5329670863655,
-9.14629481637068));
#73636=CARTESIAN_POINT('Ctrl Pts',(-16.7118367001085,-19.5804789741454,
-9.1492777193055));
#73637=CARTESIAN_POINT('Ctrl Pts',(-16.7270447244343,-19.6274619134097,
-9.15226062224032));
#73638=CARTESIAN_POINT('Ctrl Pts',(-16.7438494759073,-19.6737962949846,
-9.15524352517514));
#73639=CARTESIAN_POINT('Ctrl Pts',(-16.7685712862063,-19.7419597422966,
-9.15963173410604));
#73640=CARTESIAN_POINT('Ctrl Pts',(-16.7968473421401,-19.8089846766148,
-9.16401994303694));
#73641=CARTESIAN_POINT('Ctrl Pts',(-16.8285526457323,-19.8744745959181,
-9.16840815196783));
#73642=CARTESIAN_POINT('Ctrl Pts',(-16.8602108933972,-19.9398673173227,
-9.1727898480691));
#73643=CARTESIAN_POINT('Ctrl Pts',(-16.8952880767684,-20.0037291156991,
-9.17717154417037));
#73644=CARTESIAN_POINT('Ctrl Pts',(-16.9336103347365,-20.0656813068434,
-9.18155324027164));
#73645=CARTESIAN_POINT('Ctrl Pts',(-16.9718875610017,-20.1275606992327,
-9.18592978753128));
#73646=CARTESIAN_POINT('Ctrl Pts',(-17.0134020343728,-20.187534533793,-9.19030633479092));
#73647=CARTESIAN_POINT('Ctrl Pts',(-17.0579337571752,-20.2452482165706,
-9.19468288205056));
#73648=CARTESIAN_POINT('Ctrl Pts',(-17.1024372386062,-20.3029252981694,
-9.19905665376753));
#73649=CARTESIAN_POINT('Ctrl Pts',(-17.1499538788912,-20.3583446909812,
-9.20343042548451));
#73650=CARTESIAN_POINT('Ctrl Pts',(-17.2002209049092,-20.4111815128566,
-9.20780419720148));
#73651=CARTESIAN_POINT('Ctrl Pts',(-17.2504726345023,-20.4640022563097,
-9.21217663796503));
#73652=CARTESIAN_POINT('Ctrl Pts',(-17.3034727559334,-20.514241639775,-9.21654907872858));
#73653=CARTESIAN_POINT('Ctrl Pts',(-17.3589199436397,-20.5616098404893,
-9.22092151949214));
#73654=CARTESIAN_POINT('Ctrl Pts',(-17.4143685491366,-20.6089792524138,
-9.22529407205948));
#73655=CARTESIAN_POINT('Ctrl Pts',(-17.4722639770758,-20.6534770240218,
-9.22966662462682));
#73656=CARTESIAN_POINT('Ctrl Pts',(-17.5322712521182,-20.694853125342,-9.23403917719417));
#73657=CARTESIAN_POINT('Ctrl Pts',(-17.592340804974,-20.7362721683409,-9.23841626776149));
#73658=CARTESIAN_POINT('Ctrl Pts',(-17.6545261829441,-20.7745627981879,
-9.24279335832882));
#73659=CARTESIAN_POINT('Ctrl Pts',(-17.718463501407,-20.8095184036842,-9.24717044889615));
#73660=CARTESIAN_POINT('Ctrl Pts',(-17.7824357384127,-20.8444930997341,
-9.25154992995509));
#73661=CARTESIAN_POINT('Ctrl Pts',(-17.8481613859402,-20.8761289357272,
-9.25592941101403));
#73662=CARTESIAN_POINT('Ctrl Pts',(-17.9152544897592,-20.9042665774582,
-9.26030889207298));
#73663=CARTESIAN_POINT('Ctrl Pts',(-17.9824665156543,-20.9324540929703,
-9.2646961357327));
#73664=CARTESIAN_POINT('Ctrl Pts',(-18.051050383794,-20.9571308685661,-9.26908337939242));
#73665=CARTESIAN_POINT('Ctrl Pts',(-18.1206033812636,-20.9781869578404,
-9.27347062305214));
#73666=CARTESIAN_POINT('Ctrl Pts',(-18.1678927174319,-20.992503069587,-9.27645352598695));
#73667=CARTESIAN_POINT('Ctrl Pts',(-18.2156297492661,-21.0051465017728,
-9.27943642892176));
#73668=CARTESIAN_POINT('Ctrl Pts',(-18.2636857248405,-21.0160962871391,
-9.28241933185657));
#73669=CARTESIAN_POINT('Ctrl Pts',(-18.3343818439592,-21.0322047381968,
-9.28680754078746));
#73670=CARTESIAN_POINT('Ctrl Pts',(-18.4060444995741,-21.0447083756574,
-9.29119574971836));
#73671=CARTESIAN_POINT('Ctrl Pts',(-18.4782726371996,-21.0534976840137,
-9.29558395864926));
#73672=CARTESIAN_POINT('Ctrl Pts',(-18.5503935762932,-21.0622739475792,
-9.29996565475053));
#73673=CARTESIAN_POINT('Ctrl Pts',(-18.6230778564465,-21.0673467676749,
-9.3043473508518));
#73674=CARTESIAN_POINT('Ctrl Pts',(-18.695912956451,-21.0686573594027,-9.30872904695307));
#73675=CARTESIAN_POINT('Ctrl Pts',(-18.7686624694166,-21.0699664110809,
-9.31310559421271));
#73676=CARTESIAN_POINT('Ctrl Pts',(-18.8415619702683,-21.0675220079374,
-9.31748214147234));
#73677=CARTESIAN_POINT('Ctrl Pts',(-18.9141942210379,-21.0613171982195,
-9.32185868873198));
#73678=CARTESIAN_POINT('Ctrl Pts',(-18.9867804094897,-21.0551163235017,
-9.32623246044896));
#73679=CARTESIAN_POINT('Ctrl Pts',(-19.0590992046973,-21.0451598149104,
-9.33060623216593));
#73680=CARTESIAN_POINT('Ctrl Pts',(-19.1307351980801,-21.0314927705102,
-9.3349800038829));
#73681=CARTESIAN_POINT('Ctrl Pts',(-19.2023493923896,-21.0178298850376,
-9.33935244464645));
#73682=CARTESIAN_POINT('Ctrl Pts',(-19.273280723833,-21.0004587957695,-9.34372488541001));
#73683=CARTESIAN_POINT('Ctrl Pts',(-19.3431223955197,-20.979475994254,-9.34809732617356));
#73684=CARTESIAN_POINT('Ctrl Pts',(-19.4129658530657,-20.9584926562059,
-9.35246987874091));
#73685=CARTESIAN_POINT('Ctrl Pts',(-19.4817191341329,-20.9338975632636,
-9.35684243130824));
#73686=CARTESIAN_POINT('Ctrl Pts',(-19.5489906872856,-20.9058370401949,
-9.36121498387559));
#73687=CARTESIAN_POINT('Ctrl Pts',(-19.6163320573937,-20.877747394857,-9.36559207444291));
#73688=CARTESIAN_POINT('Ctrl Pts',(-19.6821881831277,-20.8461853247306,
-9.36996916501024));
#73689=CARTESIAN_POINT('Ctrl Pts',(-19.7461883733224,-20.8113449644729,
-9.37434625557757));
#73690=CARTESIAN_POINT('Ctrl Pts',(-19.8102235163964,-20.7764855766014,
-9.37872573663651));
#73691=CARTESIAN_POINT('Ctrl Pts',(-19.8724002944082,-20.738344586342,-9.38310521769545));
#73692=CARTESIAN_POINT('Ctrl Pts',(-19.9323758228015,-20.6971602755406,
-9.38748469875439));
#73693=CARTESIAN_POINT('Ctrl Pts',(-19.9924576574162,-20.6559029658247,
-9.39187194241411));
#73694=CARTESIAN_POINT('Ctrl Pts',(-20.0503300675359,-20.6115918569496,
-9.39625918607383));
#73695=CARTESIAN_POINT('Ctrl Pts',(-20.1056826247706,-20.5645060548421,
-9.40064642973355));
#73696=CARTESIAN_POINT('Ctrl Pts',(-20.1433170299305,-20.532492246586,-9.40362933266837));
#73697=CARTESIAN_POINT('Ctrl Pts',(-20.1797873054598,-20.4991966074029,
-9.40661223560319));
#73698=CARTESIAN_POINT('Ctrl Pts',(-20.2150061302366,-20.4647160481074,
-9.409595138538));
#73699=CARTESIAN_POINT('Ctrl Pts',(-20.2660736595598,-20.4147190086245,
-9.41392036756134));
#73700=CARTESIAN_POINT('Ctrl Pts',(-20.3147200093879,-20.3620217118595,
-9.41824559658467));
#73701=CARTESIAN_POINT('Ctrl Pts',(-20.3606400168238,-20.3068916029216,
-9.422570825608));
#73702=CARTESIAN_POINT('Ctrl Pts',(-20.4064831242461,-20.2518538177085,
-9.42688881137966));
#73703=CARTESIAN_POINT('Ctrl Pts',(-20.4496086381081,-20.194391687308,-9.43120679715132));
#73704=CARTESIAN_POINT('Ctrl Pts',(-20.4897475359155,-20.1348100397472,
-9.43552478292298));
#73705=CARTESIAN_POINT('Ctrl Pts',(-20.5298476914605,-20.0752859006867,
-9.43983860095346));
#73706=CARTESIAN_POINT('Ctrl Pts',(-20.5669666687588,-20.0136467099182,
-9.44415241898393));
#73707=CARTESIAN_POINT('Ctrl Pts',(-20.6008760498832,-19.9502298404538,
-9.44846623701441));
#73708=CARTESIAN_POINT('Ctrl Pts',(-20.634764851022,-19.8868514594022,-9.4527774369401));
#73709=CARTESIAN_POINT('Ctrl Pts',(-20.6654476851597,-19.8216979770398,
-9.45708863686578));
#73710=CARTESIAN_POINT('Ctrl Pts',(-20.6927407815271,-19.7551335821535,
-9.46139983679147));
#73711=CARTESIAN_POINT('Ctrl Pts',(-20.7031862176723,-19.7296584903219,
-9.4630497911582));
#73712=CARTESIAN_POINT('Ctrl Pts',(-20.7131356416779,-19.7039769950381,
-9.46469974552493));
#73713=CARTESIAN_POINT('Ctrl Pts',(-20.7225805821191,-19.6781103693095,
-9.46634969989166));
#73714=CARTESIAN_POINT('',(-20.8509991049198,-18.9500532671891,-8.48905627902251));
#73715=CARTESIAN_POINT('Ctrl Pts',(-20.7225807271506,-19.6781099721152,
-9.24346982890923));
#73716=CARTESIAN_POINT('Ctrl Pts',(-20.6903081412074,-19.7664941630596,
-9.23734834539027));
#73717=CARTESIAN_POINT('Ctrl Pts',(-20.6521492195846,-19.8527097500488,
-9.23135288011962));
#73718=CARTESIAN_POINT('Ctrl Pts',(-20.5973011252839,-19.9571668947513,
-9.22408573268242));
#73719=CARTESIAN_POINT('Ctrl Pts',(-20.5859221923446,-19.9779804262763,
-9.22263712070413));
#73720=CARTESIAN_POINT('Ctrl Pts',(-20.5694164036234,-20.0070019308189,
-9.22061563734104));
#73721=CARTESIAN_POINT('Ctrl Pts',(-20.5645797432616,-20.015372116021,-9.22003242009133));
#73722=CARTESIAN_POINT('Ctrl Pts',(-20.5566540595066,-20.0288737371604,
-9.21909125274794));
#73723=CARTESIAN_POINT('Ctrl Pts',(-20.5536003367204,-20.0340256384089,
-9.21873202952226));
#73724=CARTESIAN_POINT('Ctrl Pts',(-20.5471835377953,-20.0447473586356,
-9.21798421248231));
#73725=CARTESIAN_POINT('Ctrl Pts',(-20.5438165598497,-20.0503147785078,
-9.21759576604661));
#73726=CARTESIAN_POINT('Ctrl Pts',(-20.5357843430347,-20.0634591097778,
-9.21667830923621));
#73727=CARTESIAN_POINT('Ctrl Pts',(-20.5310968725028,-20.0710223438505,
-9.21615012147147));
#73728=CARTESIAN_POINT('Ctrl Pts',(-20.5153273240207,-20.0961118548183,
-9.21439682040229));
#73729=CARTESIAN_POINT('Ctrl Pts',(-20.5040352295017,-20.1135051885399,
-9.21317948307665));
#73730=CARTESIAN_POINT('Ctrl Pts',(-20.442391950146,-20.205467732651,-9.20672839923418));
#73731=CARTESIAN_POINT('Ctrl Pts',(-20.3875781975563,-20.2769400880788,
-9.20166760661514));
#73732=CARTESIAN_POINT('Ctrl Pts',(-20.239228168277,-20.4467709831743,-9.18923032568631));
#73733=CARTESIAN_POINT('Ctrl Pts',(-20.14049106098,-20.5400279545725,-9.18201783936024));
#73734=CARTESIAN_POINT('Ctrl Pts',(-19.9740096098071,-20.6694831918039,
-9.17034208316701));
#73735=CARTESIAN_POINT('Ctrl Pts',(-19.9120736714761,-20.7125431584589,
-9.16608185049325));
#73736=CARTESIAN_POINT('Ctrl Pts',(-19.8399119400585,-20.757197449934,-9.16105241312598));
#73737=CARTESIAN_POINT('Ctrl Pts',(-19.8318090901944,-20.7621365269822,
-9.16048676398966));
#73738=CARTESIAN_POINT('Ctrl Pts',(-19.819747292292,-20.7693779982016,-9.15964298569349));
#73739=CARTESIAN_POINT('Ctrl Pts',(-19.8158135092527,-20.7717223693083,
-9.15936752405193));
#73740=CARTESIAN_POINT('Ctrl Pts',(-19.8087980895348,-20.7758724801802,
-9.1588757258892));
#73741=CARTESIAN_POINT('Ctrl Pts',(-19.805719459314,-20.777683202947,-9.15865971786735));
#73742=CARTESIAN_POINT('Ctrl Pts',(-19.7990873449481,-20.7815613815112,
-9.15819396370905));
#73743=CARTESIAN_POINT('Ctrl Pts',(-19.7955324686047,-20.7836262496808,
-9.15794406161423));
#73744=CARTESIAN_POINT('Ctrl Pts',(-19.7856954071848,-20.78930190073,-9.15725188192812));
#73745=CARTESIAN_POINT('Ctrl Pts',(-19.7794007327574,-20.7928907649215,
-9.15680823068811));
#73746=CARTESIAN_POINT('Ctrl Pts',(-19.7446837696283,-20.8124489151308,
-9.15435789212968));
#73747=CARTESIAN_POINT('Ctrl Pts',(-19.7159155890041,-20.8277913938971,
-9.15231471694279));
#73748=CARTESIAN_POINT('Ctrl Pts',(-19.5415625181828,-20.9156665823046,
-9.13990730862574));
#73749=CARTESIAN_POINT('Ctrl Pts',(-19.3883704470067,-20.9718868591919,
-9.12895421470627));
#73750=CARTESIAN_POINT('Ctrl Pts',(-19.1167158273123,-21.0373915602516,
-9.1107014580258));
#73751=CARTESIAN_POINT('Ctrl Pts',(-19.0010932404552,-21.0553303039268,
-9.10326192697726));
#73752=CARTESIAN_POINT('Ctrl Pts',(-18.8703108117004,-21.0646553293364,
-9.09525608838018));
#73753=CARTESIAN_POINT('Ctrl Pts',(-18.8560477217907,-21.0655272762096,
-9.09438812835139));
#73754=CARTESIAN_POINT('Ctrl Pts',(-18.8333331427384,-21.0666851785229,
-9.09301384026215));
#73755=CARTESIAN_POINT('Ctrl Pts',(-18.8248870723574,-21.067065015745,-9.09250458426938));
#73756=CARTESIAN_POINT('Ctrl Pts',(-18.8099870479676,-21.0676456833767,
-9.09160921151416));
#73757=CARTESIAN_POINT('Ctrl Pts',(-18.803534068515,-21.067867600725,-9.09122243864934));
#73758=CARTESIAN_POINT('Ctrl Pts',(-18.7901850938562,-21.0682655359961,
-9.09042436892466));
#73759=CARTESIAN_POINT('Ctrl Pts',(-18.7832890437421,-21.0684373781228,
-9.09001320745828));
#73760=CARTESIAN_POINT('Ctrl Pts',(-18.7655855916307,-21.068791954899,-9.08896048784528));
#73761=CARTESIAN_POINT('Ctrl Pts',(-18.7547773227515,-21.0689256338714,
-9.08832047105696));
#73762=CARTESIAN_POINT('Ctrl Pts',(-18.7096624019784,-21.0691380695378,
-9.0856597279634));
#73763=CARTESIAN_POINT('Ctrl Pts',(-18.6753562818806,-21.0684656942907,
-9.08366253215187));
#73764=CARTESIAN_POINT('Ctrl Pts',(-18.5860256197608,-21.0645409901289,
-9.07851824069386));
#73765=CARTESIAN_POINT('Ctrl Pts',(-18.5310840268167,-21.0599733407905,
-9.07541053833727));
#73766=CARTESIAN_POINT('Ctrl Pts',(-18.3678442175265,-21.0399597833096,
-9.066265877723));
#73767=CARTESIAN_POINT('Ctrl Pts',(-18.260499454246,-21.0182633496938,-9.06037764802157));
#73768=CARTESIAN_POINT('Ctrl Pts',(-18.1111162202479,-20.9758121872233,
-9.0519225662748));
#73769=CARTESIAN_POINT('Ctrl Pts',(-18.0673425814505,-20.9618178069699,
-9.04941031793161));
#73770=CARTESIAN_POINT('Ctrl Pts',(-18.00306649288,-20.9389377932736,-9.04562658902648));
#73771=CARTESIAN_POINT('Ctrl Pts',(-17.982192497875,-20.9311339059033,-9.04438257031487));
#73772=CARTESIAN_POINT('Ctrl Pts',(-17.9135890799748,-20.9042441144118,
-9.04023182440806));
#73773=CARTESIAN_POINT('Ctrl Pts',(-17.8664351868196,-20.8837508983648,
-9.03727821380553));
#73774=CARTESIAN_POINT('Ctrl Pts',(-17.8129725138501,-20.8581635350126,
-9.03376034207724));
#73775=CARTESIAN_POINT('Ctrl Pts',(-17.8058862038966,-20.8547232666823,
-9.03329055270424));
#73776=CARTESIAN_POINT('Ctrl Pts',(-17.7946186247985,-20.8491751518349,
-9.03253770002197));
#73777=CARTESIAN_POINT('Ctrl Pts',(-17.790424785836,-20.8470928048693,-9.03225618189817));
#73778=CARTESIAN_POINT('Ctrl Pts',(-17.7830250350207,-20.8433879893595,
-9.03175709443563));
#73779=CARTESIAN_POINT('Ctrl Pts',(-17.7798163024653,-20.8417712511085,
-9.03153988503455));
#73780=CARTESIAN_POINT('Ctrl Pts',(-17.7730412366998,-20.8383359405492,
-9.03107956131357));
#73781=CARTESIAN_POINT('Ctrl Pts',(-17.7694759969734,-20.8365154476262,
-9.03083633212184));
#73782=CARTESIAN_POINT('Ctrl Pts',(-17.7599055900177,-20.8315943064334,
-9.03018078606027));
#73783=CARTESIAN_POINT('Ctrl Pts',(-17.7539101309969,-20.8284750257231,
-9.02976732134429));
#73784=CARTESIAN_POINT('Ctrl Pts',(-17.7247066666117,-20.813103089231,-9.02774007496838));
#73785=CARTESIAN_POINT('Ctrl Pts',(-17.7017140521055,-20.8004488948402,
-9.02610285112236));
#73786=CARTESIAN_POINT('Ctrl Pts',(-17.6365300270785,-20.7629788185537,
-9.02135508998252));
#73787=CARTESIAN_POINT('Ctrl Pts',(-17.5949575681654,-20.7371236171926,
-9.01819698633989));
#73788=CARTESIAN_POINT('Ctrl Pts',(-17.4740669076194,-20.6559950283415,
-9.0086965865316));
#73789=CARTESIAN_POINT('Ctrl Pts',(-17.3975959971134,-20.5967050176867,
-9.00226746872186));
#73790=CARTESIAN_POINT('Ctrl Pts',(-17.220170089257,-20.4385712648393,-8.98663161768537));
#73791=CARTESIAN_POINT('Ctrl Pts',(-17.1245183702649,-20.3344461504433,
-8.97756396724562));
#73792=CARTESIAN_POINT('Ctrl Pts',(-17.0313564409232,-20.210132703032,-8.96807851641956));
#73793=CARTESIAN_POINT('Ctrl Pts',(-17.0229070111065,-20.1986169366562,
-8.96721096632442));
#73794=CARTESIAN_POINT('Ctrl Pts',(-17.0096435758668,-20.1801511989274,
-8.96583720257601));
#73795=CARTESIAN_POINT('Ctrl Pts',(-17.0047536536433,-20.1732565339541,
-8.96532806446533));
#73796=CARTESIAN_POINT('Ctrl Pts',(-16.9962016494398,-20.1610440760181,
-8.96443282881721));
#73797=CARTESIAN_POINT('Ctrl Pts',(-16.9925223806488,-20.1557385046993,
-8.96404607580978));
#73798=CARTESIAN_POINT('Ctrl Pts',(-16.9849620146775,-20.1447291060193,
-8.96324797986233));
#73799=CARTESIAN_POINT('Ctrl Pts',(-16.9810844076774,-20.1390229662357,
-8.96283677264725));
#73800=CARTESIAN_POINT('Ctrl Pts',(-16.9712013673956,-20.1243254190353,
-8.96178379676295));
#73801=CARTESIAN_POINT('Ctrl Pts',(-16.9652367522292,-20.1153067038098,
-8.9611435709255));
#73802=CARTESIAN_POINT('Ctrl Pts',(-16.9406197447854,-20.0774578275874,
-8.9584807951637));
#73803=CARTESIAN_POINT('Ctrl Pts',(-16.9226004577457,-20.0482207610384,
-8.95648182164581));
#73804=CARTESIAN_POINT('Ctrl Pts',(-16.8775013535254,-19.9708946076262,
-8.95133191531324));
#73805=CARTESIAN_POINT('Ctrl Pts',(-16.8515758316577,-19.9221615039678,
-8.94822048865645));
#73806=CARTESIAN_POINT('Ctrl Pts',(-16.7800131968833,-19.7739453648798,
-8.93906933130394));
#73807=CARTESIAN_POINT('Ctrl Pts',(-16.7401515465627,-19.6718804283087,
-8.93317830736694));
#73808=CARTESIAN_POINT('Ctrl Pts',(-16.6935615489729,-19.5184736083894,
-8.9244492072757));
#73809=CARTESIAN_POINT('Ctrl Pts',(-16.6805284935058,-19.4692386718673,
-8.92166384483347));
#73810=CARTESIAN_POINT('Ctrl Pts',(-16.6658125615088,-19.4042572979707,
-8.91795697512142));
#73811=CARTESIAN_POINT('Ctrl Pts',(-16.6625125134373,-19.38889303031,-8.91707827504095));
#73812=CARTESIAN_POINT('Ctrl Pts',(-16.648882110064,-19.3218034087935,-8.91322623530355));
#73813=CARTESIAN_POINT('Ctrl Pts',(-16.6403167669215,-19.2697431464976,
-8.91019828482176));
#73814=CARTESIAN_POINT('Ctrl Pts',(-16.6326149764804,-19.2087986341417,
-8.90655268787263));
#73815=CARTESIAN_POINT('Ctrl Pts',(-16.6315783128396,-19.2001684892654,
-8.90603410192148));
#73816=CARTESIAN_POINT('Ctrl Pts',(-16.630088263151,-19.1870839188921,-8.90524396788583));
#73817=CARTESIAN_POINT('Ctrl Pts',(-16.6295957989297,-19.1826339156402,
-8.90497456762527));
#73818=CARTESIAN_POINT('Ctrl Pts',(-16.6287367225723,-19.1746392415219,
-8.90448930231885));
#73819=CARTESIAN_POINT('Ctrl Pts',(-16.62836494123,-19.1710951805231,-8.90427373132515));
#73820=CARTESIAN_POINT('Ctrl Pts',(-16.6275760433204,-19.1633873812406,
-8.90380390383939));
#73821=CARTESIAN_POINT('Ctrl Pts',(-16.6271623283961,-19.1592233940286,
-8.9035494644057));
#73822=CARTESIAN_POINT('Ctrl Pts',(-16.6260337076674,-19.1475111210151,
-8.9028320861379));
#73823=CARTESIAN_POINT('Ctrl Pts',(-16.6253470127124,-19.1399602704302,
-8.90236760815954));
#73824=CARTESIAN_POINT('Ctrl Pts',(-16.6214621608634,-19.0945387584654,
-8.89956229864038));
#73825=CARTESIAN_POINT('Ctrl Pts',(-16.619243951302,-19.0565937786277,-8.89717171253788));
#73826=CARTESIAN_POINT('Ctrl Pts',(-16.6152879480915,-18.9309310782332,
-8.8891435145921));
#73827=CARTESIAN_POINT('Ctrl Pts',(-16.6179805379353,-18.8431682047451,
-8.88336091591602));
#73828=CARTESIAN_POINT('Ctrl Pts',(-16.6422708849619,-18.5821605699798,
-8.86604056163588));
#73829=CARTESIAN_POINT('Ctrl Pts',(-16.6798383381421,-18.4111166343265,
-8.85459340835551));
#73830=CARTESIAN_POINT('Ctrl Pts',(-16.745664606849,-18.2248525605343,-8.8424327332812));
#73831=CARTESIAN_POINT('Ctrl Pts',(-16.7537054639037,-18.2032312434783,
-8.84102457385064));
#73832=CARTESIAN_POINT('Ctrl Pts',(-16.7655761001365,-18.1728416630186,
-8.83904954357946));
#73833=CARTESIAN_POINT('Ctrl Pts',(-16.7691141688392,-18.1639619052149,
-8.83847295299369));
#73834=CARTESIAN_POINT('Ctrl Pts',(-16.7749592015262,-18.1495763093885,
-8.83753959559214));
#73835=CARTESIAN_POINT('Ctrl Pts',(-16.7772294957275,-18.1440558038561,
-8.83718159657123));
#73836=CARTESIAN_POINT('Ctrl Pts',(-16.7820294176574,-18.1325231000204,
-8.83643405809275));
#73837=CARTESIAN_POINT('Ctrl Pts',(-16.7845635470042,-18.1265128340607,
-8.83604467598862));
#73838=CARTESIAN_POINT('Ctrl Pts',(-16.7906560126747,-18.1122476858005,
-8.83512091297652));
#73839=CARTESIAN_POINT('Ctrl Pts',(-16.7942392461985,-18.1040035235427,
-8.83458738615579));
#73840=CARTESIAN_POINT('Ctrl Pts',(-16.8064770433044,-18.0763307636169,
-8.83279745971867));
#73841=CARTESIAN_POINT('Ctrl Pts',(-16.8153720280101,-18.057009433696,-8.83154929582967));
#73842=CARTESIAN_POINT('Ctrl Pts',(-16.8912564925192,-17.8985090925484,
-8.82131530963366));
#73843=CARTESIAN_POINT('Ctrl Pts',(-16.9730030260183,-17.7669076653599,
-8.81289798811847));
#73844=CARTESIAN_POINT('Ctrl Pts',(-17.1527697460017,-17.5377487914963,
-8.79708128694917));
#73845=CARTESIAN_POINT('Ctrl Pts',(-17.2474057534722,-17.4385857273095,
-8.78969570626167));
#73846=CARTESIAN_POINT('Ctrl Pts',(-17.3627250874046,-17.3390719013255,
-8.78076352063304));
#73847=CARTESIAN_POINT('Ctrl Pts',(-17.3746370382221,-17.3290199497087,
-8.77984141466584));
#73848=CARTESIAN_POINT('Ctrl Pts',(-17.3911125568151,-17.3154256325307,
-8.77856506099069));
#73849=CARTESIAN_POINT('Ctrl Pts',(-17.3955815749362,-17.3117687775827,
-8.77821875001981));
#73850=CARTESIAN_POINT('Ctrl Pts',(-17.4027117950377,-17.3059828889375,
-8.77766596222476));
#73851=CARTESIAN_POINT('Ctrl Pts',(-17.4053633114003,-17.3038418874666,
-8.77746034097041));
#73852=CARTESIAN_POINT('Ctrl Pts',(-17.410854392957,-17.2994299037098,-8.77703437292913));
#73853=CARTESIAN_POINT('Ctrl Pts',(-17.4136946347415,-17.2971598378449,
-8.77681396092256));
#73854=CARTESIAN_POINT('Ctrl Pts',(-17.4204832512033,-17.2917626315522,
-8.77628697249191));
#73855=CARTESIAN_POINT('Ctrl Pts',(-17.4244369532535,-17.2886422530457,
-8.77597991846356));
#73856=CARTESIAN_POINT('Ctrl Pts',(-17.4378410971752,-17.2781407192771,
-8.77493857470123));
#73857=CARTESIAN_POINT('Ctrl Pts',(-17.447342904198,-17.2708259175234,-8.77419981912154));
#73858=CARTESIAN_POINT('Ctrl Pts',(-17.5586182815263,-17.1866583801352,
-8.76554663027551));
#73859=CARTESIAN_POINT('Ctrl Pts',(-17.6670638480853,-17.119080546469,-8.75711321429331));
#73860=CARTESIAN_POINT('Ctrl Pts',(-17.9283007809298,-16.987367211882,-8.73777944961678));
#73861=CARTESIAN_POINT('Ctrl Pts',(-18.0838982063598,-16.9305350451299,
-8.726984085091));
#73862=CARTESIAN_POINT('Ctrl Pts',(-18.2675084998527,-16.8869014756195,
-8.71536079879259));
#73863=CARTESIAN_POINT('Ctrl Pts',(-18.2905651075062,-16.8818280742839,
-8.71391917588496));
#73864=CARTESIAN_POINT('Ctrl Pts',(-18.3231584781354,-16.875225739675,-8.71190572463697));
#73865=CARTESIAN_POINT('Ctrl Pts',(-18.3326275547124,-16.8733749136939,
-8.71132365980457));
#73866=CARTESIAN_POINT('Ctrl Pts',(-18.3479910214154,-16.8704808688451,
-8.71038385170174));
#73867=CARTESIAN_POINT('Ctrl Pts',(-18.3538776840689,-16.8693978173961,
-8.71002484244759));
#73868=CARTESIAN_POINT('Ctrl Pts',(-18.3661754091762,-16.8671891122747,
-8.70927708055056));
#73869=CARTESIAN_POINT('Ctrl Pts',(-18.3725872370408,-16.8660680300109,
-8.70888847699872));
#73870=CARTESIAN_POINT('Ctrl Pts',(-18.3877913035338,-16.863481868435,-8.7079699506935));
#73871=CARTESIAN_POINT('Ctrl Pts',(-18.3965878700561,-16.8620427024331,
-8.70744085588123));
#73872=CARTESIAN_POINT('Ctrl Pts',(-18.425380879748,-16.8575185361226,-8.70571644959349));
#73873=CARTESIAN_POINT('Ctrl Pts',(-18.4454128747005,-16.854664576923,-8.70452844975692));
#73874=CARTESIAN_POINT('Ctrl Pts',(-18.4930786997523,-16.8485694952434,
-8.70172743216196));
#73875=CARTESIAN_POINT('Ctrl Pts',(-18.5207418760511,-16.8455850280324,
-8.70012237341828));
#73876=CARTESIAN_POINT('Ctrl Pts',(-18.7171642363187,-16.8283032017231,
-8.68885173277689));
#73877=CARTESIAN_POINT('Ctrl Pts',(-18.8870379552048,-16.8337569676413,
-8.67982457081734));
#73878=CARTESIAN_POINT('Ctrl Pts',(-19.157209368514,-16.8751299374255,-8.66488771521993));
#73879=CARTESIAN_POINT('Ctrl Pts',(-19.2586536417649,-16.89841091196,-8.65912337343936));
#73880=CARTESIAN_POINT('Ctrl Pts',(-19.367220372226,-16.9318973257694,-8.65239234173926));
#73881=CARTESIAN_POINT('Ctrl Pts',(-19.3764579481692,-16.934816163307,-8.65181502958846));
#73882=CARTESIAN_POINT('Ctrl Pts',(-19.3900688512375,-16.939219835748,-8.65095716118084));
#73883=CARTESIAN_POINT('Ctrl Pts',(-19.3944580255002,-16.9406557920643,
-8.65067940341618));
#73884=CARTESIAN_POINT('Ctrl Pts',(-19.4022370968834,-16.9432289908719,
-8.65018508305617));
#73885=CARTESIAN_POINT('Ctrl Pts',(-19.4056288482904,-16.9443604719225,
-8.64996886196975));
#73886=CARTESIAN_POINT('Ctrl Pts',(-19.412890511726,-16.9468034089712,-8.64950443495672));
#73887=CARTESIAN_POINT('Ctrl Pts',(-19.4167594398678,-16.9481174579821,
-8.64925608244532));
#73888=CARTESIAN_POINT('Ctrl Pts',(-19.4273710689916,-16.9517559079326,
-8.64857244880002));
#73889=CARTESIAN_POINT('Ctrl Pts',(-19.4341057934348,-16.9541031703748,
-8.64813584824327));
#73890=CARTESIAN_POINT('Ctrl Pts',(-19.4695225241903,-16.9666480743012,
-8.64582592458136));
#73891=CARTESIAN_POINT('Ctrl Pts',(-19.4979923901222,-16.9774288928147,
-8.64392089889335));
#73892=CARTESIAN_POINT('Ctrl Pts',(-19.6765790273641,-17.0494953909534,
-8.63170746959015));
#73893=CARTESIAN_POINT('Ctrl Pts',(-19.8194665893621,-17.1272423355203,
-8.62079147907306));
#73894=CARTESIAN_POINT('Ctrl Pts',(-20.0499070855908,-17.289356180983,-8.60236922010302));
#73895=CARTESIAN_POINT('Ctrl Pts',(-20.1417396026641,-17.3663539203935,
-8.59474160483249));
#73896=CARTESIAN_POINT('Ctrl Pts',(-20.2377288060895,-17.461786767082,-8.58647641459699));
#73897=CARTESIAN_POINT('Ctrl Pts',(-20.2487462312271,-17.472986924435,-8.58552260796206));
#73898=CARTESIAN_POINT('Ctrl Pts',(-20.2652268079633,-17.4901181844641,
-8.58408768011977));
#73899=CARTESIAN_POINT('Ctrl Pts',(-20.2707822500935,-17.4959593760397,
-8.58360254227211));
#73900=CARTESIAN_POINT('Ctrl Pts',(-20.2806777377058,-17.506483573896,-8.58273575284525));
#73901=CARTESIAN_POINT('Ctrl Pts',(-20.2850301942227,-17.5111547270978,
-8.58235356858448));
#73902=CARTESIAN_POINT('Ctrl Pts',(-20.2942209522223,-17.5211083577414,
-8.58154450948689));
#73903=CARTESIAN_POINT('Ctrl Pts',(-20.2990537171269,-17.5263958557571,
-8.58111787344361));
#73904=CARTESIAN_POINT('Ctrl Pts',(-20.3088371014887,-17.5372095039485,
-8.58025166298613));
#73905=CARTESIAN_POINT('Ctrl Pts',(-20.3137856966663,-17.5427373563898,
-8.57981217681295));
#73906=CARTESIAN_POINT('Ctrl Pts',(-20.3355743469661,-17.567335468225,-8.57787098251012));
#73907=CARTESIAN_POINT('Ctrl Pts',(-20.3520993491615,-17.5866828819851,
-8.57638238057284));
#73908=CARTESIAN_POINT('Ctrl Pts',(-20.4222713890859,-17.6719041523003,
-8.56998126027263));
#73909=CARTESIAN_POINT('Ctrl Pts',(-20.4722775168634,-17.7406787622017,
-8.5652140362318));
#73910=CARTESIAN_POINT('Ctrl Pts',(-20.555189851896,-17.8704624298392,-8.55672638969621));
#73911=CARTESIAN_POINT('Ctrl Pts',(-20.5894925682938,-17.9304307782471,
-8.5529812588757));
#73912=CARTESIAN_POINT('Ctrl Pts',(-20.6801422890736,-18.1085898558519,
-8.54212539585322));
#73913=CARTESIAN_POINT('Ctrl Pts',(-20.728532700323,-18.2304457785093,-8.53503486061591));
#73914=CARTESIAN_POINT('Ctrl Pts',(-20.7697993273687,-18.3710882887299,
-8.52644202941237));
#73915=CARTESIAN_POINT('Ctrl Pts',(-20.7740668394217,-18.3862575008341,
-8.52550993438047));
#73916=CARTESIAN_POINT('Ctrl Pts',(-20.7796729212571,-18.4070734489269,
-8.52422185934865));
#73917=CARTESIAN_POINT('Ctrl Pts',(-20.781158322265,-18.4126805690425,-8.52387400541102));
#73918=CARTESIAN_POINT('Ctrl Pts',(-20.7834811070905,-18.4215965298827,
-8.52331936339071));
#73919=CARTESIAN_POINT('Ctrl Pts',(-20.7843335775881,-18.4249014611416,
-8.52311344120053));
#73920=CARTESIAN_POINT('Ctrl Pts',(-20.7860768719575,-18.4317282358,-8.52268737389335));
#73921=CARTESIAN_POINT('Ctrl Pts',(-20.7869666213985,-18.4352503046051,
-8.52246716590368));
#73922=CARTESIAN_POINT('Ctrl Pts',(-20.789063834877,-18.4436430230038,-8.52194152615588));
#73923=CARTESIAN_POINT('Ctrl Pts',(-20.7902630508741,-18.4485156944848,
-8.52163562321655));
#73924=CARTESIAN_POINT('Ctrl Pts',(-20.7927674030141,-18.4588496081269,
-8.52098539973067));
#73925=CARTESIAN_POINT('Ctrl Pts',(-20.7940681557944,-18.4643118613354,
-8.52064084111419));
#73926=CARTESIAN_POINT('Ctrl Pts',(-20.7975804743657,-18.4793259527679,
-8.51969149861464));
#73927=CARTESIAN_POINT('Ctrl Pts',(-20.799747407623,-18.4888879520619,-8.51908439180955));
#73928=CARTESIAN_POINT('Ctrl Pts',(-20.8343835371362,-18.6468077555266,
-8.50902050963056));
#73929=CARTESIAN_POINT('Ctrl Pts',(-20.850858530288,-18.7982035834032,-8.4988643478769));
#73930=CARTESIAN_POINT('Ctrl Pts',(-20.8509990928545,-18.950040190495,-8.48885786576293));
#73931=CARTESIAN_POINT('Ctrl Pts',(-20.8509991049198,-18.9500532671891,
-8.48905627902251));
#73932=CARTESIAN_POINT('Ctrl Pts',(-20.8510652694519,-19.0220047205605,
-8.48473008583432));
#73933=CARTESIAN_POINT('Ctrl Pts',(-20.8474590099796,-19.0940510985681,
-8.48040389264612));
#73934=CARTESIAN_POINT('Ctrl Pts',(-20.8401779985048,-19.1657831579297,
-8.47607769945793));
#73935=CARTESIAN_POINT('Ctrl Pts',(-20.8329019842481,-19.2374659850183,
-8.47175447549056));
#73936=CARTESIAN_POINT('Ctrl Pts',(-20.8219562717605,-19.3088344307463,
-8.46743125152319));
#73937=CARTESIAN_POINT('Ctrl Pts',(-20.8073905458149,-19.3794817475932,
-8.46310802755582));
#73938=CARTESIAN_POINT('Ctrl Pts',(-20.7928276075145,-19.4501155436823,
-8.45878563098384));
#73939=CARTESIAN_POINT('Ctrl Pts',(-20.774646124242,-19.5200279993613,-8.45446323441186));
#73940=CARTESIAN_POINT('Ctrl Pts',(-20.7529470567775,-19.5888216248916,
-8.45014083783989));
#73941=CARTESIAN_POINT('Ctrl Pts',(-20.7434887927382,-19.6188076266194,
-8.44825677677934));
#73942=CARTESIAN_POINT('Ctrl Pts',(-20.733362857865,-19.6485812163244,-8.4463727157188));
#73943=CARTESIAN_POINT('Ctrl Pts',(-20.7225805821191,-19.6781103693095,
-8.44448865465826));
#73944=CARTESIAN_POINT('Origin',(-18.734,-18.952,0.));
#73945=CARTESIAN_POINT('',(-20.7249098202513,-19.6789408942641,-7.64456002557215));
#73946=CARTESIAN_POINT('',(-20.7225805730004,-19.6781103942827,-7.86510594064262));
#73947=CARTESIAN_POINT('',(-20.7225805821191,-19.6781103693095,0.));
#73948=CARTESIAN_POINT('Ctrl Pts',(-20.7225805730004,-19.6781103942827,
-7.86510594064261));
#73949=CARTESIAN_POINT('Ctrl Pts',(-20.7375769517348,-19.6370401828501,
-7.86752231323783));
#73950=CARTESIAN_POINT('Ctrl Pts',(-20.7513004020704,-19.5955070040366,
-7.86996747030577));
#73951=CARTESIAN_POINT('Ctrl Pts',(-20.774507262156,-19.5172058397638,-7.87462975166453));
#73952=CARTESIAN_POINT('Ctrl Pts',(-20.7843049850557,-19.4805608708391,
-7.87683270548543));
#73953=CARTESIAN_POINT('Ctrl Pts',(-20.7948724739946,-19.4363047255142,
-7.8795398168314));
#73954=CARTESIAN_POINT('Ctrl Pts',(-20.7965927808939,-19.4289249809921,
-7.87999277135078));
#73955=CARTESIAN_POINT('Ctrl Pts',(-20.799201287806,-19.4174569185875,-7.88069927329126));
#73956=CARTESIAN_POINT('Ctrl Pts',(-20.8001170706691,-19.4133748495651,
-7.88095126622773));
#73957=CARTESIAN_POINT('Ctrl Pts',(-20.801790523728,-19.405810588006,-7.88141921480146));
#73958=CARTESIAN_POINT('Ctrl Pts',(-20.8025515035319,-19.4023291867746,
-7.88163497809511));
#73959=CARTESIAN_POINT('Ctrl Pts',(-20.8042489771272,-19.3944683368746,
-7.88212304445236));
#73960=CARTESIAN_POINT('Ctrl Pts',(-20.8051803610547,-19.3900878537022,
-7.88239563399139));
#73961=CARTESIAN_POINT('Ctrl Pts',(-20.8078797660236,-19.3771909821251,
-7.88319991817301));
#73962=CARTESIAN_POINT('Ctrl Pts',(-20.8096091831936,-19.3686667348037,
-7.88373373668598));
#73963=CARTESIAN_POINT('Ctrl Pts',(-20.8214936637338,-19.3081778481938,
-7.88753632508516));
#73964=CARTESIAN_POINT('Ctrl Pts',(-20.8297477276156,-19.255863294928,-7.89090073532048));
#73965=CARTESIAN_POINT('Ctrl Pts',(-20.8378088430684,-19.1884349094632,
-7.89528843836827));
#73966=CARTESIAN_POINT('Ctrl Pts',(-20.8394281650497,-19.1735521182162,
-7.89626010311883));
#73967=CARTESIAN_POINT('Ctrl Pts',(-20.8475637431883,-19.090607720525,-7.90168919291301));
#73968=CARTESIAN_POINT('Ctrl Pts',(-20.8509374103621,-19.0222802059237,
-7.90621179080917));
#73969=CARTESIAN_POINT('Ctrl Pts',(-20.8511442882594,-18.7931414079384,
-7.92135272976385));
#73970=CARTESIAN_POINT('Ctrl Pts',(-20.8329752262217,-18.6328491654654,
-7.9318507301475));
#73971=CARTESIAN_POINT('Ctrl Pts',(-20.7914795954939,-18.4529688454933,
-7.94322223271909));
#73972=CARTESIAN_POINT('Ctrl Pts',(-20.7857446846322,-18.4298906240303,
-7.94467451223104));
#73973=CARTESIAN_POINT('Ctrl Pts',(-20.7771304021409,-18.3975626272888,
-7.94670021104836));
#73974=CARTESIAN_POINT('Ctrl Pts',(-20.7745746984409,-18.3882291730159,
-7.94728403381575));
#73975=CARTESIAN_POINT('Ctrl Pts',(-20.7703333350992,-18.3731464462916,
-7.9482259155125));
#73976=CARTESIAN_POINT('Ctrl Pts',(-20.7686871312369,-18.3673863092582,
-7.94858525133491));
#73977=CARTESIAN_POINT('Ctrl Pts',(-20.7652024825499,-18.3553863998426,
-7.94933309843104));
#73978=CARTESIAN_POINT('Ctrl Pts',(-20.7633596821685,-18.3491479494473,
-7.94972146322238));
#73979=CARTESIAN_POINT('Ctrl Pts',(-20.7589304691935,-18.3344041590598,
-7.9506383625105));
#73980=CARTESIAN_POINT('Ctrl Pts',(-20.7563191658415,-18.3259063784405,
-7.95116607717529));
#73981=CARTESIAN_POINT('Ctrl Pts',(-20.7474528216397,-18.2976875603047,
-7.9529161589399));
#73982=CARTESIAN_POINT('Ctrl Pts',(-20.7409621037977,-18.2780414015876,
-7.95413078979751));
#73983=CARTESIAN_POINT('Ctrl Pts',(-20.7048338630199,-18.173841818229,-7.96055734970913));
#73984=CARTESIAN_POINT('Ctrl Pts',(-20.6701375509487,-18.0911339775254,
-7.96559785907302));
#73985=CARTESIAN_POINT('Ctrl Pts',(-20.5703572778889,-17.8900856685431,
-7.97797948641753));
#73986=CARTESIAN_POINT('Ctrl Pts',(-20.4990150235356,-17.7753139913978,
-7.98515792929512));
#73987=CARTESIAN_POINT('Ctrl Pts',(-20.3708542712837,-17.6072887135831,
-7.99685019316134));
#73988=CARTESIAN_POINT('Ctrl Pts',(-20.3212057823279,-17.5490333233624,
-8.00116977687783));
#73989=CARTESIAN_POINT('Ctrl Pts',(-20.2619779474793,-17.4867141577325,
-8.00626515299267));
#73990=CARTESIAN_POINT('Ctrl Pts',(-20.2553888188801,-17.4798738974814,
-8.00683128284337));
#73991=CARTESIAN_POINT('Ctrl Pts',(-20.2455537549553,-17.4698005425575,
-8.00767564233198));
#73992=CARTESIAN_POINT('Ctrl Pts',(-20.2423428880607,-17.4665331653336,
-8.00795119911209));
#73993=CARTESIAN_POINT('Ctrl Pts',(-20.2366096484543,-17.4607367761918,
-8.00844310129746));
#73994=CARTESIAN_POINT('Ctrl Pts',(-20.2340914555426,-17.458203700939,-8.00865911766408));
#73995=CARTESIAN_POINT('Ctrl Pts',(-20.2286618090162,-17.4527695410695,
-8.00912481463519));
#73996=CARTESIAN_POINT('Ctrl Pts',(-20.2257483568813,-17.4498706009819,
-8.00937465080113));
#73997=CARTESIAN_POINT('Ctrl Pts',(-20.2176786552267,-17.441887725482,-8.0100664663301));
#73998=CARTESIAN_POINT('Ctrl Pts',(-20.2125047915287,-17.4368217888439,
-8.01050981701182));
#73999=CARTESIAN_POINT('Ctrl Pts',(-20.1839451825361,-17.4091434990124,
-8.01295545762008));
#74000=CARTESIAN_POINT('Ctrl Pts',(-20.1600679703785,-17.3870472563484,
-8.01499407407326));
#74001=CARTESIAN_POINT('Ctrl Pts',(-20.0137581027677,-17.2577797178948,
-8.02739994363735));
#74002=CARTESIAN_POINT('Ctrl Pts',(-19.8798138969812,-17.1644671727211,
-8.03835720679495));
#74003=CARTESIAN_POINT('Ctrl Pts',(-19.6336216902987,-17.0321003208917,
-8.05661529396626));
#74004=CARTESIAN_POINT('Ctrl Pts',(-19.5263234516695,-16.9853873493609,
-8.06405613720958));
#74005=CARTESIAN_POINT('Ctrl Pts',(-19.4021738928779,-16.9431603263832,
-8.072063197309));
#74006=CARTESIAN_POINT('Ctrl Pts',(-19.3885991738552,-16.9386959686313,
-8.07293117340852));
#74007=CARTESIAN_POINT('Ctrl Pts',(-19.3669223584555,-16.93180947261,-8.0743054820485));
#74008=CARTESIAN_POINT('Ctrl Pts',(-19.3588493379269,-16.9292978996104,
-8.07481474265757));
#74009=CARTESIAN_POINT('Ctrl Pts',(-19.3445847677139,-16.9249536436865,
-8.07571012077674));
#74010=CARTESIAN_POINT('Ctrl Pts',(-19.3383995141151,-16.9231008112825,
-8.07609689441409));
#74011=CARTESIAN_POINT('Ctrl Pts',(-19.3255888935864,-16.9193270887387,
-8.07689496309716));
#74012=CARTESIAN_POINT('Ctrl Pts',(-19.3189624135805,-16.9174102232587,
-8.07730612276231));
#74013=CARTESIAN_POINT('Ctrl Pts',(-19.3019291090047,-16.9125730329247,
-8.07835883230764));
#74014=CARTESIAN_POINT('Ctrl Pts',(-19.2915089929618,-16.9096999348249,
-8.0789988408874));
#74015=CARTESIAN_POINT('Ctrl Pts',(-19.2479272925843,-16.8980417291663,
-8.08165950425955));
#74016=CARTESIAN_POINT('Ctrl Pts',(-19.2145755511478,-16.88998322591,-8.08365663035751));
#74017=CARTESIAN_POINT('Ctrl Pts',(-19.1271789034915,-16.8711021398066,
-8.08880070168368));
#74018=CARTESIAN_POINT('Ctrl Pts',(-19.0728803418643,-16.8615726958346,
-8.09190825804238));
#74019=CARTESIAN_POINT('Ctrl Pts',(-18.9099125905281,-16.8394895540177,
-8.10105266393844));
#74020=CARTESIAN_POINT('Ctrl Pts',(-18.8005788010384,-16.8332235203395,
-8.10694078407108));
#74021=CARTESIAN_POINT('Ctrl Pts',(-18.6455318676336,-16.836355073568,-8.11538391013854));
#74022=CARTESIAN_POINT('Ctrl Pts',(-18.5998561999474,-16.8387595335954,
-8.11788423302371));
#74023=CARTESIAN_POINT('Ctrl Pts',(-18.5315832706288,-16.8445759646648,
-8.12168371900076));
#74024=CARTESIAN_POINT('Ctrl Pts',(-18.5089041621511,-16.846877578628,-8.12295622388119));
#74025=CARTESIAN_POINT('Ctrl Pts',(-18.4852295120212,-16.8496671680906,
-8.12429937232324));
#74026=CARTESIAN_POINT('Ctrl Pts',(-18.4841918842235,-16.8497902109685,
-8.12435827048077));
#74027=CARTESIAN_POINT('Ctrl Pts',(-18.4647180185559,-16.8521140619218,
-8.12546421814634));
#74028=CARTESIAN_POINT('Ctrl Pts',(-18.4463119143648,-16.8545564925169,
-8.12651904434817));
#74029=CARTESIAN_POINT('Ctrl Pts',(-18.3950051768962,-16.8620527702356,
-8.12949177821453));
#74030=CARTESIAN_POINT('Ctrl Pts',(-18.3621896439015,-16.8676406991701,
-8.1314305004841));
#74031=CARTESIAN_POINT('Ctrl Pts',(-18.322734327069,-16.8753205932203,-8.1338215071503));
#74032=CARTESIAN_POINT('Ctrl Pts',(-18.3159536859165,-16.8766749438753,
-8.13423457153015));
#74033=CARTESIAN_POINT('Ctrl Pts',(-18.3048275232537,-16.8789539987548,
-8.13491608070141));
#74034=CARTESIAN_POINT('Ctrl Pts',(-18.3004780020547,-16.8798592194194,
-8.13518343811733));
#74035=CARTESIAN_POINT('Ctrl Pts',(-18.2926468243224,-16.8815147768423,
-8.13566654829429));
#74036=CARTESIAN_POINT('Ctrl Pts',(-18.2891641881197,-16.8822602131825,
-8.13588201867212));
#74037=CARTESIAN_POINT('Ctrl Pts',(-18.2815669855834,-16.8839064073329,
-8.13635343036611));
#74038=CARTESIAN_POINT('Ctrl Pts',(-18.2774532718618,-16.8848106460998,
-8.13660956455088));
#74039=CARTESIAN_POINT('Ctrl Pts',(-18.2658181950799,-16.8874045859091,
-8.13733643035061));
#74040=CARTESIAN_POINT('Ctrl Pts',(-18.2583034150761,-16.8891230814121,
-8.13780876561804));
#74041=CARTESIAN_POINT('Ctrl Pts',(-18.2115398945837,-16.900086169211,-8.14076524566598));
#74042=CARTESIAN_POINT('Ctrl Pts',(-18.1725552912503,-16.9104088851109,
-8.14330544084794));
#74043=CARTESIAN_POINT('Ctrl Pts',(-17.9653010190008,-16.971672398734,-8.1571325318623));
#74044=CARTESIAN_POINT('Ctrl Pts',(-17.8035730229403,-17.0423123962943,
-8.16900644133708));
#74045=CARTESIAN_POINT('Ctrl Pts',(-17.5700156459866,-17.1811185658956,
-8.18659640531032));
#74046=CARTESIAN_POINT('Ctrl Pts',(-17.4910131495683,-17.2356466705537,
-8.19265270697207));
#74047=CARTESIAN_POINT('Ctrl Pts',(-17.4051166463315,-17.3039859247083,
-8.19935130705287));
#74048=CARTESIAN_POINT('Ctrl Pts',(-17.3943481380458,-17.3127275201632,
-8.2001934366143));
#74049=CARTESIAN_POINT('Ctrl Pts',(-17.3772490422362,-17.3268891535833,
-8.20153464069264));
#74050=CARTESIAN_POINT('Ctrl Pts',(-17.370863337019,-17.3322417261605,-8.20203642783339));
#74051=CARTESIAN_POINT('Ctrl Pts',(-17.3596004320728,-17.3417962035236,
-8.20292314923341));
#74052=CARTESIAN_POINT('Ctrl Pts',(-17.3547105149916,-17.3459828903557,
-8.20330869966901));
#74053=CARTESIAN_POINT('Ctrl Pts',(-17.3445808641742,-17.354736160995,-8.2041086115322));
#74054=CARTESIAN_POINT('Ctrl Pts',(-17.3393443636244,-17.3593063809733,
-8.20452281594534));
#74055=CARTESIAN_POINT('Ctrl Pts',(-17.325844191368,-17.3712064555667,-8.20559253814179));
#74056=CARTESIAN_POINT('Ctrl Pts',(-17.3176151432258,-17.3785754050474,
-8.20624641573205));
#74057=CARTESIAN_POINT('Ctrl Pts',(-17.2824963105024,-17.410522413642,-8.20904535830756));
#74058=CARTESIAN_POINT('Ctrl Pts',(-17.256184752552,-17.4357287715275,-8.2111636585819));
#74059=CARTESIAN_POINT('Ctrl Pts',(-17.1883711243933,-17.5041369617202,
-8.21669533302375));
#74060=CARTESIAN_POINT('Ctrl Pts',(-17.1480286396272,-17.5484432187357,
-8.22006106370756));
#74061=CARTESIAN_POINT('Ctrl Pts',(-17.0021949425094,-17.7229352452395,
-8.23265905147324));
#74062=CARTESIAN_POINT('Ctrl Pts',(-16.9104175366594,-17.8637498711217,
-8.2414764740787));
#74063=CARTESIAN_POINT('Ctrl Pts',(-16.8122471860583,-18.0623502935211,
-8.25392823211294));
#74064=CARTESIAN_POINT('Ctrl Pts',(-16.7901623422886,-18.1116997069089,
-8.25702817247595));
#74065=CARTESIAN_POINT('Ctrl Pts',(-16.7667270226798,-18.1699497858908,
-8.26075397809295));
#74066=CARTESIAN_POINT('Ctrl Pts',(-16.7635127260228,-18.1780843703571,
-8.26127576974325));
#74067=CARTESIAN_POINT('Ctrl Pts',(-16.7587252588649,-18.1904234460761,
-8.26206983659402));
#74068=CARTESIAN_POINT('Ctrl Pts',(-16.7571148562181,-18.1946135214474,
-8.26233993182966));
#74069=CARTESIAN_POINT('Ctrl Pts',(-16.7542496742715,-18.2021397780864,
-8.26282593603129));
#74070=CARTESIAN_POINT('Ctrl Pts',(-16.7529899839128,-18.2054740322665,
-8.26304154698378));
#74071=CARTESIAN_POINT('Ctrl Pts',(-16.7502728584379,-18.2127212550191,
-8.2635108614417));
#74072=CARTESIAN_POINT('Ctrl Pts',(-16.7488185970028,-18.2166353071776,
-8.26376474461393));
#74073=CARTESIAN_POINT('Ctrl Pts',(-16.7447705687403,-18.2276298384392,
-8.26447901828793));
#74074=CARTESIAN_POINT('Ctrl Pts',(-16.7422030695044,-18.2347198281789,
-8.26494092708758));
#74075=CARTESIAN_POINT('Ctrl Pts',(-16.7271661854344,-18.2769465781668,
-8.26769903644834));
#74076=CARTESIAN_POINT('Ctrl Pts',(-16.7155897347785,-18.3123917691351,
-8.27004310493703));
#74077=CARTESIAN_POINT('Ctrl Pts',(-16.680740099376,-18.4294872443724,-8.27783956209834));
#74078=CARTESIAN_POINT('Ctrl Pts',(-16.6614419056787,-18.5122308727529,
-8.28342858341367));
#74079=CARTESIAN_POINT('Ctrl Pts',(-16.6171404602724,-18.7718509713058,
-8.30082694090861));
#74080=CARTESIAN_POINT('Ctrl Pts',(-16.6094832357551,-18.9509273227642,
-8.31255834900709));
#74081=CARTESIAN_POINT('Ctrl Pts',(-16.6263017938675,-19.1515369502787,
-8.32494667262787));
#74082=CARTESIAN_POINT('Ctrl Pts',(-16.628568198236,-19.1741794639391,-8.32633548483591));
#74083=CARTESIAN_POINT('Ctrl Pts',(-16.6322985450934,-19.2062250553771,
-8.32828832310606));
#74084=CARTESIAN_POINT('Ctrl Pts',(-16.6334614295865,-19.2156609625164,
-8.32886177544001));
#74085=CARTESIAN_POINT('Ctrl Pts',(-16.6354566483555,-19.2309987808936,
-8.32979143955576));
#74086=CARTESIAN_POINT('Ctrl Pts',(-16.6362504017109,-19.2369054974522,
-8.330148864309));
#74087=CARTESIAN_POINT('Ctrl Pts',(-16.6379662154926,-19.249277690343,-8.33089630464623));
#74088=CARTESIAN_POINT('Ctrl Pts',(-16.6388932735334,-19.2557424190993,
-8.33128615804059));
#74089=CARTESIAN_POINT('Ctrl Pts',(-16.641173991873,-19.2711393323343,-8.33221304448785));
#74090=CARTESIAN_POINT('Ctrl Pts',(-16.6425549484176,-19.2800673921619,
-8.33274920782139));
#74091=CARTESIAN_POINT('Ctrl Pts',(-16.647421065704,-19.3102472975736,-8.33455742314247));
#74092=CARTESIAN_POINT('Ctrl Pts',(-16.6511734077091,-19.3314551515858,
-8.33582100452812));
#74093=CARTESIAN_POINT('Ctrl Pts',(-16.6894830919419,-19.5302464016374,
-8.34760783215506));
#74094=CARTESIAN_POINT('Ctrl Pts',(-16.7463443575211,-19.7027663999737,
-8.35731961999596));
#74095=CARTESIAN_POINT('Ctrl Pts',(-16.8344242330958,-19.8867908148481,
-8.368426120785));
#74096=CARTESIAN_POINT('Ctrl Pts',(-16.844730935649,-19.9074498114198,-8.36968569531807));
#74097=CARTESIAN_POINT('Ctrl Pts',(-16.8994260274842,-20.0127350664337,
-8.37618922527099));
#74098=CARTESIAN_POINT('Ctrl Pts',(-16.9491644025574,-20.0944437469731,
-8.3815173085108));
#74099=CARTESIAN_POINT('Ctrl Pts',(-17.0098276787814,-20.1804187650058,
-8.38775119259468));
#74100=CARTESIAN_POINT('Ctrl Pts',(-17.0154671465867,-20.1882959512832,
-8.38832850850654));
#74101=CARTESIAN_POINT('Ctrl Pts',(-17.0238743864598,-20.1998704713225,
-8.38918638145135));
#74102=CARTESIAN_POINT('Ctrl Pts',(-17.0266006026634,-20.2035980282553,
-8.3894641399494));
#74103=CARTESIAN_POINT('Ctrl Pts',(-17.0314591743147,-20.2101957405938,
-8.38995846111537));
#74104=CARTESIAN_POINT('Ctrl Pts',(-17.0335866272514,-20.2130694454873,
-8.39017468227016));
#74105=CARTESIAN_POINT('Ctrl Pts',(-17.0381609035332,-20.2192156305914,
-8.39063910886491));
#74106=CARTESIAN_POINT('Ctrl Pts',(-17.0406098869413,-20.2224863713803,
-8.39088746088674));
#74107=CARTESIAN_POINT('Ctrl Pts',(-17.0473595113515,-20.2314466494183,
-8.39157109184889));
#74108=CARTESIAN_POINT('Ctrl Pts',(-17.0516794132692,-20.2371215144025,
-8.39200769019514));
#74109=CARTESIAN_POINT('Ctrl Pts',(-17.0749154365423,-20.2673277237891,
-8.39435060087743));
#74110=CARTESIAN_POINT('Ctrl Pts',(-17.0943385641695,-20.2914621126119,
-8.3962898044529));
#74111=CARTESIAN_POINT('Ctrl Pts',(-17.2195873812324,-20.4402836910671,
-8.40863151368927));
#74112=CARTESIAN_POINT('Ctrl Pts',(-17.3390319459713,-20.5527803351579,
-8.41964613513472));
#74113=CARTESIAN_POINT('Ctrl Pts',(-17.5646709594519,-20.7206760457512,
-8.4380232878025));
#74114=CARTESIAN_POINT('Ctrl Pts',(-17.6648165734466,-20.7829560725207,
-8.44552423348077));
#74115=CARTESIAN_POINT('Ctrl Pts',(-17.782369035971,-20.843108684175,-8.45358726558593));
#74116=CARTESIAN_POINT('Ctrl Pts',(-17.7951668753124,-20.8494946447379,
-8.45445602036142));
#74117=CARTESIAN_POINT('Ctrl Pts',(-17.8156348684865,-20.859450137226,-8.45583132493096));
#74118=CARTESIAN_POINT('Ctrl Pts',(-17.8232632265163,-20.8631041503412,
-8.45634080939984));
#74119=CARTESIAN_POINT('Ctrl Pts',(-17.8367536640226,-20.8694670035107,
-8.45723644793592));
#74120=CARTESIAN_POINT('Ctrl Pts',(-17.8426065837236,-20.8721949056878,
-8.45762325933131));
#74121=CARTESIAN_POINT('Ctrl Pts',(-17.8547361793791,-20.8777808017584,
-8.45842127846437));
#74122=CARTESIAN_POINT('Ctrl Pts',(-17.8610145302108,-20.8806349924083,
-8.45883235144981));
#74123=CARTESIAN_POINT('Ctrl Pts',(-17.8771619324139,-20.8878807314515,
-8.45988457537688));
#74124=CARTESIAN_POINT('Ctrl Pts',(-17.8870509275065,-20.8922275525357,
-8.46052418780893));
#74125=CARTESIAN_POINT('Ctrl Pts',(-17.9284285662296,-20.9100389336873,
-8.46318100360758));
#74126=CARTESIAN_POINT('Ctrl Pts',(-17.9602093615057,-20.9228145636113,
-8.46517476504808));
#74127=CARTESIAN_POINT('Ctrl Pts',(-18.0437776850987,-20.9540750178992,
-8.47030821499117));
#74128=CARTESIAN_POINT('Ctrl Pts',(-18.0960008937031,-20.9713238975377,
-8.47340872758479));
#74129=CARTESIAN_POINT('Ctrl Pts',(-18.2538216920665,-21.0167156670898,
-8.4825408426409));
#74130=CARTESIAN_POINT('Ctrl Pts',(-18.3609865215301,-21.0387400016039,
-8.48842367542667));
#74131=CARTESIAN_POINT('Ctrl Pts',(-18.5016775786826,-21.0564656108686,
-8.4961435522461));
#74132=CARTESIAN_POINT('Ctrl Pts',(-18.5340722027113,-21.0597898422532,
-8.49792169480362));
#74133=CARTESIAN_POINT('Ctrl Pts',(-18.6522825775706,-21.0691705350073,
-8.50444936866397));
#74134=CARTESIAN_POINT('Ctrl Pts',(-18.7383602080486,-21.0707416539178,
-8.50927612889432));
#74135=CARTESIAN_POINT('Ctrl Pts',(-18.8338936818678,-21.0666637516451,
-8.51494188325393));
#74136=CARTESIAN_POINT('Ctrl Pts',(-18.8435010798833,-21.0661880322748,
-8.51551516134385));
#74137=CARTESIAN_POINT('Ctrl Pts',(-18.8577021944282,-21.0653877947978,
-8.5163681587277));
#74138=CARTESIAN_POINT('Ctrl Pts',(-18.8622987852553,-21.0651137273914,
-8.51664512516844));
#74139=CARTESIAN_POINT('Ctrl Pts',(-18.8704615536325,-21.0646002980545,
-8.51713857360574));
#74140=CARTESIAN_POINT('Ctrl Pts',(-18.8740280567105,-21.0643668994937,
-8.51735471857563));
#74141=CARTESIAN_POINT('Ctrl Pts',(-18.8816790799238,-21.063846740259,-8.517819590728));
#74142=CARTESIAN_POINT('Ctrl Pts',(-18.8857633031915,-21.0635571657281,
-8.51806846767783));
#74143=CARTESIAN_POINT('Ctrl Pts',(-18.8969977639433,-21.0627278712461,
-8.51875499058577));
#74144=CARTESIAN_POINT('Ctrl Pts',(-18.9041460619185,-21.0621636741561,
-8.51919397419287));
#74145=CARTESIAN_POINT('Ctrl Pts',(-18.9426968143835,-21.0589238041009,
-8.52157257020084));
#74146=CARTESIAN_POINT('Ctrl Pts',(-18.9740376418705,-21.055583599726,-8.52354624705379));
#74147=CARTESIAN_POINT('Ctrl Pts',(-19.1675181476385,-21.0305832503529,
-8.53593094290034));
#74148=CARTESIAN_POINT('Ctrl Pts',(-19.3267651978501,-20.9908907591632,
-8.54694858740966));
#74149=CARTESIAN_POINT('Ctrl Pts',(-19.5894103359619,-20.8920170109195,
-8.56528158817152));
#74150=CARTESIAN_POINT('Ctrl Pts',(-19.6953717245056,-20.8417526575434,
-8.57273930452554));
#74151=CARTESIAN_POINT('Ctrl Pts',(-19.8101120405206,-20.7751605038146,
-8.5808399341808));
#74152=CARTESIAN_POINT('Ctrl Pts',(-19.8234898862179,-20.7671978279436,
-8.58178512023024));
#74153=CARTESIAN_POINT('Ctrl Pts',(-19.8435544307931,-20.7549534015224,
-8.58320410595264));
#74154=CARTESIAN_POINT('Ctrl Pts',(-19.8503066561389,-20.7507805466739,
-8.58368186786966));
#74155=CARTESIAN_POINT('Ctrl Pts',(-19.8622901834543,-20.7432812982607,
-8.58453025648648));
#74156=CARTESIAN_POINT('Ctrl Pts',(-19.8675306149866,-20.7399697351279,
-8.5849014242043));
#74157=CARTESIAN_POINT('Ctrl Pts',(-19.8777828624621,-20.7334278865183,
-8.58562792440446));
#74158=CARTESIAN_POINT('Ctrl Pts',(-19.8827957227794,-20.7301993532136,
-8.58598331723653));
#74159=CARTESIAN_POINT('Ctrl Pts',(-19.8965063352287,-20.7212868554088,
-8.5869558567801));
#74160=CARTESIAN_POINT('Ctrl Pts',(-19.9051760618663,-20.7155599207609,
-8.58757139381875));
#74161=CARTESIAN_POINT('Ctrl Pts',(-19.9394052752561,-20.6925854941156,
-8.59000424639734));
#74162=CARTESIAN_POINT('Ctrl Pts',(-19.9646295784435,-20.6748437900011,
-8.591802869364));
#74163=CARTESIAN_POINT('Ctrl Pts',(-20.0278333115618,-20.6282923009128,
-8.59633269942516));
#74164=CARTESIAN_POINT('Ctrl Pts',(-20.0652445440261,-20.5987388751438,
-8.59903571713064));
#74165=CARTESIAN_POINT('Ctrl Pts',(-20.2548236585266,-20.4382918613778,
-8.61293427422033));
#74166=CARTESIAN_POINT('Ctrl Pts',(-20.3887826666009,-20.2875321456035,
-8.6233575791137));
#74167=CARTESIAN_POINT('Ctrl Pts',(-20.5222696864977,-20.0857910118521,
-8.63711213022692));
#74168=CARTESIAN_POINT('Ctrl Pts',(-20.5440198585186,-20.0507347895498,
-8.6395001000153));
#74169=CARTESIAN_POINT('Ctrl Pts',(-20.5684453767921,-20.0086711334096,
-8.6423902045905));
#74170=CARTESIAN_POINT('Ctrl Pts',(-20.5721265261176,-20.0022545381827,
-8.6428317414232));
#74171=CARTESIAN_POINT('Ctrl Pts',(-20.578037029276,-19.9918257074463,-8.64355066140592));
#74172=CARTESIAN_POINT('Ctrl Pts',(-20.5802871333345,-19.9878252205756,
-8.64382674485742));
#74173=CARTESIAN_POINT('Ctrl Pts',(-20.5842655206248,-19.9806978504854,
-8.64431922367947));
#74174=CARTESIAN_POINT('Ctrl Pts',(-20.5859989159615,-19.9775738781084,
-8.64453528702635));
#74175=CARTESIAN_POINT('Ctrl Pts',(-20.5897066045093,-19.97085172727,-8.64500067096878));
#74176=CARTESIAN_POINT('Ctrl Pts',(-20.5916783155431,-19.9672522442628,
-8.64525014494193));
#74177=CARTESIAN_POINT('Ctrl Pts',(-20.5970870909802,-19.957309673638,-8.64593996075882));
#74178=CARTESIAN_POINT('Ctrl Pts',(-20.600502179122,-19.9509547839456,-8.64638166115672));
#74179=CARTESIAN_POINT('Ctrl Pts',(-20.6189552149497,-19.9161918873852,
-8.64880170059864));
#74180=CARTESIAN_POINT('Ctrl Pts',(-20.6333762963376,-19.8874632985264,
-8.65081549346985));
#74181=CARTESIAN_POINT('Ctrl Pts',(-20.6750700256576,-19.7994623073921,
-8.6570009759816));
#74182=CARTESIAN_POINT('Ctrl Pts',(-20.7002399655389,-19.7392940263136,
-8.66125187701144));
#74183=CARTESIAN_POINT('Ctrl Pts',(-20.7225804318258,-19.6781107809139,
-8.66553671816755));
#74184=CARTESIAN_POINT('',(-20.8507519460844,-18.9524633045424,-7.68905625084234));
#74185=CARTESIAN_POINT('Ctrl Pts',(-20.7225805821191,-19.6781103693095,
-8.44448865465826));
#74186=CARTESIAN_POINT('Ctrl Pts',(-20.697822657537,-19.7459142874996,-8.44016253253484));
#74187=CARTESIAN_POINT('Ctrl Pts',(-20.6696010727523,-19.8124278882354,
-8.43583641041142));
#74188=CARTESIAN_POINT('Ctrl Pts',(-20.6380875232199,-19.8772781765061,
-8.431510288288));
#74189=CARTESIAN_POINT('Ctrl Pts',(-20.6065602995994,-19.9421566040554,
-8.42718228901091));
#74190=CARTESIAN_POINT('Ctrl Pts',(-20.5717385063017,-20.0053698483387,
-8.42285428973383));
#74191=CARTESIAN_POINT('Ctrl Pts',(-20.5338393726596,-20.0665704251524,
-8.41852629045674));
#74192=CARTESIAN_POINT('Ctrl Pts',(-20.4958706164931,-20.1278834303579,
-8.41419034043762));
#74193=CARTESIAN_POINT('Ctrl Pts',(-20.454813509682,-20.1871759749339,-8.4098543904185));
#74194=CARTESIAN_POINT('Ctrl Pts',(-20.4109277577034,-20.244130912657,-8.40551844039938));
#74195=CARTESIAN_POINT('Ctrl Pts',(-20.3707283792957,-20.2963016740203,
-8.40154670725781));
#74196=CARTESIAN_POINT('Ctrl Pts',(-20.3281562877958,-20.3465112289193,
-8.39757497411623));
#74197=CARTESIAN_POINT('Ctrl Pts',(-20.2834377820476,-20.3945434342034,
-8.39360324097466));
#74198=CARTESIAN_POINT('Ctrl Pts',(-20.234030095452,-20.447612294745,-8.38921503204376));
#74199=CARTESIAN_POINT('Ctrl Pts',(-20.1817963672774,-20.4982434590661,
-8.38482682311287));
#74200=CARTESIAN_POINT('Ctrl Pts',(-20.1270066890246,-20.5461208750697,
-8.38043861418197));
#74201=CARTESIAN_POINT('Ctrl Pts',(-20.0722983277385,-20.5939272330497,
-8.3760569180807));
#74202=CARTESIAN_POINT('Ctrl Pts',(-20.01504190713,-20.6389876412174,-8.37167522197942));
#74203=CARTESIAN_POINT('Ctrl Pts',(-19.9555455237306,-20.6810215537852,
-8.36729352587815));
#74204=CARTESIAN_POINT('Ctrl Pts',(-19.8961190533168,-20.7230060731604,
-8.36291697861851));
#74205=CARTESIAN_POINT('Ctrl Pts',(-19.8344582408823,-20.7619708847354,
-8.35854043135888));
#74206=CARTESIAN_POINT('Ctrl Pts',(-19.7709042257784,-20.7976756558407,
-8.35416388409924));
#74207=CARTESIAN_POINT('Ctrl Pts',(-19.7073905157073,-20.833357783499,-8.34979011238226));
#74208=CARTESIAN_POINT('Ctrl Pts',(-19.6419864047148,-20.8657837371301,
-8.34541634066529));
#74209=CARTESIAN_POINT('Ctrl Pts',(-19.5750607832523,-20.8947572568067,
-8.34104256894831));
#74210=CARTESIAN_POINT('Ctrl Pts',(-19.5081555274813,-20.9237219597439,
-8.33667012818477));
#74211=CARTESIAN_POINT('Ctrl Pts',(-19.4397301228484,-20.9492361229378,
-8.33229768742123));
#74212=CARTESIAN_POINT('Ctrl Pts',(-19.3701752330597,-20.9711508296414,
-8.32792524665768));
#74213=CARTESIAN_POINT('Ctrl Pts',(-19.3006185647447,-20.9930660967064,
-8.32355269409035));
#74214=CARTESIAN_POINT('Ctrl Pts',(-19.2299328146161,-21.0113815814961,
-8.31918014152301));
#74215=CARTESIAN_POINT('Ctrl Pts',(-19.158524056411,-21.0259981498372,-8.31480758895567));
#74216=CARTESIAN_POINT('Ctrl Pts',(-19.0870411875032,-21.0406298878043,
-8.31043049838835));
#74217=CARTESIAN_POINT('Ctrl Pts',(-19.0148342859549,-21.0515549478116,
-8.30605340782102));
#74218=CARTESIAN_POINT('Ctrl Pts',(-18.9423190546122,-21.0587254618211,
-8.3016763172537));
#74219=CARTESIAN_POINT('Ctrl Pts',(-18.8697642200103,-21.0658998919145,
-8.29729683619476));
#74220=CARTESIAN_POINT('Ctrl Pts',(-18.7969012025329,-21.0693156708866,
-8.29291735513582));
#74221=CARTESIAN_POINT('Ctrl Pts',(-18.724147530365,-21.0689770732916,-8.28853787407688));
#74222=CARTESIAN_POINT('Ctrl Pts',(-18.6512649028016,-21.0686378755345,
-8.28415063041716));
#74223=CARTESIAN_POINT('Ctrl Pts',(-18.5784924896217,-21.0645310394331,
-8.27976338675744));
#74224=CARTESIAN_POINT('Ctrl Pts',(-18.506243930903,-21.0567128481077,-8.27537614309772));
#74225=CARTESIAN_POINT('Ctrl Pts',(-18.4571218728287,-21.0513972313654,
-8.2723932401629));
#74226=CARTESIAN_POINT('Ctrl Pts',(-18.408241843936,-21.0443670563134,-8.26941033722807));
#74227=CARTESIAN_POINT('Ctrl Pts',(-18.3597305432933,-21.0356533717911,
-8.26642743429324));
#74228=CARTESIAN_POINT('Ctrl Pts',(-18.2883645862438,-21.0228344939807,
-8.26203922536235));
#74229=CARTESIAN_POINT('Ctrl Pts',(-18.2175186632354,-21.0063198837036,
-8.25765101643146));
#74230=CARTESIAN_POINT('Ctrl Pts',(-18.147604719472,-20.9861655721633,-8.25326280750056));
#74231=CARTESIAN_POINT('Ctrl Pts',(-18.0777945395931,-20.966041172963,-8.2488811113993));
#74232=CARTESIAN_POINT('Ctrl Pts',(-18.008914052767,-20.9422879285592,-8.24449941529804));
#74233=CARTESIAN_POINT('Ctrl Pts',(-17.9413659204126,-20.915013045264,-8.24011771919678));
#74234=CARTESIAN_POINT('Ctrl Pts',(-17.8738971624894,-20.8877702121273,
-8.23574117193714));
#74235=CARTESIAN_POINT('Ctrl Pts',(-17.807758093989,-20.8570141403844,-8.2313646246775));
#74236=CARTESIAN_POINT('Ctrl Pts',(-17.7433354489135,-20.8229015867278,
-8.22698807741786));
#74237=CARTESIAN_POINT('Ctrl Pts',(-17.6789536597432,-20.7888106667569,
-8.22261430570089));
#74238=CARTESIAN_POINT('Ctrl Pts',(-17.6162865594647,-20.7513677135309,
-8.21824053398391));
#74239=CARTESIAN_POINT('Ctrl Pts',(-17.5556988450228,-20.7107766737648,
-8.21386676226694));
#74240=CARTESIAN_POINT('Ctrl Pts',(-17.4951295676258,-20.6701979859885,
-8.20949432150338));
#74241=CARTESIAN_POINT('Ctrl Pts',(-17.436638820346,-20.6264733818697,-8.20512188073983));
#74242=CARTESIAN_POINT('Ctrl Pts',(-17.3805632774559,-20.5798507419506,
-8.20074943997627));
#74243=CARTESIAN_POINT('Ctrl Pts',(-17.3244863007081,-20.5332269098855,
-8.19637688740893));
#74244=CARTESIAN_POINT('Ctrl Pts',(-17.2708250206049,-20.4837052048259,
-8.1920043348416));
#74245=CARTESIAN_POINT('Ctrl Pts',(-17.2198825933099,-20.4315734110743,
-8.18763178227426));
#74246=CARTESIAN_POINT('Ctrl Pts',(-17.1688872960423,-20.3793875129808,
-8.18325469170693));
#74247=CARTESIAN_POINT('Ctrl Pts',(-17.1206168232086,-20.3245864635404,
-8.17887760113961));
#74248=CARTESIAN_POINT('Ctrl Pts',(-17.0753364363194,-20.2674938929992,
-8.17450051057228));
#74249=CARTESIAN_POINT('Ctrl Pts',(-17.0300313201303,-20.2103701420863,
-8.17012102951334));
#74250=CARTESIAN_POINT('Ctrl Pts',(-16.9877198211694,-20.1509527715826,
-8.1657415484544));
#74251=CARTESIAN_POINT('Ctrl Pts',(-16.9486243453007,-20.0895951703514,
-8.16136206739546));
#74252=CARTESIAN_POINT('Ctrl Pts',(-16.9094595729634,-20.028128813184,-8.15697482373574));
#74253=CARTESIAN_POINT('Ctrl Pts',(-16.8735224451874,-19.9647157776944,
-8.15258758007602));
#74254=CARTESIAN_POINT('Ctrl Pts',(-16.8409895323044,-19.8997343347135,
-8.1482003364163));
#74255=CARTESIAN_POINT('Ctrl Pts',(-16.8188702864078,-19.8555532150832,
-8.14521743348146));
#74256=CARTESIAN_POINT('Ctrl Pts',(-16.7983237185206,-19.8106475457988,
-8.14223453054663));
#74257=CARTESIAN_POINT('Ctrl Pts',(-16.7793923012851,-19.765140666874,-8.1392516276118));
#74258=CARTESIAN_POINT('Ctrl Pts',(-16.7515419099038,-19.6981945754734,
-8.1348634186809));
#74259=CARTESIAN_POINT('Ctrl Pts',(-16.7270805292278,-19.6296853205151,
-8.13047520975));
#74260=CARTESIAN_POINT('Ctrl Pts',(-16.7061840240079,-19.5599896113515,
-8.12608700081911));
#74261=CARTESIAN_POINT('Ctrl Pts',(-16.6853185326665,-19.490397342176,-8.12170530471784));
#74262=CARTESIAN_POINT('Ctrl Pts',(-16.6680075510804,-19.4196225726488,
-8.11732360861658));
#74263=CARTESIAN_POINT('Ctrl Pts',(-16.6543788886961,-19.3480619060438,
-8.11294191251532));
#74264=CARTESIAN_POINT('Ctrl Pts',(-16.6407662410746,-19.276585328917,-8.10856536525568));
#74265=CARTESIAN_POINT('Ctrl Pts',(-16.6308274068039,-19.2043251607433,
-8.10418881799604));
#74266=CARTESIAN_POINT('Ctrl Pts',(-16.6246399100932,-19.1316914330408,
-8.0998122707364));
#74267=CARTESIAN_POINT('Ctrl Pts',(-16.618456337403,-19.0591037685929,-8.09543849901943));
#74268=CARTESIAN_POINT('Ctrl Pts',(-16.6160194227851,-18.9861434941228,
-8.09106472730246));
#74269=CARTESIAN_POINT('Ctrl Pts',(-16.6173550828665,-18.9132276545354,
-8.08669095558548));
#74270=CARTESIAN_POINT('Ctrl Pts',(-16.618690336502,-18.8403340034828,-8.08231851482193));
#74271=CARTESIAN_POINT('Ctrl Pts',(-16.6237958768595,-18.7674852424751,
-8.07794607405837));
#74272=CARTESIAN_POINT('Ctrl Pts',(-16.6326455110292,-18.6950986343316,
-8.07357363329481));
#74273=CARTESIAN_POINT('Ctrl Pts',(-16.641495371485,-18.6227101752548,-8.06920108072747));
#74274=CARTESIAN_POINT('Ctrl Pts',(-16.6540894553072,-18.5507843710743,
-8.06482852816014));
#74275=CARTESIAN_POINT('Ctrl Pts',(-16.6703498741218,-18.4797319003331,
-8.0604559755928));
#74276=CARTESIAN_POINT('Ctrl Pts',(-16.6866271686124,-18.4086056886577,
-8.05607888502548));
#74277=CARTESIAN_POINT('Ctrl Pts',(-16.7065782873147,-18.3383550912945,
-8.05170179445816));
#74278=CARTESIAN_POINT('Ctrl Pts',(-16.730074689432,-18.2693783261095,-8.04732470389083));
#74279=CARTESIAN_POINT('Ctrl Pts',(-16.7535839238066,-18.200363890153,-8.04294522283189));
#74280=CARTESIAN_POINT('Ctrl Pts',(-16.780642117511,-18.1326251197526,-8.03856574177295));
#74281=CARTESIAN_POINT('Ctrl Pts',(-16.8110725105121,-18.0665403057327,
-8.034186260714));
#74282=CARTESIAN_POINT('Ctrl Pts',(-16.8415568411806,-18.0003383568236,
-8.02979901705429));
#74283=CARTESIAN_POINT('Ctrl Pts',(-16.8754250830333,-17.9357966461506,
-8.02541177339457));
#74284=CARTESIAN_POINT('Ctrl Pts',(-16.9124547443358,-17.8732683922461,
-8.02102452973485));
#74285=CARTESIAN_POINT('Ctrl Pts',(-16.937631345852,-17.830755204799,-8.01804162680002));
#74286=CARTESIAN_POINT('Ctrl Pts',(-16.964268439743,-17.7891722056906,-8.0150587238652));
#74287=CARTESIAN_POINT('Ctrl Pts',(-16.992285306212,-17.7486218693016,-8.01207582093037));
#74288=CARTESIAN_POINT('Ctrl Pts',(-17.0335014860011,-17.6889674480278,
-8.00768761199947));
#74289=CARTESIAN_POINT('Ctrl Pts',(-17.0778664461833,-17.6313165376485,
-8.00329940306857));
#74290=CARTESIAN_POINT('Ctrl Pts',(-17.1251586260629,-17.5760209182156,
-7.99891119413767));
#74291=CARTESIAN_POINT('Ctrl Pts',(-17.1723806165064,-17.5208073666501,
-7.99452949803641));
#74292=CARTESIAN_POINT('Ctrl Pts',(-17.222520891325,-17.467942530263,-7.99014780193514));
#74293=CARTESIAN_POINT('Ctrl Pts',(-17.2753151507582,-17.4177485504024,
-7.98576610583387));
#74294=CARTESIAN_POINT('Ctrl Pts',(-17.3280473727351,-17.3676135524627,
-7.98138955857422));
#74295=CARTESIAN_POINT('Ctrl Pts',(-17.3834270362638,-17.3201435071857,
-7.97701301131459));
#74296=CARTESIAN_POINT('Ctrl Pts',(-17.4411513321106,-17.2756255424468,
-7.97263646405494));
#74297=CARTESIAN_POINT('Ctrl Pts',(-17.498839020048,-17.2311358103542,-7.96826269233796));
#74298=CARTESIAN_POINT('Ctrl Pts',(-17.5588680090007,-17.189594738041,-7.96388892062099));
#74299=CARTESIAN_POINT('Ctrl Pts',(-17.6209016583813,-17.1512498557863,
-7.95951514890401));
#74300=CARTESIAN_POINT('Ctrl Pts',(-17.682916430714,-17.112916642008,-7.95514270814045));
#74301=CARTESIAN_POINT('Ctrl Pts',(-17.7469342423164,-17.077777940832,-7.95077026737688));
#74302=CARTESIAN_POINT('Ctrl Pts',(-17.8125900634655,-17.0460375846162,
-7.94639782661332));
#74303=CARTESIAN_POINT('Ctrl Pts',(-17.8782475634413,-17.014296416796,-7.94202527404596));
#74304=CARTESIAN_POINT('Ctrl Pts',(-17.9455427209596,-16.9859539746113,
-7.9376527214786));
#74305=CARTESIAN_POINT('Ctrl Pts',(-18.0140880608572,-16.9611670587717,
-7.93328016891123));
#74306=CARTESIAN_POINT('Ctrl Pts',(-18.0827045396937,-16.9363544181361,
-7.9289030783439));
#74307=CARTESIAN_POINT('Ctrl Pts',(-18.1525733368288,-16.9151048356871,
-7.92452598777657));
#74308=CARTESIAN_POINT('Ctrl Pts',(-18.2232900373613,-16.8975257767347,
-7.92014889720925));
#74309=CARTESIAN_POINT('Ctrl Pts',(-18.2940453589085,-16.8799371172058,
-7.91576941615031));
#74310=CARTESIAN_POINT('Ctrl Pts',(-18.3656490319753,-16.866023064409,-7.91138993509137));
#74311=CARTESIAN_POINT('Ctrl Pts',(-18.4376872969909,-16.8558397527776,
-7.90701045403243));
#74312=CARTESIAN_POINT('Ctrl Pts',(-18.5098532493477,-16.8456383912947,
-7.9026232103727));
#74313=CARTESIAN_POINT('Ctrl Pts',(-18.5824548510295,-16.8391810190705,
-7.89823596671298));
#74314=CARTESIAN_POINT('Ctrl Pts',(-18.6550746705926,-16.8364717462587,
-7.89384872305326));
#74315=CARTESIAN_POINT('Ctrl Pts',(-18.7044491502656,-16.8346297018115,
-7.89086582011848));
#74316=CARTESIAN_POINT('Ctrl Pts',(-18.7538320255735,-16.834519193629,-7.8878829171837));
#74317=CARTESIAN_POINT('Ctrl Pts',(-18.8030934396838,-16.8361278165748,
-7.88490001424892));
#74318=CARTESIAN_POINT('Ctrl Pts',(-18.8755629038514,-16.8384942943756,
-7.88051180531802));
#74319=CARTESIAN_POINT('Ctrl Pts',(-18.9480521075246,-16.8445928606293,
-7.87612359638712));
#74320=CARTESIAN_POINT('Ctrl Pts',(-19.0201453327478,-16.8544276297237,
-7.87173538745623));
#74321=CARTESIAN_POINT('Ctrl Pts',(-19.0921315596717,-16.8642478023901,
-7.86735369135495));
#74322=CARTESIAN_POINT('Ctrl Pts',(-19.1637225008054,-16.8777931053666,
-7.86297199525368));
#74323=CARTESIAN_POINT('Ctrl Pts',(-19.2345042258077,-16.8950156733828,
-7.8585902991524));
#74324=CARTESIAN_POINT('Ctrl Pts',(-19.3052027766498,-16.912218003511,-7.85421375189277));
#74325=CARTESIAN_POINT('Ctrl Pts',(-19.3750935339399,-16.933088901349,-7.84983720463313));
#74326=CARTESIAN_POINT('Ctrl Pts',(-19.4437711636785,-16.9575291691252,
-7.8454606573735));
#74327=CARTESIAN_POINT('Ctrl Pts',(-19.5124052390626,-16.9819539372387,
-7.84108688565653));
#74328=CARTESIAN_POINT('Ctrl Pts',(-19.5798272600409,-17.0099434226001,
-7.83671311393956));
#74329=CARTESIAN_POINT('Ctrl Pts',(-19.6456468756563,-17.0413485471949,
-7.83233934222259));
#74330=CARTESIAN_POINT('Ctrl Pts',(-19.7114464621417,-17.0727441151049,
-7.82796690145903));
#74331=CARTESIAN_POINT('Ctrl Pts',(-19.7756441762372,-17.1075530511358,
-7.82359446069548));
#74332=CARTESIAN_POINT('Ctrl Pts',(-19.8378710435211,-17.145578753647,-7.81922201993193));
#74333=CARTESIAN_POINT('Ctrl Pts',(-19.900099501953,-17.1836054284797,-7.81484946736458));
#74334=CARTESIAN_POINT('Ctrl Pts',(-19.9603566029526,-17.2248487798652,
-7.81047691479722));
#74335=CARTESIAN_POINT('Ctrl Pts',(-20.0183007689805,-17.2690678757608,
-7.80610436222987));
#74336=CARTESIAN_POINT('Ctrl Pts',(-20.0763050716493,-17.3133328639019,
-7.80172727166255));
#74337=CARTESIAN_POINT('Ctrl Pts',(-20.1319912623922,-17.3605794693661,
-7.79735018109523));
#74338=CARTESIAN_POINT('Ctrl Pts',(-20.1850500777746,-17.4105258121556,
-7.79297309052791));
#74339=CARTESIAN_POINT('Ctrl Pts',(-20.2381378705453,-17.4604994324967,
-7.78859360946898));
#74340=CARTESIAN_POINT('Ctrl Pts',(-20.2885950971609,-17.5131753771409,
-7.78421412841004));
#74341=CARTESIAN_POINT('Ctrl Pts',(-20.3361505972381,-17.5682361242721,
-7.7798346473511));
#74342=CARTESIAN_POINT('Ctrl Pts',(-20.38379038912,-17.623394466208,-7.77544740369138));
#74343=CARTESIAN_POINT('Ctrl Pts',(-20.4285178872514,-17.6809456706585,
-7.77106016003166));
#74344=CARTESIAN_POINT('Ctrl Pts',(-20.4701036879201,-17.7405409685878,
-7.76667291637194));
#74345=CARTESIAN_POINT('Ctrl Pts',(-20.4983780251765,-17.7810600285903,
-7.76369001343712));
#74346=CARTESIAN_POINT('Ctrl Pts',(-20.5252009588539,-17.822523395732,-7.76070711050231));
#74347=CARTESIAN_POINT('Ctrl Pts',(-20.5505126306682,-17.864815166302,-7.7577242075675));
#74348=CARTESIAN_POINT('Ctrl Pts',(-20.5890325091508,-17.929175745687,-7.75318475796427));
#74349=CARTESIAN_POINT('Ctrl Pts',(-20.6241921153262,-17.9956925763863,
-7.74864530836104));
#74350=CARTESIAN_POINT('Ctrl Pts',(-20.6557527999575,-18.0639937073108,
-7.74410585875782));
#74351=CARTESIAN_POINT('Ctrl Pts',(-20.6876473131872,-18.1330172836155,
-7.73951839377987));
#74352=CARTESIAN_POINT('Ctrl Pts',(-20.7158660149379,-18.2038627902845,
-7.73493092880193));
#74353=CARTESIAN_POINT('Ctrl Pts',(-20.7402081049561,-18.2761168447072,
-7.73034346382399));
#74354=CARTESIAN_POINT('Ctrl Pts',(-20.7642010194568,-18.3473344496376,
-7.72582180381415));
#74355=CARTESIAN_POINT('Ctrl Pts',(-20.7844276391867,-18.4199200369922,
-7.72130014380432));
#74356=CARTESIAN_POINT('Ctrl Pts',(-20.8007427486143,-18.4934551155553,
-7.71677848379448));
#74357=CARTESIAN_POINT('Ctrl Pts',(-20.8174140154884,-18.5685954586084,
-7.71215811633248));
#74358=CARTESIAN_POINT('Ctrl Pts',(-20.8300007712016,-18.6447268210057,
-7.70753774887049));
#74359=CARTESIAN_POINT('Ctrl Pts',(-20.8384015048748,-18.7213849391716,
-7.70291738140849));
#74360=CARTESIAN_POINT('Ctrl Pts',(-20.8468022385479,-18.7980430573375,
-7.69829701394649));
#74361=CARTESIAN_POINT('Ctrl Pts',(-20.8510168371563,-18.8752274520633,
-7.6936766464845));
#74362=CARTESIAN_POINT('Ctrl Pts',(-20.850999949394,-18.9524628884561,-7.6890562790225));
#74363=CARTESIAN_POINT('Ctrl Pts',(-20.8476070359586,-18.9524685808987,
-7.68905589349203));
#74364=CARTESIAN_POINT('Ctrl Pts',(-20.8480883281253,-19.2000067147174,
-7.67422393751874));
#74365=CARTESIAN_POINT('Ctrl Pts',(-20.8073980344604,-19.4473941194524,
-7.65939198154544));
#74366=CARTESIAN_POINT('Ctrl Pts',(-20.7249098202513,-19.6789408942641,
-7.64456002557215));
#74367=CARTESIAN_POINT('Origin',(-18.734,-18.952,0.));
#74368=CARTESIAN_POINT('',(-20.7225805835101,-19.6781103655001,-6.84500601987795));
#74369=CARTESIAN_POINT('',(-20.7225805740154,-19.678110391503,-7.06814851970791));
#74370=CARTESIAN_POINT('',(-20.7225805821191,-19.6781103693095,0.));
#74371=CARTESIAN_POINT('',(-20.8510002457943,-18.9509645098827,-7.10922383901745));
#74372=CARTESIAN_POINT('Ctrl Pts',(-20.7225805740154,-19.678110391503,-7.06814851970791));
#74373=CARTESIAN_POINT('Ctrl Pts',(-20.746868289606,-19.6115942253996,-7.07222367278122));
#74374=CARTESIAN_POINT('Ctrl Pts',(-20.7678086356895,-19.5438870495728,
-7.07619430904908));
#74375=CARTESIAN_POINT('Ctrl Pts',(-20.829027411365,-19.3038845351043,-7.08986548609027));
#74376=CARTESIAN_POINT('Ctrl Pts',(-20.8510859889779,-19.1277568944903,
-7.0991404004068));
#74377=CARTESIAN_POINT('Ctrl Pts',(-20.8509997481143,-18.9509672928449,
-7.10922281586367));
#74378=CARTESIAN_POINT('Ctrl Pts',(-20.850999746731,-18.9509644609977,-7.10922297736565));
#74379=CARTESIAN_POINT('Ctrl Pts',(-20.8509866388502,-18.9241674207522,
-7.11075122973925));
#74380=CARTESIAN_POINT('Ctrl Pts',(-20.8504647357519,-18.8973740150214,
-7.11229817883972));
#74381=CARTESIAN_POINT('Ctrl Pts',(-20.8488772347217,-18.8561184486926,
-7.11471899714347));
#74382=CARTESIAN_POINT('Ctrl Pts',(-20.8481713903698,-18.8416446808493,
-7.11557568457049));
#74383=CARTESIAN_POINT('Ctrl Pts',(-20.8470399810025,-18.8224889222828,
-7.11672061828107));
#74384=CARTESIAN_POINT('Ctrl Pts',(-20.8467473096478,-18.8177990864489,
-7.11700181224313));
#74385=CARTESIAN_POINT('Ctrl Pts',(-20.8462061820977,-18.8095688211845,
-7.11749689627056));
#74386=CARTESIAN_POINT('Ctrl Pts',(-20.84596443064,-18.8060279489741,-7.11771041834802));
#74387=CARTESIAN_POINT('Ctrl Pts',(-20.8454718256639,-18.7990703880803,
-7.11813103347815));
#74388=CARTESIAN_POINT('Ctrl Pts',(-20.8452215797289,-18.7956536602765,
-7.11833809294867));
#74389=CARTESIAN_POINT('Ctrl Pts',(-20.844666932601,-18.7883250321715,-7.11878332283099));
#74390=CARTESIAN_POINT('Ctrl Pts',(-20.8443599504862,-18.7844133827758,
-7.11902163417546));
#74391=CARTESIAN_POINT('Ctrl Pts',(-20.8435234725859,-18.7741216578765,
-7.11965036568249));
#74392=CARTESIAN_POINT('Ctrl Pts',(-20.8429759117637,-18.7677431489571,
-7.12004177913951));
#74393=CARTESIAN_POINT('Ctrl Pts',(-20.8405832036317,-18.7412797723747,
-7.12167265453771));
#74394=CARTESIAN_POINT('Ctrl Pts',(-20.8384800666777,-18.7212200432533,
-7.12292554864206));
#74395=CARTESIAN_POINT('Ctrl Pts',(-20.8355857385863,-18.6969616625413,
-7.12445842633881));
#74396=CARTESIAN_POINT('Ctrl Pts',(-20.8350679540685,-18.6927305995594,
-7.12472644129594));
#74397=CARTESIAN_POINT('Ctrl Pts',(-20.8313092275801,-18.662767106493,-7.12662898074645));
#74398=CARTESIAN_POINT('Ctrl Pts',(-20.8276085513941,-18.6370955961657,
-7.12828257683198));
#74399=CARTESIAN_POINT('Ctrl Pts',(-20.7949897013469,-18.436934131115,-7.14132865003135));
#74400=CARTESIAN_POINT('Ctrl Pts',(-20.7447788267489,-18.2666183148405,
-7.15326722317378));
#74401=CARTESIAN_POINT('Ctrl Pts',(-20.650345255995,-18.0504506566882,-7.16847632404371));
#74402=CARTESIAN_POINT('Ctrl Pts',(-20.6244734804001,-17.9973894131658,
-7.17222246512559));
#74403=CARTESIAN_POINT('Ctrl Pts',(-20.5792806416933,-17.9137672016062,
-7.17813934634324));
#74404=CARTESIAN_POINT('Ctrl Pts',(-20.5613370651451,-17.8825012897303,
-7.18035501009081));
#74405=CARTESIAN_POINT('Ctrl Pts',(-20.536883982782,-17.8423066085726,-7.18320968006345));
#74406=CARTESIAN_POINT('Ctrl Pts',(-20.5310916875033,-17.8329506033169,
-7.18387462150893));
#74407=CARTESIAN_POINT('Ctrl Pts',(-20.5215271011513,-17.8177672023027,
-7.18495461053093));
#74408=CARTESIAN_POINT('Ctrl Pts',(-20.5177986866752,-17.811912536722,-7.1853712685657));
#74409=CARTESIAN_POINT('Ctrl Pts',(-20.5105552822049,-17.8006608624826,
-7.18617247903258));
#74410=CARTESIAN_POINT('Ctrl Pts',(-20.507044329755,-17.7952613577613,-7.18655717563589));
#74411=CARTESIAN_POINT('Ctrl Pts',(-20.4989233190818,-17.7828958759464,
-7.18743869924245));
#74412=CARTESIAN_POINT('Ctrl Pts',(-20.4942965442247,-17.7759409646788,
-7.18793489340288));
#74413=CARTESIAN_POINT('Ctrl Pts',(-20.4818382944251,-17.7574521134627,
-7.18925512890039));
#74414=CARTESIAN_POINT('Ctrl Pts',(-20.473933765784,-17.7459677196544,-7.19007640843862));
#74415=CARTESIAN_POINT('Ctrl Pts',(-20.4094922514753,-17.6542938047509,
-7.1966441130327));
#74416=CARTESIAN_POINT('Ctrl Pts',(-20.3475528107261,-17.578039846708,-7.20217270330802));
#74417=CARTESIAN_POINT('Ctrl Pts',(-20.1871361598569,-17.4064279507383,
-7.21512831208192));
#74418=CARTESIAN_POINT('Ctrl Pts',(-20.0842734926071,-17.3157980809827,
-7.22240524090073));
#74419=CARTESIAN_POINT('Ctrl Pts',(-19.9317674131666,-17.2056671649268,
-7.23282860991743));
#74420=CARTESIAN_POINT('Ctrl Pts',(-19.8890657264697,-17.1771344824893,
-7.23571524646854));
#74421=CARTESIAN_POINT('Ctrl Pts',(-19.8300448816548,-17.1407300237036,
-7.23972171332931));
#74422=CARTESIAN_POINT('Ctrl Pts',(-19.8145979528711,-17.1314722386223,
-7.24077179125907));
#74423=CARTESIAN_POINT('Ctrl Pts',(-19.7915652683004,-17.1180645010709,
-7.24234261682033));
#74424=CARTESIAN_POINT('Ctrl Pts',(-19.784068779426,-17.1137619131528,-7.24285465988697));
#74425=CARTESIAN_POINT('Ctrl Pts',(-19.7704483273461,-17.1060549966457,
-7.24378679889659));
#74426=CARTESIAN_POINT('Ctrl Pts',(-19.7643333689349,-17.1026349099216,
-7.24420593845753));
#74427=CARTESIAN_POINT('Ctrl Pts',(-19.7546719209946,-17.0972940675338,
-7.24486937067347));
#74428=CARTESIAN_POINT('Ctrl Pts',(-19.7511366636923,-17.0953529487323,
-7.24511238230894));
#74429=CARTESIAN_POINT('Ctrl Pts',(-19.7475868213506,-17.0934170032813,
-7.24535667124713));
#74430=CARTESIAN_POINT('Ctrl Pts',(-19.7475777274738,-17.0934120439225,
-7.24535729706082));
#74431=CARTESIAN_POINT('Ctrl Pts',(-19.7475594840348,-17.0934020950104,
-7.24535855252391));
#74432=CARTESIAN_POINT('Ctrl Pts',(-19.7475503350351,-17.093397105765,-7.24535918213463));
#74433=CARTESIAN_POINT('Ctrl Pts',(-19.7475319812136,-17.0933870970083,
-7.24536044520128));
#74434=CARTESIAN_POINT('Ctrl Pts',(-19.7475227762295,-17.0933820774097,
-7.24536107866839));
#74435=CARTESIAN_POINT('Ctrl Pts',(-19.7475043103821,-17.0933720079187,
-7.24536234945181));
#74436=CARTESIAN_POINT('Ctrl Pts',(-19.7474950492077,-17.0933669578578,
-7.24536298678955));
#74437=CARTESIAN_POINT('Ctrl Pts',(-19.7474764703428,-17.0933568270983,
-7.24536426535814));
#74438=CARTESIAN_POINT('Ctrl Pts',(-19.7474671527697,-17.0933517464648,
-7.24536490658093));
#74439=CARTESIAN_POINT('Ctrl Pts',(-19.7474484608541,-17.0933415544252,
-7.24536619293709));
#74440=CARTESIAN_POINT('Ctrl Pts',(-19.7474390861883,-17.093336442844,-7.24536683809274));
#74441=CARTESIAN_POINT('Ctrl Pts',(-19.7474202797423,-17.0933261887242,
-7.24536813233846));
#74442=CARTESIAN_POINT('Ctrl Pts',(-19.7474108477663,-17.09332104608,-7.24536878144202));
#74443=CARTESIAN_POINT('Ctrl Pts',(-19.747391926084,-17.0933107295019,-7.24537008362602));
#74444=CARTESIAN_POINT('Ctrl Pts',(-19.7473824364263,-17.0933055555957,
-7.24537073670312));
#74445=CARTESIAN_POINT('Ctrl Pts',(-19.7473633987774,-17.0932951761679,
-7.2453720468758));
#74446=CARTESIAN_POINT('Ctrl Pts',(-19.7473538509974,-17.0932899707628,
-7.24537270395685));
#74447=CARTESIAN_POINT('Ctrl Pts',(-19.7473346966567,-17.093279528097,-7.24537402216826));
#74448=CARTESIAN_POINT('Ctrl Pts',(-19.747325090272,-17.0932742909334,-7.24537468328653));
#74449=CARTESIAN_POINT('Ctrl Pts',(-19.747305818564,-17.0932637846683,-7.24537600958331));
#74450=CARTESIAN_POINT('Ctrl Pts',(-19.7472961530412,-17.0932585154592,
-7.24537667477558));
#74451=CARTESIAN_POINT('Ctrl Pts',(-19.747276762527,-17.0932479448174,-7.24537800925691));
#74452=CARTESIAN_POINT('Ctrl Pts',(-19.7472670376847,-17.0932426434673,
-7.24537867853574));
#74453=CARTESIAN_POINT('Ctrl Pts',(-19.7472475657517,-17.093232028837,-7.2453800186287));
#74454=CARTESIAN_POINT('Ctrl Pts',(-19.7472377621061,-17.0932266847277,
-7.24538069333527));
#74455=CARTESIAN_POINT('Ctrl Pts',(-19.7472181122366,-17.0932159735023,
-7.24538204568256));
#74456=CARTESIAN_POINT('Ctrl Pts',(-19.7472082678274,-17.0932106073755,
-7.24538272319859));
#74457=CARTESIAN_POINT('Ctrl Pts',(-19.7471885165869,-17.0931998412995,
-7.24538408253095));
#74458=CARTESIAN_POINT('Ctrl Pts',(-19.7471786113506,-17.0931944422209,
-7.24538476423753));
#74459=CARTESIAN_POINT('Ctrl Pts',(-19.7471587045236,-17.0931835917501,
-7.2453861342864));
#74460=CARTESIAN_POINT('Ctrl Pts',(-19.7471487549029,-17.0931781686866,
-7.24538681905178));
#74461=CARTESIAN_POINT('Ctrl Pts',(-19.7441393580398,-17.0915379211943,
-7.2455939362838));
#74462=CARTESIAN_POINT('Ctrl Pts',(-19.7411360224105,-17.0899103939135,
-7.24580083676566));
#74463=CARTESIAN_POINT('Ctrl Pts',(-19.734094710212,-17.0861166788207,-7.24628637285296));
#74464=CARTESIAN_POINT('Ctrl Pts',(-19.730053643727,-17.0839563346765,-7.2465653748392));
#74465=CARTESIAN_POINT('Ctrl Pts',(-19.7176093263313,-17.0773554933554,
-7.24742554672184));
#74466=CARTESIAN_POINT('Ctrl Pts',(-19.7091832947715,-17.0729585244077,
-7.24800935846962));
#74467=CARTESIAN_POINT('Ctrl Pts',(-19.5939326404601,-17.0138010722072,
-7.25601063328275));
#74468=CARTESIAN_POINT('Ctrl Pts',(-19.482680090488,-16.9681727197242,-7.2639085184497));
#74469=CARTESIAN_POINT('Ctrl Pts',(-19.2643432133411,-16.8996186070641,
-7.27902715286637));
#74470=CARTESIAN_POINT('Ctrl Pts',(-19.158142028617,-16.8750694943601,-7.28622009168223));
#74471=CARTESIAN_POINT('Ctrl Pts',(-18.9765362974362,-16.847608501746,-7.29801960758239));
#74472=CARTESIAN_POINT('Ctrl Pts',(-18.9020074916349,-16.8403506339402,
-7.30272662723546));
#74473=CARTESIAN_POINT('Ctrl Pts',(-18.8084824368351,-16.8362273237884,
-7.30846140055924));
#74474=CARTESIAN_POINT('Ctrl Pts',(-18.7897110327954,-16.835649847663,-7.30960397013258));
#74475=CARTESIAN_POINT('Ctrl Pts',(-18.7623861790448,-16.8351730558821,
-7.31125530604847));
#74476=CARTESIAN_POINT('Ctrl Pts',(-18.753837494632,-16.835075683058,-7.31177024611993));
#74477=CARTESIAN_POINT('Ctrl Pts',(-18.7388400531612,-16.8349957119377,
-7.31267074275303));
#74478=CARTESIAN_POINT('Ctrl Pts',(-18.7323915726135,-16.8349907897751,
-7.31305699344597));
#74479=CARTESIAN_POINT('Ctrl Pts',(-18.7198640355442,-16.8350384674625,
-7.31380558151473));
#74480=CARTESIAN_POINT('Ctrl Pts',(-18.7137850364791,-16.8350877882703,
-7.31416801775506));
#74481=CARTESIAN_POINT('Ctrl Pts',(-18.6992436604134,-16.8352684100428,
-7.31503307664059));
#74482=CARTESIAN_POINT('Ctrl Pts',(-18.690781650748,-16.8354242738534,-7.31553492693704));
#74483=CARTESIAN_POINT('Ctrl Pts',(-18.6601926562498,-16.8361712217935,
-7.31734362593767));
#74484=CARTESIAN_POINT('Ctrl Pts',(-18.6380738560968,-16.8370585889712,
-7.31864121513094));
#74485=CARTESIAN_POINT('Ctrl Pts',(-18.4309382179136,-16.8486248645878,
-7.33070667458507));
#74486=CARTESIAN_POINT('Ctrl Pts',(-18.2480668271197,-16.8832060533965,
-7.34062083838386));
#74487=CARTESIAN_POINT('Ctrl Pts',(-17.9957351896204,-16.9662748173921,
-7.35510190619751));
#74488=CARTESIAN_POINT('Ctrl Pts',(-17.9209448170173,-16.9957079245597,
-7.35951815846977));
#74489=CARTESIAN_POINT('Ctrl Pts',(-17.8152483351737,-17.0444135928366,
-7.36617480174179));
#74490=CARTESIAN_POINT('Ctrl Pts',(-17.7828765934529,-17.0603461103899,
-7.36827316987093));
#74491=CARTESIAN_POINT('Ctrl Pts',(-17.7443150231686,-17.0805651404608,
-7.37086431307254));
#74492=CARTESIAN_POINT('Ctrl Pts',(-17.7377186261131,-17.0840684682947,
-7.37131085341731));
#74493=CARTESIAN_POINT('Ctrl Pts',(-17.7274774565254,-17.089577203062,-7.37200948613473));
#74494=CARTESIAN_POINT('Ctrl Pts',(-17.72381974778,-17.091558610862,-7.37226007914074));
#74495=CARTESIAN_POINT('Ctrl Pts',(-17.7170375932739,-17.0952584513303,
-7.37272676780927));
#74496=CARTESIAN_POINT('Ctrl Pts',(-17.7139116406221,-17.0969740018784,
-7.37294267966426));
#74497=CARTESIAN_POINT('Ctrl Pts',(-17.7068420605829,-17.1008771231945,
-7.37343281451122));
#74498=CARTESIAN_POINT('Ctrl Pts',(-17.702901100051,-17.1030693914606,-7.37370733474758));
#74499=CARTESIAN_POINT('Ctrl Pts',(-17.6927446607421,-17.1087617620941,
-7.3744180977834));
#74500=CARTESIAN_POINT('Ctrl Pts',(-17.6865398720474,-17.1122806843829,
-7.37485550627048));
#74501=CARTESIAN_POINT('Ctrl Pts',(-17.6485646925553,-17.134071939506,-7.37755163874075));
#74502=CARTESIAN_POINT('Ctrl Pts',(-17.6172574934826,-17.1531342349018,
-7.37985651015451));
#74503=CARTESIAN_POINT('Ctrl Pts',(-17.4431946581303,-17.2654126553866,
-7.39307508997707));
#74504=CARTESIAN_POINT('Ctrl Pts',(-17.3116151507582,-17.3747936954772,
-7.40457887290739));
#74505=CARTESIAN_POINT('Ctrl Pts',(-17.1290716563344,-17.568164802461,-7.4218605509172));
#74506=CARTESIAN_POINT('Ctrl Pts',(-17.06832692473,-17.6419113369407,-7.42792345417126));
#74507=CARTESIAN_POINT('Ctrl Pts',(-17.0003026282046,-17.7369114330647,
-7.4351006451469));
#74508=CARTESIAN_POINT('Ctrl Pts',(-16.9881101287382,-17.7544961742685,
-7.43640483688866));
#74509=CARTESIAN_POINT('Ctrl Pts',(-16.9711646351047,-17.7797450502855,
-7.43824384141809));
#74510=CARTESIAN_POINT('Ctrl Pts',(-16.9661910750996,-17.7872589129673,
-7.4387869668367));
#74511=CARTESIAN_POINT('Ctrl Pts',(-16.9576980652593,-17.8002695490169,
-7.43972037008653));
#74512=CARTESIAN_POINT('Ctrl Pts',(-16.9541558127354,-17.805751220011,-7.44011149910188));
#74513=CARTESIAN_POINT('Ctrl Pts',(-16.9474249306634,-17.8162737577625,
-7.44085826804866));
#74514=CARTESIAN_POINT('Ctrl Pts',(-16.9442321496843,-17.8213118826221,
-7.44121406002586));
#74515=CARTESIAN_POINT('Ctrl Pts',(-16.9359915233256,-17.8344377386945,
-7.44213649720445));
#74516=CARTESIAN_POINT('Ctrl Pts',(-16.9309769064983,-17.8425462520201,
-7.44270191117853));
#74517=CARTESIAN_POINT('Ctrl Pts',(-16.9140962511439,-17.8702586059278,
-7.4446195765534));
#74518=CARTESIAN_POINT('Ctrl Pts',(-16.9024935405953,-17.8900215405943,
-7.44596221069099));
#74519=CARTESIAN_POINT('Ctrl Pts',(-16.8043405028427,-18.0636009964475,
-7.45755042631187));
#74520=CARTESIAN_POINT('Ctrl Pts',(-16.7370196429506,-18.2274900491444,
-7.46703498002691));
#74521=CARTESIAN_POINT('Ctrl Pts',(-16.6682260941955,-18.4811345108922,
-7.48133695378272));
#74522=CARTESIAN_POINT('Ctrl Pts',(-16.6507522877699,-18.5657193323404,
-7.48606346403716));
#74523=CARTESIAN_POINT('Ctrl Pts',(-16.6331395152954,-18.6883880526693,
-7.49314030236153));
#74524=CARTESIAN_POINT('Ctrl Pts',(-16.6287846908924,-18.7257829729442,
-7.49532720628924));
#74525=CARTESIAN_POINT('Ctrl Pts',(-16.6247551783058,-18.7708027119098,
-7.49801652806066));
#74526=CARTESIAN_POINT('Ctrl Pts',(-16.6241214512125,-18.77833745219,-7.4984685224453));
#74527=CARTESIAN_POINT('Ctrl Pts',(-16.6232000990504,-18.7900424412373,
-7.4991738467582));
#74528=CARTESIAN_POINT('Ctrl Pts',(-16.6228844304726,-18.79421050702,-7.49942563050811));
#74529=CARTESIAN_POINT('Ctrl Pts',(-16.622322490706,-18.8019340189597,-7.49989338918839));
#74530=CARTESIAN_POINT('Ctrl Pts',(-16.6220728526338,-18.8054891623207,
-7.50010917304562));
#74531=CARTESIAN_POINT('Ctrl Pts',(-16.6215294670781,-18.8135177086928,
-7.50059754107513));
#74532=CARTESIAN_POINT('Ctrl Pts',(-16.6212409528226,-18.8179913988441,
-7.50087041330138));
#74533=CARTESIAN_POINT('Ctrl Pts',(-16.6204331437055,-18.8311688394999,
-7.50167628804254));
#74534=CARTESIAN_POINT('Ctrl Pts',(-16.6199534162411,-18.8398747973703,
-7.502211426756));
#74535=CARTESIAN_POINT('Ctrl Pts',(-16.6169219287903,-18.9018570173764,
-7.50603952088913));
#74536=CARTESIAN_POINT('Ctrl Pts',(-16.6163308645768,-18.9552055382128,
-7.50942951252395));
#74537=CARTESIAN_POINT('Ctrl Pts',(-16.6182285227753,-19.0262657143222,
-7.51402367808511));
#74538=CARTESIAN_POINT('Ctrl Pts',(-16.6189259022126,-19.0440101961314,
-7.51517747973296));
#74539=CARTESIAN_POINT('Ctrl Pts',(-16.6223540538807,-19.1100518571353,
-7.51949180158957));
#74540=CARTESIAN_POINT('Ctrl Pts',(-16.6265166660615,-19.1582589459159,
-7.52268074662665));
#74541=CARTESIAN_POINT('Ctrl Pts',(-16.6454648144414,-19.3148691955398,
-7.5331014298174));
#74542=CARTESIAN_POINT('Ctrl Pts',(-16.6670001823719,-19.4222855452956,
-7.54033412189648));
#74543=CARTESIAN_POINT('Ctrl Pts',(-16.711722965055,-19.5805861668141,-7.55090754546354));
#74544=CARTESIAN_POINT('Ctrl Pts',(-16.7287685493419,-19.6330085355309,
-7.55439665486008));
#74545=CARTESIAN_POINT('Ctrl Pts',(-16.7597140585279,-19.7168926158931,
-7.5599541857702));
#74546=CARTESIAN_POINT('Ctrl Pts',(-16.7723675331868,-19.748783517653,-7.56206104536376));
#74547=CARTESIAN_POINT('Ctrl Pts',(-16.7900202527158,-19.7903009984069,
-7.56479756735056));
#74548=CARTESIAN_POINT('Ctrl Pts',(-16.7943256150807,-19.8002152492467,
-7.5654505709248));
#74549=CARTESIAN_POINT('Ctrl Pts',(-16.801502790366,-19.8164021733181,-7.56651606950218));
#74550=CARTESIAN_POINT('Ctrl Pts',(-16.8043296294835,-19.8226944615553,
-7.56693009394265));
#74551=CARTESIAN_POINT('Ctrl Pts',(-16.8098619204464,-19.8348495569959,
-7.56772960894873));
#74552=CARTESIAN_POINT('Ctrl Pts',(-16.8125635355261,-19.840714016932,-7.56811522585636));
#74553=CARTESIAN_POINT('Ctrl Pts',(-16.8188645805864,-19.8542287992774,
-7.56900364654562));
#74554=CARTESIAN_POINT('Ctrl Pts',(-16.8224831099357,-19.8618701352942,
-7.56950578426038));
#74555=CARTESIAN_POINT('Ctrl Pts',(-16.8323404327509,-19.8823677167773,
-7.5708523952996));
#74556=CARTESIAN_POINT('Ctrl Pts',(-16.8386638468601,-19.8951829513108,
-7.57169392720912));
#74557=CARTESIAN_POINT('Ctrl Pts',(-16.8978743785234,-20.0121804172648,
-7.57937578355708));
#74558=CARTESIAN_POINT('Ctrl Pts',(-16.959174384457,-20.1118875431223,-7.58589942217557));
#74559=CARTESIAN_POINT('Ctrl Pts',(-17.1248260473085,-20.3371885100922,
-7.60120841485988));
#74560=CARTESIAN_POINT('Ctrl Pts',(-17.2360472925864,-20.4567637133646,
-7.60981056431433));
#74561=CARTESIAN_POINT('Ctrl Pts',(-17.384542851605,-20.583474198908,-7.62101974207945));
#74562=CARTESIAN_POINT('Ctrl Pts',(-17.4097150985187,-20.6039721234287,
-7.62291303699605));
#74563=CARTESIAN_POINT('Ctrl Pts',(-17.441061810619,-20.6283210320993,-7.62527637617195));
#74564=CARTESIAN_POINT('Ctrl Pts',(-17.4467992531642,-20.6327306738812,
-7.62570916793069));
#74565=CARTESIAN_POINT('Ctrl Pts',(-17.4558297968618,-20.6395979424802,
-7.62639091787312));
#74566=CARTESIAN_POINT('Ctrl Pts',(-17.4591076999722,-20.6420755918964,
-7.6266384918909));
#74567=CARTESIAN_POINT('Ctrl Pts',(-17.4652486200129,-20.6466892621697,
-7.62710255766595));
#74568=CARTESIAN_POINT('Ctrl Pts',(-17.4681098369447,-20.6488275852177,
-7.62731888432482));
#74569=CARTESIAN_POINT('Ctrl Pts',(-17.474654132372,-20.6536926825989,-7.62781390872651));
#74570=CARTESIAN_POINT('Ctrl Pts',(-17.478340648725,-20.6564147361972,-7.6280929287195));
#74571=CARTESIAN_POINT('Ctrl Pts',(-17.4897013524436,-20.6647464018606,
-7.62895321007945));
#74572=CARTESIAN_POINT('Ctrl Pts',(-17.4974043847981,-20.6703162218043,
-7.62953711425411));
#74573=CARTESIAN_POINT('Ctrl Pts',(-17.6024905108618,-20.7452281187138,
-7.63750797473245));
#74574=CARTESIAN_POINT('Ctrl Pts',(-17.7055287611058,-20.8062440750724,
-7.64537152959528));
#74575=CARTESIAN_POINT('Ctrl Pts',(-17.9113004362447,-20.9056468486291,
-7.66046832742099));
#74576=CARTESIAN_POINT('Ctrl Pts',(-18.0129739427331,-20.9454130233632,
-7.66767364089163));
#74577=CARTESIAN_POINT('Ctrl Pts',(-18.1890958317102,-20.9990483206543,
-7.67950324040887));
#74578=CARTESIAN_POINT('Ctrl Pts',(-18.2620468182198,-21.0170883091843,
-7.68422764383675));
#74579=CARTESIAN_POINT('Ctrl Pts',(-18.3542890648221,-21.0347536132033,
-7.6899811799499));
#74580=CARTESIAN_POINT('Ctrl Pts',(-18.3728151392171,-21.0380461499747,
-7.69112597537445));
#74581=CARTESIAN_POINT('Ctrl Pts',(-18.3998260415797,-21.0424760141134,
-7.69277991515912));
#74582=CARTESIAN_POINT('Ctrl Pts',(-18.4082773660338,-21.0438094963808,
-7.6932952606614));
#74583=CARTESIAN_POINT('Ctrl Pts',(-18.4231132223346,-21.0460582624343,
-7.69419622489128));
#74584=CARTESIAN_POINT('Ctrl Pts',(-18.4294942417659,-21.0469956657775,
-7.69458253997317));
#74585=CARTESIAN_POINT('Ctrl Pts',(-18.4418961018197,-21.0487597011936,
-7.6953310776126));
#74586=CARTESIAN_POINT('Ctrl Pts',(-18.4479164077418,-21.0495895955375,
-7.69569339985829));
#74587=CARTESIAN_POINT('Ctrl Pts',(-18.4623217801259,-21.051512192436,-7.69655790776223));
#74588=CARTESIAN_POINT('Ctrl Pts',(-18.4707100252494,-21.0525806087103,
-7.6970593233283));
#74589=CARTESIAN_POINT('Ctrl Pts',(-18.5010310085101,-21.0562581332465,
-7.69886480164759));
#74590=CARTESIAN_POINT('Ctrl Pts',(-18.5229983294144,-21.0585742786541,
-7.70015964857557));
#74591=CARTESIAN_POINT('Ctrl Pts',(-18.7300515698798,-21.0771336873533,
-7.7122504139795));
#74592=CARTESIAN_POINT('Ctrl Pts',(-18.9164774519554,-21.0692899551196,
-7.72218745783808));
#74593=CARTESIAN_POINT('Ctrl Pts',(-19.2071139739458,-21.0183468027605,
-7.73827355701547));
#74594=CARTESIAN_POINT('Ctrl Pts',(-19.313094178067,-20.9911835347628,-7.74429703988687));
#74595=CARTESIAN_POINT('Ctrl Pts',(-19.4276559444185,-20.9521673888345,
-7.75144017293873));
#74596=CARTESIAN_POINT('Ctrl Pts',(-19.4387901513323,-20.9482712693633,
-7.75214127981236));
#74597=CARTESIAN_POINT('Ctrl Pts',(-19.4545996008962,-20.942590427378,-7.75314736748704));
#74598=CARTESIAN_POINT('Ctrl Pts',(-19.4593022049987,-20.9408817824684,
-7.75344797508748));
#74599=CARTESIAN_POINT('Ctrl Pts',(-19.4674062068257,-20.9379047092452,
-7.75396840202993));
#74600=CARTESIAN_POINT('Ctrl Pts',(-19.4708105153217,-20.9366441602408,
-7.75418775233713));
#74601=CARTESIAN_POINT('Ctrl Pts',(-19.4774131010705,-20.9341800217499,
-7.75461462403103));
#74602=CARTESIAN_POINT('Ctrl Pts',(-19.4806117122579,-20.9329774426284,
-7.75482207911996));
#74603=CARTESIAN_POINT('Ctrl Pts',(-19.489251472756,-20.9297052617764,-7.75538418810968));
#74604=CARTESIAN_POINT('Ctrl Pts',(-19.4946869725986,-20.9276209700844,
-7.75573970867091));
#74605=CARTESIAN_POINT('Ctrl Pts',(-19.5149316906852,-20.9197620169374,
-7.75707070697389));
#74606=CARTESIAN_POINT('Ctrl Pts',(-19.5296838931936,-20.9138432068835,
-7.75805430571519));
#74607=CARTESIAN_POINT('Ctrl Pts',(-19.6585815730293,-20.860434534178,-7.76676058775287));
#74608=CARTESIAN_POINT('Ctrl Pts',(-19.768419834445,-20.8032005102041,-7.77494143333174));
#74609=CARTESIAN_POINT('Ctrl Pts',(-20.0135308825098,-20.6468230523889,
-7.79415453954332));
#74610=CARTESIAN_POINT('Ctrl Pts',(-20.1433214528168,-20.540539676929,-7.80507087500697));
#74611=CARTESIAN_POINT('Ctrl Pts',(-20.2740377425466,-20.404730611505,-7.81664823128841));
#74612=CARTESIAN_POINT('Ctrl Pts',(-20.2885732390007,-20.3891654653027,
-7.81794616042519));
#74613=CARTESIAN_POINT('Ctrl Pts',(-20.308910170494,-20.3667182890134,-7.81977794443242));
#74614=CARTESIAN_POINT('Ctrl Pts',(-20.3149060462295,-20.3600149002377,
-7.82032002345927));
#74615=CARTESIAN_POINT('Ctrl Pts',(-20.3251770157455,-20.3483836360491,
-7.82125219272436));
#74616=CARTESIAN_POINT('Ctrl Pts',(-20.3294723482453,-20.3434738739644,
-7.82164312821546));
#74617=CARTESIAN_POINT('Ctrl Pts',(-20.3376538037636,-20.3340344047315,
-7.82238991155202));
#74618=CARTESIAN_POINT('Ctrl Pts',(-20.3415435938569,-20.3295079720858,
-7.82274590959635));
#74619=CARTESIAN_POINT('Ctrl Pts',(-20.3516099372605,-20.3176933609615,
-7.82366971094577));
#74620=CARTESIAN_POINT('Ctrl Pts',(-20.3577564351206,-20.3103796631465,
-7.82423627564897));
#74621=CARTESIAN_POINT('Ctrl Pts',(-20.3785535031676,-20.2852904294535,
-7.82616210536949));
#74622=CARTESIAN_POINT('Ctrl Pts',(-20.392963695283,-20.2673171150141,-7.82751163975618));
#74623=CARTESIAN_POINT('Ctrl Pts',(-20.5142337192113,-20.1108971021652,
-7.83901216327063));
#74624=CARTESIAN_POINT('Ctrl Pts',(-20.6038499556641,-19.9599397095911,
-7.84841819641638));
#74625=CARTESIAN_POINT('Ctrl Pts',(-20.6913707348718,-19.759648453698,-7.86031013461783));
#74626=CARTESIAN_POINT('Ctrl Pts',(-20.7076099334921,-19.7191101143336,
-7.86269371541934));
#74627=CARTESIAN_POINT('Ctrl Pts',(-20.7225805730004,-19.6781103942827,
-7.86510594064261));
#74628=CARTESIAN_POINT('',(-20.8523539331562,-18.9537405760439,-6.88905704666127));
#74629=CARTESIAN_POINT('Ctrl Pts',(-20.7249098202513,-19.6789408942641,
-7.64456002557215));
#74630=CARTESIAN_POINT('Ctrl Pts',(-20.6989345116989,-19.7518543277492,
-7.63988948401012));
#74631=CARTESIAN_POINT('Ctrl Pts',(-20.3954318373018,-20.4707351797969,
-7.59282700688761));
#74632=CARTESIAN_POINT('Ctrl Pts',(-19.0148744683191,-21.4394564387197,
-7.50337259420462));
#74633=CARTESIAN_POINT('Ctrl Pts',(-16.794474806048,-20.5345839704445,-7.3761967875232));
#74634=CARTESIAN_POINT('Ctrl Pts',(-16.3534691287178,-18.1777889355253,
-7.24902098084176));
#74635=CARTESIAN_POINT('Ctrl Pts',(-18.0964527733798,-16.5312844993037,
-7.12184517416032));
#74636=CARTESIAN_POINT('Ctrl Pts',(-20.292776587038,-17.0731745935747,-7.00185719610017));
#74637=CARTESIAN_POINT('Ctrl Pts',(-20.8471439801893,-18.3695361434103,
-6.92426115360048));
#74638=CARTESIAN_POINT('Ctrl Pts',(-20.8523539331563,-18.9537405760439,
-6.88905704666127));
#74639=CARTESIAN_POINT('Ctrl Pts',(-20.8509992391743,-18.9537948079469,
-6.88983562681212));
#74640=CARTESIAN_POINT('Ctrl Pts',(-20.8509308803788,-19.0344248933761,
-6.88542680327367));
#74641=CARTESIAN_POINT('Ctrl Pts',(-20.846256125498,-19.1149800327588,-6.88096325172215));
#74642=CARTESIAN_POINT('Ctrl Pts',(-20.8342751935892,-19.2186387282606,
-6.87493021363211));
#74643=CARTESIAN_POINT('Ctrl Pts',(-20.8311546068468,-19.2421629736403,
-6.87354147870167));
#74644=CARTESIAN_POINT('Ctrl Pts',(-20.8267567240817,-19.2715211958718,
-6.87177823640636));
#74645=CARTESIAN_POINT('Ctrl Pts',(-20.8258491613927,-19.2774098721672,
-6.87142304382925));
#74646=CARTESIAN_POINT('Ctrl Pts',(-20.8242842192338,-19.2872867738242,
-6.87082461715517));
#74647=CARTESIAN_POINT('Ctrl Pts',(-20.8236402480805,-19.2912771298949,
-6.87058211407328));
#74648=CARTESIAN_POINT('Ctrl Pts',(-20.8224405316354,-19.2985781517168,
-6.87013703098857));
#74649=CARTESIAN_POINT('Ctrl Pts',(-20.8218883299891,-19.3018893976088,
-6.8699346501367));
#74650=CARTESIAN_POINT('Ctrl Pts',(-20.82073183337,-19.3087240321801,-6.86951581921289));
#74651=CARTESIAN_POINT('Ctrl Pts',(-20.8201264940706,-19.312247178472,-6.86929930838652));
#74652=CARTESIAN_POINT('Ctrl Pts',(-20.8187199416278,-19.3203110438727,
-6.86880236553774));
#74653=CARTESIAN_POINT('Ctrl Pts',(-20.8179128178603,-19.3248506761268,
-6.86852160159985));
#74654=CARTESIAN_POINT('Ctrl Pts',(-20.8153705417999,-19.338883443171,-6.86765067971333));
#74655=CARTESIAN_POINT('Ctrl Pts',(-20.8135853308845,-19.3483672215856,
-6.8670577851907));
#74656=CARTESIAN_POINT('Ctrl Pts',(-20.7945684251442,-19.445726446506,-6.86092929323585));
#74657=CARTESIAN_POINT('Ctrl Pts',(-20.7718441164442,-19.5324271271654,
-6.85512345423274));
#74658=CARTESIAN_POINT('Ctrl Pts',(-20.7369695611002,-19.6377557279032,
-6.84783205872112));
#74659=CARTESIAN_POINT('Ctrl Pts',(-20.7299277273801,-19.6579889234461,
-6.84641998651614));
#74660=CARTESIAN_POINT('Ctrl Pts',(-20.7225805835101,-19.6781103655001,
-6.84500601987795));
#74661=CARTESIAN_POINT('Origin',(-18.734,-18.952,0.));
#74662=CARTESIAN_POINT('',(-20.7225805821268,-19.6781103692884,-6.04247206352563));
#74663=CARTESIAN_POINT('',(-20.722580459427,-19.6781107053232,-6.26710642520023));
#74664=CARTESIAN_POINT('',(-20.7225805821191,-19.6781103693095,0.));
#74665=CARTESIAN_POINT('Ctrl Pts',(-20.722580459427,-19.6781107053232,-6.26710642520023));
#74666=CARTESIAN_POINT('Ctrl Pts',(-20.7522829120589,-19.5967653726242,
-6.27277691375044));
#74667=CARTESIAN_POINT('Ctrl Pts',(-20.7769957147056,-19.5135926739805,
-6.27836345422882));
#74668=CARTESIAN_POINT('Ctrl Pts',(-20.8065479309516,-19.3858237632587,
-6.28658119025069));
#74669=CARTESIAN_POINT('Ctrl Pts',(-20.8151860571151,-19.3422858497125,
-6.28932042021308));
#74670=CARTESIAN_POINT('Ctrl Pts',(-20.8243855590297,-19.2868388869226,
-6.29273471116654));
#74671=CARTESIAN_POINT('Ctrl Pts',(-20.8262235216218,-19.2751557056022,
-6.29345001935078));
#74672=CARTESIAN_POINT('Ctrl Pts',(-20.829011487268,-19.2564119044014,-6.29459117866218));
#74673=CARTESIAN_POINT('Ctrl Pts',(-20.8300239038893,-19.2493609516757,
-6.29501899909521));
#74674=CARTESIAN_POINT('Ctrl Pts',(-20.8318772341774,-19.235973529657,-6.29582857368071));
#74675=CARTESIAN_POINT('Ctrl Pts',(-20.8327250735656,-19.2296381137333,
-6.2962105427308));
#74676=CARTESIAN_POINT('Ctrl Pts',(-20.8345859301686,-19.2152372049915,
-6.29707621867975));
#74677=CARTESIAN_POINT('Ctrl Pts',(-20.8355812164636,-19.2071694917844,
-6.29755936090405));
#74678=CARTESIAN_POINT('Ctrl Pts',(-20.8380346041774,-19.186293726902,-6.29880491120655));
#74679=CARTESIAN_POINT('Ctrl Pts',(-20.8394222482478,-19.173477614248,-6.29956509812174));
#74680=CARTESIAN_POINT('Ctrl Pts',(-20.8476032823545,-19.0908752941647,
-6.30443707438618));
#74681=CARTESIAN_POINT('Ctrl Pts',(-20.8510436183048,-19.0207966598717,
-6.30844173449181));
#74682=CARTESIAN_POINT('Ctrl Pts',(-20.8508787730343,-18.7582834169534,
-6.32314072120312));
#74683=CARTESIAN_POINT('Ctrl Pts',(-20.8245352117492,-18.5668343657836,
-6.33317505048021));
#74684=CARTESIAN_POINT('Ctrl Pts',(-20.7592947599496,-18.3336572753103,
-6.34683377332967));
#74685=CARTESIAN_POINT('Ctrl Pts',(-20.7441979055401,-18.2862146546721,
-6.34969727122593));
#74686=CARTESIAN_POINT('Ctrl Pts',(-20.7248154855874,-18.2319974235725,
-6.35311518075376));
#74687=CARTESIAN_POINT('Ctrl Pts',(-20.7221455095431,-18.224657277244,-6.35358104992598));
#74688=CARTESIAN_POINT('Ctrl Pts',(-20.7178168236286,-18.2129590312568,
-6.35432879726889));
#74689=CARTESIAN_POINT('Ctrl Pts',(-20.7161841985248,-18.2085912662877,
-6.35460916292821));
#74690=CARTESIAN_POINT('Ctrl Pts',(-20.71326896642,-18.2008700182166,-6.35510693818837));
#74691=CARTESIAN_POINT('Ctrl Pts',(-20.7119922425317,-18.197514361109,-6.35532399424251));
#74692=CARTESIAN_POINT('Ctrl Pts',(-20.7092701408979,-18.190414167292,-6.35578481427573));
#74693=CARTESIAN_POINT('Ctrl Pts',(-20.7078226713603,-18.1866705470788,
-6.3560286972433));
#74694=CARTESIAN_POINT('Ctrl Pts',(-20.7038921045113,-18.1765901617635,
-6.35668781580685));
#74695=CARTESIAN_POINT('Ctrl Pts',(-20.7013891054747,-18.1702612806059,
-6.35710422051401));
#74696=CARTESIAN_POINT('Ctrl Pts',(-20.6888792594576,-18.139070523753,-6.35916878035654));
#74697=CARTESIAN_POINT('Ctrl Pts',(-20.6784319312075,-18.1143893734034,
-6.36084140787467));
#74698=CARTESIAN_POINT('Ctrl Pts',(-20.6469617788922,-18.0438068633169,
-6.36572426776327));
#74699=CARTESIAN_POINT('Ctrl Pts',(-20.6247626639235,-17.9984521986412,
-6.36898510632641));
#74700=CARTESIAN_POINT('Ctrl Pts',(-20.5384183339973,-17.836937373781,-6.38094763674447));
#74701=CARTESIAN_POINT('Ctrl Pts',(-20.4650107302126,-17.72607384636,-6.3898158399104));
#74702=CARTESIAN_POINT('Ctrl Pts',(-20.3168837441426,-17.5424516024276,
-6.40514176592233));
#74703=CARTESIAN_POINT('Ctrl Pts',(-20.2462642351261,-17.4669377121572,
-6.41168271063618));
#74704=CARTESIAN_POINT('Ctrl Pts',(-20.1600892166794,-17.3873416507626,
-6.41884336375736));
#74705=CARTESIAN_POINT('Ctrl Pts',(-20.1496786628018,-17.37791609424,-6.41969617205793));
#74706=CARTESIAN_POINT('Ctrl Pts',(-20.1329049466645,-17.3630304525861,
-6.42105106458451));
#74707=CARTESIAN_POINT('Ctrl Pts',(-20.1266019391698,-17.3575034918229,
-6.42155594954601));
#74708=CARTESIAN_POINT('Ctrl Pts',(-20.1153950607495,-17.3477935835852,
-6.42244625021074));
#74709=CARTESIAN_POINT('Ctrl Pts',(-20.1105046349862,-17.3435953458113,
-6.42283229861664));
#74710=CARTESIAN_POINT('Ctrl Pts',(-20.100317802618,-17.3349308426697,-6.42363140074097));
#74711=CARTESIAN_POINT('Ctrl Pts',(-20.0950184851612,-17.3304681063441,
-6.4240443065721));
#74712=CARTESIAN_POINT('Ctrl Pts',(-20.0812910654333,-17.3190224817341,
-6.42510678284943));
#74713=CARTESIAN_POINT('Ctrl Pts',(-20.0728304798146,-17.3120787386936,
-6.42575475548946));
#74714=CARTESIAN_POINT('Ctrl Pts',(-20.0366931800307,-17.2828863273493,
-6.42849395872503));
#74715=CARTESIAN_POINT('Ctrl Pts',(-20.0085118961594,-17.2612695018461,
-6.43055985079432));
#74716=CARTESIAN_POINT('Ctrl Pts',(-19.9330683713103,-17.2063583904643,
-6.43592265549204));
#74717=CARTESIAN_POINT('Ctrl Pts',(-19.8849624544593,-17.1742723086868,
-6.43917563760426));
#74718=CARTESIAN_POINT('Ctrl Pts',(-19.6972068262767,-17.0598619808836,
-6.45137513556485));
#74719=CARTESIAN_POINT('Ctrl Pts',(-19.549598372377,-16.9917072816964,-6.45992615368772));
#74720=CARTESIAN_POINT('Ctrl Pts',(-19.3750799293361,-16.9342846186329,
-6.47018693705132));
#74721=CARTESIAN_POINT('Ctrl Pts',(-19.3543878741379,-16.9278266698602,
-6.47140655612698));
#74722=CARTESIAN_POINT('Ctrl Pts',(-19.2933234967709,-16.9097928647942,
-6.47502422703232));
#74723=CARTESIAN_POINT('Ctrl Pts',(-19.2527040405183,-16.8991000156803,
-6.4774541115432));
#74724=CARTESIAN_POINT('Ctrl Pts',(-19.2045513088841,-16.8879443372843,
-6.48039070956155));
#74725=CARTESIAN_POINT('Ctrl Pts',(-19.1972972546151,-16.8863040002784,
-6.48083458362917));
#74726=CARTESIAN_POINT('Ctrl Pts',(-19.1855410114021,-16.8837106362707,
-6.481556568));
#74727=CARTESIAN_POINT('Ctrl Pts',(-19.1810440223166,-16.8827339904478,
-6.48183336043624));
#74728=CARTESIAN_POINT('Ctrl Pts',(-19.173048981748,-16.8810249242269,-6.48232661751927));
#74729=CARTESIAN_POINT('Ctrl Pts',(-19.16955222348,-16.8802866913469,-6.48254274612517));
#74730=CARTESIAN_POINT('Ctrl Pts',(-19.1620433867143,-16.8787212827171,
-6.48300771786059));
#74731=CARTESIAN_POINT('Ctrl Pts',(-19.1580308316259,-16.8778969086322,
-6.48325671146392));
#74732=CARTESIAN_POINT('Ctrl Pts',(-19.1469794989126,-16.8756598366607,
-6.48394387745948));
#74733=CARTESIAN_POINT('Ctrl Pts',(-19.1399359648255,-16.8742713051324,
-6.48438339157216));
#74734=CARTESIAN_POINT('Ctrl Pts',(-19.10181476387,-16.866957498513,-6.48677001261174));
#74735=CARTESIAN_POINT('Ctrl Pts',(-19.0706160601182,-16.8616939666992,
-6.48875145077311));
#74736=CARTESIAN_POINT('Ctrl Pts',(-18.8775506369572,-16.8335559602815,
-6.50113860295273));
#74737=CARTESIAN_POINT('Ctrl Pts',(-18.7136066526049,-16.8287958513289,
-6.51214893227153));
#74738=CARTESIAN_POINT('Ctrl Pts',(-18.4341379738477,-16.8530782226375,
-6.53047402769161));
#74739=CARTESIAN_POINT('Ctrl Pts',(-18.3185533953526,-16.8728651239564,
-6.53793080217616));
#74740=CARTESIAN_POINT('Ctrl Pts',(-18.1913415586007,-16.9056825537609,
-6.54595268826156));
#74741=CARTESIAN_POINT('Ctrl Pts',(-18.1775384319861,-16.9093928880337,
-6.54682085688366));
#74742=CARTESIAN_POINT('Ctrl Pts',(-18.1556307548697,-16.9155203142669,
-6.54819541176844));
#74743=CARTESIAN_POINT('Ctrl Pts',(-18.1475014691584,-16.9178466206608,
-6.54870472773245));
#74744=CARTESIAN_POINT('Ctrl Pts',(-18.1331893056846,-16.9220351725402,
-6.54960017024048));
#74745=CARTESIAN_POINT('Ctrl Pts',(-18.1270006426208,-16.9238771061146,
-6.54998695320867));
#74746=CARTESIAN_POINT('Ctrl Pts',(-18.1142184373658,-16.927745225341,-6.55078500960992));
#74747=CARTESIAN_POINT('Ctrl Pts',(-18.1076261696227,-16.9297753822928,
-6.55119614781788));
#74748=CARTESIAN_POINT('Ctrl Pts',(-18.0907312520088,-16.9350688885102,
-6.55224873715808));
#74749=CARTESIAN_POINT('Ctrl Pts',(-18.0804433745375,-16.9383789992883,
-6.55288864768084));
#74750=CARTESIAN_POINT('Ctrl Pts',(-18.0376200282087,-16.9525201241054,
-6.55554835816367));
#74751=CARTESIAN_POINT('Ctrl Pts',(-18.0053237106633,-16.9640624001404,
-6.55754465093477));
#74752=CARTESIAN_POINT('Ctrl Pts',(-17.9219260024534,-16.9961733659085,
-6.56268609096014));
#74753=CARTESIAN_POINT('Ctrl Pts',(-17.8713207952001,-17.017960901597,-6.56579190216776));
#74754=CARTESIAN_POINT('Ctrl Pts',(-17.7229741070182,-17.0888128347816,
-6.57493326333654));
#74755=CARTESIAN_POINT('Ctrl Pts',(-17.6281231247613,-17.1434986888472,
-6.5808200738016));
#74756=CARTESIAN_POINT('Ctrl Pts',(-17.5024553388562,-17.2295499260154,
-6.58911213608491));
#74757=CARTESIAN_POINT('Ctrl Pts',(-17.4677390864689,-17.2549084825652,
-6.59146172692335));
#74758=CARTESIAN_POINT('Ctrl Pts',(-17.3741943210367,-17.3277075793914,
-6.59802361195137));
#74759=CARTESIAN_POINT('Ctrl Pts',(-17.3171021846353,-17.3772633997974,
-6.60229272212173));
#74760=CARTESIAN_POINT('Ctrl Pts',(-17.2559606255376,-17.4363553393903,
-6.60733217674834));
#74761=CARTESIAN_POINT('Ctrl Pts',(-17.2491787461259,-17.4429986858368,
-6.60789806543709));
#74762=CARTESIAN_POINT('Ctrl Pts',(-17.2391916072032,-17.4529143295949,
-6.60874213335978));
#74763=CARTESIAN_POINT('Ctrl Pts',(-17.2359518077676,-17.4561518822973,
-6.6090176424153));
#74764=CARTESIAN_POINT('Ctrl Pts',(-17.2302042609199,-17.4619328428253,
-6.60950949241245));
#74765=CARTESIAN_POINT('Ctrl Pts',(-17.227692418761,-17.4644721084171,-6.60972550458597));
#74766=CARTESIAN_POINT('Ctrl Pts',(-17.2223036025189,-17.4699474035801,
-6.61019123021394));
#74767=CARTESIAN_POINT('Ctrl Pts',(-17.2194287921008,-17.4728854161186,
-6.61044109942881));
#74768=CARTESIAN_POINT('Ctrl Pts',(-17.211511719523,-17.481023825935,-6.61113309750282));
#74769=CARTESIAN_POINT('Ctrl Pts',(-17.2064876187868,-17.4862417011649,
-6.61157659884844));
#74770=CARTESIAN_POINT('Ctrl Pts',(-17.1790233510643,-17.5150597938577,
-6.6140245931114));
#74771=CARTESIAN_POINT('Ctrl Pts',(-17.1571045790015,-17.5391482398456,
-6.61606549334081));
#74772=CARTESIAN_POINT('Ctrl Pts',(-17.029071351026,-17.686546842809,-6.62847213283241));
#74773=CARTESIAN_POINT('Ctrl Pts',(-16.9369055296477,-17.821245919886,-6.63942730611795));
#74774=CARTESIAN_POINT('Ctrl Pts',(-16.8066268614934,-18.0685044158201,
-6.65768272269842));
#74775=CARTESIAN_POINT('Ctrl Pts',(-16.7608186248174,-18.1761812535905,
-6.66512290945199));
#74776=CARTESIAN_POINT('Ctrl Pts',(-16.7196357938293,-18.3006705698452,
-6.67312935843537));
#74777=CARTESIAN_POINT('Ctrl Pts',(-16.7152852999757,-18.314282070732,-6.67399732649369));
#74778=CARTESIAN_POINT('Ctrl Pts',(-16.7085806033823,-18.3360156284829,
-6.67537162484848));
#74779=CARTESIAN_POINT('Ctrl Pts',(-16.7061367276736,-18.344109360051,-6.67588088314543));
#74780=CARTESIAN_POINT('Ctrl Pts',(-16.7019120785144,-18.3584097638266,
-6.67677625857528));
#74781=CARTESIAN_POINT('Ctrl Pts',(-16.7001111039519,-18.364610309,-6.67716303182294));
#74782=CARTESIAN_POINT('Ctrl Pts',(-16.6964447786512,-18.3774520878494,
-6.67796110101941));
#74783=CARTESIAN_POINT('Ctrl Pts',(-16.6945834619512,-18.3840944009193,
-6.67837226158113));
#74784=CARTESIAN_POINT('Ctrl Pts',(-16.6898890442752,-18.4011676942213,
-6.67942497614906));
#74785=CARTESIAN_POINT('Ctrl Pts',(-16.6871032805823,-18.4116115702577,
-6.68006498882599));
#74786=CARTESIAN_POINT('Ctrl Pts',(-16.6758102423518,-18.4552900204834,
-6.68272569202054));
#74787=CARTESIAN_POINT('Ctrl Pts',(-16.6680311666412,-18.4887086678556,
-6.68472285294477));
#74788=CARTESIAN_POINT('Ctrl Pts',(-16.6498822315711,-18.5762622847695,
-6.68986703424781));
#74789=CARTESIAN_POINT('Ctrl Pts',(-16.6408076643616,-18.6306400852839,
-6.69297466354843));
#74790=CARTESIAN_POINT('Ctrl Pts',(-16.6200900399427,-18.7937895408449,
-6.70211919669863));
#74791=CARTESIAN_POINT('Ctrl Pts',(-16.6147400615673,-18.9031731072094,
-6.70800737156691));
#74792=CARTESIAN_POINT('Ctrl Pts',(-16.6191735951262,-19.0582981501148,
-6.71645648286419));
#74793=CARTESIAN_POINT('Ctrl Pts',(-16.6219707858252,-19.1040604441326,
-6.71896277593144));
#74794=CARTESIAN_POINT('Ctrl Pts',(-16.6283556179594,-19.1721332981296,
-6.72275427608508));
#74795=CARTESIAN_POINT('Ctrl Pts',(-16.6308183899938,-19.1945365906223,
-6.72401242111201));
#74796=CARTESIAN_POINT('Ctrl Pts',(-16.6344001338201,-19.2229362854735,
-6.72562505655993));
#74797=CARTESIAN_POINT('Ctrl Pts',(-16.6351880138896,-19.2289734908284,
-6.72596889247919));
#74798=CARTESIAN_POINT('Ctrl Pts',(-16.6421026002959,-19.2802329316424,
-6.72889756666278));
#74799=CARTESIAN_POINT('Ctrl Pts',(-16.6496635822766,-19.3252460583367,
-6.73153084884893));
#74800=CARTESIAN_POINT('Ctrl Pts',(-16.6601768009813,-19.3774461257432,
-6.73469309994365));
#74801=CARTESIAN_POINT('Ctrl Pts',(-16.6617216040197,-19.384907972089,-6.73514774646076));
#74802=CARTESIAN_POINT('Ctrl Pts',(-16.6642649460114,-19.3968674306772,
-6.73588086185389));
#74803=CARTESIAN_POINT('Ctrl Pts',(-16.6652379567274,-19.4013704841021,
-6.73615790999352));
#74804=CARTESIAN_POINT('Ctrl Pts',(-16.6669938388295,-19.409370056143,-6.73665193556535));
#74805=CARTESIAN_POINT('Ctrl Pts',(-16.6677708968192,-19.4128678026972,
-6.73686857783967));
#74806=CARTESIAN_POINT('Ctrl Pts',(-16.6694442848269,-19.4203108661067,
-6.73733095349621));
#74807=CARTESIAN_POINT('Ctrl Pts',(-16.67034303185,-19.4242555299196,-6.7375768182143));
#74808=CARTESIAN_POINT('Ctrl Pts',(-16.6728164511585,-19.4349696506205,
-6.73824678468645));
#74809=CARTESIAN_POINT('Ctrl Pts',(-16.6744131455428,-19.4417338984473,
-6.73867212111415));
#74810=CARTESIAN_POINT('Ctrl Pts',(-16.6827429505346,-19.4762610347788,
-6.74085483072734));
#74811=CARTESIAN_POINT('Ctrl Pts',(-16.690003879291,-19.5038920072432,-6.74264009147455));
#74812=CARTESIAN_POINT('Ctrl Pts',(-16.7130202464255,-19.5847829142683,
-6.74796360774868));
#74813=CARTESIAN_POINT('Ctrl Pts',(-16.7303144179089,-19.6375775834551,
-6.75156300851509));
#74814=CARTESIAN_POINT('Ctrl Pts',(-16.7982331468631,-19.8202899871938,
-6.76433115205645));
#74815=CARTESIAN_POINT('Ctrl Pts',(-16.8595957319666,-19.9458482870958,
-6.77364484468825));
#74816=CARTESIAN_POINT('Ctrl Pts',(-16.9801585301175,-20.1410464608048,
-6.78845579730063));
#74817=CARTESIAN_POINT('Ctrl Pts',(-17.0323003627838,-20.2145424454453,
-6.79412862371263));
#74818=CARTESIAN_POINT('Ctrl Pts',(-17.0976038733076,-20.2951622599452,
-6.80045885254198));
#74819=CARTESIAN_POINT('Ctrl Pts',(-17.1063409359772,-20.3057367266937,
-6.80129157022892));
#74820=CARTESIAN_POINT('Ctrl Pts',(-17.1205207373237,-20.3225627848582,
-6.80262069699413));
#74821=CARTESIAN_POINT('Ctrl Pts',(-17.1258983778,-20.3288684955553,-6.80311974208911));
#74822=CARTESIAN_POINT('Ctrl Pts',(-17.1355143198483,-20.3400107641331,
-6.80400330668057));
#74823=CARTESIAN_POINT('Ctrl Pts',(-17.1397378667413,-20.3448598647644,
-6.80438842776142));
#74824=CARTESIAN_POINT('Ctrl Pts',(-17.1485857338772,-20.3549252283744,
-6.80518911371549));
#74825=CARTESIAN_POINT('Ctrl Pts',(-17.1532138612621,-20.3601380532445,
-6.80560451329396));
#74826=CARTESIAN_POINT('Ctrl Pts',(-17.1653039699175,-20.3736208479004,
-6.80668089360052));
#74827=CARTESIAN_POINT('Ctrl Pts',(-17.1728056838422,-20.3818550221435,
-6.80734019483284));
#74828=CARTESIAN_POINT('Ctrl Pts',(-17.2057051598498,-20.4173991707385,
-6.81019518318211));
#74829=CARTESIAN_POINT('Ctrl Pts',(-17.2317580123588,-20.4440955428683,
-6.81236272837021));
#74830=CARTESIAN_POINT('Ctrl Pts',(-17.3028866992972,-20.5132284937725,
-6.81805484253141));
#74831=CARTESIAN_POINT('Ctrl Pts',(-17.3491420227038,-20.5544009904482,
-6.82152807009403));
#74832=CARTESIAN_POINT('Ctrl Pts',(-17.5072090051151,-20.6831338878177,
-6.83280485535002));
#74833=CARTESIAN_POINT('Ctrl Pts',(-17.6260116162018,-20.7614750704277,
-6.84034767604244));
#74834=CARTESIAN_POINT('Ctrl Pts',(-17.8186314866175,-20.8623635136665,
-6.85238551067464));
#74835=CARTESIAN_POINT('Ctrl Pts',(-17.8873256450474,-20.8937848073749,
-6.85665147002291));
#74836=CARTESIAN_POINT('Ctrl Pts',(-17.9663619226266,-20.9249446671622,
-6.86168670128342));
#74837=CARTESIAN_POINT('Ctrl Pts',(-17.9752046884064,-20.9283624528559,
-6.8622518079189));
#74838=CARTESIAN_POINT('Ctrl Pts',(-17.9883506908276,-20.9333422375274,
-6.86309493026967));
#74839=CARTESIAN_POINT('Ctrl Pts',(-17.9926366590347,-20.9349499111801,
-6.86337028448628));
#74840=CARTESIAN_POINT('Ctrl Pts',(-18.0002758518047,-20.9377871563594,
-6.86386196523651));
#74841=CARTESIAN_POINT('Ctrl Pts',(-18.0036270065953,-20.9390221554576,
-6.86407796387979));
#74842=CARTESIAN_POINT('Ctrl Pts',(-18.0108435161693,-20.9416609286274,
-6.86454378281918));
#74843=CARTESIAN_POINT('Ctrl Pts',(-18.0147097841405,-20.9430619015281,
-6.86479375952265));
#74844=CARTESIAN_POINT('Ctrl Pts',(-18.0254049015843,-20.9469021454816,
-6.86548635139786));
#74845=CARTESIAN_POINT('Ctrl Pts',(-18.0322421646884,-20.9493175813126,
-6.86593034285788));
#74846=CARTESIAN_POINT('Ctrl Pts',(-18.0699627717014,-20.9624257455144,
-6.86838601277451));
#74847=CARTESIAN_POINT('Ctrl Pts',(-18.1010763267448,-20.9724367028159,
-6.8704343626453));
#74848=CARTESIAN_POINT('Ctrl Pts',(-18.2882853699942,-21.0279239049622,
-6.88284352534821));
#74849=CARTESIAN_POINT('Ctrl Pts',(-18.44896241195,-21.0560140477838,-6.89379189706699));
#74850=CARTESIAN_POINT('Ctrl Pts',(-18.7278429650211,-21.0722090017009,
-6.91203860527139));
#74851=CARTESIAN_POINT('Ctrl Pts',(-18.8447906932749,-21.0693231544684,
-6.91947663997359));
#74852=CARTESIAN_POINT('Ctrl Pts',(-18.9751271092756,-21.0552714723962,
-6.92748108555126));
#74853=CARTESIAN_POINT('Ctrl Pts',(-18.9893179661189,-21.0535960414207,
-6.9283490271902));
#74854=CARTESIAN_POINT('Ctrl Pts',(-19.0118766208041,-21.0507008027958,
-6.92972329175296));
#74855=CARTESIAN_POINT('Ctrl Pts',(-19.0202557616169,-21.0495743415254,
-6.93023254245332));
#74856=CARTESIAN_POINT('Ctrl Pts',(-19.0350218816356,-21.0474991089574,
-6.93112790904712));
#74857=CARTESIAN_POINT('Ctrl Pts',(-19.0414116473184,-21.0465712614734,
-6.93151468101459));
#74858=CARTESIAN_POINT('Ctrl Pts',(-19.0546190451169,-21.0445916973954,
-6.93231275189821));
#74859=CARTESIAN_POINT('Ctrl Pts',(-19.0614359894512,-21.04353586119,-6.93272391540586));
#74860=CARTESIAN_POINT('Ctrl Pts',(-19.078921087689,-21.0407401170678,-6.93377664647683));
#74861=CARTESIAN_POINT('Ctrl Pts',(-19.0895813806296,-21.038951777519,-6.93441667261602));
#74862=CARTESIAN_POINT('Ctrl Pts',(-19.1340181229977,-21.0311468252706,
-6.93707750666116));
#74863=CARTESIAN_POINT('Ctrl Pts',(-19.1676606140742,-21.0243910558106,
-6.93907478201967));
#74864=CARTESIAN_POINT('Ctrl Pts',(-19.2548778709147,-21.0046598440315,
-6.94421932469722));
#74865=CARTESIAN_POINT('Ctrl Pts',(-19.3081373223509,-20.9904045654281,
-6.94732719367996));
#74866=CARTESIAN_POINT('Ctrl Pts',(-19.4635933629355,-20.9422181057136,
-6.95637679664332));
#74867=CARTESIAN_POINT('Ctrl Pts',(-19.5638266130352,-20.9025546091438,
-6.96217621955508));
#74868=CARTESIAN_POINT('Ctrl Pts',(-19.7686877885259,-20.8028267082135,
-6.97457694609246));
#74869=CARTESIAN_POINT('Ctrl Pts',(-19.8720744085514,-20.7411105447019,
-6.98117295068701));
#74870=CARTESIAN_POINT('Ctrl Pts',(-19.9773653041375,-20.6654240535901,
-6.98885801498727));
#74871=CARTESIAN_POINT('Ctrl Pts',(-19.985042292683,-20.6598268182876,-6.98942432887112));
#74872=CARTESIAN_POINT('Ctrl Pts',(-19.9963650565162,-20.6514541639817,
-6.99026891085024));
#74873=CARTESIAN_POINT('Ctrl Pts',(-20.0000400377689,-20.6487181891077,
-6.99054450404216));
#74874=CARTESIAN_POINT('Ctrl Pts',(-20.0064391953981,-20.643921736002,-6.99102701716286));
#74875=CARTESIAN_POINT('Ctrl Pts',(-20.0091673014988,-20.6418665686252,
-6.99123356436192));
#74876=CARTESIAN_POINT('Ctrl Pts',(-20.0150562182121,-20.6374078832479,
-6.99168125696093));
#74877=CARTESIAN_POINT('Ctrl Pts',(-20.0182151964123,-20.6350021080908,
-6.9919225576278));
#74878=CARTESIAN_POINT('Ctrl Pts',(-20.0266049605384,-20.6285753623349,
-6.99256642937428));
#74879=CARTESIAN_POINT('Ctrl Pts',(-20.0318236998357,-20.6245388399348,
-6.99297007424193));
#74880=CARTESIAN_POINT('Ctrl Pts',(-20.0434209072886,-20.6154818237276,
-6.99387391430647));
#74881=CARTESIAN_POINT('Ctrl Pts',(-20.0497895078531,-20.6104489309782,
-6.99437492431482));
#74882=CARTESIAN_POINT('Ctrl Pts',(-20.0690124349333,-20.5950772723018,
-6.99590097655186));
#74883=CARTESIAN_POINT('Ctrl Pts',(-20.0817747057316,-20.5846250124554,
-6.99693302824633));
#74884=CARTESIAN_POINT('Ctrl Pts',(-20.1289520063921,-20.5450568080324,
-7.00081521503053));
#74885=CARTESIAN_POINT('Ctrl Pts',(-20.1625547210036,-20.5149945565157,
-7.00371569066448));
#74886=CARTESIAN_POINT('Ctrl Pts',(-20.2500895844626,-20.4315004725714,
-7.01158889597075));
#74887=CARTESIAN_POINT('Ctrl Pts',(-20.3021508636173,-20.3762020752341,
-7.01661527365881));
#74888=CARTESIAN_POINT('Ctrl Pts',(-20.4510455466623,-20.199963809805,-7.03185549933659));
#74889=CARTESIAN_POINT('Ctrl Pts',(-20.5377040853262,-20.0710742049076,
-7.0419423529683));
#74890=CARTESIAN_POINT('Ctrl Pts',(-20.6206410394289,-19.9126497532631,
-7.0529593810999));
#74891=CARTESIAN_POINT('Ctrl Pts',(-20.6313863131782,-19.8912484296231,
-7.05442203207489));
#74892=CARTESIAN_POINT('Ctrl Pts',(-20.6459733677997,-19.8609230029996,
-7.05645965424622));
#74893=CARTESIAN_POINT('Ctrl Pts',(-20.6501200623779,-19.8521483744456,
-7.0570451925395));
#74894=CARTESIAN_POINT('Ctrl Pts',(-20.6567308342652,-19.8379069304022,
-7.05798909874007));
#74895=CARTESIAN_POINT('Ctrl Pts',(-20.6592322466665,-19.8324576922908,
-7.05834875421579));
#74896=CARTESIAN_POINT('Ctrl Pts',(-20.6643974319548,-19.8210782565451,
-7.05909669053979));
#74897=CARTESIAN_POINT('Ctrl Pts',(-20.6670571110406,-19.8151462611903,
-7.05948482743104));
#74898=CARTESIAN_POINT('Ctrl Pts',(-20.6732798529584,-19.8010943865385,
-7.06040016366369));
#74899=CARTESIAN_POINT('Ctrl Pts',(-20.6768193260813,-19.7929641461986,
-7.06092655095774));
#74900=CARTESIAN_POINT('Ctrl Pts',(-20.6883950565319,-19.7659112964969,
-7.06266762262549));
#74901=CARTESIAN_POINT('Ctrl Pts',(-20.6962069166949,-19.7468935120836,
-7.06387468139385));
#74902=CARTESIAN_POINT('Ctrl Pts',(-20.7102289848657,-19.7112901289879,
-7.06610478058572));
#74903=CARTESIAN_POINT('Ctrl Pts',(-20.7165093627717,-19.6947374676077,
-7.06712985185229));
#74904=CARTESIAN_POINT('Ctrl Pts',(-20.7225805740154,-19.678110391503,-7.06814851970791));
#74905=CARTESIAN_POINT('Ctrl Pts',(-20.7225805835101,-19.6781103655001,
-6.84500601987795));
#74906=CARTESIAN_POINT('Ctrl Pts',(-20.7143219854172,-19.7007279847972,
-6.84341664278283));
#74907=CARTESIAN_POINT('Ctrl Pts',(-20.7056776273264,-19.7232044037876,
-6.84182487853371));
#74908=CARTESIAN_POINT('Ctrl Pts',(-20.6822899566468,-19.7810495426352,
-6.83770203086913));
#74909=CARTESIAN_POINT('Ctrl Pts',(-20.6669669703437,-19.8161734031987,
-6.83517286881883));
#74910=CARTESIAN_POINT('Ctrl Pts',(-20.6103476751077,-19.9369061608838,
-6.82641399128989));
#74911=CARTESIAN_POINT('Ctrl Pts',(-20.5642445701084,-20.0201428700487,
-6.82026486865833));
#74912=CARTESIAN_POINT('Ctrl Pts',(-20.4876288281751,-20.1388496640421,
-6.81139907214313));
#74913=CARTESIAN_POINT('Ctrl Pts',(-20.4612923602198,-20.176862367634,-6.80854270242055));
#74914=CARTESIAN_POINT('Ctrl Pts',(-20.4265842288022,-20.2236097438781,
-6.80500499427594));
#74915=CARTESIAN_POINT('Ctrl Pts',(-20.4193562061972,-20.2331741410964,
-6.80427979467784));
#74916=CARTESIAN_POINT('Ctrl Pts',(-20.4076825967969,-20.2483513473345,
-6.80312662672716));
#74917=CARTESIAN_POINT('Ctrl Pts',(-20.4032891848287,-20.2540037902906,
-6.80269661531298));
#74918=CARTESIAN_POINT('Ctrl Pts',(-20.3949230715704,-20.2646554468028,
-6.8018852212007));
#74919=CARTESIAN_POINT('Ctrl Pts',(-20.3909562691669,-20.269659172603,-6.80150361041117));
#74920=CARTESIAN_POINT('Ctrl Pts',(-20.3819261606153,-20.2809444918424,
-6.80064186669378));
#74921=CARTESIAN_POINT('Ctrl Pts',(-20.3768494431342,-20.2872152647369,
-6.80016227846972));
#74922=CARTESIAN_POINT('Ctrl Pts',(-20.3617613838255,-20.3056357385139,
-6.79875112185494));
#74923=CARTESIAN_POINT('Ctrl Pts',(-20.3516500886938,-20.3177031323707,
-6.79782360748397));
#74924=CARTESIAN_POINT('Ctrl Pts',(-20.2603445454015,-20.4242354505289,
-6.78960465912225));
#74925=CARTESIAN_POINT('Ctrl Pts',(-20.1710907798022,-20.5114810019239,
-6.78267611821987));
#74926=CARTESIAN_POINT('Ctrl Pts',(-19.9449935097697,-20.696494222655,-6.76672054894049));
#74927=CARTESIAN_POINT('Ctrl Pts',(-19.8031955937225,-20.786821706128,-6.75786063141456));
#74928=CARTESIAN_POINT('Ctrl Pts',(-19.6328541194331,-20.8688239755822,
-6.74686258294512));
#74929=CARTESIAN_POINT('Ctrl Pts',(-19.6133072136024,-20.8778690569118,
-6.74559506334164));
#74930=CARTESIAN_POINT('Ctrl Pts',(-19.5878766232969,-20.8891688883436,
-6.74393470548453));
#74931=CARTESIAN_POINT('Ctrl Pts',(-19.582115381972,-20.8916981431034,-6.74355781304137));
#74932=CARTESIAN_POINT('Ctrl Pts',(-19.5732577041436,-20.895539764418,-6.7429770922349));
#74933=CARTESIAN_POINT('Ctrl Pts',(-19.5701692144989,-20.8968705237624,
-6.74277437202766));
#74934=CARTESIAN_POINT('Ctrl Pts',(-19.5637954373323,-20.8995988495023,
-6.74235550462217));
#74935=CARTESIAN_POINT('Ctrl Pts',(-19.5605098099,-20.900995454047,-6.74213929977439));
#74936=CARTESIAN_POINT('Ctrl Pts',(-19.5530170090569,-20.9041580258165,
-6.74164561503926));
#74937=CARTESIAN_POINT('Ctrl Pts',(-19.5488076657731,-20.9059186998903,
-6.74136781969645));
#74938=CARTESIAN_POINT('Ctrl Pts',(-19.5378417976435,-20.9104638798799,
-6.74064301992948));
#74939=CARTESIAN_POINT('Ctrl Pts',(-19.5310765541438,-20.9132270056576,
-6.7401947735487));
#74940=CARTESIAN_POINT('Ctrl Pts',(-19.4877712048934,-20.9306531170134,
-6.7373191550399));
#74941=CARTESIAN_POINT('Ctrl Pts',(-19.4508448173797,-20.9443283463676,
-6.73483853185894));
#74942=CARTESIAN_POINT('Ctrl Pts',(-19.2327777342574,-21.0182398563808,
-6.72011012947499));
#74943=CARTESIAN_POINT('Ctrl Pts',(-19.0445337523876,-21.054785395015,-6.70717973171493));
#74944=CARTESIAN_POINT('Ctrl Pts',(-18.7989193959445,-21.0687214835421,
-6.69136696687255));
#74945=CARTESIAN_POINT('Ctrl Pts',(-18.7438094961671,-21.0696942558855,
-6.68787822026557));
#74946=CARTESIAN_POINT('Ctrl Pts',(-18.6544278808095,-21.0677820774067,
-6.682321199515));
#74947=CARTESIAN_POINT('Ctrl Pts',(-18.6201567100273,-21.066215089064,-6.6802144960893));
#74948=CARTESIAN_POINT('Ctrl Pts',(-18.57515544615,-21.0630599762427,-6.67747814418383));
#74949=CARTESIAN_POINT('Ctrl Pts',(-18.5643795816716,-21.0622214898092,
-6.67682515815192));
#74950=CARTESIAN_POINT('Ctrl Pts',(-18.5467375972623,-21.0607127291629,
-6.67575968085642));
#74951=CARTESIAN_POINT('Ctrl Pts',(-18.5398675938761,-21.0600913624076,
-6.67534566027352));
#74952=CARTESIAN_POINT('Ctrl Pts',(-18.5265730905179,-21.0588233829699,
-6.6745461476453));
#74953=CARTESIAN_POINT('Ctrl Pts',(-18.5201482788146,-21.0581809353846,
-6.67416052928455));
#74954=CARTESIAN_POINT('Ctrl Pts',(-18.5053175481295,-21.0566293782444,
-6.67327209800026));
#74955=CARTESIAN_POINT('Ctrl Pts',(-18.4969138991525,-21.0556992816254,
-6.67276995119458));
#74956=CARTESIAN_POINT('Ctrl Pts',(-18.4743220287201,-21.0530617707871,
-6.67142329969202));
#74957=CARTESIAN_POINT('Ctrl Pts',(-18.4601449959225,-21.0512609806989,
-6.67058173668987));
#74958=CARTESIAN_POINT('Ctrl Pts',(-18.3301963150198,-21.0334158426373,
-6.6628974703257));
#74959=CARTESIAN_POINT('Ctrl Pts',(-18.2159141693931,-21.0079527390782,
-6.65637169077549));
#74960=CARTESIAN_POINT('Ctrl Pts',(-17.9487676730689,-20.9247238206964,
-6.64105377620314));
#74961=CARTESIAN_POINT('Ctrl Pts',(-17.799362609964,-20.8584810782739,-6.63244520774425));
#74962=CARTESIAN_POINT('Ctrl Pts',(-17.6312115529206,-20.7593712013123,
-6.62123549888504));
#74963=CARTESIAN_POINT('Ctrl Pts',(-17.6037566214886,-20.7423303233863,
-6.61935066406941));
#74964=CARTESIAN_POINT('Ctrl Pts',(-17.5706533514501,-20.7207186864475,
-6.61699673764266));
#74965=CARTESIAN_POINT('Ctrl Pts',(-17.5646229467832,-20.7167375216916,
-6.61656454944253));
#74966=CARTESIAN_POINT('Ctrl Pts',(-17.5551975453834,-20.7104455175486,
-6.61588354107986));
#74967=CARTESIAN_POINT('Ctrl Pts',(-17.5517886243604,-20.7081554964885,
-6.61563610011723));
#74968=CARTESIAN_POINT('Ctrl Pts',(-17.5454268423729,-20.703854905758,-6.61517214672524));
#74969=CARTESIAN_POINT('Ctrl Pts',(-17.5424723998708,-20.7018467759582,
-6.61495579855911));
#74970=CARTESIAN_POINT('Ctrl Pts',(-17.5357367750153,-20.6972436148394,
-6.61446054399009));
#74971=CARTESIAN_POINT('Ctrl Pts',(-17.5319589462618,-20.694643777627,-6.61418131417358));
#74972=CARTESIAN_POINT('Ctrl Pts',(-17.520362212717,-20.6866074519778,-6.61331975655933));
#74973=CARTESIAN_POINT('Ctrl Pts',(-17.5125716462733,-20.6811305503357,
-6.61273477479369));
#74974=CARTESIAN_POINT('Ctrl Pts',(-17.4083391333826,-20.6067974239799,
-6.60482735084867));
#74975=CARTESIAN_POINT('Ctrl Pts',(-17.317818016391,-20.5300219586709,-6.59703648355805));
#74976=CARTESIAN_POINT('Ctrl Pts',(-17.1570251419339,-20.36861511464,-6.58198658575987));
#74977=CARTESIAN_POINT('Ctrl Pts',(-17.0859583110822,-20.2852704691975,
-6.57475560850043));
#74978=CARTESIAN_POINT('Ctrl Pts',(-16.9892643541347,-20.1522580379777,
-6.56418578683252));
#74979=CARTESIAN_POINT('Ctrl Pts',(-16.9586308567259,-20.1064639693811,
-6.56069855252346));
#74980=CARTESIAN_POINT('Ctrl Pts',(-16.9118770017224,-20.0303007865398,
-6.55514365851298));
#74981=CARTESIAN_POINT('Ctrl Pts',(-16.8946498109096,-20.000644794519,-6.55303760619089));
#74982=CARTESIAN_POINT('Ctrl Pts',(-16.8729501547281,-19.9611081523475,
-6.55030196344546));
#74983=CARTESIAN_POINT('Ctrl Pts',(-16.8678230108253,-19.9515945385897,
-6.54964905059574));
#74984=CARTESIAN_POINT('Ctrl Pts',(-16.8595430786369,-19.935945032989,-6.54858366210338));
#74985=CARTESIAN_POINT('Ctrl Pts',(-16.8563470787238,-19.9298323409278,
-6.54816965763335));
#74986=CARTESIAN_POINT('Ctrl Pts',(-16.8502172749656,-19.9179675646923,
-6.54737015497548));
#74987=CARTESIAN_POINT('Ctrl Pts',(-16.8472798033342,-19.9122174712506,
-6.54698453058293));
#74988=CARTESIAN_POINT('Ctrl Pts',(-16.8405565056246,-19.898906662827,-6.54609605518229));
#74989=CARTESIAN_POINT('Ctrl Pts',(-16.8367895611247,-19.8913364936408,
-6.54559387050442));
#74990=CARTESIAN_POINT('Ctrl Pts',(-16.8267775234656,-19.8709100620896,
-6.54424705036412));
#74991=CARTESIAN_POINT('Ctrl Pts',(-16.8206170346202,-19.858012648875,-6.54340535776289));
#74992=CARTESIAN_POINT('Ctrl Pts',(-16.7652105321332,-19.7389291661411,
-6.53571092690519));
#74993=CARTESIAN_POINT('Ctrl Pts',(-16.7247165888992,-19.6288862082935,
-6.52917611752084));
#74994=CARTESIAN_POINT('Ctrl Pts',(-16.649971561305,-19.3584910897564,-6.51381941340986));
#74995=CARTESIAN_POINT('Ctrl Pts',(-16.6248187145037,-19.1964415528838,
-6.50518270586816));
#74996=CARTESIAN_POINT('Ctrl Pts',(-16.6173417152226,-19.0014918697698,
-6.49397028877299));
#74997=CARTESIAN_POINT('Ctrl Pts',(-16.6168382986956,-18.9698277186779,
-6.4921221548721));
#74998=CARTESIAN_POINT('Ctrl Pts',(-16.6170921265095,-18.9309851370272,
-6.48980907832235));
#74999=CARTESIAN_POINT('Ctrl Pts',(-16.6171755905183,-18.9238045150507,
-6.48937954428305));
#75000=CARTESIAN_POINT('Ctrl Pts',(-16.6173640441411,-18.9125283082934,
-6.48870179743376));
#75001=CARTESIAN_POINT('Ctrl Pts',(-16.6174443928772,-18.9084322896644,
-6.48845494207859));
#75002=CARTESIAN_POINT('Ctrl Pts',(-16.6176170939468,-18.9007636118522,
-6.48799147988173));
#75003=CARTESIAN_POINT('Ctrl Pts',(-16.6177066036871,-18.8971909445545,
-6.48777503361597));
#75004=CARTESIAN_POINT('Ctrl Pts',(-16.6179320477313,-18.8890191128216,
-6.48727875032715));
#75005=CARTESIAN_POINT('Ctrl Pts',(-16.6180739294109,-18.8844201683435,
-6.48699858470329));
#75006=CARTESIAN_POINT('Ctrl Pts',(-16.6184842939782,-18.8723911015177,
-6.48626357535467));
#75007=CARTESIAN_POINT('Ctrl Pts',(-16.6187769262391,-18.8649619414311,
-6.48580743280859));
#75008=CARTESIAN_POINT('Ctrl Pts',(-16.6209807527879,-18.8156226721339,
-6.48276412425206));
#75009=CARTESIAN_POINT('Ctrl Pts',(-16.624098162374,-18.7737787654935,-6.48011647832541));
#75010=CARTESIAN_POINT('Ctrl Pts',(-16.6300173621386,-18.7171130862076,
-6.47646446287558));
#75011=CARTESIAN_POINT('Ctrl Pts',(-16.6317375859846,-18.7021850144727,
-6.47549605174676));
#75012=CARTESIAN_POINT('Ctrl Pts',(-16.6545632958296,-18.5210798102523,
-6.46367979187551));
#75013=CARTESIAN_POINT('Ctrl Pts',(-16.6951610935069,-18.3579522419709,
-6.45240533508982));
#75014=CARTESIAN_POINT('Ctrl Pts',(-16.7753516803641,-18.1465060216482,
-6.43782943095842));
#75015=CARTESIAN_POINT('Ctrl Pts',(-16.7984018495846,-18.0925905720646,
-6.43410940993404));
#75016=CARTESIAN_POINT('Ctrl Pts',(-16.8391184726181,-18.0073310203449,
-6.42822885809885));
#75017=CARTESIAN_POINT('Ctrl Pts',(-16.8553960358253,-17.9753614400452,
-6.42602408576242));
#75018=CARTESIAN_POINT('Ctrl Pts',(-16.8777100589974,-17.9341604679788,
-6.42318121114312));
#75019=CARTESIAN_POINT('Ctrl Pts',(-16.8830163610748,-17.9245423446355,
-6.42251743923023));
#75020=CARTESIAN_POINT('Ctrl Pts',(-16.8917953916259,-17.9089183641132,
-6.42143887014229));
#75021=CARTESIAN_POINT('Ctrl Pts',(-16.8952231543605,-17.902887598033,-6.42102247051382));
#75022=CARTESIAN_POINT('Ctrl Pts',(-16.9018912720787,-17.8912888665283,
-6.42022143194358));
#75023=CARTESIAN_POINT('Ctrl Pts',(-16.9051275171653,-17.8857186381904,
-6.4198366505565));
#75024=CARTESIAN_POINT('Ctrl Pts',(-16.9126232268814,-17.8729515367666,
-6.4189544765716));
#75025=CARTESIAN_POINT('Ctrl Pts',(-16.916900028782,-17.865764927226,-6.41845771995237));
#75026=CARTESIAN_POINT('Ctrl Pts',(-16.9284367184189,-17.8466378375732,
-6.4171349960188));
#75027=CARTESIAN_POINT('Ctrl Pts',(-16.9357725122799,-17.8347434536846,
-6.41631180721062));
#75028=CARTESIAN_POINT('Ctrl Pts',(-16.9966445312147,-17.7381973484278,
-6.40962267679503));
#75029=CARTESIAN_POINT('Ctrl Pts',(-17.0560120669031,-17.6573644910778,
-6.40398437651985));
#75030=CARTESIAN_POINT('Ctrl Pts',(-17.2321291162792,-17.4501412498993,
-6.38899950788371));
#75031=CARTESIAN_POINT('Ctrl Pts',(-17.3588741841571,-17.3332927326408,
-6.37997057777922));
#75032=CARTESIAN_POINT('Ctrl Pts',(-17.5307433376399,-17.2097438452632,
-6.36791119503487));
#75033=CARTESIAN_POINT('Ctrl Pts',(-17.5638129195058,-17.18736268972,-6.36559564730284));
#75034=CARTESIAN_POINT('Ctrl Pts',(-17.6039789913882,-17.1618043060634,
-6.36276379572246));
#75035=CARTESIAN_POINT('Ctrl Pts',(-17.6104873602938,-17.1577125517882,
-6.36230433879136));
#75036=CARTESIAN_POINT('Ctrl Pts',(-17.6205918606746,-17.1514364722087,
-6.36158986450907));
#75037=CARTESIAN_POINT('Ctrl Pts',(-17.6241725376006,-17.1492272174991,
-6.36133645841383));
#75038=CARTESIAN_POINT('Ctrl Pts',(-17.630796648954,-17.1451673975155,-6.36086721270737));
#75039=CARTESIAN_POINT('Ctrl Pts',(-17.6338381772874,-17.1433138330682,
-6.36065157397906));
#75040=CARTESIAN_POINT('Ctrl Pts',(-17.6406887430015,-17.1391626429884,
-6.3601654805608));
#75041=CARTESIAN_POINT('Ctrl Pts',(-17.6445003276663,-17.1368693570971,
-6.35989474979174));
#75042=CARTESIAN_POINT('Ctrl Pts',(-17.6542707535155,-17.1310327247085,
-6.35920013124528));
#75043=CARTESIAN_POINT('Ctrl Pts',(-17.6602397710093,-17.127506637175,-6.35877516278824));
#75044=CARTESIAN_POINT('Ctrl Pts',(-17.6951944725997,-17.1070887330212,
-6.35628349365683));
#75045=CARTESIAN_POINT('Ctrl Pts',(-17.72455935678,-17.0908595423594,-6.3541781573002));
#75046=CARTESIAN_POINT('Ctrl Pts',(-17.7705072620938,-17.0668726314496,
-6.35087960364614));
#75047=CARTESIAN_POINT('Ctrl Pts',(-17.7868276594351,-17.0586199608626,
-6.34970715444302));
#75048=CARTESIAN_POINT('Ctrl Pts',(-17.8254388926516,-17.0397197126319,
-6.34693470648031));
#75049=CARTESIAN_POINT('Ctrl Pts',(-17.8478131141558,-17.029248866828,-6.34532920737995));
#75050=CARTESIAN_POINT('Ctrl Pts',(-17.9113756774904,-17.0008475428734,
-6.34078022524983));
#75051=CARTESIAN_POINT('Ctrl Pts',(-17.9529585126555,-16.9838331618609,
-6.33781851446724));
#75052=CARTESIAN_POINT('Ctrl Pts',(-18.0975170120735,-16.9299874800686,
-6.32762836554599));
#75053=CARTESIAN_POINT('Ctrl Pts',(-18.2027950636094,-16.8998133596006,
-6.32039833415335));
#75054=CARTESIAN_POINT('Ctrl Pts',(-18.3638784916733,-16.8668788601433,
-6.3098304989886));
#75055=CARTESIAN_POINT('Ctrl Pts',(-18.4182309964562,-16.8579582491381,
-6.30634429873058));
#75056=CARTESIAN_POINT('Ctrl Pts',(-18.5068944892584,-16.8469376717436,
-6.30079085898782));
#75057=CARTESIAN_POINT('Ctrl Pts',(-18.5410147577039,-16.8435358122439,
-6.29868525194005));
#75058=CARTESIAN_POINT('Ctrl Pts',(-18.5859799076044,-16.8401534562664,
-6.29595009418729));
#75059=CARTESIAN_POINT('Ctrl Pts',(-18.5967617762978,-16.8394253980584,
-6.29529723139733));
#75060=CARTESIAN_POINT('Ctrl Pts',(-18.6144340908385,-16.8383679201721,
-6.29423190364988));
#75061=CARTESIAN_POINT('Ctrl Pts',(-18.6213213104347,-16.8379895718846,
-6.29381791020152));
#75062=CARTESIAN_POINT('Ctrl Pts',(-18.6346591961947,-16.8373222238807,
-6.29301841436067));
#75063=CARTESIAN_POINT('Ctrl Pts',(-18.6411095689713,-16.8370290637074,
-6.29263278583931));
#75064=CARTESIAN_POINT('Ctrl Pts',(-18.6560100706432,-16.8364201568125,
-6.29174428024787));
#75065=CARTESIAN_POINT('Ctrl Pts',(-18.6644609879816,-16.836125516257,-6.29124206965336));
#75066=CARTESIAN_POINT('Ctrl Pts',(-18.6872016712451,-16.8354690559113,
-6.28989513410677));
#75067=CARTESIAN_POINT('Ctrl Pts',(-18.701493867076,-16.8352013116252,-6.2890533528143));
#75068=CARTESIAN_POINT('Ctrl Pts',(-18.8329520607706,-16.8340703657281,
-6.28135185329706));
#75069=CARTESIAN_POINT('Ctrl Pts',(-18.9500047419029,-16.8427905052208,
-6.27481076412205));
#75070=CARTESIAN_POINT('Ctrl Pts',(-19.2275946151357,-16.8868348352363,
-6.25942584745279));
#75071=CARTESIAN_POINT('Ctrl Pts',(-19.3858917478135,-16.931216092929,-6.25076843480755));
#75072=CARTESIAN_POINT('Ctrl Pts',(-19.5663314778003,-17.0052368748225,
-6.23955363471204));
#75073=CARTESIAN_POINT('Ctrl Pts',(-19.5949288075185,-17.0177136431849,
-6.23773211010064));
#75074=CARTESIAN_POINT('Ctrl Pts',(-19.6297250736602,-17.0338194334036,
-6.23544866828161));
#75075=CARTESIAN_POINT('Ctrl Pts',(-19.6361965328241,-17.0368547035552,
-6.23502109578778));
#75076=CARTESIAN_POINT('Ctrl Pts',(-19.6463460525425,-17.0416779317097,
-6.23434575973968));
#75077=CARTESIAN_POINT('Ctrl Pts',(-19.6500345842939,-17.0434439060081,
-6.23409933766474));
#75078=CARTESIAN_POINT('Ctrl Pts',(-19.6569379622463,-17.0467736883354,
-6.23363623519491));
#75079=CARTESIAN_POINT('Ctrl Pts',(-19.6601539720458,-17.0483349558805,
-6.23341971263518));
#75080=CARTESIAN_POINT('Ctrl Pts',(-19.6675103600951,-17.0519292950798,
-6.23292265129036));
#75081=CARTESIAN_POINT('Ctrl Pts',(-19.6716480462529,-17.0539677514517,
-6.23264177999507));
#75082=CARTESIAN_POINT('Ctrl Pts',(-19.6824717821642,-17.0593441612441,
-6.23190372259834));
#75083=CARTESIAN_POINT('Ctrl Pts',(-19.689146809453,-17.0627039898041,-6.23144522047047));
#75084=CARTESIAN_POINT('Ctrl Pts',(-19.7338275216001,-17.0854910179538,
-6.22835436897585));
#75085=CARTESIAN_POINT('Ctrl Pts',(-19.7712532163773,-17.1060270722113,
-6.22565942242448));
#75086=CARTESIAN_POINT('Ctrl Pts',(-19.8142369740676,-17.1313328240116,
-6.22246030372404));
#75087=CARTESIAN_POINT('Ctrl Pts',(-19.8204255531634,-17.1350188770393,
-6.22199712856155));
#75088=CARTESIAN_POINT('Ctrl Pts',(-19.9612667908131,-17.2198837866833,
-6.21139886678943));
#75089=CARTESIAN_POINT('Ctrl Pts',(-20.086479596813,-17.3157810033686,-6.20082561343532));
#75090=CARTESIAN_POINT('Ctrl Pts',(-20.2683631252552,-17.4903510055799,
-6.18444648527678));
#75091=CARTESIAN_POINT('Ctrl Pts',(-20.3323175773567,-17.5605715644623,
-6.17842085925353));
#75092=CARTESIAN_POINT('Ctrl Pts',(-20.4046232468636,-17.6515531901783,
-6.17128278093974));
#75093=CARTESIAN_POINT('Ctrl Pts',(-20.4176410439852,-17.6684514713499,
-6.16998273407402));
#75094=CARTESIAN_POINT('Ctrl Pts',(-20.4357852638612,-17.6927554238908,
-6.16814850795982));
#75095=CARTESIAN_POINT('Ctrl Pts',(-20.4411229328079,-17.7000010850858,
-6.16760607468737));
#75096=CARTESIAN_POINT('Ctrl Pts',(-20.4502504309153,-17.7125581794305,
-6.16667348775311));
#75097=CARTESIAN_POINT('Ctrl Pts',(-20.4540621747525,-17.7178534590016,
-6.1662824868314));
#75098=CARTESIAN_POINT('Ctrl Pts',(-20.4613129495777,-17.7280250909617,
-6.16553570874941));
#75099=CARTESIAN_POINT('Ctrl Pts',(-20.4647559574677,-17.7328985191761,
-6.16517978076402));
#75100=CARTESIAN_POINT('Ctrl Pts',(-20.4736538370317,-17.7456067535594,
-6.16425644286757));
#75101=CARTESIAN_POINT('Ctrl Pts',(-20.4790764376013,-17.7534640726189,
-6.16369026905189));
#75102=CARTESIAN_POINT('Ctrl Pts',(-20.4973780555938,-17.7803705543315,
-6.16176721165222));
#75103=CARTESIAN_POINT('Ctrl Pts',(-20.5100000731756,-17.7995931595424,
-6.16042002013654));
#75104=CARTESIAN_POINT('Ctrl Pts',(-20.6162011652518,-17.9672217366862,
-6.14888906976616));
#75105=CARTESIAN_POINT('Ctrl Pts',(-20.6913089535726,-18.1265196452655,
-6.13945581009008));
#75106=CARTESIAN_POINT('Ctrl Pts',(-20.7729860249327,-18.3759800718239,
-6.12517350255245));
#75107=CARTESIAN_POINT('Ctrl Pts',(-20.7949379617914,-18.4602731565903,
-6.12040915521734));
#75108=CARTESIAN_POINT('Ctrl Pts',(-20.818900132923,-18.5827961291658,-6.11328128615683));
#75109=CARTESIAN_POINT('Ctrl Pts',(-20.8251640469048,-18.6201075595146,
-6.11108389291071));
#75110=CARTESIAN_POINT('Ctrl Pts',(-20.8314778231644,-18.6650625199462,
-6.10838294459277));
#75111=CARTESIAN_POINT('Ctrl Pts',(-20.8324907021525,-18.6725664565944,
-6.10793032174421));
#75112=CARTESIAN_POINT('Ctrl Pts',(-20.8340004993208,-18.6842232368771,
-6.10722422659029));
#75113=CARTESIAN_POINT('Ctrl Pts',(-20.8345254155557,-18.6883724788151,
-6.10697230589792));
#75114=CARTESIAN_POINT('Ctrl Pts',(-20.835474833797,-18.6960601175115,-6.10650442296411));
#75115=CARTESIAN_POINT('Ctrl Pts',(-20.835902697796,-18.6995980409213,-6.10628865262771));
#75116=CARTESIAN_POINT('Ctrl Pts',(-20.836848273354,-18.7075859868555,-6.10580048235774));
#75117=CARTESIAN_POINT('Ctrl Pts',(-20.837360790625,-18.7120365565819,-6.10552779540454));
#75118=CARTESIAN_POINT('Ctrl Pts',(-20.8388276184309,-18.7251399565725,
-6.10472296328847));
#75119=CARTESIAN_POINT('Ctrl Pts',(-20.8397426744963,-18.7337969628086,
-6.10418869001278));
#75120=CARTESIAN_POINT('Ctrl Pts',(-20.8458591842653,-18.7952888792466,
-6.10037679337727));
#75121=CARTESIAN_POINT('Ctrl Pts',(-20.8491244443308,-18.8482929538423,
-6.09700301862787));
#75122=CARTESIAN_POINT('Ctrl Pts',(-20.8507874982812,-18.9177948251246,
-6.09251065584329));
#75123=CARTESIAN_POINT('Ctrl Pts',(-20.8509892979677,-18.9342348571539,
-6.09144298497249));
#75124=CARTESIAN_POINT('Ctrl Pts',(-20.8510113339811,-18.9694500117011,
-6.08914723831414));
#75125=CARTESIAN_POINT('Ctrl Pts',(-20.8507733241541,-18.9882237924484,
-6.08791800906747));
#75126=CARTESIAN_POINT('Ctrl Pts',(-20.8462294472628,-19.1630893871222,
-6.07643127822385));
#75127=CARTESIAN_POINT('Ctrl Pts',(-20.8249136862804,-19.3182816586248,
-6.0660096583617));
#75128=CARTESIAN_POINT('Ctrl Pts',(-20.7855427580425,-19.4743833987669,
-6.05574893351126));
#75129=CARTESIAN_POINT('Ctrl Pts',(-20.7843514048602,-19.4790400558735,
-6.05544300635235));
#75130=CARTESIAN_POINT('Ctrl Pts',(-20.7672397017651,-19.5449885839064,
-6.05111271590937));
#75131=CARTESIAN_POINT('Ctrl Pts',(-20.7485917903037,-19.6055444826611,
-6.0471663605319));
#75132=CARTESIAN_POINT('Ctrl Pts',(-20.7257108607384,-19.6694941509089,
-6.04302907618597));
#75133=CARTESIAN_POINT('Ctrl Pts',(-20.7241527163644,-19.6738048039783,
-6.04275033647391));
#75134=CARTESIAN_POINT('Ctrl Pts',(-20.7225805821268,-19.6781103692884,
-6.04247206352563));
#75135=CARTESIAN_POINT('Origin',(-18.734,-18.952,0.));
#75136=CARTESIAN_POINT('',(-20.7225806512393,-19.6781101800117,-5.24452704027197));
#75137=CARTESIAN_POINT('',(-20.7225805821191,-19.6781103693095,-5.46434836675477));
#75138=CARTESIAN_POINT('',(-20.7225805821191,-19.6781103693095,0.));
#75139=CARTESIAN_POINT('',(-20.850999355781,-18.9536515516794,-5.51218507055412));
#75140=CARTESIAN_POINT('Ctrl Pts',(-20.7225805821191,-19.6781103693095,
-5.46434836675477));
#75141=CARTESIAN_POINT('Ctrl Pts',(-20.723192165304,-19.6764354415064,-5.46445566646443));
#75142=CARTESIAN_POINT('Ctrl Pts',(-20.7238016299532,-19.6747597476393,
-5.46456309084474));
#75143=CARTESIAN_POINT('Ctrl Pts',(-20.7256303769629,-19.6697118502574,
-5.46488693162053));
#75144=CARTESIAN_POINT('Ctrl Pts',(-20.7268431849093,-19.6663373843159,
-5.46510373048139));
#75145=CARTESIAN_POINT('Ctrl Pts',(-20.7294018383849,-19.6591610624263,
-5.46556547520601));
#75146=CARTESIAN_POINT('Ctrl Pts',(-20.7307453742014,-19.6553584966566,
-5.46581054749099));
#75147=CARTESIAN_POINT('Ctrl Pts',(-20.7343556019155,-19.645046875665,-5.4664761725672));
#75148=CARTESIAN_POINT('Ctrl Pts',(-20.7366013615508,-19.638530618166,-5.46689793361378));
#75149=CARTESIAN_POINT('Ctrl Pts',(-20.7477596008164,-19.6056334283903,
-5.46903245536519));
#75150=CARTESIAN_POINT('Ctrl Pts',(-20.7561823297465,-19.5790907753001,
-5.47077168259425));
#75151=CARTESIAN_POINT('Ctrl Pts',(-20.7792348623651,-19.5011441823547,
-5.47591306665285));
#75152=CARTESIAN_POINT('Ctrl Pts',(-20.7924441376168,-19.4493448821175,
-5.47937189794215));
#75153=CARTESIAN_POINT('Ctrl Pts',(-20.8350198964028,-19.2513733902427,
-5.4926211182554));
#75154=CARTESIAN_POINT('Ctrl Pts',(-20.8508830562357,-19.1027271546237,
-5.50259347648227));
#75155=CARTESIAN_POINT('Ctrl Pts',(-20.850999355781,-18.9536515516794,-5.51218507055412));
#75156=CARTESIAN_POINT('Ctrl Pts',(-20.8509993578165,-18.9536489404629,
-5.51218523856097));
#75157=CARTESIAN_POINT('Ctrl Pts',(-20.8510649773718,-18.8694029900064,
-5.51760566003188));
#75158=CARTESIAN_POINT('Ctrl Pts',(-20.8461018014202,-18.7852181728266,
-5.52290055521964));
#75159=CARTESIAN_POINT('Ctrl Pts',(-20.8349011934136,-18.6912099913197,
-5.52867294427367));
#75160=CARTESIAN_POINT('Ctrl Pts',(-20.8335940937956,-18.6808876607733,
-5.52930492195785));
#75161=CARTESIAN_POINT('Ctrl Pts',(-20.8312616502042,-18.6634977245725,
-5.53036658643347));
#75162=CARTESIAN_POINT('Ctrl Pts',(-20.8302765582527,-18.6564249915505,
-5.53079753558967));
#75163=CARTESIAN_POINT('Ctrl Pts',(-20.8283990621847,-18.6434267119139,
-5.5315880186461));
#75164=CARTESIAN_POINT('Ctrl Pts',(-20.827517252791,-18.6374997309757,-5.53194788389538));
#75165=CARTESIAN_POINT('Ctrl Pts',(-20.825646330153,-18.6252811756259,-5.53268858144462));
#75166=CARTESIAN_POINT('Ctrl Pts',(-20.824653965858,-18.6189901547168,-5.53306930663188));
#75167=CARTESIAN_POINT('Ctrl Pts',(-20.8223696973148,-18.6049219707014,
-5.53391930288454));
#75168=CARTESIAN_POINT('Ctrl Pts',(-20.8210627048583,-18.5971473268443,
-5.53438808989743));
#75169=CARTESIAN_POINT('Ctrl Pts',(-20.8176411993383,-18.5774675579438,
-5.5355723965986));
#75170=CARTESIAN_POINT('Ctrl Pts',(-20.815468048469,-18.5655728140616,-5.53628604971493));
#75171=CARTESIAN_POINT('Ctrl Pts',(-20.8024833837919,-18.497791162282,-5.5403413460611));
#75172=CARTESIAN_POINT('Ctrl Pts',(-20.7895226632367,-18.4423367872297,
-5.54361378928937));
#75173=CARTESIAN_POINT('Ctrl Pts',(-20.7635221180252,-18.3483650949568,
-5.54912160343954));
#75174=CARTESIAN_POINT('Ctrl Pts',(-20.7515805956661,-18.3095796629295,
-5.55138385254816));
#75175=CARTESIAN_POINT('Ctrl Pts',(-20.7072759613866,-18.1791378045608,
-5.55899523440277));
#75176=CARTESIAN_POINT('Ctrl Pts',(-20.6697202997907,-18.0893752959372,
-5.56423294202583));
#75177=CARTESIAN_POINT('Ctrl Pts',(-20.5749345088226,-17.900487267687,-5.575741133546));
#75178=CARTESIAN_POINT('Ctrl Pts',(-20.515576913746,-17.8027848451378,-5.5820144547951));
#75179=CARTESIAN_POINT('Ctrl Pts',(-20.441714467317,-17.7007846057636,-5.58944723154195));
#75180=CARTESIAN_POINT('Ctrl Pts',(-20.4347032415601,-17.6912711891749,
-5.59014960929642));
#75181=CARTESIAN_POINT('Ctrl Pts',(-20.4246086589607,-17.6778114606168,
-5.59115720652724));
#75182=CARTESIAN_POINT('Ctrl Pts',(-20.4215902367403,-17.6738164203315,
-5.59145803488116));
#75183=CARTESIAN_POINT('Ctrl Pts',(-20.4163586720484,-17.6669430045232,
-5.59197872083395));
#75184=CARTESIAN_POINT('Ctrl Pts',(-20.4141522225773,-17.6640595154036,
-5.59219810811991));
#75185=CARTESIAN_POINT('Ctrl Pts',(-20.4098553839566,-17.6584740426378,
-5.5926249521417));
#75186=CARTESIAN_POINT('Ctrl Pts',(-20.4077658687508,-17.6557714373895,
-5.59283234212935));
#75187=CARTESIAN_POINT('Ctrl Pts',(-20.4021012310066,-17.6484812580356,
-5.59339405878653));
#75188=CARTESIAN_POINT('Ctrl Pts',(-20.3985137604331,-17.6439033800854,
-5.59374925001738));
#75189=CARTESIAN_POINT('Ctrl Pts',(-20.3850731745406,-17.6268970135584,
-5.59507776404666));
#75190=CARTESIAN_POINT('Ctrl Pts',(-20.3750996332916,-17.6145649504899,
-5.59605916982759));
#75191=CARTESIAN_POINT('Ctrl Pts',(-20.2853517053845,-17.5061090604366,
-5.60484300666774));
#75192=CARTESIAN_POINT('Ctrl Pts',(-20.1973605142541,-17.4171179450614,
-5.61311310745137));
#75193=CARTESIAN_POINT('Ctrl Pts',(-20.0321701174072,-17.2772379764777,
-5.62741665042648));
#75194=CARTESIAN_POINT('Ctrl Pts',(-19.9585208567808,-17.222657833255,-5.63344658060375));
#75195=CARTESIAN_POINT('Ctrl Pts',(-19.8341707683413,-17.1424436807893,
-5.64296804818991));
#75196=CARTESIAN_POINT('Ctrl Pts',(-19.7855715780523,-17.1137758883874,
-5.64654257052223));
#75197=CARTESIAN_POINT('Ctrl Pts',(-19.7154818800429,-17.0761219158005,
-5.65149050811432));
#75198=CARTESIAN_POINT('Ctrl Pts',(-19.6949028474367,-17.0654976671957,
-5.65291918538296));
#75199=CARTESIAN_POINT('Ctrl Pts',(-19.6584462476372,-17.0474277527893,
-5.65540870699129));
#75200=CARTESIAN_POINT('Ctrl Pts',(-19.6426430670796,-17.039837842838,-5.65647446684823));
#75201=CARTESIAN_POINT('Ctrl Pts',(-19.6192400192665,-17.0289535487961,
-5.65803352456691));
#75202=CARTESIAN_POINT('Ctrl Pts',(-19.6117124894652,-17.0255062071014,
-5.65853209629923));
#75203=CARTESIAN_POINT('Ctrl Pts',(-19.5986006284094,-17.0195942434106,
-5.65939557996678));
#75204=CARTESIAN_POINT('Ctrl Pts',(-19.5930255428042,-17.0171094674979,
-5.65976118196537));
#75205=CARTESIAN_POINT('Ctrl Pts',(-19.5819064119512,-17.0122112805998,
-5.66048730988549));
#75206=CARTESIAN_POINT('Ctrl Pts',(-19.5763626196646,-17.0097974416917,
-5.66084784779554));
#75207=CARTESIAN_POINT('Ctrl Pts',(-19.5631489934511,-17.0041112764891,
-5.66170367722274));
#75208=CARTESIAN_POINT('Ctrl Pts',(-19.5554699804815,-17.0008604338197,
-5.6621982340119));
#75209=CARTESIAN_POINT('Ctrl Pts',(-19.5280515796337,-16.989443655501,-5.66395429549978));
#75210=CARTESIAN_POINT('Ctrl Pts',(-19.5082076248653,-16.9815310408094,
-5.6652072381635));
#75211=CARTESIAN_POINT('Ctrl Pts',(-19.3084660712501,-16.9053690997746,
-5.67764965640986));
#75212=CARTESIAN_POINT('Ctrl Pts',(-19.1201875471757,-16.8616474525009,
-5.68790565115474));
#75213=CARTESIAN_POINT('Ctrl Pts',(-18.8531492053921,-16.8369985791891,
-5.70254804019266));
#75214=CARTESIAN_POINT('Ctrl Pts',(-18.7774029112869,-16.8340901911473,
-5.70672656395101));
#75215=CARTESIAN_POINT('Ctrl Pts',(-18.6668516139817,-16.8357786704258,
-5.71305904194058));
#75216=CARTESIAN_POINT('Ctrl Pts',(-18.6320536306303,-16.8371694530356,
-5.71508642344316));
#75217=CARTESIAN_POINT('Ctrl Pts',(-18.5899319468194,-16.839894881452,-5.7175987823462));
#75218=CARTESIAN_POINT('Ctrl Pts',(-18.5825584452229,-16.8404107673196,
-5.71804074767399));
#75219=CARTESIAN_POINT('Ctrl Pts',(-18.5710565700527,-16.8412760475873,
-5.71873376464452));
#75220=CARTESIAN_POINT('Ctrl Pts',(-18.5669261816538,-16.8415989710012,
-5.71898335569992));
#75221=CARTESIAN_POINT('Ctrl Pts',(-18.5592408321956,-16.8422225327113,
-5.71944915900284));
#75222=CARTESIAN_POINT('Ctrl Pts',(-18.5556856738514,-16.8425200335916,
-5.71966519360376));
#75223=CARTESIAN_POINT('Ctrl Pts',(-18.5476150003735,-16.8432159474172,
-5.72015688339496));
#75224=CARTESIAN_POINT('Ctrl Pts',(-18.5431000230561,-16.8436198762006,
-5.72043284384559));
#75225=CARTESIAN_POINT('Ctrl Pts',(-18.5314073438093,-16.8447038182057,
-5.72114976964708));
#75226=CARTESIAN_POINT('Ctrl Pts',(-18.5242318248041,-16.84540599749,-5.72159193389962));
#75227=CARTESIAN_POINT('Ctrl Pts',(-18.4793497899922,-16.8500296306153,
-5.72437082687246));
#75228=CARTESIAN_POINT('Ctrl Pts',(-18.4417531864418,-16.8549264310823,
-5.72675693701609));
#75229=CARTESIAN_POINT('Ctrl Pts',(-18.2366588711491,-16.887261103057,-5.74002148790082));
#75230=CARTESIAN_POINT('Ctrl Pts',(-18.0727946768144,-16.9337567774534,
-5.75147113698783));
#75231=CARTESIAN_POINT('Ctrl Pts',(-17.8287253679685,-17.0359707178545,
-5.76866278538847));
#75232=CARTESIAN_POINT('Ctrl Pts',(-17.7437679165177,-17.0784645778304,
-5.77468924611025));
#75233=CARTESIAN_POINT('Ctrl Pts',(-17.6435447412113,-17.1373233536333,
-5.78182820053321));
#75234=CARTESIAN_POINT('Ctrl Pts',(-17.6253151209964,-17.1484030678603,
-5.78312834037129));
#75235=CARTESIAN_POINT('Ctrl Pts',(-17.5996365788949,-17.1645466103439,
-5.78496267368201));
#75236=CARTESIAN_POINT('Ctrl Pts',(-17.592048155024,-17.1693850727093,-5.78550512249112));
#75237=CARTESIAN_POINT('Ctrl Pts',(-17.5790118633132,-17.1778145607328,
-5.78643772774021));
#75238=CARTESIAN_POINT('Ctrl Pts',(-17.5735493637989,-17.1813826242763,
-5.78682873152825));
#75239=CARTESIAN_POINT('Ctrl Pts',(-17.5631229840833,-17.1882620328694,
-5.78757550937497));
#75240=CARTESIAN_POINT('Ctrl Pts',(-17.5581564458295,-17.1915692173964,
-5.78793143428601));
#75241=CARTESIAN_POINT('Ctrl Pts',(-17.5452805070876,-17.2002220176809,
-5.78885475186381));
#75242=CARTESIAN_POINT('Ctrl Pts',(-17.5373931075313,-17.2056002514883,
-5.78942090854513));
#75243=CARTESIAN_POINT('Ctrl Pts',(-17.510634010907,-17.224113053529,-5.79134384442678));
#75244=CARTESIAN_POINT('Ctrl Pts',(-17.4919396130848,-17.2375019103998,
-5.79269093324734));
#75245=CARTESIAN_POINT('Ctrl Pts',(-17.3325077768454,-17.3556629832336,
-5.80422227560228));
#75246=CARTESIAN_POINT('Ctrl Pts',(-17.2050834126516,-17.4772481249502,
-5.81365594412651));
#75247=CARTESIAN_POINT('Ctrl Pts',(-17.039077082204,-17.6805840586418,-5.82793846872569));
#75248=CARTESIAN_POINT('Ctrl Pts',(-16.9882547430038,-17.7513196534878,
-5.83270258609255));
#75249=CARTESIAN_POINT('Ctrl Pts',(-16.9217945585225,-17.8569970707073,
-5.83983014512697));
#75250=CARTESIAN_POINT('Ctrl Pts',(-16.90251926848,-17.889550985693,-5.84202747481105));
#75251=CARTESIAN_POINT('Ctrl Pts',(-16.8804458017486,-17.9292179267824,
-5.84472835267362));
#75252=CARTESIAN_POINT('Ctrl Pts',(-16.8767994796401,-17.9358540663859,
-5.84518097171932));
#75253=CARTESIAN_POINT('Ctrl Pts',(-16.8711945565141,-17.9461857171335,
-5.84588706220637));
#75254=CARTESIAN_POINT('Ctrl Pts',(-16.8692111317297,-17.9498677891718,
-5.84613898206746));
#75255=CARTESIAN_POINT('Ctrl Pts',(-16.8655578583016,-17.9566982047321,
-5.8466068642418));
#75256=CARTESIAN_POINT('Ctrl Pts',(-16.863885043555,-17.959844896381,-5.84682263465507));
#75257=CARTESIAN_POINT('Ctrl Pts',(-16.8601272308887,-17.9669568964184,
-5.84731080610661));
#75258=CARTESIAN_POINT('Ctrl Pts',(-16.8580468821083,-17.9709245852896,
-5.84758349417042));
#75259=CARTESIAN_POINT('Ctrl Pts',(-16.8519611864967,-17.9826214936684,
-5.84838833254776));
#75260=CARTESIAN_POINT('Ctrl Pts',(-16.8479909597664,-17.9903687410194,
-5.84892261102267));
#75261=CARTESIAN_POINT('Ctrl Pts',(-16.8201469732622,-18.0455374523063,
-5.85273461148439));
#75262=CARTESIAN_POINT('Ctrl Pts',(-16.7980188014963,-18.0938138114598,
-5.85610849055743));
#75263=CARTESIAN_POINT('Ctrl Pts',(-16.7705824356547,-18.1601476048199,
-5.86074703213836));
#75264=CARTESIAN_POINT('Ctrl Pts',(-16.7636640157269,-18.1775228680619,
-5.8619623206863));
#75265=CARTESIAN_POINT('Ctrl Pts',(-16.739913223645,-18.239550698721,-5.86629680707674));
#75266=CARTESIAN_POINT('Ctrl Pts',(-16.724361626426,-18.2846773929496,-5.8694426967701));
#75267=CARTESIAN_POINT('Ctrl Pts',(-16.6782280979619,-18.4348408869696,
-5.87981966685946));
#75268=CARTESIAN_POINT('Ctrl Pts',(-16.6542559121023,-18.5417322139677,
-5.88705182587264));
#75269=CARTESIAN_POINT('Ctrl Pts',(-16.6307922327491,-18.704530637206,-5.8976241297015));
#75270=CARTESIAN_POINT('Ctrl Pts',(-16.6250643057784,-18.7593473176632,
-5.90111265616119));
#75271=CARTESIAN_POINT('Ctrl Pts',(-16.6192506984924,-18.8485552851426,
-5.90666936732001));
#75272=CARTESIAN_POINT('Ctrl Pts',(-16.6178522138597,-18.8828322277822,
-5.90877597596377));
#75273=CARTESIAN_POINT('Ctrl Pts',(-16.6171091801909,-18.9279361511284,
-5.91151222463));
#75274=CARTESIAN_POINT('Ctrl Pts',(-16.6170139119708,-18.9387439941796,
-5.91216520000266));
#75275=CARTESIAN_POINT('Ctrl Pts',(-16.6169934394926,-18.9564501519871,
-5.91323066435871));
#75276=CARTESIAN_POINT('Ctrl Pts',(-16.6170191774154,-18.9633481119614,
-5.9136446825898));
#75277=CARTESIAN_POINT('Ctrl Pts',(-16.6171342791504,-18.9767024269151,
-5.91444419375255));
#75278=CARTESIAN_POINT('Ctrl Pts',(-16.6172194670201,-18.9831587327522,
-5.91482981298356));
#75279=CARTESIAN_POINT('Ctrl Pts',(-16.617484417735,-18.9980681579844,-5.91571825066866));
#75280=CARTESIAN_POINT('Ctrl Pts',(-16.6176852862598,-19.0065208283215,
-5.91622040297404));
#75281=CARTESIAN_POINT('Ctrl Pts',(-16.6183618793784,-19.0292564901604,
-5.91756707898111));
#75282=CARTESIAN_POINT('Ctrl Pts',(-16.6189316026856,-19.0435363987407,
-5.91840866081854));
#75283=CARTESIAN_POINT('Ctrl Pts',(-16.6254887723869,-19.1745657602676,
-5.92609439349616));
#75284=CARTESIAN_POINT('Ctrl Pts',(-16.6409925033073,-19.2906443606613,
-5.93262147566152));
#75285=CARTESIAN_POINT('Ctrl Pts',(-16.7008707918916,-19.5640784168669,
-5.94794486672316));
#75286=CARTESIAN_POINT('Ctrl Pts',(-16.7540025484123,-19.7187153940254,
-5.95655738493446));
#75287=CARTESIAN_POINT('Ctrl Pts',(-16.838239885856,-19.8947728879494,-5.96776743646225));
#75288=CARTESIAN_POINT('Ctrl Pts',(-16.8528070799986,-19.9235143187644,
-5.96964708166029));
#75289=CARTESIAN_POINT('Ctrl Pts',(-16.8714335886739,-19.958274062563,-5.97199523340606));
#75290=CARTESIAN_POINT('Ctrl Pts',(-16.8748761534455,-19.9646201880982,
-5.97242704984411));
#75291=CARTESIAN_POINT('Ctrl Pts',(-16.8803270273673,-19.9745469986074,
-5.97310760140977));
#75292=CARTESIAN_POINT('Ctrl Pts',(-16.8823134428908,-19.97813973093,-5.97335496039194));
#75293=CARTESIAN_POINT('Ctrl Pts',(-16.8860480084109,-19.9848481011705,
-5.97381884467594));
#75294=CARTESIAN_POINT('Ctrl Pts',(-16.8877935990292,-19.987965099636,-5.97403520622955));
#75295=CARTESIAN_POINT('Ctrl Pts',(-16.8917990286321,-19.9950750844817,
-5.97453060323972));
#75296=CARTESIAN_POINT('Ctrl Pts',(-16.8940639562644,-19.9990651387677,
-5.97480996282954));
#75297=CARTESIAN_POINT('Ctrl Pts',(-16.9000116291057,-20.0094640855736,
-5.97554149543378));
#75298=CARTESIAN_POINT('Ctrl Pts',(-16.9037149645511,-20.01586104459,-5.97599494777293));
#75299=CARTESIAN_POINT('Ctrl Pts',(-16.9282493267195,-20.0577332103697,
-5.97898511057316));
#75300=CARTESIAN_POINT('Ctrl Pts',(-16.9500756956761,-20.092611673444,-5.98157997802144));
#75301=CARTESIAN_POINT('Ctrl Pts',(-16.9785954782324,-20.135363514194,-5.98487201392494));
#75302=CARTESIAN_POINT('Ctrl Pts',(-16.9843504442667,-20.1438559761172,
-5.98553162334431));
#75303=CARTESIAN_POINT('Ctrl Pts',(-16.9905429064728,-20.1528525317468,
-5.98623618234779));
#75304=CARTESIAN_POINT('Ctrl Pts',(-16.9909192462669,-20.1533987372795,
-5.98627898093399));
#75305=CARTESIAN_POINT('Ctrl Pts',(-17.0042628851189,-20.1727457285681,
-5.98779574614873));
#75306=CARTESIAN_POINT('Ctrl Pts',(-17.0175330097642,-20.1913351602275,
-5.9892801694208));
#75307=CARTESIAN_POINT('Ctrl Pts',(-17.0582335406493,-20.2464425609985,
-5.99375508029232));
#75308=CARTESIAN_POINT('Ctrl Pts',(-17.0865472209864,-20.2822909156953,
-5.9967662323036));
#75309=CARTESIAN_POINT('Ctrl Pts',(-17.1865154855057,-20.4007713969403,
-6.00700650583097));
#75310=CARTESIAN_POINT('Ctrl Pts',(-17.2634088145626,-20.4787651800786,
-6.0142370854979));
#75311=CARTESIAN_POINT('Ctrl Pts',(-17.3875660103565,-20.5865753622057,
-6.02480607213136));
#75312=CARTESIAN_POINT('Ctrl Pts',(-17.4305385826985,-20.6210447137009,
-6.02829287176991));
#75313=CARTESIAN_POINT('Ctrl Pts',(-17.5023719924443,-20.6741954165705,
-6.03384715446885));
#75314=CARTESIAN_POINT('Ctrl Pts',(-17.5304270171886,-20.6939175907363,
-6.03595301961624));
#75315=CARTESIAN_POINT('Ctrl Pts',(-17.5679391609692,-20.7189487547639,
-6.03868845848497));
#75316=CARTESIAN_POINT('Ctrl Pts',(-17.5769741552405,-20.7248781637844,
-6.03934135028552));
#75317=CARTESIAN_POINT('Ctrl Pts',(-17.591849770131,-20.7344784513021,-6.04040671323086));
#75318=CARTESIAN_POINT('Ctrl Pts',(-17.5976635482948,-20.7381903726155,
-6.04082071306157));
#75319=CARTESIAN_POINT('Ctrl Pts',(-17.6089545765941,-20.745321913891,-6.04162021283985));
#75320=CARTESIAN_POINT('Ctrl Pts',(-17.6144295272225,-20.7487450151534,
-6.04200583896018));
#75321=CARTESIAN_POINT('Ctrl Pts',(-17.6271101523052,-20.7565928523384,
-6.04289432703066));
#75322=CARTESIAN_POINT('Ctrl Pts',(-17.6343268773118,-20.7609995920514,
-6.04339652258957));
#75323=CARTESIAN_POINT('Ctrl Pts',(-17.6538130468195,-20.7727387077009,
-6.0447433911984));
#75324=CARTESIAN_POINT('Ctrl Pts',(-17.6661308005046,-20.779990340027,-6.04558512105175));
#75325=CARTESIAN_POINT('Ctrl Pts',(-17.7800283110356,-20.8454991939601,
-6.05328251020523));
#75326=CARTESIAN_POINT('Ctrl Pts',(-17.8862102831229,-20.8953628239355,
-6.05981994772241));
#75327=CARTESIAN_POINT('Ctrl Pts',(-18.1493513218196,-20.9932374662671,
-6.07518832521485));
#75328=CARTESIAN_POINT('Ctrl Pts',(-18.3087952660216,-21.0323012183235,
-6.08383357512629));
#75329=CARTESIAN_POINT('Ctrl Pts',(-18.502352701236,-21.0565234722268,-6.09504693551604));
#75330=CARTESIAN_POINT('Ctrl Pts',(-18.5336629896907,-21.0597344140016,
-6.09688405070898));
#75331=CARTESIAN_POINT('Ctrl Pts',(-18.5721759019377,-21.0628181670366,
-6.0991848575549));
#75332=CARTESIAN_POINT('Ctrl Pts',(-18.5793232747794,-21.0633539448271,
-6.09961358317473));
#75333=CARTESIAN_POINT('Ctrl Pts',(-18.5905569848703,-21.0641386935524,
-6.10029033648786));
#75334=CARTESIAN_POINT('Ctrl Pts',(-18.5946416350763,-21.0644121295011,
-6.10053701332016));
#75335=CARTESIAN_POINT('Ctrl Pts',(-18.6022940450339,-21.0649021078387,
-6.10100032690858));
#75336=CARTESIAN_POINT('Ctrl Pts',(-18.6058615687777,-21.0651214630624,
-6.10121680421671));
#75337=CARTESIAN_POINT('Ctrl Pts',(-18.6140274954184,-21.0656028037622,
-6.10171340629773));
#75338=CARTESIAN_POINT('Ctrl Pts',(-18.6186261947882,-21.0658588169678,
-6.1019938612747));
#75339=CARTESIAN_POINT('Ctrl Pts',(-18.6328371901955,-21.0666034430593,
-6.10286289260626));
#75340=CARTESIAN_POINT('Ctrl Pts',(-18.6424518537548,-21.0670415041728,
-6.10345418875523));
#75341=CARTESIAN_POINT('Ctrl Pts',(-18.7385994139874,-21.0707653472408,
-6.10939834059158));
#75342=CARTESIAN_POINT('Ctrl Pts',(-18.8252445049579,-21.0688038923811,
-6.11500419074483));
#75343=CARTESIAN_POINT('Ctrl Pts',(-19.0379891875534,-21.0509017578764,
-6.12902183930854));
#75344=CARTESIAN_POINT('Ctrl Pts',(-19.1632601108586,-21.028905714308,-6.13748318541922));
#75345=CARTESIAN_POINT('Ctrl Pts',(-19.3790109779968,-20.9706554764984,
-6.15194737755517));
#75346=CARTESIAN_POINT('Ctrl Pts',(-19.4703936180671,-20.9391431933131,
-6.158042051408));
#75347=CARTESIAN_POINT('Ctrl Pts',(-19.5727827931087,-20.8957968620567,
-6.16482097640456));
#75348=CARTESIAN_POINT('Ctrl Pts',(-19.5861890752623,-20.889956813707,-6.1657077354927));
#75349=CARTESIAN_POINT('Ctrl Pts',(-19.6065883499041,-20.8808178562875,
-6.16705600375849));
#75350=CARTESIAN_POINT('Ctrl Pts',(-19.6136253670399,-20.8776188530583,
-6.16752091729008));
#75351=CARTESIAN_POINT('Ctrl Pts',(-19.6264196577487,-20.8717178433137,
-6.16836590062807));
#75352=CARTESIAN_POINT('Ctrl Pts',(-19.6321825539075,-20.8690283108749,
-6.16874639429736));
#75353=CARTESIAN_POINT('Ctrl Pts',(-19.644624186251,-20.8631534060413,-6.1695676512391));
#75354=CARTESIAN_POINT('Ctrl Pts',(-19.6512985340453,-20.8599588967214,
-6.17000809224879));
#75355=CARTESIAN_POINT('Ctrl Pts',(-19.6694152821869,-20.8511707302691,
-6.17120336567527));
#75356=CARTESIAN_POINT('Ctrl Pts',(-19.6808242886947,-20.8455086453087,
-6.17195581038795));
#75357=CARTESIAN_POINT('Ctrl Pts',(-19.7368646511553,-20.8170636582214,
-6.17565131416446));
#75358=CARTESIAN_POINT('Ctrl Pts',(-19.7807305318687,-20.7928030130521,
-6.17854200685107));
#75359=CARTESIAN_POINT('Ctrl Pts',(-19.9725202516072,-20.6776559891513,
-6.19124137582172));
#75360=CARTESIAN_POINT('Ctrl Pts',(-20.1097822700602,-20.5703460784515,
-6.2004348615193));
#75361=CARTESIAN_POINT('Ctrl Pts',(-20.2767028854959,-20.4030992219948,
-6.21342110654374));
#75362=CARTESIAN_POINT('Ctrl Pts',(-20.3190029979136,-20.3567723989518,
-6.21691359532654));
#75363=CARTESIAN_POINT('Ctrl Pts',(-20.3790003035009,-20.2848988890064,
-6.22229884916606));
#75364=CARTESIAN_POINT('Ctrl Pts',(-20.3982951711891,-20.2607271690287,
-6.2241048731261));
#75365=CARTESIAN_POINT('Ctrl Pts',(-20.421376504265,-20.2304757904981,-6.22637104482212));
#75366=CARTESIAN_POINT('Ctrl Pts',(-20.4256717695497,-20.2247868772316,
-6.22679745990223));
#75367=CARTESIAN_POINT('Ctrl Pts',(-20.4323832448442,-20.2158037990533,
-6.22747137329916));
#75368=CARTESIAN_POINT('Ctrl Pts',(-20.4348188361803,-20.2125240873201,
-6.22771753952508));
#75369=CARTESIAN_POINT('Ctrl Pts',(-20.4393684434147,-20.2063604976654,
-6.22818043108767));
#75370=CARTESIAN_POINT('Ctrl Pts',(-20.4414846510342,-20.2034783065243,
-6.22839700021274));
#75371=CARTESIAN_POINT('Ctrl Pts',(-20.4463180499241,-20.1968603275623,
-6.22889452790784));
#75372=CARTESIAN_POINT('Ctrl Pts',(-20.4490303145,-20.1931210088653,-6.22917582132584));
#75373=CARTESIAN_POINT('Ctrl Pts',(-20.457396701613,-20.1815067277241,-6.23004998870746));
#75374=CARTESIAN_POINT('Ctrl Pts',(-20.4630088913764,-20.173601911421,-6.23064562817186));
#75375=CARTESIAN_POINT('Ctrl Pts',(-20.5258583291827,-20.083777234927,-6.23741900611765));
#75376=CARTESIAN_POINT('Ctrl Pts',(-20.5772738357686,-19.9979506705685,
-6.24393193266537));
#75377=CARTESIAN_POINT('Ctrl Pts',(-20.6603886086506,-19.8339120813832,
-6.25604820103993));
#75378=CARTESIAN_POINT('Ctrl Pts',(-20.6938230701706,-19.7568678175932,
-6.26161635848641));
#75379=CARTESIAN_POINT('Ctrl Pts',(-20.722580459427,-19.6781107053232,-6.26710642520023));
#75380=CARTESIAN_POINT('',(-20.8509997150768,-18.9509016536907,-5.28730624892625));
#75381=CARTESIAN_POINT('Ctrl Pts',(-20.7225805821268,-19.6781103692884,
-6.04247206352563));
#75382=CARTESIAN_POINT('Ctrl Pts',(-20.7198613276793,-19.6855575244605,
-6.04199074651453));
#75383=CARTESIAN_POINT('Ctrl Pts',(-20.7171002195281,-19.6929894585156,
-6.04151082617329));
#75384=CARTESIAN_POINT('Ctrl Pts',(-20.711464594033,-19.7079014409026,-6.04054865701149));
#75385=CARTESIAN_POINT('Ctrl Pts',(-20.7085892401259,-19.715380995668,-6.04006644838188));
#75386=CARTESIAN_POINT('Ctrl Pts',(-20.7033484419158,-19.728785952518,-6.03920288357619));
#75387=CARTESIAN_POINT('Ctrl Pts',(-20.7009985599696,-19.7347172977286,
-6.03882101045798));
#75388=CARTESIAN_POINT('Ctrl Pts',(-20.6959422695857,-19.7473133163989,
-6.03801050624609));
#75389=CARTESIAN_POINT('Ctrl Pts',(-20.6932286285942,-19.753975014128,-6.03758212482112));
#75390=CARTESIAN_POINT('Ctrl Pts',(-20.6858431534448,-19.7718443371081,
-6.03643369174065));
#75391=CARTESIAN_POINT('Ctrl Pts',(-20.6811087182911,-19.7830259208666,
-6.03571576750528));
#75392=CARTESIAN_POINT('Ctrl Pts',(-20.657151087923,-19.8382791209533,-6.03217087236694));
#75393=CARTESIAN_POINT('Ctrl Pts',(-20.6365257003521,-19.8817296736474,
-6.02939218845373));
#75394=CARTESIAN_POINT('Ctrl Pts',(-20.5374257010067,-20.0733618598878,
-6.01711751652667));
#75395=CARTESIAN_POINT('Ctrl Pts',(-20.4430008541251,-20.2126007647328,
-6.00819945238123));
#75396=CARTESIAN_POINT('Ctrl Pts',(-20.268449046075,-20.4138139274042,-5.9936158203979));
#75397=CARTESIAN_POINT('Ctrl Pts',(-20.1986332455675,-20.4837565623116,
-5.98812314209123));
#75398=CARTESIAN_POINT('Ctrl Pts',(-20.1168931538418,-20.5549315393085,
-5.98170196872616));
#75399=CARTESIAN_POINT('Ctrl Pts',(-20.1095379797514,-20.5612477288602,
-5.98112423045765));
#75400=CARTESIAN_POINT('Ctrl Pts',(-20.0986146017065,-20.5704984797559,
-5.98026584768058));
#75401=CARTESIAN_POINT('Ctrl Pts',(-20.0950796393385,-20.5734723416122,
-5.97998800650598));
#75402=CARTESIAN_POINT('Ctrl Pts',(-20.0887912534957,-20.5787275264372,
-5.97949359408108));
#75403=CARTESIAN_POINT('Ctrl Pts',(-20.08604175398,-20.5810134686683,-5.97927736481212));
#75404=CARTESIAN_POINT('Ctrl Pts',(-20.0801385596345,-20.5858961615167,
-5.97881298399141));
#75405=CARTESIAN_POINT('Ctrl Pts',(-20.0769831836897,-20.5884907137006,
-5.97856468618755));
#75406=CARTESIAN_POINT('Ctrl Pts',(-20.068301446452,-20.5955873752138,-5.9778813537645));
#75407=CARTESIAN_POINT('Ctrl Pts',(-20.062759884528,-20.6000706829207,-5.97744500161648));
#75408=CARTESIAN_POINT('Ctrl Pts',(-20.033057799455,-20.6238534737716,-5.97510573783096));
#75409=CARTESIAN_POINT('Ctrl Pts',(-20.0085005799993,-20.6426487637712,
-5.97317005364767));
#75410=CARTESIAN_POINT('Ctrl Pts',(-19.9329337704002,-20.6979030235584,
-5.9672306842145));
#75411=CARTESIAN_POINT('Ctrl Pts',(-19.880709934652,-20.7326388686644,-5.96314956878737));
#75412=CARTESIAN_POINT('Ctrl Pts',(-19.7118261887119,-20.8344557117345,
-5.95019055033212));
#75413=CARTESIAN_POINT('Ctrl Pts',(-19.5902576457128,-20.8927760311196,
-5.94122489787439));
#75414=CARTESIAN_POINT('Ctrl Pts',(-19.4256424190388,-20.9532464318815,
-5.92993144791107));
#75415=CARTESIAN_POINT('Ctrl Pts',(-19.3869105031309,-20.9662156565853,
-5.92732950143879));
#75416=CARTESIAN_POINT('Ctrl Pts',(-19.3014162200389,-20.9921174902234,
-5.92171052523676));
#75417=CARTESIAN_POINT('Ctrl Pts',(-19.2545346195584,-21.0045800483641,
-5.9187089134785));
#75418=CARTESIAN_POINT('Ctrl Pts',(-19.1949880210372,-21.0182375587605,
-5.91499304460613));
#75419=CARTESIAN_POINT('Ctrl Pts',(-19.1826878316498,-21.0209434127713,
-5.91423057635414));
#75420=CARTESIAN_POINT('Ctrl Pts',(-19.1631556955338,-21.0250578029709,
-5.91302770587397));
#75421=CARTESIAN_POINT('Ctrl Pts',(-19.1559394285447,-21.0265385959881,
-5.912584998256));
#75422=CARTESIAN_POINT('Ctrl Pts',(-19.1424773013202,-21.0292279033673,
-5.91176223329126));
#75423=CARTESIAN_POINT('Ctrl Pts',(-19.1362334578543,-21.0304459855792,
-5.91138187425359));
#75424=CARTESIAN_POINT('Ctrl Pts',(-19.1223512322694,-21.0330893047646,
-5.9105389287685));
#75425=CARTESIAN_POINT('Ctrl Pts',(-19.1147102787907,-21.0345006746932,
-5.9100767889578));
#75426=CARTESIAN_POINT('Ctrl Pts',(-19.0924792252143,-21.0384805552392,
-5.90873741059866));
#75427=CARTESIAN_POINT('Ctrl Pts',(-19.0778695329014,-21.040938061153,-5.90786370346111));
#75428=CARTESIAN_POINT('Ctrl Pts',(-18.9612384320707,-21.0592998936367,
-5.90093809103395));
#75429=CARTESIAN_POINT('Ctrl Pts',(-18.8581971184174,-21.0678755262067,
-5.89512921233333));
#75430=CARTESIAN_POINT('Ctrl Pts',(-18.5952937615171,-21.0704748661084,
-5.88065398522196));
#75431=CARTESIAN_POINT('Ctrl Pts',(-18.436006941572,-21.0539912990993,-5.8722257145276));
#75432=CARTESIAN_POINT('Ctrl Pts',(-18.2326895487442,-21.0093606567924,
-5.86047064271721));
#75433=CARTESIAN_POINT('Ctrl Pts',(-18.1856551300218,-20.9973269068382,
-5.85767577255944));
#75434=CARTESIAN_POINT('Ctrl Pts',(-18.1316340607186,-20.9815084304755,
-5.85433394701235));
#75435=CARTESIAN_POINT('Ctrl Pts',(-18.1242003943299,-20.9792872591053,
-5.85387115419921));
#75436=CARTESIAN_POINT('Ctrl Pts',(-18.1123334864648,-20.9756702663182,
-5.85312741534205));
#75437=CARTESIAN_POINT('Ctrl Pts',(-18.1078922614552,-20.9743005957629,
-5.85284795639191));
#75438=CARTESIAN_POINT('Ctrl Pts',(-18.1000301583745,-20.9718475477278,
-5.85235121012464));
#75439=CARTESIAN_POINT('Ctrl Pts',(-18.0966074820963,-20.9707700845092,
-5.85213427132756));
#75440=CARTESIAN_POINT('Ctrl Pts',(-18.0893539546411,-20.9684663782786,
-5.85167304524102));
#75441=CARTESIAN_POINT('Ctrl Pts',(-18.0855239138788,-20.9672379372249,
-5.85142863566316));
#75442=CARTESIAN_POINT('Ctrl Pts',(-18.0751862144247,-20.9638897184746,
-5.85076663741833));
#75443=CARTESIAN_POINT('Ctrl Pts',(-18.0686853620824,-20.9617493060037,
-5.85034786238183));
#75444=CARTESIAN_POINT('Ctrl Pts',(-18.0363462607953,-20.9509275234716,
-5.84825266424105));
#75445=CARTESIAN_POINT('Ctrl Pts',(-18.0106682735654,-20.9417796446503,
-5.84655090551181));
#75446=CARTESIAN_POINT('Ctrl Pts',(-17.9367556887233,-20.9138282986456,
-5.84155567797127));
#75447=CARTESIAN_POINT('Ctrl Pts',(-17.8890268916447,-20.8937488226499,
-5.8382090057249));
#75448=CARTESIAN_POINT('Ctrl Pts',(-17.7166866316975,-20.8136876544287,
-5.82578742191394));
#75449=CARTESIAN_POINT('Ctrl Pts',(-17.5972859045534,-20.7432823710876,
-5.81654128797264));
#75450=CARTESIAN_POINT('Ctrl Pts',(-17.4531220622001,-20.6380184934663,
-5.80498306959785));
#75451=CARTESIAN_POINT('Ctrl Pts',(-17.4213206238985,-20.6133788836463,
-5.80240339928618));
#75452=CARTESIAN_POINT('Ctrl Pts',(-17.3446605537976,-20.5504067313845,
-5.79611643858223));
#75453=CARTESIAN_POINT('Ctrl Pts',(-17.3006635986976,-20.511075371361,-5.7924477674415));
#75454=CARTESIAN_POINT('Ctrl Pts',(-17.2495974566835,-20.4614328555569,
-5.78811126925235));
#75455=CARTESIAN_POINT('Ctrl Pts',(-17.2409054344102,-20.4528354620286,
-5.78737020289195));
#75456=CARTESIAN_POINT('Ctrl Pts',(-17.226702324861,-20.4385414638611,-5.78615421854932));
#75457=CARTESIAN_POINT('Ctrl Pts',(-17.2211479739558,-20.4328884344259,
-5.7856773888439));
#75458=CARTESIAN_POINT('Ctrl Pts',(-17.2111852191959,-20.4226341303159,
-5.78481969216978));
#75459=CARTESIAN_POINT('Ctrl Pts',(-17.2067656191817,-20.4180439111116,
-5.78443833715607));
#75460=CARTESIAN_POINT('Ctrl Pts',(-17.1973608827445,-20.4081874214596,
-5.78362492011295));
#75461=CARTESIAN_POINT('Ctrl Pts',(-17.1923819338307,-20.4029153397648,
-5.78319312868977));
#75462=CARTESIAN_POINT('Ctrl Pts',(-17.1789583927564,-20.3885543895332,
-5.78202574705693));
#75463=CARTESIAN_POINT('Ctrl Pts',(-17.1705663641182,-20.3794166141702,
-5.78129240919149));
#75464=CARTESIAN_POINT('Ctrl Pts',(-17.1277906707188,-20.3320098848024,
-5.77753527178085));
#75465=CARTESIAN_POINT('Ctrl Pts',(-17.0947282909668,-20.2925687542299,
-5.77456717922136));
#75466=CARTESIAN_POINT('Ctrl Pts',(-16.9574786046277,-20.1161587534877,
-5.76188221478874));
#75467=CARTESIAN_POINT('Ctrl Pts',(-16.8687774004017,-19.9679914318969,
-5.75276386095583));
#75468=CARTESIAN_POINT('Ctrl Pts',(-16.7622678956206,-19.7279862790549,
-5.73833990504607));
#75469=CARTESIAN_POINT('Ctrl Pts',(-16.7309001330982,-19.6429913259418,
-5.73327612219215));
#75470=CARTESIAN_POINT('Ctrl Pts',(-16.7023135357154,-19.5470062078873,
-5.72734232094472));
#75471=CARTESIAN_POINT('Ctrl Pts',(-16.6996202589123,-19.5377314552345,
-5.7267667652014));
#75472=CARTESIAN_POINT('Ctrl Pts',(-16.6957347023549,-19.5240007430237,
-5.72591101727965));
#75473=CARTESIAN_POINT('Ctrl Pts',(-16.6944933295053,-19.5195586433914,
-5.72563360367855));
#75474=CARTESIAN_POINT('Ctrl Pts',(-16.6923155684646,-19.5116663849891,
-5.72513966287343));
#75475=CARTESIAN_POINT('Ctrl Pts',(-16.6913733927432,-19.5082178741954,
-5.72492347522903));
#75476=CARTESIAN_POINT('Ctrl Pts',(-16.6893720889957,-19.5008191242431,
-5.72445885615565));
#75477=CARTESIAN_POINT('Ctrl Pts',(-16.6883156872461,-19.4968682570044,
-5.72421027676385));
#75478=CARTESIAN_POINT('Ctrl Pts',(-16.6854441713462,-19.4860029229224,
-5.72352539355565));
#75479=CARTESIAN_POINT('Ctrl Pts',(-16.6836526419961,-19.4790823588084,
-5.72308776244723));
#75480=CARTESIAN_POINT('Ctrl Pts',(-16.6742279538407,-19.4419001464867,
-5.72072948001408));
#75481=CARTESIAN_POINT('Ctrl Pts',(-16.6672300736544,-19.4114832617611,
-5.71877543470159));
#75482=CARTESIAN_POINT('Ctrl Pts',(-16.6277110565621,-19.2204787233204,
-5.7063968597271));
#75483=CARTESIAN_POINT('Ctrl Pts',(-16.6132534093868,-19.0567262630695,
-5.69536058959103));
#75484=CARTESIAN_POINT('Ctrl Pts',(-16.6210919675133,-18.7758322166447,
-5.67700329075265));
#75485=CARTESIAN_POINT('Ctrl Pts',(-16.6340766898099,-18.6591768353486,
-5.6695392360968));
#75486=CARTESIAN_POINT('Ctrl Pts',(-16.6594065810645,-18.530152324898,-5.66151057757297));
#75487=CARTESIAN_POINT('Ctrl Pts',(-16.6623022073903,-18.5161541709416,
-5.66064232264771));
#75488=CARTESIAN_POINT('Ctrl Pts',(-16.6671361131119,-18.4939233971635,
-5.65926765737429));
#75489=CARTESIAN_POINT('Ctrl Pts',(-16.6689822908034,-18.4856713981177,
-5.65875831659285));
#75490=CARTESIAN_POINT('Ctrl Pts',(-16.6723253377142,-18.4711379835352,
-5.6578628452105));
#75491=CARTESIAN_POINT('Ctrl Pts',(-16.6738015868424,-18.464851981585,-5.65747605805226));
#75492=CARTESIAN_POINT('Ctrl Pts',(-16.6769142498729,-18.4518652257022,
-5.65667800713446));
#75493=CARTESIAN_POINT('Ctrl Pts',(-16.678554700752,-18.4451655108729,-5.65626687853038));
#75494=CARTESIAN_POINT('Ctrl Pts',(-16.6828491740303,-18.4279903974839,
-5.65521434301624));
#75495=CARTESIAN_POINT('Ctrl Pts',(-16.685550733427,-18.4175270042033,-5.65457447640615));
#75496=CARTESIAN_POINT('Ctrl Pts',(-16.6971570196483,-18.3739558282852,
-5.65191519260697));
#75497=CARTESIAN_POINT('Ctrl Pts',(-16.7067855018262,-18.3410450379083,
-5.64991927298028));
#75498=CARTESIAN_POINT('Ctrl Pts',(-16.7339485491348,-18.2559291679024,
-5.64477901105708));
#75499=CARTESIAN_POINT('Ctrl Pts',(-16.7527281729848,-18.2041477412728,
-5.64167398117025));
#75500=CARTESIAN_POINT('Ctrl Pts',(-16.8147534794709,-18.0519278133802,
-5.63253398323416));
#75501=CARTESIAN_POINT('Ctrl Pts',(-16.8637797234717,-17.9540450145168,
-5.62664775917396));
#75502=CARTESIAN_POINT('Ctrl Pts',(-16.9416255080197,-17.8246943657777,
-5.61842857635207));
#75503=CARTESIAN_POINT('Ctrl Pts',(-16.964153940979,-17.7896450327833,-5.61615173333929));
#75504=CARTESIAN_POINT('Ctrl Pts',(-17.0311691688804,-17.6918535530327,
-5.60959402237034));
#75505=CARTESIAN_POINT('Ctrl Pts',(-17.0780562126549,-17.6308454345246,
-5.60525295951788));
#75506=CARTESIAN_POINT('Ctrl Pts',(-17.1343452729096,-17.5653190284406,
-5.60013340262089));
#75507=CARTESIAN_POINT('Ctrl Pts',(-17.1405878546146,-17.5581502627241,
-5.59956679206036));
#75508=CARTESIAN_POINT('Ctrl Pts',(-17.1499110353158,-17.5475883251614,
-5.59872185141719));
#75509=CARTESIAN_POINT('Ctrl Pts',(-17.1529548136374,-17.54416260945,-5.5984461995367));
#75510=CARTESIAN_POINT('Ctrl Pts',(-17.1583908761751,-17.5380842852842,
-5.59795419332101));
#75511=CARTESIAN_POINT('Ctrl Pts',(-17.1607787746501,-17.535427822072,-5.59773816856348));
#75512=CARTESIAN_POINT('Ctrl Pts',(-17.1659280394438,-17.5297285033819,
-5.59727252853963));
#75513=CARTESIAN_POINT('Ctrl Pts',(-17.1686915042528,-17.5266876847324,
-5.59702275810791));
#75514=CARTESIAN_POINT('Ctrl Pts',(-17.1763461053308,-17.5183139437054,
-5.59633130563363));
#75515=CARTESIAN_POINT('Ctrl Pts',(-17.1812557056297,-17.5129980832504,
-5.59588825459382));
#75516=CARTESIAN_POINT('Ctrl Pts',(-17.2083373842509,-17.4839754087953,
-5.59344728684747));
#75517=CARTESIAN_POINT('Ctrl Pts',(-17.2310239128924,-17.4607571520029,
-5.59141320372699));
#75518=CARTESIAN_POINT('Ctrl Pts',(-17.3706342740981,-17.3242971697599,
-5.57900885727586));
#75519=CARTESIAN_POINT('Ctrl Pts',(-17.4997640738172,-17.2243298334111,
-5.56804743882401));
#75520=CARTESIAN_POINT('Ctrl Pts',(-17.739058298427,-17.0797210381389,-5.54978433289827));
#75521=CARTESIAN_POINT('Ctrl Pts',(-17.8438879987841,-17.0276700036513,
-5.54234245908303));
#75522=CARTESIAN_POINT('Ctrl Pts',(-17.9657765590723,-16.9792541960539,
-5.53433428229327));
#75523=CARTESIAN_POINT('Ctrl Pts',(-17.9791124357856,-16.9741127324091,
-5.53346614086503));
#75524=CARTESIAN_POINT('Ctrl Pts',(-18.0004192888552,-16.9661450626522,
-5.53209162075742));
#75525=CARTESIAN_POINT('Ctrl Pts',(-18.0083567183911,-16.9632309528131,
-5.53158231260737));
#75526=CARTESIAN_POINT('Ctrl Pts',(-18.0223859693702,-16.9581754936131,
-5.53068687918324));
#75527=CARTESIAN_POINT('Ctrl Pts',(-18.0284704879456,-16.956014328731,-5.53030009752698));
#75528=CARTESIAN_POINT('Ctrl Pts',(-18.0410752470856,-16.9516020731792,
-5.52950203937665));
#75529=CARTESIAN_POINT('Ctrl Pts',(-18.0475968000327,-16.9493549421735,
-5.5290908981296));
#75530=CARTESIAN_POINT('Ctrl Pts',(-18.0643640190189,-16.9436689892503,
-5.52803829178658));
#75531=CARTESIAN_POINT('Ctrl Pts',(-18.0746253254795,-16.9402766490095,
-5.52739836739773));
#75532=CARTESIAN_POINT('Ctrl Pts',(-18.1175532159352,-16.9264486323259,
-5.52473852225137));
#75533=CARTESIAN_POINT('Ctrl Pts',(-18.1504460339223,-16.9167285326677,
-5.52274211172097));
#75534=CARTESIAN_POINT('Ctrl Pts',(-18.2367448549157,-16.8934908737408,
-5.51760029990378));
#75535=CARTESIAN_POINT('Ctrl Pts',(-18.2904687928593,-16.8812505668078,
-5.51449424212405));
#75536=CARTESIAN_POINT('Ctrl Pts',(-18.4520702392655,-16.8510106601424,
-5.50535245073789));
#75537=CARTESIAN_POINT('Ctrl Pts',(-18.5609275332916,-16.8392559540426,
-5.49946545520543));
#75538=CARTESIAN_POINT('Ctrl Pts',(-18.7135737336649,-16.8346539491919,
-5.49115109301115));
#75539=CARTESIAN_POINT('Ctrl Pts',(-18.7569710264611,-16.8346800745713,
-5.48877924591538));
#75540=CARTESIAN_POINT('Ctrl Pts',(-18.8292972566213,-16.8369475101901,
-5.48477243494056));
#75541=CARTESIAN_POINT('Ctrl Pts',(-18.8582363099455,-16.8384499454004,
-5.48315476497162));
#75542=CARTESIAN_POINT('Ctrl Pts',(-18.9346302399487,-16.8439904591386,
-5.4788257899165));
#75543=CARTESIAN_POINT('Ctrl Pts',(-18.9819924562815,-16.8490364456496,
-5.47608199229976));
#75544=CARTESIAN_POINT('Ctrl Pts',(-19.0367858363314,-16.8567507661122,
-5.47279662993194));
#75545=CARTESIAN_POINT('Ctrl Pts',(-19.0444254167679,-16.8578689937587,
-5.47233604094988));
#75546=CARTESIAN_POINT('Ctrl Pts',(-19.0566426431864,-16.8597255859386,
-5.47159517480974));
#75547=CARTESIAN_POINT('Ctrl Pts',(-19.0612243583322,-16.8604372547504,
-5.47131636665814));
#75548=CARTESIAN_POINT('Ctrl Pts',(-19.0693462033892,-16.8617261448277,
-5.47082035706679));
#75549=CARTESIAN_POINT('Ctrl Pts',(-19.0728872470253,-16.8622973179467,
-5.4706035005397));
#75550=CARTESIAN_POINT('Ctrl Pts',(-19.0804023027107,-16.8635291064289,
-5.4701419743159));
#75551=CARTESIAN_POINT('Ctrl Pts',(-19.08437582362,-16.8641920561954,-5.4698971799282));
#75552=CARTESIAN_POINT('Ctrl Pts',(-19.0951226615497,-16.8660166226016,
-5.4692330761317));
#75553=CARTESIAN_POINT('Ctrl Pts',(-19.1018921854005,-16.8671998742338,
-5.468812567668));
#75554=CARTESIAN_POINT('Ctrl Pts',(-19.1358176007472,-16.873300108826,-5.46669464178307));
#75555=CARTESIAN_POINT('Ctrl Pts',(-19.1628799077318,-16.8787145692043,
-5.46497123826257));
#75556=CARTESIAN_POINT('Ctrl Pts',(-19.2413208806372,-16.8960099601536,
-5.45989180490496));
#75557=CARTESIAN_POINT('Ctrl Pts',(-19.292369163295,-16.9092830237788,-5.4564805846112));
#75558=CARTESIAN_POINT('Ctrl Pts',(-19.4893962962023,-16.9684493731692,
-5.443025941233));
#75559=CARTESIAN_POINT('Ctrl Pts',(-19.630743738301,-17.028213400295,-5.43278495773439));
#75560=CARTESIAN_POINT('Ctrl Pts',(-19.8351666165557,-17.1421157417419,
-5.41775117662028));
#75561=CARTESIAN_POINT('Ctrl Pts',(-19.9036042009194,-17.1855692257347,
-5.41266576978646));
#75562=CARTESIAN_POINT('Ctrl Pts',(-19.9802494915794,-17.2406467292543,
-5.40690975551563));
#75563=CARTESIAN_POINT('Ctrl Pts',(-19.9910345962073,-17.248552950817,-5.40609821615784));
#75564=CARTESIAN_POINT('Ctrl Pts',(-20.0082998157767,-17.2614628123634,
-5.40479630893277));
#75565=CARTESIAN_POINT('Ctrl Pts',(-20.0148269539294,-17.2664026814517,
-5.40430347382937));
#75566=CARTESIAN_POINT('Ctrl Pts',(-20.0262667052871,-17.2751653314715,
-5.4034385049794));
#75567=CARTESIAN_POINT('Ctrl Pts',(-20.0311913849779,-17.2789721295821,
-5.40306574858598));
#75568=CARTESIAN_POINT('Ctrl Pts',(-20.0414189170293,-17.28695036271,-5.40229074539027));
#75569=CARTESIAN_POINT('Ctrl Pts',(-20.046718767995,-17.2911255444738,-5.40188865314042));
#75570=CARTESIAN_POINT('Ctrl Pts',(-20.0603035781497,-17.301933199629,-5.40085666677675));
#75571=CARTESIAN_POINT('Ctrl Pts',(-20.0685588512478,-17.3086028155483,
-5.40022826594452));
#75572=CARTESIAN_POINT('Ctrl Pts',(-20.0864173484392,-17.3232543981682,
-5.39886583046651));
#75573=CARTESIAN_POINT('Ctrl Pts',(-20.0960008459766,-17.331259852644,-5.39813276376099));
#75574=CARTESIAN_POINT('Ctrl Pts',(-20.1235847797125,-17.3547192027848,
-5.39601658069598));
#75575=CARTESIAN_POINT('Ctrl Pts',(-20.1413973090868,-17.3703917415524,
-5.39464226554776));
#75576=CARTESIAN_POINT('Ctrl Pts',(-20.2021281744288,-17.425665033814,-5.38992380358323));
#75577=CARTESIAN_POINT('Ctrl Pts',(-20.2436705206517,-17.4667409547304,
-5.38663873181035));
#75578=CARTESIAN_POINT('Ctrl Pts',(-20.3969219790516,-17.6313544932354,
-5.37416526857529));
#75579=CARTESIAN_POINT('Ctrl Pts',(-20.4955963124143,-17.7661729973952,
-5.36539600128428));
#75580=CARTESIAN_POINT('Ctrl Pts',(-20.6055540151064,-17.9609190737075,
-5.35285736722032));
#75581=CARTESIAN_POINT('Ctrl Pts',(-20.6316259216043,-18.0118029633074,
-5.34958651530647));
#75582=CARTESIAN_POINT('Ctrl Pts',(-20.6593252176873,-18.0717214043159,
-5.34567035599239));
#75583=CARTESIAN_POINT('Ctrl Pts',(-20.6629947229612,-18.0797919098864,
-5.34514155844039));
#75584=CARTESIAN_POINT('Ctrl Pts',(-20.6684560496856,-18.0920062954349,
-5.34433890238172));
#75585=CARTESIAN_POINT('Ctrl Pts',(-20.670285537329,-18.0961333648752,-5.34406729485529));
#75586=CARTESIAN_POINT('Ctrl Pts',(-20.673536575191,-18.1035310311175,-5.34357967327026));
#75587=CARTESIAN_POINT('Ctrl Pts',(-20.6749630741608,-18.1067993953323,
-5.34336396583261));
#75588=CARTESIAN_POINT('Ctrl Pts',(-20.6780343512004,-18.1138850212355,
-5.34289572459172));
#75589=CARTESIAN_POINT('Ctrl Pts',(-20.6796761250838,-18.1177034748547,
-5.34264301807798));
#75590=CARTESIAN_POINT('Ctrl Pts',(-20.6842304188109,-18.1283824531688,
-5.34193529686528));
#75591=CARTESIAN_POINT('Ctrl Pts',(-20.6871179358036,-18.1352534818269,
-5.34147880744297));
#75592=CARTESIAN_POINT('Ctrl Pts',(-20.7036702204672,-18.1752304365363,
-5.33881692638574));
#75593=CARTESIAN_POINT('Ctrl Pts',(-20.7165285144512,-18.2086615378309,
-5.33656739661333));
#75594=CARTESIAN_POINT('Ctrl Pts',(-20.7551281736653,-18.3171568528273,
-5.32922798578443));
#75595=CARTESIAN_POINT('Ctrl Pts',(-20.7774988580308,-18.3933447911045,
-5.32401735506563));
#75596=CARTESIAN_POINT('Ctrl Pts',(-20.8323034292351,-18.628040232454,-5.30810742997659));
#75597=CARTESIAN_POINT('Ctrl Pts',(-20.8509158166609,-18.7891922537898,
-5.2974224999678));
#75598=CARTESIAN_POINT('Ctrl Pts',(-20.8509997150768,-18.9509016536907,
-5.28730624892625));
#75599=CARTESIAN_POINT('Ctrl Pts',(-20.8509997162491,-18.9509039154662,
-5.28730610743365));
#75600=CARTESIAN_POINT('Ctrl Pts',(-20.8510131380821,-18.9768271137295,
-5.28568439929136));
#75601=CARTESIAN_POINT('Ctrl Pts',(-20.8505504063414,-19.0027494389046,
-5.28407670778165));
#75602=CARTESIAN_POINT('Ctrl Pts',(-20.8489736679247,-19.0462644244691,
-5.28140093350177));
#75603=CARTESIAN_POINT('Ctrl Pts',(-20.8481159279852,-19.0638627293641,
-5.28032511708845));
#75604=CARTESIAN_POINT('Ctrl Pts',(-20.8465415703195,-19.0895615458405,
-5.27876302123768));
#75605=CARTESIAN_POINT('Ctrl Pts',(-20.8459978383086,-19.0976715452308,
-5.2782713554403));
#75606=CARTESIAN_POINT('Ctrl Pts',(-20.8449526635068,-19.1120220081581,
-5.27740361134384));
#75607=CARTESIAN_POINT('Ctrl Pts',(-20.844470224362,-19.1182637184008,-5.27702694083171));
#75608=CARTESIAN_POINT('Ctrl Pts',(-20.843461131979,-19.1306063535202,-5.27628355624966));
#75609=CARTESIAN_POINT('Ctrl Pts',(-20.842935681016,-19.1367073128147,-5.27591680815732));
#75610=CARTESIAN_POINT('Ctrl Pts',(-20.8418361314369,-19.1488572085538,
-5.27518781569256));
#75611=CARTESIAN_POINT('Ctrl Pts',(-20.8412624478398,-19.1549061227731,
-5.27482556195104));
#75612=CARTESIAN_POINT('Ctrl Pts',(-20.8398285560976,-19.1693626419309,
-5.2739613853597));
#75613=CARTESIAN_POINT('Ctrl Pts',(-20.838944023514,-19.1777677718445,-5.27346023124555));
#75614=CARTESIAN_POINT('Ctrl Pts',(-20.8360988468823,-19.2033318591447,
-5.27193973537557));
#75615=CARTESIAN_POINT('Ctrl Pts',(-20.8339785147008,-19.2204725858573,
-5.27092540743934));
#75616=CARTESIAN_POINT('Ctrl Pts',(-20.8260337998877,-19.2788270918117,
-5.26748809935229));
#75617=CARTESIAN_POINT('Ctrl Pts',(-20.8192037229416,-19.319895539757,-5.26509636444063));
#75618=CARTESIAN_POINT('Ctrl Pts',(-20.7899098998943,-19.4687639214598,
-5.25649244291624));
#75619=CARTESIAN_POINT('Ctrl Pts',(-20.7602778622481,-19.5748697263155,
-5.25049681220908));
#75620=CARTESIAN_POINT('Ctrl Pts',(-20.7225806512393,-19.6781101800116,
-5.24452704027197));
#75621=CARTESIAN_POINT('Origin',(-18.734,-18.952,0.));
#75622=CARTESIAN_POINT('',(-20.7225805839746,-19.678110364228,-4.44630500845844));
#75623=CARTESIAN_POINT('',(-20.7225805678527,-19.6781104083805,-4.66702139913379));
#75624=CARTESIAN_POINT('',(-20.7225805821191,-19.6781103693095,0.));
#75625=CARTESIAN_POINT('Ctrl Pts',(-20.7225805678527,-19.6781104083805,
-4.66702139913379));
#75626=CARTESIAN_POINT('Ctrl Pts',(-20.7691765609132,-19.550499117769,-4.67446203916752));
#75627=CARTESIAN_POINT('Ctrl Pts',(-20.8033897580608,-19.4186748613786,
-4.68169555986857));
#75628=CARTESIAN_POINT('Ctrl Pts',(-20.830945610111,-19.2453826582096,-4.69152890075376));
#75629=CARTESIAN_POINT('Ctrl Pts',(-20.8360618100052,-19.2061457370852,
-4.69377787057993));
#75630=CARTESIAN_POINT('Ctrl Pts',(-20.8416060206598,-19.1517834556233,
-4.69695251884968));
#75631=CARTESIAN_POINT('Ctrl Pts',(-20.842976080738,-19.1367604708237,-4.69783600284219));
#75632=CARTESIAN_POINT('Ctrl Pts',(-20.8450676748484,-19.1107556837715,
-4.69937794229532));
#75633=CARTESIAN_POINT('Ctrl Pts',(-20.8458643547855,-19.0997803445484,
-4.7000326018113));
#75634=CARTESIAN_POINT('Ctrl Pts',(-20.8468897381308,-19.0839455008159,
-4.70098335630389));
#75635=CARTESIAN_POINT('Ctrl Pts',(-20.8471873278431,-19.0790904286316,
-4.70127570854314));
#75636=CARTESIAN_POINT('Ctrl Pts',(-20.8476764826095,-19.0706328030768,
-4.70178652843945));
#75637=CARTESIAN_POINT('Ctrl Pts',(-20.8478755777288,-19.0670306778501,
-4.70200457442121));
#75638=CARTESIAN_POINT('Ctrl Pts',(-20.8482735902435,-19.0594793970784,
-4.70246271750475));
#75639=CARTESIAN_POINT('Ctrl Pts',(-20.8484706504419,-19.0555302034396,
-4.70270291271344));
#75640=CARTESIAN_POINT('Ctrl Pts',(-20.8489642020017,-19.0450493172144,
-4.70334190839892));
#75641=CARTESIAN_POINT('Ctrl Pts',(-20.8492414963038,-19.038516824435,-4.70374176028672));
#75642=CARTESIAN_POINT('Ctrl Pts',(-20.8502933311571,-19.0106966931555,
-4.70545104988098));
#75643=CARTESIAN_POINT('Ctrl Pts',(-20.8507767750839,-18.9894001258531,
-4.70677554117578));
#75644=CARTESIAN_POINT('Ctrl Pts',(-20.8509781231563,-18.9629269108544,
-4.70843890180712));
#75645=CARTESIAN_POINT('Ctrl Pts',(-20.8509985064309,-18.9577528859984,
-4.70876479897971));
#75646=CARTESIAN_POINT('Ctrl Pts',(-20.8510131829577,-18.9040721336999,
-4.71215398694898));
#75647=CARTESIAN_POINT('Ctrl Pts',(-20.8493592892078,-18.8555823858534,
-4.71528283048994));
#75648=CARTESIAN_POINT('Ctrl Pts',(-20.8326138632352,-18.6113421565125,
-4.73125354343386));
#75649=CARTESIAN_POINT('Ctrl Pts',(-20.7920024717649,-18.4182599620961,
-4.74444618606871));
#75650=CARTESIAN_POINT('Ctrl Pts',(-20.7092042437438,-18.1887683984147,
-4.75978168055878));
#75651=CARTESIAN_POINT('Ctrl Pts',(-20.6915454806286,-18.144553069643,-4.76272646534576));
#75652=CARTESIAN_POINT('Ctrl Pts',(-20.6673796253022,-18.0895101133125,
-4.76638241527231));
#75653=CARTESIAN_POINT('Ctrl Pts',(-20.6622477601342,-18.078097164296,-4.7671399405995));
#75654=CARTESIAN_POINT('Ctrl Pts',(-20.6539422309451,-18.0600555950774,
-4.76833676900666));
#75655=CARTESIAN_POINT('Ctrl Pts',(-20.6508347867218,-18.0533969763163,
-4.76877833878035));
#75656=CARTESIAN_POINT('Ctrl Pts',(-20.6449719414798,-18.041002895943,-4.76960003552102));
#75657=CARTESIAN_POINT('Ctrl Pts',(-20.6422252369273,-18.0352634341076,
-4.76998045774046));
#75658=CARTESIAN_POINT('Ctrl Pts',(-20.6360566854916,-18.0225215950203,
-4.77082485155876));
#75659=CARTESIAN_POINT('Ctrl Pts',(-20.6326219512864,-18.0155255322615,
-4.77128836875544));
#75660=CARTESIAN_POINT('Ctrl Pts',(-20.6224963088177,-17.9951857501949,
-4.77263575676896));
#75661=CARTESIAN_POINT('Ctrl Pts',(-20.6157027231138,-17.9818934615505,
-4.77351603000565));
#75662=CARTESIAN_POINT('Ctrl Pts',(-20.5587597163249,-17.8733282758606,
-4.78070606476363));
#75663=CARTESIAN_POINT('Ctrl Pts',(-20.5015468641977,-17.7819302471413,
-4.78675002458835));
#75664=CARTESIAN_POINT('Ctrl Pts',(-20.3582472358736,-17.587673189725,-4.80001576019911));
#75665=CARTESIAN_POINT('Ctrl Pts',(-20.268862992358,-17.4878417496967,-4.80713451610839));
#75666=CARTESIAN_POINT('Ctrl Pts',(-20.1586113012438,-17.3859728591617,
-4.81548043959687));
#75667=CARTESIAN_POINT('Ctrl Pts',(-20.1464278923326,-17.3749756517987,
-4.81639768451699));
#75668=CARTESIAN_POINT('Ctrl Pts',(-20.0943136527319,-17.329023719481,-4.82030605725783));
#75669=CARTESIAN_POINT('Ctrl Pts',(-20.0532070431934,-17.2954381951771,
-4.82335179591882));
#75670=CARTESIAN_POINT('Ctrl Pts',(-20.0039435818771,-17.2581853521563,
-4.82701711043678));
#75671=CARTESIAN_POINT('Ctrl Pts',(-19.9969687793924,-17.2529783348072,
-4.82753639671103));
#75672=CARTESIAN_POINT('Ctrl Pts',(-19.9863559862622,-17.2451568461038,
-4.82832739005602));
#75673=CARTESIAN_POINT('Ctrl Pts',(-19.9827413826037,-17.2425105946938,
-4.82859694230027));
#75674=CARTESIAN_POINT('Ctrl Pts',(-19.9762362610291,-17.2377798355797,
-4.82908236895107));
#75675=CARTESIAN_POINT('Ctrl Pts',(-19.973348857078,-17.2356911377957,-4.82929794843881));
#75676=CARTESIAN_POINT('Ctrl Pts',(-19.9670611496364,-17.2311668602427,
-4.8297676626275));
#75677=CARTESIAN_POINT('Ctrl Pts',(-19.9636589425287,-17.2287340953903,
-4.83002197954957));
#75678=CARTESIAN_POINT('Ctrl Pts',(-19.9540764340201,-17.2219249019935,
-4.83073867367661));
#75679=CARTESIAN_POINT('Ctrl Pts',(-19.9478798989552,-17.2175715821844,
-4.8312025854209));
#75680=CARTESIAN_POINT('Ctrl Pts',(-19.9105771489598,-17.1916626868087,
-4.83399740183433));
#75681=CARTESIAN_POINT('Ctrl Pts',(-19.8789228841748,-17.170912573062,-4.83637763839291));
#75682=CARTESIAN_POINT('Ctrl Pts',(-19.772643790887,-17.1052481182388,-4.84435386952129));
#75683=CARTESIAN_POINT('Ctrl Pts',(-19.6958061437537,-17.0640909820055,
-4.85009296043012));
#75684=CARTESIAN_POINT('Ctrl Pts',(-19.4572972918382,-16.9546843936829,
-4.86743040953152));
#75685=CARTESIAN_POINT('Ctrl Pts',(-19.2894390514096,-16.9016489409764,
-4.87894076707727));
#75686=CARTESIAN_POINT('Ctrl Pts',(-19.0943175057405,-16.8657619227104,
-4.89115241284343));
#75687=CARTESIAN_POINT('Ctrl Pts',(-19.0716295238202,-16.8619702417863,
-4.89255651866887));
#75688=CARTESIAN_POINT('Ctrl Pts',(-19.0394420665603,-16.8571288101742,
-4.89452689951001));
#75689=CARTESIAN_POINT('Ctrl Pts',(-19.0299909856626,-16.8557725555024,
-4.89510283244979));
#75690=CARTESIAN_POINT('Ctrl Pts',(-19.0146187594493,-16.8536726380584,
-4.89603541559247));
#75691=CARTESIAN_POINT('Ctrl Pts',(-19.0087031542095,-16.852890001875,-4.89639329396217));
#75692=CARTESIAN_POINT('Ctrl Pts',(-18.9963128079649,-16.8513040303786,
-4.89714081000732));
#75693=CARTESIAN_POINT('Ctrl Pts',(-18.9898374946947,-16.8505055927307,
-4.89753028932198));
#75694=CARTESIAN_POINT('Ctrl Pts',(-18.9744228356038,-16.8486771930396,
-4.89845469933594));
#75695=CARTESIAN_POINT('Ctrl Pts',(-18.9654803640939,-16.8476742611929,
-4.89898877271228));
#75696=CARTESIAN_POINT('Ctrl Pts',(-18.9353259461931,-16.8444868754622,
-4.90078247937644));
#75697=CARTESIAN_POINT('Ctrl Pts',(-18.9140870314545,-16.8425658539026,
-4.90203382867938));
#75698=CARTESIAN_POINT('Ctrl Pts',(-18.7982688068135,-16.8338523528477,
-4.90879743545244));
#75699=CARTESIAN_POINT('Ctrl Pts',(-18.7033386434557,-16.8330986696004,
-4.91411649058406));
#75700=CARTESIAN_POINT('Ctrl Pts',(-18.4394827966976,-16.8487470235508,
-4.92865997844835));
#75701=CARTESIAN_POINT('Ctrl Pts',(-18.2721344894038,-16.8790595276087,
-4.93757834575934));
#75702=CARTESIAN_POINT('Ctrl Pts',(-18.073699387599,-16.9402465966317,-4.94942153759797));
#75703=CARTESIAN_POINT('Ctrl Pts',(-18.0375041290859,-16.9524896227224,
-4.95163836765537));
#75704=CARTESIAN_POINT('Ctrl Pts',(-17.9948815496122,-16.9682043581939,
-4.95433857606212));
#75705=CARTESIAN_POINT('Ctrl Pts',(-17.988113533526,-16.970739136838,-4.95477006902078));
#75706=CARTESIAN_POINT('Ctrl Pts',(-17.9771169276943,-16.974921951183,-4.95547580868114));
#75707=CARTESIAN_POINT('Ctrl Pts',(-17.9728803606414,-16.9765490413683,
-4.95574883248008));
#75708=CARTESIAN_POINT('Ctrl Pts',(-17.9653223641581,-16.9794796773338,
-4.95623798003841));
#75709=CARTESIAN_POINT('Ctrl Pts',(-17.9619989686874,-16.9807780088053,
-4.95645378912896));
#75710=CARTESIAN_POINT('Ctrl Pts',(-17.9548271270823,-16.9836007092489,
-4.95692107648361));
#75711=CARTESIAN_POINT('Ctrl Pts',(-17.9509799189032,-16.9851279437539,
-4.95717272114551));
#75712=CARTESIAN_POINT('Ctrl Pts',(-17.9402910535353,-16.9894074564656,
-4.95787454574103));
#75713=CARTESIAN_POINT('Ctrl Pts',(-17.9334593387876,-16.9921841847513,
-4.95832616167301));
#75714=CARTESIAN_POINT('Ctrl Pts',(-17.8947004582634,-17.0081740781143,
-4.96090514637648));
#75715=CARTESIAN_POINT('Ctrl Pts',(-17.8630880106106,-17.0221308532686,
-4.96307356553371));
#75716=CARTESIAN_POINT('Ctrl Pts',(-17.7641680976425,-17.068728989231,-4.97003473754875));
#75717=CARTESIAN_POINT('Ctrl Pts',(-17.6982440524071,-17.1041656731925,
-4.97493571902539));
#75718=CARTESIAN_POINT('Ctrl Pts',(-17.4686237155528,-17.2437491694053,
-4.99265950552603));
#75719=CARTESIAN_POINT('Ctrl Pts',(-17.3174956185351,-17.3668044597351,
-5.00547447246498));
#75720=CARTESIAN_POINT('Ctrl Pts',(-17.1708087165715,-17.5242152144634,
-5.01869370746706));
#75721=CARTESIAN_POINT('Ctrl Pts',(-17.1566211235977,-17.5399049912863,
-5.01998335157798));
#75722=CARTESIAN_POINT('Ctrl Pts',(-17.137194266815,-17.562046978977,-5.02176547919559));
#75723=CARTESIAN_POINT('Ctrl Pts',(-17.1317546068941,-17.5683209716385,
-5.02226631761537));
#75724=CARTESIAN_POINT('Ctrl Pts',(-17.1224238907934,-17.5792116354617,
-5.02312865197092));
#75725=CARTESIAN_POINT('Ctrl Pts',(-17.1185154401928,-17.5838132116645,
-5.0234908652011));
#75726=CARTESIAN_POINT('Ctrl Pts',(-17.1104578906896,-17.5933823535067,
-5.02423970368474));
#75727=CARTESIAN_POINT('Ctrl Pts',(-17.1063117761606,-17.5983523584487,
-5.02462620429654));
#75728=CARTESIAN_POINT('Ctrl Pts',(-17.0966468974293,-17.6100463926137,
-5.02552998315794));
#75729=CARTESIAN_POINT('Ctrl Pts',(-17.0911466283647,-17.6167856091155,
-5.02604650678409));
#75730=CARTESIAN_POINT('Ctrl Pts',(-17.0733869430483,-17.6388215851803,
-5.0277216343407));
#75731=CARTESIAN_POINT('Ctrl Pts',(-17.0612981949239,-17.6542550391029,
-5.02887339664198));
#75732=CARTESIAN_POINT('Ctrl Pts',(-17.0003521246543,-17.7343303634945,
-5.03474408331668));
#75733=CARTESIAN_POINT('Ctrl Pts',(-16.9550180180235,-17.8015742178492,
-5.03932427760283));
#75734=CARTESIAN_POINT('Ctrl Pts',(-16.8275649624743,-18.0162503607255,
-5.05316172570832));
#75735=CARTESIAN_POINT('Ctrl Pts',(-16.7591218671788,-18.170993865104,-5.06203404371519));
#75736=CARTESIAN_POINT('Ctrl Pts',(-16.6939626106512,-18.3838024684258,
-5.07454412732924));
#75737=CARTESIAN_POINT('Ctrl Pts',(-16.6801439271473,-18.4359814291646,
-5.0776392203901));
#75738=CARTESIAN_POINT('Ctrl Pts',(-16.6664208298208,-18.4971573698522,
-5.08135962970058));
#75739=CARTESIAN_POINT('Ctrl Pts',(-16.6645600091364,-18.505700144063,-5.08188121416451));
#75740=CARTESIAN_POINT('Ctrl Pts',(-16.6618241473143,-18.518645204009,-5.08267502688484));
#75741=CARTESIAN_POINT('Ctrl Pts',(-16.6609100756644,-18.5230392693642,
-5.08294507726038));
#75742=CARTESIAN_POINT('Ctrl Pts',(-16.659295173072,-18.5309280520047,-5.08343103368197));
#75743=CARTESIAN_POINT('Ctrl Pts',(-16.658589189201,-18.5344216595742,-5.08364664197009));
#75744=CARTESIAN_POINT('Ctrl Pts',(-16.6570751835372,-18.542012504429,-5.08411598915867));
#75745=CARTESIAN_POINT('Ctrl Pts',(-16.6562704721389,-18.5461103005463,
-5.08436990793588));
#75746=CARTESIAN_POINT('Ctrl Pts',(-16.6540462440104,-18.5576165899978,
-5.08508438019229));
#75747=CARTESIAN_POINT('Ctrl Pts',(-16.6526542085713,-18.5650302418684,
-5.08554645329898));
#75748=CARTESIAN_POINT('Ctrl Pts',(-16.6446091918002,-18.6091756448927,
-5.08830755001023));
#75749=CARTESIAN_POINT('Ctrl Pts',(-16.6388895262453,-18.6460683158044,
-5.09065455983395));
#75750=CARTESIAN_POINT('Ctrl Pts',(-16.6233425450778,-18.7674708982687,
-5.09846553204106));
#75751=CARTESIAN_POINT('Ctrl Pts',(-16.6176332923926,-18.8524210077317,
-5.10406664451242));
#75752=CARTESIAN_POINT('Ctrl Pts',(-16.6158271713325,-19.115707342499,-5.12145998327809));
#75753=CARTESIAN_POINT('Ctrl Pts',(-16.6371175926894,-19.2934160825607,
-5.13317340558461));
#75754=CARTESIAN_POINT('Ctrl Pts',(-16.6859740385284,-19.4884674680425,
-5.14554744331572));
#75755=CARTESIAN_POINT('Ctrl Pts',(-16.6918639708136,-19.5104695023179,
-5.14693756203306));
#75756=CARTESIAN_POINT('Ctrl Pts',(-16.7007152895663,-19.5415190724221,
-5.14889189946053));
#75757=CARTESIAN_POINT('Ctrl Pts',(-16.7033842292597,-19.5506476815881,
-5.14946556413045));
#75758=CARTESIAN_POINT('Ctrl Pts',(-16.7078257583753,-19.5654675773988,
-5.15039547802102));
#75759=CARTESIAN_POINT('Ctrl Pts',(-16.7095610053027,-19.5711698343924,
-5.15075294151145));
#75760=CARTESIAN_POINT('Ctrl Pts',(-16.7132478150417,-19.5831039934743,
-5.15150038777389));
#75761=CARTESIAN_POINT('Ctrl Pts',(-16.715204179666,-19.5893343556317,-5.15189020868588));
#75762=CARTESIAN_POINT('Ctrl Pts',(-16.7199347134666,-19.6041591673668,
-5.15281688090697));
#75763=CARTESIAN_POINT('Ctrl Pts',(-16.7227351250823,-19.6127451587187,
-5.15335286356986));
#75764=CARTESIAN_POINT('Ctrl Pts',(-16.7323932945808,-19.6417264545518,
-5.15515982128339));
#75765=CARTESIAN_POINT('Ctrl Pts',(-16.7395071627998,-19.6620354624039,
-5.1564223419963));
#75766=CARTESIAN_POINT('Ctrl Pts',(-16.8091034175928,-19.8514169975164,
-5.16816955223975));
#75767=CARTESIAN_POINT('Ctrl Pts',(-16.8926263182991,-20.0119658805139,
-5.17784950510681));
#75768=CARTESIAN_POINT('Ctrl Pts',(-17.0637496983472,-20.2582400141959,
-5.19417301241013));
#75769=CARTESIAN_POINT('Ctrl Pts',(-17.1402042650119,-20.3505012982325,
-5.20073948503146));
#75770=CARTESIAN_POINT('Ctrl Pts',(-17.2307011257851,-20.4425945916122,
-5.20839126428913));
#75771=CARTESIAN_POINT('Ctrl Pts',(-17.2374234109787,-20.4493437305056,
-5.20895904648627));
#75772=CARTESIAN_POINT('Ctrl Pts',(-17.247449426917,-20.4592748355662,-5.20980540341093));
#75773=CARTESIAN_POINT('Ctrl Pts',(-17.2507184263142,-20.4624919094522,
-5.21008128688877));
#75774=CARTESIAN_POINT('Ctrl Pts',(-17.256552161142,-20.468195780738,-5.21057354661375));
#75775=CARTESIAN_POINT('Ctrl Pts',(-17.2591127623494,-20.4706867346699,
-5.21078959197053));
#75776=CARTESIAN_POINT('Ctrl Pts',(-17.2646303350937,-20.476027115976,-5.21125509407607));
#75777=CARTESIAN_POINT('Ctrl Pts',(-17.2675892522231,-20.4788743826915,
-5.21150470502881));
#75778=CARTESIAN_POINT('Ctrl Pts',(-17.2757767494028,-20.4867071855417,
-5.2121952769454));
#75779=CARTESIAN_POINT('Ctrl Pts',(-17.281022537944,-20.4916745387342,-5.21263760128345));
#75780=CARTESIAN_POINT('Ctrl Pts',(-17.3098521404919,-20.51869538535,-5.21506728156679));
#75781=CARTESIAN_POINT('Ctrl Pts',(-17.3339113496193,-20.5402326856838,
-5.21709041868506));
#75782=CARTESIAN_POINT('Ctrl Pts',(-17.4822884581557,-20.6670650010254,
-5.22949111444313));
#75783=CARTESIAN_POINT('Ctrl Pts',(-17.6179259216366,-20.7582691633827,
-5.24046260206151));
#75784=CARTESIAN_POINT('Ctrl Pts',(-17.8665680921382,-20.8866632224974,
-5.25874172871462));
#75785=CARTESIAN_POINT('Ctrl Pts',(-17.9747357728673,-20.9316175290176,
-5.26618974429921));
#75786=CARTESIAN_POINT('Ctrl Pts',(-18.0996602058279,-20.9717785821859,
-5.27420185751572));
#75787=CARTESIAN_POINT('Ctrl Pts',(-18.1132848903825,-20.9760072292008,
-5.275068346271));
#75788=CARTESIAN_POINT('Ctrl Pts',(-18.1350443039693,-20.9825202374226,
-5.27644075236257));
#75789=CARTESIAN_POINT('Ctrl Pts',(-18.1431515801917,-20.9848941213038,
-5.27694958516799));
#75790=CARTESIAN_POINT('Ctrl Pts',(-18.1574791314231,-20.9889964070899,
-5.27784446579406));
#75791=CARTESIAN_POINT('Ctrl Pts',(-18.1636934695377,-20.9907449907101,
-5.27823116744733));
#75792=CARTESIAN_POINT('Ctrl Pts',(-18.1765671885943,-20.9943039155187,
-5.279029331701));
#75793=CARTESIAN_POINT('Ctrl Pts',(-18.1832276252643,-20.9961101769564,
-5.27944065771707));
#75794=CARTESIAN_POINT('Ctrl Pts',(-18.2003549537786,-21.0006651929261,
-5.28049429900883));
#75795=CARTESIAN_POINT('Ctrl Pts',(-18.2108343871675,-21.0033663388569,
-5.28113506762424));
#75796=CARTESIAN_POINT('Ctrl Pts',(-18.2547281810703,-21.0143220291703,
-5.2838031282882));
#75797=CARTESIAN_POINT('Ctrl Pts',(-18.2883217226217,-21.0218417089202,
-5.28580672432724));
#75798=CARTESIAN_POINT('Ctrl Pts',(-18.3763829169174,-21.0393100580302,
-5.29097124066264));
#75799=CARTESIAN_POINT('Ctrl Pts',(-18.4310846950575,-21.0479475726715,
-5.29409236020354));
#75800=CARTESIAN_POINT('Ctrl Pts',(-18.594865672738,-21.0672618694223,-5.30326042037942));
#75801=CARTESIAN_POINT('Ctrl Pts',(-18.7045007947106,-21.0716277488065,
-5.30915871255457));
#75802=CARTESIAN_POINT('Ctrl Pts',(-18.8739982842528,-21.0652195180955,
-5.31839460246183));
#75803=CARTESIAN_POINT('Ctrl Pts',(-18.9338894852895,-21.0603974491121,
-5.32168325163462));
#75804=CARTESIAN_POINT('Ctrl Pts',(-19.051583025937,-21.0458615288197,-5.32832474052661));
#75805=CARTESIAN_POINT('Ctrl Pts',(-19.1093464228304,-21.0362813711832,
-5.3316711224459));
#75806=CARTESIAN_POINT('Ctrl Pts',(-19.1753598861204,-21.0224999228472,
-5.3356714603907));
#75807=CARTESIAN_POINT('Ctrl Pts',(-19.1840751004848,-21.0206229422488,
-5.33620317116771));
#75808=CARTESIAN_POINT('Ctrl Pts',(-19.1971954794535,-21.0177103919284,
-5.33700939648203));
#75809=CARTESIAN_POINT('Ctrl Pts',(-19.2016097308295,-21.0167156255202,
-5.33728163019653));
#75810=CARTESIAN_POINT('Ctrl Pts',(-19.2094979154796,-21.0149114028133,
-5.33776992516007));
#75811=CARTESIAN_POINT('Ctrl Pts',(-19.2129730221529,-21.0141073122575,
-5.33798567622846));
#75812=CARTESIAN_POINT('Ctrl Pts',(-19.2204857561669,-21.0123489562675,
-5.33845348976367));
#75813=CARTESIAN_POINT('Ctrl Pts',(-19.2245225594754,-21.0113916165969,
-5.33870572212657));
#75814=CARTESIAN_POINT('Ctrl Pts',(-19.2357692537056,-21.0086894863316,
-5.33941080843201));
#75815=CARTESIAN_POINT('Ctrl Pts',(-19.2429727446804,-21.006918676877,-5.33986511973635));
#75816=CARTESIAN_POINT('Ctrl Pts',(-19.2843476322461,-20.9965167322221,
-5.34248954072507));
#75817=CARTESIAN_POINT('Ctrl Pts',(-19.3183064302945,-20.9870717047429,
-5.34470237886729));
#75818=CARTESIAN_POINT('Ctrl Pts',(-19.4259113774478,-20.9542281709081,
-5.351869160434));
#75819=CARTESIAN_POINT('Ctrl Pts',(-19.4985163961957,-20.927644720345,-5.35693806707062));
#75820=CARTESIAN_POINT('Ctrl Pts',(-19.7398391010537,-20.8239896048735,
-5.37426982775066));
#75821=CARTESIAN_POINT('Ctrl Pts',(-19.8998680925405,-20.7287486842645,
-5.38651055335972));
#75822=CARTESIAN_POINT('Ctrl Pts',(-20.0650216354066,-20.5984178310324,
-5.39948466512282));
#75823=CARTESIAN_POINT('Ctrl Pts',(-20.0843145167135,-20.5826321036715,
-5.40100815747494));
#75824=CARTESIAN_POINT('Ctrl Pts',(-20.1108536419003,-20.5601232872844,
-5.40311585822893));
#75825=CARTESIAN_POINT('Ctrl Pts',(-20.1183378379905,-20.5536851169297,
-5.40371161556621));
#75826=CARTESIAN_POINT('Ctrl Pts',(-20.1303182962737,-20.5432323968035,
-5.40466759882434));
#75827=CARTESIAN_POINT('Ctrl Pts',(-20.1348428614278,-20.5392506430618,
-5.40502917650968));
#75828=CARTESIAN_POINT('Ctrl Pts',(-20.1439056124033,-20.5312062129399,
-5.40575453771887));
#75829=CARTESIAN_POINT('Ctrl Pts',(-20.1484433925525,-20.527143164711,-5.40611830063494));
#75830=CARTESIAN_POINT('Ctrl Pts',(-20.1591474237462,-20.517475408303,-5.40697776366185));
#75831=CARTESIAN_POINT('Ctrl Pts',(-20.1652982732665,-20.5118537397415,
-5.40747274187518));
#75832=CARTESIAN_POINT('Ctrl Pts',(-20.1844111719896,-20.4941769562572,
-5.40901443777274));
#75833=CARTESIAN_POINT('Ctrl Pts',(-20.1972555320385,-20.481995296866,-5.41005574820745));
#75834=CARTESIAN_POINT('Ctrl Pts',(-20.2267942716557,-20.4532683338876,
-5.41246410561028));
#75835=CARTESIAN_POINT('Ctrl Pts',(-20.243369074385,-20.4366031143289,-5.41382590490901));
#75836=CARTESIAN_POINT('Ctrl Pts',(-20.2996028027923,-20.3781471656349,
-5.41848799285678));
#75837=CARTESIAN_POINT('Ctrl Pts',(-20.3378326805298,-20.3350145802317,
-5.42173082938301));
#75838=CARTESIAN_POINT('Ctrl Pts',(-20.4753967613963,-20.1664214927511,
-5.43380595582215));
#75839=CARTESIAN_POINT('Ctrl Pts',(-20.5621526223952,-20.0314143648029,
-5.44225421016962));
#75840=CARTESIAN_POINT('Ctrl Pts',(-20.6392394613238,-19.8750162295932,
-5.45197646644191));
#75841=CARTESIAN_POINT('Ctrl Pts',(-20.6454737662907,-19.8620353795311,
-5.45278327657294));
#75842=CARTESIAN_POINT('Ctrl Pts',(-20.6532775002094,-19.8453526858455,
-5.45382122623665));
#75843=CARTESIAN_POINT('Ctrl Pts',(-20.6549695786014,-19.8417083914765,
-5.45404802790572));
#75844=CARTESIAN_POINT('Ctrl Pts',(-20.6763865889926,-19.7952358347431,
-5.45694131536283));
#75845=CARTESIAN_POINT('Ctrl Pts',(-20.6946840974345,-19.7517683888456,
-5.45965908549561));
#75846=CARTESIAN_POINT('Ctrl Pts',(-20.7142605909899,-19.7005427147481,
-5.46291526173001));
#75847=CARTESIAN_POINT('Ctrl Pts',(-20.7169681034621,-19.6933404754991,
-5.46337428170636));
#75848=CARTESIAN_POINT('Ctrl Pts',(-20.7206230839558,-19.6834545923031,
-5.464006196137));
#75849=CARTESIAN_POINT('Ctrl Pts',(-20.7216045310241,-19.6807834564002,
-5.46417712267594));
#75850=CARTESIAN_POINT('Ctrl Pts',(-20.7225805821191,-19.6781103693095,
-5.46434836675477));
#75851=CARTESIAN_POINT('Ctrl Pts',(-20.7225806512393,-19.6781101800116,
-5.24452704027197));
#75852=CARTESIAN_POINT('Ctrl Pts',(-20.701412508508,-19.7360828682028,-5.24117482982837));
#75853=CARTESIAN_POINT('Ctrl Pts',(-20.6777012517521,-19.7931519033798,
-5.23782819558385));
#75854=CARTESIAN_POINT('Ctrl Pts',(-20.6249328031585,-19.9059353994099,
-5.23098485563475));
#75855=CARTESIAN_POINT('Ctrl Pts',(-20.5958562751286,-19.9615096209843,
-5.22749301409946));
#75856=CARTESIAN_POINT('Ctrl Pts',(-20.5488219989097,-20.0424431755143,
-5.22210866281003));
#75857=CARTESIAN_POINT('Ctrl Pts',(-20.5327016317153,-20.0688336580986,
-5.2203028599762));
#75858=CARTESIAN_POINT('Ctrl Pts',(-20.5121619813386,-20.1008602082743,
-5.21803693468279));
#75859=CARTESIAN_POINT('Ctrl Pts',(-20.5082836583955,-20.1068408142658,
-5.21761053618827));
#75860=CARTESIAN_POINT('Ctrl Pts',(-20.5021352896038,-20.1162178859737,
-5.21693664317567));
#75861=CARTESIAN_POINT('Ctrl Pts',(-20.4998854482371,-20.1196276253236,
-5.21669048061429));
#75862=CARTESIAN_POINT('Ctrl Pts',(-20.4956478281365,-20.126009674404,-5.21622759205944));
#75863=CARTESIAN_POINT('Ctrl Pts',(-20.4936623833027,-20.1289834672085,
-5.21601102225427));
#75864=CARTESIAN_POINT('Ctrl Pts',(-20.489094629283,-20.135787642446,-5.2155134878238));
#75865=CARTESIAN_POINT('Ctrl Pts',(-20.4865073176134,-20.1396146011748,
-5.21523218831693));
#75866=CARTESIAN_POINT('Ctrl Pts',(-20.4784512074551,-20.1514469472664,
-5.21435798358808));
#75867=CARTESIAN_POINT('Ctrl Pts',(-20.4729400168071,-20.1594231256028,
-5.21376231253154));
#75868=CARTESIAN_POINT('Ctrl Pts',(-20.4106714931198,-20.2482318523178,
-5.20706093232178));
#75869=CARTESIAN_POINT('Ctrl Pts',(-20.348384924969,-20.325026218361,-5.20062766912869));
#75870=CARTESIAN_POINT('Ctrl Pts',(-20.166459304275,-20.5197658532761,-5.18307321918491));
#75871=CARTESIAN_POINT('Ctrl Pts',(-20.0377573524291,-20.6283241657014,
-5.17192751593069));
#75872=CARTESIAN_POINT('Ctrl Pts',(-19.871209325056,-20.7379003579268,-5.15940136273166));
#75873=CARTESIAN_POINT('Ctrl Pts',(-19.8444569005771,-20.7546565880787,
-5.1574387430459));
#75874=CARTESIAN_POINT('Ctrl Pts',(-19.8041717030768,-20.7786516911934,
-5.15455521984329));
#75875=CARTESIAN_POINT('Ctrl Pts',(-19.7909197325146,-20.7863512677238,
-5.15361791191717));
#75876=CARTESIAN_POINT('Ctrl Pts',(-19.766647314889,-20.8001035037864,-5.15192121243094));
#75877=CARTESIAN_POINT('Ctrl Pts',(-19.7556544276193,-20.8062031385127,
-5.15116015889834));
#75878=CARTESIAN_POINT('Ctrl Pts',(-19.7382624440951,-20.8156518152792,
-5.14996747465325));
#75879=CARTESIAN_POINT('Ctrl Pts',(-19.731899561837,-20.8190665793456,-5.14953350372701));
#75880=CARTESIAN_POINT('Ctrl Pts',(-19.7254731395678,-20.8224732065016,
-5.14909755972947));
#75881=CARTESIAN_POINT('Ctrl Pts',(-19.7254270075463,-20.8224976587616,
-5.14909443043108));
#75882=CARTESIAN_POINT('Ctrl Pts',(-19.7253331174823,-20.8225474207042,
-5.14908806178418));
#75883=CARTESIAN_POINT('Ctrl Pts',(-19.7252853582169,-20.8225727308782,
-5.14908482236145));
#75884=CARTESIAN_POINT('Ctrl Pts',(-19.725188154278,-20.8226242396454,-5.14907822946432));
#75885=CARTESIAN_POINT('Ctrl Pts',(-19.7251387087258,-20.8226504385362,
-5.14907487593968));
#75886=CARTESIAN_POINT('Ctrl Pts',(-19.7250380707156,-20.8227037568112,
-5.1490680506963));
#75887=CARTESIAN_POINT('Ctrl Pts',(-19.7249868772868,-20.8227308765295,
-5.14906457892176));
#75888=CARTESIAN_POINT('Ctrl Pts',(-19.7248826796944,-20.8227860697253,
-5.14905751288047));
#75889=CARTESIAN_POINT('Ctrl Pts',(-19.7248296747771,-20.8228141434087,
-5.14905391857337));
#75890=CARTESIAN_POINT('Ctrl Pts',(-19.7247217880893,-20.8228712789663,
-5.14904660301622));
#75891=CARTESIAN_POINT('Ctrl Pts',(-19.7246669055455,-20.8229003410425,
-5.1490428817253));
#75892=CARTESIAN_POINT('Ctrl Pts',(-19.7245551950909,-20.8229594890356,
-5.1490353075901));
#75893=CARTESIAN_POINT('Ctrl Pts',(-19.7244983664698,-20.8229895751058,
-5.14903145471009));
#75894=CARTESIAN_POINT('Ctrl Pts',(-19.724382693013,-20.8230508079185,-5.14902361263113));
#75895=CARTESIAN_POINT('Ctrl Pts',(-19.7243238472484,-20.8230819549137,
-5.14901962338252));
#75896=CARTESIAN_POINT('Ctrl Pts',(-19.7242040658153,-20.8231453478539,
-5.14901150361136));
#75897=CARTESIAN_POINT('Ctrl Pts',(-19.7241431295488,-20.823177593859,-5.14900737306257));
#75898=CARTESIAN_POINT('Ctrl Pts',(-19.7240190907779,-20.8232432244343,
-5.1489989655602));
#75899=CARTESIAN_POINT('Ctrl Pts',(-19.7239559877364,-20.8232766090135,
-5.14899468858556));
#75900=CARTESIAN_POINT('Ctrl Pts',(-19.7238275365145,-20.8233445576436,
-5.14898598293039));
#75901=CARTESIAN_POINT('Ctrl Pts',(-19.7237621877721,-20.8233791216965,
-5.14898155422824));
#75902=CARTESIAN_POINT('Ctrl Pts',(-19.7236291613103,-20.8234494727203,
-5.14897253948635));
#75903=CARTESIAN_POINT('Ctrl Pts',(-19.7235614862716,-20.8234852579563,
-5.14896795364603));
#75904=CARTESIAN_POINT('Ctrl Pts',(-19.7234348771654,-20.8235521975867,
-5.14895937476716));
#75905=CARTESIAN_POINT('Ctrl Pts',(-19.7233759422767,-20.8235833535505,
-5.14895538160964));
#75906=CARTESIAN_POINT('Ctrl Pts',(-19.72324832144,-20.8236508126687,-5.14894673503811));
#75907=CARTESIAN_POINT('Ctrl Pts',(-19.7231796338908,-20.8236871153938,
-5.14894208158675));
#75908=CARTESIAN_POINT('Ctrl Pts',(-19.7230309113934,-20.8237657076947,
-5.14893200650377));
#75909=CARTESIAN_POINT('Ctrl Pts',(-19.72295087472,-20.8238079964528,-5.14892658485174));
#75910=CARTESIAN_POINT('Ctrl Pts',(-19.7227776039674,-20.8238995328303,
-5.14891484835399));
#75911=CARTESIAN_POINT('Ctrl Pts',(-19.7226843682897,-20.8239487789514,
-5.14890853353066));
#75912=CARTESIAN_POINT('Ctrl Pts',(-19.7224825594817,-20.8240553529944,
-5.14889486615894));
#75913=CARTESIAN_POINT('Ctrl Pts',(-19.7223739845068,-20.8241126787202,
-5.14888751366245));
#75914=CARTESIAN_POINT('Ctrl Pts',(-19.7221390264431,-20.8242367064135,
-5.14887160419482));
#75915=CARTESIAN_POINT('Ctrl Pts',(-19.7220126419178,-20.8243034048552,
-5.14886304736537));
#75916=CARTESIAN_POINT('Ctrl Pts',(-19.7217267158614,-20.8244542630756,
-5.14884369088451));
#75917=CARTESIAN_POINT('Ctrl Pts',(-19.7215671702725,-20.8245384152899,
-5.14883289149962));
#75918=CARTESIAN_POINT('Ctrl Pts',(-19.7156957099711,-20.8276343539857,
-5.14843551524378));
#75919=CARTESIAN_POINT('Ctrl Pts',(-19.709970007852,-20.8306200366296,-5.14804986596609));
#75920=CARTESIAN_POINT('Ctrl Pts',(-19.6967131593703,-20.8374558897946,
-5.14716120869103));
#75921=CARTESIAN_POINT('Ctrl Pts',(-19.6891723883767,-20.8412872336508,
-5.14665886789929));
#75922=CARTESIAN_POINT('Ctrl Pts',(-19.6688197918885,-20.8514750582571,
-5.14531135253574));
#75923=CARTESIAN_POINT('Ctrl Pts',(-19.6559660407866,-20.8577471434665,
-5.14446912563664));
#75924=CARTESIAN_POINT('Ctrl Pts',(-19.5375051525996,-20.9140719774847,
-5.13678489397074));
#75925=CARTESIAN_POINT('Ctrl Pts',(-19.4279803503686,-20.9554329321603,
-5.13025973450201));
#75926=CARTESIAN_POINT('Ctrl Pts',(-19.1589144830927,-21.0323093763631,
-5.11494068576974));
#75927=CARTESIAN_POINT('Ctrl Pts',(-18.9976163601083,-21.0588302951818,
-5.10633050195121));
#75928=CARTESIAN_POINT('Ctrl Pts',(-18.802657888277,-21.0681324864585,-5.09512065436378));
#75929=CARTESIAN_POINT('Ctrl Pts',(-18.7703916462459,-21.0689331585919,
-5.09323794340659));
#75930=CARTESIAN_POINT('Ctrl Pts',(-18.7308982435761,-21.069010051562,-5.09088638021151));
#75931=CARTESIAN_POINT('Ctrl Pts',(-18.7236748263827,-21.0689871437202,
-5.09045434401347));
#75932=CARTESIAN_POINT('Ctrl Pts',(-18.7123457678714,-21.0688932317858,
-5.08977352241842));
#75933=CARTESIAN_POINT('Ctrl Pts',(-18.7082398968279,-21.0688472493251,
-5.08952611497209));
#75934=CARTESIAN_POINT('Ctrl Pts',(-18.7005621239105,-21.0687389236498,
-5.08906218984495));
#75935=CARTESIAN_POINT('Ctrl Pts',(-18.6969902372455,-21.0686794842991,
-5.08884583621685));
#75936=CARTESIAN_POINT('Ctrl Pts',(-18.6888325025982,-21.068523077253,-5.08835052346686));
#75937=CARTESIAN_POINT('Ctrl Pts',(-18.684246824114,-21.0684202465344,-5.08807124063714));
#75938=CARTESIAN_POINT('Ctrl Pts',(-18.6701371321334,-21.068057964413,-5.08720936039492));
#75939=CARTESIAN_POINT('Ctrl Pts',(-18.6606146606291,-21.0677491247349,
-5.08662410618977));
#75940=CARTESIAN_POINT('Ctrl Pts',(-18.5315868426045,-21.0626923044512,
-5.07864842441961));
#75941=CARTESIAN_POINT('Ctrl Pts',(-18.4127041625726,-21.0478901317207,
-5.07078117013936));
#75942=CARTESIAN_POINT('Ctrl Pts',(-18.1891105519226,-21.0005750194232,
-5.05568285004451));
#75943=CARTESIAN_POINT('Ctrl Pts',(-18.0843911619887,-20.9698146482621,
-5.04847967986346));
#75944=CARTESIAN_POINT('Ctrl Pts',(-17.9123447350746,-20.9044863820415,
-5.03665529331572));
#75945=CARTESIAN_POINT('Ctrl Pts',(-17.8436493653112,-20.8741337988686,
-5.03193390296942));
#75946=CARTESIAN_POINT('Ctrl Pts',(-17.7599283654259,-20.8316880653889,
-5.02618361841979));
#75947=CARTESIAN_POINT('Ctrl Pts',(-17.743266084539,-20.8229594108491,-5.02503920847367));
#75948=CARTESIAN_POINT('Ctrl Pts',(-17.7191977435569,-20.8099393318205,
-5.02338571958801));
#75949=CARTESIAN_POINT('Ctrl Pts',(-17.7116982316541,-20.8058234215264,
-5.02287044425809));
#75950=CARTESIAN_POINT('Ctrl Pts',(-17.698588966041,-20.7985250021227,-5.02196956096895));
#75951=CARTESIAN_POINT('Ctrl Pts',(-17.6929684619539,-20.7953621269109,
-5.02158325704022));
#75952=CARTESIAN_POINT('Ctrl Pts',(-17.6820796660661,-20.7891688945382,
-5.0208347107161));
#75953=CARTESIAN_POINT('Ctrl Pts',(-17.676809803319,-20.7861414409006,-5.02047236877512));
#75954=CARTESIAN_POINT('Ctrl Pts',(-17.6642380443395,-20.778846978069,-5.01960776566425));
#75955=CARTESIAN_POINT('Ctrl Pts',(-17.6569485004485,-20.7745588038596,
-5.01910627497618));
#75956=CARTESIAN_POINT('Ctrl Pts',(-17.6307077474832,-20.7589099063787,
-5.01730024107344));
#75957=CARTESIAN_POINT('Ctrl Pts',(-17.6119085675366,-20.7472960969243,
-5.01600492121));
#75958=CARTESIAN_POINT('Ctrl Pts',(-17.4368585585138,-20.6353292242278,
-5.00391935116773));
#75959=CARTESIAN_POINT('Ctrl Pts',(-17.2942716497095,-20.5151255478294,
-4.99398693202737));
#75960=CARTESIAN_POINT('Ctrl Pts',(-17.1152599276401,-20.3186676595058,
-4.97949760014236));
#75961=CARTESIAN_POINT('Ctrl Pts',(-17.0647371429149,-20.2564766861742,
-4.97509416313345));
#75962=CARTESIAN_POINT('Ctrl Pts',(-16.996776374576,-20.1623882895478,-4.96845494489296));
#75963=CARTESIAN_POINT('Ctrl Pts',(-16.9764407449288,-20.1326654280783,
-4.96636033250357));
#75964=CARTESIAN_POINT('Ctrl Pts',(-16.9528176247318,-20.096173969665,-4.9637733559986));
#75965=CARTESIAN_POINT('Ctrl Pts',(-16.9487941436464,-20.0898860986497,
-4.96332705308486));
#75966=CARTESIAN_POINT('Ctrl Pts',(-16.9425809731613,-20.0800621295238,
-4.96262871174907));
#75967=CARTESIAN_POINT('Ctrl Pts',(-16.9403682606245,-20.0765405642337,
-4.96237817067017));
#75968=CARTESIAN_POINT('Ctrl Pts',(-16.9362776969439,-20.0699875835524,
-4.96191152822627));
#75969=CARTESIAN_POINT('Ctrl Pts',(-16.9343971224923,-20.0669579357728,
-4.96169561035057));
#75970=CARTESIAN_POINT('Ctrl Pts',(-16.9301549244374,-20.0600849658929,
-4.96120539646741));
#75971=CARTESIAN_POINT('Ctrl Pts',(-16.9277979369043,-20.0562388576151,
-4.96093080280682));
#75972=CARTESIAN_POINT('Ctrl Pts',(-16.9217435016202,-20.0462880438659,
-4.96021972596023));
#75973=CARTESIAN_POINT('Ctrl Pts',(-16.9180646357774,-20.0401721777926,
-4.95978207540537));
#75974=CARTESIAN_POINT('Ctrl Pts',(-16.8956520622646,-20.0024826101223,
-4.95708180604267));
#75975=CARTESIAN_POINT('Ctrl Pts',(-16.8777125917328,-19.9704466296272,
-4.95477288084186));
#75976=CARTESIAN_POINT('Ctrl Pts',(-16.7812823468265,-19.7872238540327,
-4.94155895734582));
#75977=CARTESIAN_POINT('Ctrl Pts',(-16.7204314381137,-19.627462679868,-4.930065518428));
#75978=CARTESIAN_POINT('Ctrl Pts',(-16.6563720880417,-19.3694561012144,
-4.91278860405544));
#75979=CARTESIAN_POINT('Ctrl Pts',(-16.6396562380864,-19.2753199787532,
-4.9067213552348));
#75980=CARTESIAN_POINT('Ctrl Pts',(-16.6270442302635,-19.1590857808435,
-4.89953960663383));
#75981=CARTESIAN_POINT('Ctrl Pts',(-16.6250581125698,-19.1377721844143,
-4.89823493270904));
#75982=CARTESIAN_POINT('Ctrl Pts',(-16.6226955445641,-19.1074468109817,
-4.89639537240257));
#75983=CARTESIAN_POINT('Ctrl Pts',(-16.6220529413086,-19.0984576382393,
-4.89585216655937));
#75984=CARTESIAN_POINT('Ctrl Pts',(-16.6210439463346,-19.0829515692758,
-4.89491866842861));
#75985=CARTESIAN_POINT('Ctrl Pts',(-16.6206502597991,-19.0764366316263,
-4.89452752450061));
#75986=CARTESIAN_POINT('Ctrl Pts',(-16.6199544872604,-19.0639649164083,
-4.89378075649995));
#75987=CARTESIAN_POINT('Ctrl Pts',(-16.6196474338811,-19.0580084888501,
-4.89342498024006));
#75988=CARTESIAN_POINT('Ctrl Pts',(-16.6189150599378,-19.0425293199526,
-4.89250264727081));
#75989=CARTESIAN_POINT('Ctrl Pts',(-16.6185288729768,-19.0330047942884,
-4.89193732122574));
#75990=CARTESIAN_POINT('Ctrl Pts',(-16.6174336357373,-19.0005850339198,
-4.89002027993911));
#75991=CARTESIAN_POINT('Ctrl Pts',(-16.6170318259038,-18.9776805368961,
-4.88867817331972));
#75992=CARTESIAN_POINT('Ctrl Pts',(-16.6167704492709,-18.7781623171578,
-4.87708348006839));
#75993=CARTESIAN_POINT('Ctrl Pts',(-16.6386383823485,-18.6022188590461,
-4.86759312005003));
#75994=CARTESIAN_POINT('Ctrl Pts',(-16.7033225289012,-18.347458107908,-4.85328889686386));
#75995=CARTESIAN_POINT('Ctrl Pts',(-16.7296224565645,-18.2652757430582,
-4.84856665876379));
#75996=CARTESIAN_POINT('Ctrl Pts',(-16.7744881232805,-18.1498668095713,
-4.84149558513031));
#75997=CARTESIAN_POINT('Ctrl Pts',(-16.7890515430464,-18.1151729230826,
-4.83930986967051));
#75998=CARTESIAN_POINT('Ctrl Pts',(-16.8076413505476,-18.0739974314149,
-4.83662186527621));
#75999=CARTESIAN_POINT('Ctrl Pts',(-16.8107890926625,-18.0671237607708,
-4.83616994232323));
#76000=CARTESIAN_POINT('Ctrl Pts',(-16.8157341543096,-18.0564763455102,
-4.83546470562457));
#76001=CARTESIAN_POINT('Ctrl Pts',(-16.8175059832761,-18.0526907352522,
-4.83521293744017));
#76002=CARTESIAN_POINT('Ctrl Pts',(-16.8208093575034,-18.0456869925087,
-4.83474519286304));
#76003=CARTESIAN_POINT('Ctrl Pts',(-16.8223378226635,-18.0424674710373,
-4.83452940744883));
#76004=CARTESIAN_POINT('Ctrl Pts',(-16.8258074206715,-18.035206576849,-4.83404101685401));
#76005=CARTESIAN_POINT('Ctrl Pts',(-16.8277532550989,-18.0311675248798,
-4.8337681235017));
#76006=CARTESIAN_POINT('Ctrl Pts',(-16.8335218058151,-18.0192901380843,
-4.83296212984865));
#76007=CARTESIAN_POINT('Ctrl Pts',(-16.8373800891638,-18.0114693195347,
-4.83242689242618));
#76008=CARTESIAN_POINT('Ctrl Pts',(-16.8651908063611,-17.9559634612137,
-4.82859712169009));
#76009=CARTESIAN_POINT('Ctrl Pts',(-16.8908883822631,-17.9091792501178,
-4.82520546127254));
#76010=CARTESIAN_POINT('Ctrl Pts',(-16.9273695634691,-17.848331125134,-4.82062021747684));
#76011=CARTESIAN_POINT('Ctrl Pts',(-16.9366036937779,-17.8333557251065,
-4.8194771529287));
#76012=CARTESIAN_POINT('Ctrl Pts',(-16.9719946087679,-17.7775304117428,
-4.81516520472423));
#76013=CARTESIAN_POINT('Ctrl Pts',(-16.9993656811007,-17.7374690806475,
-4.81196755704903));
#76014=CARTESIAN_POINT('Ctrl Pts',(-17.0928605310547,-17.6102418812309,
-4.80153803629925));
#76015=CARTESIAN_POINT('Ctrl Pts',(-17.1643723371996,-17.5272452590906,
-4.79430523469923));
#76016=CARTESIAN_POINT('Ctrl Pts',(-17.2810731876476,-17.4113089686908,
-4.78373158107755));
#76017=CARTESIAN_POINT('Ctrl Pts',(-17.321667310296,-17.3740131905885,-4.78024235191638));
#76018=CARTESIAN_POINT('Ctrl Pts',(-17.3898211268824,-17.3161366480742,
-4.77468465258231));
#76019=CARTESIAN_POINT('Ctrl Pts',(-17.4165057341725,-17.2945698129473,
-4.77257774142542));
#76020=CARTESIAN_POINT('Ctrl Pts',(-17.4522728780004,-17.2670722838763,
-4.7698411632716));
#76021=CARTESIAN_POINT('Ctrl Pts',(-17.4608922195501,-17.2605502047134,
-4.76918815389577));
#76022=CARTESIAN_POINT('Ctrl Pts',(-17.4750937108824,-17.2499742839813,
-4.76812264827348));
#76023=CARTESIAN_POINT('Ctrl Pts',(-17.4806463157958,-17.2458812682546,
-4.76770862255072));
#76024=CARTESIAN_POINT('Ctrl Pts',(-17.4914348451035,-17.2380097651368,
-4.76690910674101));
#76025=CARTESIAN_POINT('Ctrl Pts',(-17.4966682387519,-17.2342279535976,
-4.76652349030325));
#76026=CARTESIAN_POINT('Ctrl Pts',(-17.508794111383,-17.2255495922055,-4.76563507308644));
#76027=CARTESIAN_POINT('Ctrl Pts',(-17.5156988144551,-17.2206702496235,
-4.76513293835758));
#76028=CARTESIAN_POINT('Ctrl Pts',(-17.5343516609808,-17.207655694599,-4.76378634062934));
#76029=CARTESIAN_POINT('Ctrl Pts',(-17.5461533760406,-17.1995977613702,
-4.76294481895271));
#76030=CARTESIAN_POINT('Ctrl Pts',(-17.6551776126149,-17.1267660568906,
-4.7552637544997));
#76031=CARTESIAN_POINT('Ctrl Pts',(-17.7575297815945,-17.0700202272178,
-4.7487408193637));
#76032=CARTESIAN_POINT('Ctrl Pts',(-18.0124223312777,-16.9551273613875,
-4.73343473580252));
#76033=CARTESIAN_POINT('Ctrl Pts',(-18.1679887777992,-16.9055899459226,
-4.72483467487124));
#76034=CARTESIAN_POINT('Ctrl Pts',(-18.3595755969936,-16.8681208820909,
-4.713625662658));
#76035=CARTESIAN_POINT('Ctrl Pts',(-18.3916173547746,-16.8626173939183,
-4.7117296076978));
#76036=CARTESIAN_POINT('Ctrl Pts',(-18.4309325495454,-16.8567932004747,
-4.70936319797136));
#76037=CARTESIAN_POINT('Ctrl Pts',(-18.4380993054476,-16.855769051888,-4.70893020995935));
#76038=CARTESIAN_POINT('Ctrl Pts',(-18.4493423561248,-16.8542211948253,
-4.70824821888843));
#76039=CARTESIAN_POINT('Ctrl Pts',(-18.4534152406589,-16.8536725513348,
-4.70800060161163));
#76040=CARTESIAN_POINT('Ctrl Pts',(-18.4610310011228,-16.8526692293886,
-4.70753649923065));
#76041=CARTESIAN_POINT('Ctrl Pts',(-18.4645734390048,-16.8522116567716,
-4.70732017949619));
#76042=CARTESIAN_POINT('Ctrl Pts',(-18.4726622399494,-16.8511876415534,
-4.70682522962215));
#76043=CARTESIAN_POINT('Ctrl Pts',(-18.4772092785096,-16.8506269929698,
-4.70654627760946));
#76044=CARTESIAN_POINT('Ctrl Pts',(-18.4911906232533,-16.8489491538935,
-4.70568640953065));
#76045=CARTESIAN_POINT('Ctrl Pts',(-18.5006305072274,-16.8478807241849,
-4.70510285426571));
#76046=CARTESIAN_POINT('Ctrl Pts',(-18.5854821663644,-16.8388550173133,
-4.69983257637252));
#76047=CARTESIAN_POINT('Ctrl Pts',(-18.6612558909031,-16.8348922985301,
-4.69495116258859));
#76048=CARTESIAN_POINT('Ctrl Pts',(-18.9219988317722,-16.835270365541,-4.67789831655831));
#76049=CARTESIAN_POINT('Ctrl Pts',(-19.1061355323877,-16.8597708283004,
-4.66550103539425));
#76050=CARTESIAN_POINT('Ctrl Pts',(-19.3361766263971,-16.9217514690625,
-4.65047362438357));
#76051=CARTESIAN_POINT('Ctrl Pts',(-19.387066148928,-16.9375444431611,-4.64717204461378));
#76052=CARTESIAN_POINT('Ctrl Pts',(-19.4491379036165,-16.9594077070313,
-4.64317037238864));
#76053=CARTESIAN_POINT('Ctrl Pts',(-19.460929182786,-16.9636790397394,-4.64241132003099));
#76054=CARTESIAN_POINT('Ctrl Pts',(-19.4795054404177,-16.9705955355016,
-4.64121709005571));
#76055=CARTESIAN_POINT('Ctrl Pts',(-19.4863157803131,-16.9731713105016,
-4.64077960867383));
#76056=CARTESIAN_POINT('Ctrl Pts',(-19.4990579101942,-16.9780658688821,
-4.63996167685359));
#76057=CARTESIAN_POINT('Ctrl Pts',(-19.5049927715524,-16.9803763778228,
-4.63958095452098));
#76058=CARTESIAN_POINT('Ctrl Pts',(-19.5182499976492,-16.9856065804052,
-4.63873100461963));
#76059=CARTESIAN_POINT('Ctrl Pts',(-19.5255666877404,-16.9885404712933,
-4.63826226086022));
#76060=CARTESIAN_POINT('Ctrl Pts',(-19.5440619743999,-16.9960770113323,
-4.63707813758241));
#76061=CARTESIAN_POINT('Ctrl Pts',(-19.5552179418437,-17.0007347076697,
-4.63636462361637));
#76062=CARTESIAN_POINT('Ctrl Pts',(-19.6186385932735,-17.0278535395828,
-4.63231158884045));
#76063=CARTESIAN_POINT('Ctrl Pts',(-19.6700237506961,-17.0523196556421,
-4.62904117540495));
#76064=CARTESIAN_POINT('Ctrl Pts',(-19.7441234589785,-17.0913386639317,
-4.62431037108652));
#76065=CARTESIAN_POINT('Ctrl Pts',(-19.767642783662,-17.1043007076207,-4.62280637074052));
#76066=CARTESIAN_POINT('Ctrl Pts',(-19.891285029825,-17.1755427024923,-4.61486888328844));
#76067=CARTESIAN_POINT('Ctrl Pts',(-19.9867433515099,-17.2415193516592,
-4.60864395678167));
#76068=CARTESIAN_POINT('Ctrl Pts',(-20.1382163806034,-17.3657241310027,
-4.5979650732624));
#76069=CARTESIAN_POINT('Ctrl Pts',(-20.1971739750625,-17.4199377643235,
-4.59356330534814));
#76070=CARTESIAN_POINT('Ctrl Pts',(-20.277994046911,-17.5031841055979,-4.58692635700263));
#76071=CARTESIAN_POINT('Ctrl Pts',(-20.3024071368253,-17.5296484899652,
-4.58483223435928));
#76072=CARTESIAN_POINT('Ctrl Pts',(-20.3310517233175,-17.5623343884094,
-4.58224580120193));
#76073=CARTESIAN_POINT('Ctrl Pts',(-20.3359416520772,-17.5679741120326,
-4.58179952928709));
#76074=CARTESIAN_POINT('Ctrl Pts',(-20.3435094238394,-17.5767961200587,
-4.58110122599477));
#76075=CARTESIAN_POINT('Ctrl Pts',(-20.3462079433198,-17.5799606989424,
-4.58085069169639));
#76076=CARTESIAN_POINT('Ctrl Pts',(-20.3512028583503,-17.5858533640531,
-4.58038405528615));
#76077=CARTESIAN_POINT('Ctrl Pts',(-20.3535016924873,-17.5885793079941,
-4.58016813662203));
#76078=CARTESIAN_POINT('Ctrl Pts',(-20.3586930848236,-17.5947668845043,
-4.57967791240857));
#76079=CARTESIAN_POINT('Ctrl Pts',(-20.3615814577661,-17.598231944853,-4.57940330915237));
#76080=CARTESIAN_POINT('Ctrl Pts',(-20.3701034741884,-17.6085221465587,
-4.5785876626009));
#76081=CARTESIAN_POINT('Ctrl Pts',(-20.3757053375998,-17.6153733134639,
-4.57804440659786));
#76082=CARTESIAN_POINT('Ctrl Pts',(-20.4168972455648,-17.666401264886,-4.57399800027048));
#76083=CARTESIAN_POINT('Ctrl Pts',(-20.4507385734215,-17.7119537513666,
-4.57038515258016));
#76084=CARTESIAN_POINT('Ctrl Pts',(-20.5175961194107,-17.8099379597198,
-4.56270245993221));
#76085=CARTESIAN_POINT('Ctrl Pts',(-20.5502246796521,-17.862574398703,-4.55862482500236));
#76086=CARTESIAN_POINT('Ctrl Pts',(-20.6341054045249,-18.0121591340198,
-4.54729669943314));
#76087=CARTESIAN_POINT('Ctrl Pts',(-20.6802113236659,-18.1117819658407,
-4.54004811994042));
#76088=CARTESIAN_POINT('Ctrl Pts',(-20.737683337339,-18.2664292201099,-4.52944129938011));
#76089=CARTESIAN_POINT('Ctrl Pts',(-20.7549277316741,-18.3190654488591,
-4.52593479478235));
#76090=CARTESIAN_POINT('Ctrl Pts',(-20.7795153219938,-18.4054279742752,
-4.52035281203362));
#76091=CARTESIAN_POINT('Ctrl Pts',(-20.7881324592452,-18.4387612930963,
-4.51823847279913));
#76092=CARTESIAN_POINT('Ctrl Pts',(-20.7983855428401,-18.4828321739193,
-4.5154938061602));
#76093=CARTESIAN_POINT('Ctrl Pts',(-20.8007569915616,-18.493391601517,-4.51483996346439));
#76094=CARTESIAN_POINT('Ctrl Pts',(-20.8045078950316,-18.5107136069883,
-4.5137734466202));
#76095=CARTESIAN_POINT('Ctrl Pts',(-20.8059354161052,-18.5174654705448,
-4.51335923738922));
#76096=CARTESIAN_POINT('Ctrl Pts',(-20.8086343584915,-18.5305466189247,
-4.51255960765106));
#76097=CARTESIAN_POINT('Ctrl Pts',(-20.8099098928332,-18.5368749680933,
-4.51217405953265));
#76098=CARTESIAN_POINT('Ctrl Pts',(-20.8127876276471,-18.5514973718676,
-4.51128614295279));
#76099=CARTESIAN_POINT('Ctrl Pts',(-20.8143691793942,-18.5597954148903,
-4.51078443813165));
#76100=CARTESIAN_POINT('Ctrl Pts',(-20.8184877291796,-18.5821305946227,
-4.50943975416288));
#76101=CARTESIAN_POINT('Ctrl Pts',(-20.8209326205792,-18.5961844268039,
-4.50859970311708));
#76102=CARTESIAN_POINT('Ctrl Pts',(-20.8418093118175,-18.7238153633244,
-4.50102303982116));
#76103=CARTESIAN_POINT('Ctrl Pts',(-20.8510962905331,-18.83870077858,-4.49459283785146));
#76104=CARTESIAN_POINT('Ctrl Pts',(-20.8508421940249,-19.1400360575658,
-4.47808641480517));
#76105=CARTESIAN_POINT('Ctrl Pts',(-20.8261075481251,-19.3254189869919,
-4.46831883007838));
#76106=CARTESIAN_POINT('Ctrl Pts',(-20.7737437540471,-19.5188655758418,
-4.45654187285768));
#76107=CARTESIAN_POINT('Ctrl Pts',(-20.7698906309532,-19.5325518732858,
-4.45569948325786));
#76108=CARTESIAN_POINT('Ctrl Pts',(-20.7643392700573,-19.5515351286692,
-4.45451694403742));
#76109=CARTESIAN_POINT('Ctrl Pts',(-20.7627574775556,-19.5568661155281,
-4.45418329897582));
#76110=CARTESIAN_POINT('Ctrl Pts',(-20.7601843572481,-19.5654144474497,
-4.45364569800847));
#76111=CARTESIAN_POINT('Ctrl Pts',(-20.7592063133213,-19.5686358098699,
-4.45344251465341));
#76112=CARTESIAN_POINT('Ctrl Pts',(-20.7571469227646,-19.5753610313025,
-4.45301706305863));
#76113=CARTESIAN_POINT('Ctrl Pts',(-20.7560641558258,-19.5788644155073,
-4.45279470933072));
#76114=CARTESIAN_POINT('Ctrl Pts',(-20.7534222730193,-19.5873343854775,
-4.45225541434439));
#76115=CARTESIAN_POINT('Ctrl Pts',(-20.7518539349012,-19.5922980510786,
-4.4519379369362));
#76116=CARTESIAN_POINT('Ctrl Pts',(-20.7463005708686,-19.6096509614781,
-4.45082314131569));
#76117=CARTESIAN_POINT('Ctrl Pts',(-20.7422197134157,-19.622008908838,-4.4500204769994));
#76118=CARTESIAN_POINT('Ctrl Pts',(-20.7330366644334,-19.6489798965801,
-4.44825065621382));
#76119=CARTESIAN_POINT('Ctrl Pts',(-20.7278880804562,-19.6635748542383,
-4.44728126432251));
#76120=CARTESIAN_POINT('Ctrl Pts',(-20.7225805839746,-19.678110364228,-4.44630500845845));
#76121=CARTESIAN_POINT('Origin',(-18.734,-18.952,0.));
#76122=CARTESIAN_POINT('',(-20.7225805821191,-19.6781103693095,-3.64442446878243));
#76123=CARTESIAN_POINT('',(-20.7225805144725,-19.6781105545716,-3.86819367631211));
#76124=CARTESIAN_POINT('',(-20.7225805821191,-19.6781103693095,0.));
#76125=CARTESIAN_POINT('',(-20.850999091379,-18.950054148737,-3.9109852266757));
#76126=CARTESIAN_POINT('Ctrl Pts',(-20.7225805144725,-19.6781105545716,
-3.86819367631211));
#76127=CARTESIAN_POINT('Ctrl Pts',(-20.7339917000002,-19.6468590308957,
-3.87027308349242));
#76128=CARTESIAN_POINT('Ctrl Pts',(-20.7446699030894,-19.6153283311154,
-3.87233005795932));
#76129=CARTESIAN_POINT('Ctrl Pts',(-20.759305937768,-19.5685008207448,-3.87532605152801));
#76130=CARTESIAN_POINT('Ctrl Pts',(-20.7638396682874,-19.5534053089804,
-3.87628298861571));
#76131=CARTESIAN_POINT('Ctrl Pts',(-20.7704398408054,-19.5305040451152,
-3.87772167942554));
#76132=CARTESIAN_POINT('Ctrl Pts',(-20.7726308327077,-19.5227350402634,
-3.87820748126762));
#76133=CARTESIAN_POINT('Ctrl Pts',(-20.7764754410657,-19.508797853311,-3.87907500430636));
#76134=CARTESIAN_POINT('Ctrl Pts',(-20.7781456752986,-19.5026343944495,
-3.87945726175366));
#76135=CARTESIAN_POINT('Ctrl Pts',(-20.7816285950472,-19.4895475364464,
-3.88026600625009));
#76136=CARTESIAN_POINT('Ctrl Pts',(-20.7834341154902,-19.4826223001252,
-3.88069225692262));
#76137=CARTESIAN_POINT('Ctrl Pts',(-20.7870374715709,-19.4685085137492,
-3.88155753403966));
#76138=CARTESIAN_POINT('Ctrl Pts',(-20.7888327535059,-19.461319410277,-3.88199647325397));
#76139=CARTESIAN_POINT('Ctrl Pts',(-20.7932121438162,-19.4433822751305,
-3.88308724193768));
#76140=CARTESIAN_POINT('Ctrl Pts',(-20.7957499029133,-19.4326230729711,
-3.88373758668791));
#76141=CARTESIAN_POINT('Ctrl Pts',(-20.8334343576381,-19.2670610545227,
-3.89368680767375));
#76142=CARTESIAN_POINT('Ctrl Pts',(-20.8511450351567,-19.1088094550095,
-3.90236296950705));
#76143=CARTESIAN_POINT('Ctrl Pts',(-20.8509991056246,-18.9500540337685,
-3.91098525629469));
#76144=CARTESIAN_POINT('Ctrl Pts',(-20.8509991057315,-18.9500541499897,
-3.91098524998252));
#76145=CARTESIAN_POINT('Ctrl Pts',(-20.8508677552328,-18.8071505928033,
-3.91874659410215));
#76146=CARTESIAN_POINT('Ctrl Pts',(-20.8362671717988,-18.6646421546169,
-3.9264424364072));
#76147=CARTESIAN_POINT('Ctrl Pts',(-20.8054602107921,-18.5151512492231,
-3.93541352843948));
#76148=CARTESIAN_POINT('Ctrl Pts',(-20.8034244703783,-18.5056071353841,
-3.93599034923015));
#76149=CARTESIAN_POINT('Ctrl Pts',(-20.8001174997672,-18.4906120914082,
-3.93690350748031));
#76150=CARTESIAN_POINT('Ctrl Pts',(-20.7988904876265,-18.4851514189999,
-3.93723749209016));
#76151=CARTESIAN_POINT('Ctrl Pts',(-20.7965251623796,-18.4748165890272,
-3.93787243749969));
#76152=CARTESIAN_POINT('Ctrl Pts',(-20.795391185985,-18.4699414658693,-3.93817315633918));
#76153=CARTESIAN_POINT('Ctrl Pts',(-20.7934048895302,-18.4615372779484,
-3.93869371378611));
#76154=CARTESIAN_POINT('Ctrl Pts',(-20.7925607518292,-18.458006263577,-3.93891308271453));
#76155=CARTESIAN_POINT('Ctrl Pts',(-20.7909045653938,-18.4511564288955,
-3.93933994041501));
#76156=CARTESIAN_POINT('Ctrl Pts',(-20.7900935637945,-18.4478373968713,
-3.93954736266223));
#76157=CARTESIAN_POINT('Ctrl Pts',(-20.7878796792858,-18.4388712429774,
-3.94010927374737));
#76158=CARTESIAN_POINT('Ctrl Pts',(-20.7864615548879,-18.4332279670829,
-3.94046462818654));
#76159=CARTESIAN_POINT('Ctrl Pts',(-20.7810870799278,-18.4122078279738,
-3.94179437413913));
#76160=CARTESIAN_POINT('Ctrl Pts',(-20.7769811546349,-18.396870223128,-3.9427768674802));
#76161=CARTESIAN_POINT('Ctrl Pts',(-20.7391408561341,-18.2616273392847,
-3.95153986855596));
#76162=CARTESIAN_POINT('Ctrl Pts',(-20.6950603853006,-18.1448812701311,
-3.95978535644781));
#76163=CARTESIAN_POINT('Ctrl Pts',(-20.6100511858113,-17.96853979006,-3.97272142857487));
#76164=CARTESIAN_POINT('Ctrl Pts',(-20.5759023984443,-17.905979727209,-3.97741812474979));
#76165=CARTESIAN_POINT('Ctrl Pts',(-20.4894057397083,-17.7649374867526,
-3.98816741794171));
#76166=CARTESIAN_POINT('Ctrl Pts',(-20.4348357081262,-17.6879870599765,
-3.99415326834526));
#76167=CARTESIAN_POINT('Ctrl Pts',(-20.3617156831655,-17.5982296750814,
-4.00126722239978));
#76168=CARTESIAN_POINT('Ctrl Pts',(-20.3478648540158,-17.5817472041432,
-4.0025798484107));
#76169=CARTESIAN_POINT('Ctrl Pts',(-20.3291372683196,-17.5601393702983,
-4.00430963397666));
#76170=CARTESIAN_POINT('Ctrl Pts',(-20.3244831877986,-17.5548235084573,
-4.00473592830462));
#76171=CARTESIAN_POINT('Ctrl Pts',(-20.3152194689624,-17.5443488179071,
-4.00557743634176));
#76172=CARTESIAN_POINT('Ctrl Pts',(-20.3106109842,-17.5391890905926,-4.00599269058446));
#76173=CARTESIAN_POINT('Ctrl Pts',(-20.3016578333715,-17.5292633744369,
-4.00679298141101));
#76174=CARTESIAN_POINT('Ctrl Pts',(-20.2973165252565,-17.5244944723293,
-4.00717815273047));
#76175=CARTESIAN_POINT('Ctrl Pts',(-20.2872662273235,-17.5135551134005,
-4.00806327701928));
#76176=CARTESIAN_POINT('Ctrl Pts',(-20.2815421165878,-17.5073986483377,
-4.00856257979323));
#76177=CARTESIAN_POINT('Ctrl Pts',(-20.2661032197986,-17.4909906958999,
-4.009896588182));
#76178=CARTESIAN_POINT('Ctrl Pts',(-20.2563221612917,-17.4808019458866,
-4.01072843890351));
#76179=CARTESIAN_POINT('Ctrl Pts',(-20.1714442557834,-17.3941390664928,
-4.01783640143235));
#76180=CARTESIAN_POINT('Ctrl Pts',(-20.0907374091159,-17.3233672534982,
-4.02384940625994));
#76181=CARTESIAN_POINT('Ctrl Pts',(-19.9105739166692,-17.1881103556605,
-4.03622626818153));
#76182=CARTESIAN_POINT('Ctrl Pts',(-19.8103776060796,-17.1252425182423,
-4.04254151760226));
#76183=CARTESIAN_POINT('Ctrl Pts',(-19.6539374711222,-17.0444446560424,
-4.05224819475398));
#76184=CARTESIAN_POINT('Ctrl Pts',(-19.6013415514799,-17.0199622104733,
-4.05549044429343));
#76185=CARTESIAN_POINT('Ctrl Pts',(-19.5207342985949,-16.9863961669037,
-4.06052168939224));
#76186=CARTESIAN_POINT('Ctrl Pts',(-19.493427583706,-16.9756855424803,-4.06223656050007));
#76187=CARTESIAN_POINT('Ctrl Pts',(-19.4593546534484,-16.9631313731406,
-4.0643995491408));
#76188=CARTESIAN_POINT('Ctrl Pts',(-19.4527887179666,-16.9607489952267,
-4.0648174171707));
#76189=CARTESIAN_POINT('Ctrl Pts',(-19.4423642044375,-16.9570248517356,
-4.06548270052494));
#76190=CARTESIAN_POINT('Ctrl Pts',(-19.4385132587242,-16.9556616629554,
-4.06572886278131));
#76191=CARTESIAN_POINT('Ctrl Pts',(-19.4312842020671,-16.9531261851919,
-4.06619175108062));
#76192=CARTESIAN_POINT('Ctrl Pts',(-19.4279070585022,-16.951951305728,-4.06640832093716));
#76193=CARTESIAN_POINT('Ctrl Pts',(-19.4201600771924,-16.9492781799044,
-4.06690585590914));
#76194=CARTESIAN_POINT('Ctrl Pts',(-19.4157883136037,-16.9477856814404,
-4.06718715590882));
#76195=CARTESIAN_POINT('Ctrl Pts',(-19.4022263801768,-16.9432052120397,
-4.06806136367723));
#76196=CARTESIAN_POINT('Ctrl Pts',(-19.3930200083535,-16.9401661063384,
-4.06865703730769));
#76197=CARTESIAN_POINT('Ctrl Pts',(-19.2895324269085,-16.9067904780016,
-4.07537527310461));
#76198=CARTESIAN_POINT('Ctrl Pts',(-19.193265016635,-16.8830463379857,-4.08182716728371));
#76199=CARTESIAN_POINT('Ctrl Pts',(-18.929784823183,-16.8373572780874,-4.09944296715288));
#76200=CARTESIAN_POINT('Ctrl Pts',(-18.7609960367477,-16.8284808495551,
-4.11062975816369));
#76201=CARTESIAN_POINT('Ctrl Pts',(-18.5459926054869,-16.8428402538046,
-4.12416079473513));
#76202=CARTESIAN_POINT('Ctrl Pts',(-18.4991735865144,-16.8475383767336,
-4.12706847298146));
#76203=CARTESIAN_POINT('Ctrl Pts',(-18.4408421272215,-16.855362947944,-4.13064512008699));
#76204=CARTESIAN_POINT('Ctrl Pts',(-18.4291505339283,-16.8570309600565,
-4.13135970110613));
#76205=CARTESIAN_POINT('Ctrl Pts',(-18.4102896003126,-16.8598830426988,
-4.13250889118889));
#76206=CARTESIAN_POINT('Ctrl Pts',(-18.4031114500929,-16.8610063234234,
-4.13294541500388));
#76207=CARTESIAN_POINT('Ctrl Pts',(-18.3896505484418,-16.863183819332,-4.13376248271698));
#76208=CARTESIAN_POINT('Ctrl Pts',(-18.3833665138931,-16.8642294807137,
-4.13414329298243));
#76209=CARTESIAN_POINT('Ctrl Pts',(-18.3692954875216,-16.8666362173132,
-4.13499462928351));
#76210=CARTESIAN_POINT('Ctrl Pts',(-18.3615111799843,-16.8680125794238,
-4.13546466425508));
#76211=CARTESIAN_POINT('Ctrl Pts',(-18.3417722729069,-16.8716167948235,
-4.13665426541073));
#76212=CARTESIAN_POINT('Ctrl Pts',(-18.3298287233502,-16.873904126691,-4.13737193548605));
#76213=CARTESIAN_POINT('Ctrl Pts',(-18.2610582986873,-16.8876898021478,
-4.1414928921393));
#76214=CARTESIAN_POINT('Ctrl Pts',(-18.2047002031986,-16.901416413084,-4.14482426033528));
#76215=CARTESIAN_POINT('Ctrl Pts',(-17.9819385892691,-16.9654703850837,
-4.15790804927205));
#76216=CARTESIAN_POINT('Ctrl Pts',(-17.8214651537316,-17.0338826082114,
-4.16708455584795));
#76217=CARTESIAN_POINT('Ctrl Pts',(-17.6227131093607,-17.149260852885,-4.179771905794));
#76218=CARTESIAN_POINT('Ctrl Pts',(-17.5754054539349,-17.1792945009904,
-4.18290877768369));
#76219=CARTESIAN_POINT('Ctrl Pts',(-17.5057219806043,-17.2275152709477,
-4.18779537036499));
#76220=CARTESIAN_POINT('Ctrl Pts',(-17.4824326783955,-17.2443426781843,
-4.18947613929834));
#76221=CARTESIAN_POINT('Ctrl Pts',(-17.4539345386543,-17.2658298131928,
-4.19160254512058));
#76222=CARTESIAN_POINT('Ctrl Pts',(-17.4483955439157,-17.2700491494604,
-4.19201918815838));
#76223=CARTESIAN_POINT('Ctrl Pts',(-17.4396690466386,-17.2767648599085,
-4.19268108617326));
#76224=CARTESIAN_POINT('Ctrl Pts',(-17.4364676607751,-17.2792432276448,
-4.19292508720424));
#76225=CARTESIAN_POINT('Ctrl Pts',(-17.4304468926759,-17.2839319165853,
-4.19338624156579));
#76226=CARTESIAN_POINT('Ctrl Pts',(-17.4276260047776,-17.2861402164602,
-4.19360325259075));
#76227=CARTESIAN_POINT('Ctrl Pts',(-17.421194077331,-17.291201761179,-4.19410021849645));
#76228=CARTESIAN_POINT('Ctrl Pts',(-17.4175867325698,-17.2940596243904,
-4.19438050036752));
#76229=CARTESIAN_POINT('Ctrl Pts',(-17.4080439837439,-17.301670498524,-4.19512602741155));
#76230=CARTESIAN_POINT('Ctrl Pts',(-17.4021248829129,-17.3064437144276,
-4.19559266622832));
#76231=CARTESIAN_POINT('Ctrl Pts',(-17.3611207346591,-17.3398759879602,
-4.19885391415649));
#76232=CARTESIAN_POINT('Ctrl Pts',(-17.3269404522327,-17.3696207571177,
-4.20171901078609));
#76233=CARTESIAN_POINT('Ctrl Pts',(-17.2894212158693,-17.4044484127776,
-4.20500893655988));
#76234=CARTESIAN_POINT('Ctrl Pts',(-17.2851158301567,-17.4084785586425,
-4.2053887019268));
#76235=CARTESIAN_POINT('Ctrl Pts',(-17.2636231234322,-17.4287664137077,
-4.20729555781074));
#76236=CARTESIAN_POINT('Ctrl Pts',(-17.2466927464502,-17.4452930634201,
-4.20883323813897));
#76237=CARTESIAN_POINT('Ctrl Pts',(-17.1284398755276,-17.5646615671128,
-4.21981020068044));
#76238=CARTESIAN_POINT('Ctrl Pts',(-17.0375844448488,-17.6773586527658,
-4.22947212622353));
#76239=CARTESIAN_POINT('Ctrl Pts',(-16.9252306107284,-17.8502460464882,
-4.24279355778659));
#76240=CARTESIAN_POINT('Ctrl Pts',(-16.8938372374362,-17.9035198546591,
-4.2467246209479));
#76241=CARTESIAN_POINT('Ctrl Pts',(-16.8473267330603,-17.9909896167273,
-4.25289751514259));
#76242=CARTESIAN_POINT('Ctrl Pts',(-16.8307063098121,-18.0243414537257,
-4.25518924739902));
#76243=CARTESIAN_POINT('Ctrl Pts',(-16.8102724707932,-18.0682096558271,
-4.25812611102926));
#76244=CARTESIAN_POINT('Ctrl Pts',(-16.8056506283698,-18.0783400619033,
-4.25879906924924));
#76245=CARTESIAN_POINT('Ctrl Pts',(-16.7982659483824,-18.0948703362515,
-4.25988879295217));
#76246=CARTESIAN_POINT('Ctrl Pts',(-16.7954544592642,-18.1012481164458,
-4.26030722416042));
#76247=CARTESIAN_POINT('Ctrl Pts',(-16.7901095978453,-18.1135368468801,
-4.26110964456268));
#76248=CARTESIAN_POINT('Ctrl Pts',(-16.7875715653679,-18.1194456744491,
-4.26149378964269));
#76249=CARTESIAN_POINT('Ctrl Pts',(-16.781823763534,-18.1329971597848,-4.26237099455689));
#76250=CARTESIAN_POINT('Ctrl Pts',(-16.7786318656496,-18.1406473191925,
-4.26286344239535));
#76251=CARTESIAN_POINT('Ctrl Pts',(-16.7702752310087,-18.1610117871001,
-4.2641671427367));
#76252=CARTESIAN_POINT('Ctrl Pts',(-16.7651889943345,-18.1737580334519,
-4.26497574320061));
#76253=CARTESIAN_POINT('Ctrl Pts',(-16.7275795357931,-18.2707373687653,
-4.27107396391681));
#76254=CARTESIAN_POINT('Ctrl Pts',(-16.700349111353,-18.3569295994903,-4.27618099605698));
#76255=CARTESIAN_POINT('Ctrl Pts',(-16.6452676424002,-18.5800477179326,
-4.28890311167347));
#76256=CARTESIAN_POINT('Ctrl Pts',(-16.6253021079877,-18.7184562078926,
-4.29632347502236));
#76257=CARTESIAN_POINT('Ctrl Pts',(-16.6166375322596,-18.9130256558026,
-4.30708178341982));
#76258=CARTESIAN_POINT('Ctrl Pts',(-16.6163418218673,-18.968303707417,-4.31017826428166));
#76259=CARTESIAN_POINT('Ctrl Pts',(-16.6191706651434,-19.0519831320674,
-4.31500785401755));
#76260=CARTESIAN_POINT('Ctrl Pts',(-16.6207066568436,-19.08041654205,-4.31667390547102));
#76261=CARTESIAN_POINT('Ctrl Pts',(-16.6233297507466,-19.1157324064544,
-4.31878386147019));
#76262=CARTESIAN_POINT('Ctrl Pts',(-16.6238780581976,-19.1226534197843,
-4.31919930486241));
#76263=CARTESIAN_POINT('Ctrl Pts',(-16.6247996081737,-19.1336013825182,
-4.31985972740497));
#76264=CARTESIAN_POINT('Ctrl Pts',(-16.6251503689035,-19.1376302448607,
-4.32010346206463));
#76265=CARTESIAN_POINT('Ctrl Pts',(-16.6258337042167,-19.1452270958155,
-4.32056440891715));
#76266=CARTESIAN_POINT('Ctrl Pts',(-16.6261637946523,-19.1487952538634,
-4.32078148053715));
#76267=CARTESIAN_POINT('Ctrl Pts',(-16.6269392326948,-19.1569516359477,
-4.3212789704458));
#76268=CARTESIAN_POINT('Ctrl Pts',(-16.6273905078855,-19.1615392493075,
-4.32155971824884));
#76269=CARTESIAN_POINT('Ctrl Pts',(-16.6286284567157,-19.1737157531584,
-4.32230728971806));
#76270=CARTESIAN_POINT('Ctrl Pts',(-16.6294411698588,-19.1813018467447,
-4.32277551896893));
#76271=CARTESIAN_POINT('Ctrl Pts',(-16.6354230540826,-19.2344255718266,
-4.32607105529165));
#76272=CARTESIAN_POINT('Ctrl Pts',(-16.6420283922313,-19.2797857598849,
-4.32897049370731));
#76273=CARTESIAN_POINT('Ctrl Pts',(-16.6567510987132,-19.3620633594794,
-4.33434424974106));
#76274=CARTESIAN_POINT('Ctrl Pts',(-16.6643956519628,-19.3990487341738,
-4.33680275869016));
#76275=CARTESIAN_POINT('Ctrl Pts',(-16.703903744442,-19.5673492742669,-4.34813514041002));
#76276=CARTESIAN_POINT('Ctrl Pts',(-16.747308258994,-19.6956436502566,-4.35715618972546));
#76277=CARTESIAN_POINT('Ctrl Pts',(-16.8280764553227,-19.8755804272229,
-4.36990178836925));
#76278=CARTESIAN_POINT('Ctrl Pts',(-16.8559888461057,-19.9310917295683,
-4.3738525506462));
#76279=CARTESIAN_POINT('Ctrl Pts',(-16.9045504775818,-20.0179272672908,
-4.38005259591364));
#76280=CARTESIAN_POINT('Ctrl Pts',(-16.9236588781968,-20.0500673004922,
-4.3823523257157));
#76281=CARTESIAN_POINT('Ctrl Pts',(-16.9495583751451,-20.0911142910218,
-4.38529781204679));
#76282=CARTESIAN_POINT('Ctrl Pts',(-16.9555817670222,-20.10049548392,-4.38597159802395));
#76283=CARTESIAN_POINT('Ctrl Pts',(-16.9654926666097,-20.1156663750822,
-4.38706232698372));
#76284=CARTESIAN_POINT('Ctrl Pts',(-16.9693351123407,-20.1214851246701,
-4.3874809414376));
#76285=CARTESIAN_POINT('Ctrl Pts',(-16.9767758776042,-20.1326327651176,
-4.38828348979272));
#76286=CARTESIAN_POINT('Ctrl Pts',(-16.9803698579053,-20.1379644465768,
-4.38866758077857));
#76287=CARTESIAN_POINT('Ctrl Pts',(-16.9886489814745,-20.1501266319347,
-4.38954435320516));
#76288=CARTESIAN_POINT('Ctrl Pts',(-16.9933500509916,-20.1569462071033,
-4.39003642474036));
#76289=CARTESIAN_POINT('Ctrl Pts',(-17.0059334137057,-20.174972851478,-4.39133846794334));
#76290=CARTESIAN_POINT('Ctrl Pts',(-17.0138847678329,-20.1861314044111,
-4.39214579845206));
#76291=CARTESIAN_POINT('Ctrl Pts',(-17.0745473175795,-20.2695370136281,
-4.39819239748218));
#76292=CARTESIAN_POINT('Ctrl Pts',(-17.131684041257,-20.3384607291917,-4.40325275680924));
#76293=CARTESIAN_POINT('Ctrl Pts',(-17.288727770133,-20.5051780945823,-4.41593712263578));
#76294=CARTESIAN_POINT('Ctrl Pts',(-17.3942502941685,-20.5970662521818,
-4.42336238006537));
#76295=CARTESIAN_POINT('Ctrl Pts',(-17.5535787635507,-20.7102417494571,
-4.43415301056376));
#76296=CARTESIAN_POINT('Ctrl Pts',(-17.6003707804107,-20.7407683657582,
-4.43728098721985));
#76297=CARTESIAN_POINT('Ctrl Pts',(-17.6729278130065,-20.784112725906,-4.44215503288807));
#76298=CARTESIAN_POINT('Ctrl Pts',(-17.6978392325704,-20.798315765815,-4.44383256947258));
#76299=CARTESIAN_POINT('Ctrl Pts',(-17.7291438673546,-20.8153307744653,
-4.44595536300871));
#76300=CARTESIAN_POINT('Ctrl Pts',(-17.735273998735,-20.8186236347251,-4.44637174353714));
#76301=CARTESIAN_POINT('Ctrl Pts',(-17.7449953287191,-20.8237839468382,
-4.44703331869259));
#76302=CARTESIAN_POINT('Ctrl Pts',(-17.7485759027929,-20.8256714577183,
-4.4472772614451));
#76303=CARTESIAN_POINT('Ctrl Pts',(-17.7553359429512,-20.8292102970675,
-4.44773837028484));
#76304=CARTESIAN_POINT('Ctrl Pts',(-17.758514195629,-20.8308638270862,-4.44795539444513));
#76305=CARTESIAN_POINT('Ctrl Pts',(-17.7657862001301,-20.8346237631418,
-4.44845247445339));
#76306=CARTESIAN_POINT('Ctrl Pts',(-17.7698826306683,-20.8367248852377,
-4.44873285784151));
#76307=CARTESIAN_POINT('Ctrl Pts',(-17.7807679828604,-20.8422633749844,
-4.44947883016849));
#76308=CARTESIAN_POINT('Ctrl Pts',(-17.7875685683302,-20.8456774927272,
-4.44994581534779));
#76309=CARTESIAN_POINT('Ctrl Pts',(-17.8350857344075,-20.869212781581,-4.45321451189403));
#76310=CARTESIAN_POINT('Ctrl Pts',(-17.8764191311835,-20.8880542573626,
-4.45608706631556));
#76311=CARTESIAN_POINT('Ctrl Pts',(-17.9236576980185,-20.9077780490075,
-4.45937718209051));
#76312=CARTESIAN_POINT('Ctrl Pts',(-17.9290016899543,-20.9099836932757,
-4.45974949026986));
#76313=CARTESIAN_POINT('Ctrl Pts',(-18.0801810755522,-20.971656945802,-4.47028367104066));
#76314=CARTESIAN_POINT('Ctrl Pts',(-18.232190867034,-21.014688697066,-4.48087398619109));
#76315=CARTESIAN_POINT('Ctrl Pts',(-18.4891812364084,-21.057317310925,-4.49778554889153));
#76316=CARTESIAN_POINT('Ctrl Pts',(-18.5918946355419,-21.0667360916899,
-4.50430475197365));
#76317=CARTESIAN_POINT('Ctrl Pts',(-18.7097046862916,-21.0689123739475,
-4.51149034843639));
#76318=CARTESIAN_POINT('Ctrl Pts',(-18.7245123799087,-21.0690305297247,
-4.51238847350152));
#76319=CARTESIAN_POINT('Ctrl Pts',(-18.7470890259737,-21.0689737904363,
-4.51375036900016));
#76320=CARTESIAN_POINT('Ctrl Pts',(-18.7548575690699,-21.0689115041298,
-4.51421765079908));
#76321=CARTESIAN_POINT('Ctrl Pts',(-18.76898648262,-21.0687204381559,-4.51506512559451));
#76322=CARTESIAN_POINT('Ctrl Pts',(-18.7753469232033,-21.0686057499172,
-4.51544575524532));
#76323=CARTESIAN_POINT('Ctrl Pts',(-18.789072577685,-21.0682963623672,-4.51626528409207));
#76324=CARTESIAN_POINT('Ctrl Pts',(-18.7964375041551,-21.0680918794704,
-4.51670387194656));
#76325=CARTESIAN_POINT('Ctrl Pts',(-18.8163931962319,-21.0674335465806,
-4.51788920339165));
#76326=CARTESIAN_POINT('Ctrl Pts',(-18.8289813468477,-21.0669057385281,
-4.51863362607209));
#76327=CARTESIAN_POINT('Ctrl Pts',(-18.8900499132638,-21.0637988468246,
-4.52222991958248));
#76328=CARTESIAN_POINT('Ctrl Pts',(-18.9384387864532,-21.0596648830024,
-4.52503281529519));
#76329=CARTESIAN_POINT('Ctrl Pts',(-19.0271594313944,-21.0490006270932,
-4.53011167662205));
#76330=CARTESIAN_POINT('Ctrl Pts',(-19.0675252961146,-21.0429603546819,
-4.5323993561184));
#76331=CARTESIAN_POINT('Ctrl Pts',(-19.2400326012144,-21.0120235601538,
-4.54212611109203));
#76332=CARTESIAN_POINT('Ctrl Pts',(-19.3698061794308,-20.9757380922083,
-4.54929593551354));
#76333=CARTESIAN_POINT('Ctrl Pts',(-19.5537918917088,-20.9048350887584,
-4.56013222940999));
#76334=CARTESIAN_POINT('Ctrl Pts',(-19.6112871208758,-20.8796902727224,
-4.56362576714972));
#76335=CARTESIAN_POINT('Ctrl Pts',(-19.6953393038403,-20.8383914171856,
-4.56901248367176));
#76336=CARTESIAN_POINT('Ctrl Pts',(-19.7227978808744,-20.8241443212404,
-4.5708188659577));
#76337=CARTESIAN_POINT('Ctrl Pts',(-19.7561871501496,-20.8058805923223,
-4.57308543694436));
#76338=CARTESIAN_POINT('Ctrl Pts',(-19.7624240636873,-20.8024279943996,
-4.57351187890429));
#76339=CARTESIAN_POINT('Ctrl Pts',(-19.7722074770424,-20.7969474042102,
-4.57418582534221));
#76340=CARTESIAN_POINT('Ctrl Pts',(-19.7757658138193,-20.7949404977365,
-4.57443199751141));
#76341=CARTESIAN_POINT('Ctrl Pts',(-19.7824276977631,-20.7911577279672,
-4.57489489396021));
#76342=CARTESIAN_POINT('Ctrl Pts',(-19.7855325623306,-20.7893842971619,
-4.57511146199046));
#76343=CARTESIAN_POINT('Ctrl Pts',(-19.7926381815843,-20.7853018131917,
-4.57560897879283));
#76344=CARTESIAN_POINT('Ctrl Pts',(-19.7966358701506,-20.7829875325341,
-4.57589026235824));
#76345=CARTESIAN_POINT('Ctrl Pts',(-19.8089993459826,-20.7757761306816,
-4.57676436928368));
#76346=CARTESIAN_POINT('Ctrl Pts',(-19.8173389570027,-20.7708346996762,
-4.57735995760433));
#76347=CARTESIAN_POINT('Ctrl Pts',(-19.9078161053869,-20.7163816868856,
-4.58388436068923));
#76348=CARTESIAN_POINT('Ctrl Pts',(-19.986523198797,-20.661405824452,-4.59012233657905));
#76349=CARTESIAN_POINT('Ctrl Pts',(-20.1599400145677,-20.5218534134479,
-4.60477531850831));
#76350=CARTESIAN_POINT('Ctrl Pts',(-20.2513338677791,-20.4337041015626,
-4.61320515862001));
#76351=CARTESIAN_POINT('Ctrl Pts',(-20.3724500085333,-20.2938520750625,
-4.62512676308915));
#76352=CARTESIAN_POINT('Ctrl Pts',(-20.4087695858815,-20.2482381017544,
-4.62882513898398));
#76353=CARTESIAN_POINT('Ctrl Pts',(-20.4642421849682,-20.1723389341196,
-4.63467555352348));
#76354=CARTESIAN_POINT('Ctrl Pts',(-20.4845888313357,-20.142967724368,-4.63687127240738));
#76355=CARTESIAN_POINT('Ctrl Pts',(-20.5101992127512,-20.1039225947349,
-4.63970433693292));
#76356=CARTESIAN_POINT('Ctrl Pts',(-20.5161437266752,-20.0947042715433,
-4.64036713243605));
#76357=CARTESIAN_POINT('Ctrl Pts',(-20.5257284537054,-20.0795842397072,
-4.64144451610046));
#76358=CARTESIAN_POINT('Ctrl Pts',(-20.5294117352557,-20.0737101997125,
-4.6418607000435));
#76359=CARTESIAN_POINT('Ctrl Pts',(-20.5364622218308,-20.0623424943512,
-4.64266159601023));
#76360=CARTESIAN_POINT('Ctrl Pts',(-20.5398333285156,-20.0568513506027,
-4.643046449035));
#76361=CARTESIAN_POINT('Ctrl Pts',(-20.5475262599853,-20.0441911806493,
-4.64392917004843));
#76362=CARTESIAN_POINT('Ctrl Pts',(-20.5518307570477,-20.037011710788,-4.64442639942141));
#76363=CARTESIAN_POINT('Ctrl Pts',(-20.5632211405642,-20.0177556314884,
-4.64575121615546));
#76364=CARTESIAN_POINT('Ctrl Pts',(-20.5702300657121,-20.005633810653,-4.64657601092085));
#76365=CARTESIAN_POINT('Ctrl Pts',(-20.6269881215836,-19.9051849130035,
-4.6533376470631));
#76366=CARTESIAN_POINT('Ctrl Pts',(-20.6704575918116,-19.8134530243061,
-4.65904092207757));
#76367=CARTESIAN_POINT('Ctrl Pts',(-20.7124616914314,-19.7053857462978,
-4.66542611012426));
#76368=CARTESIAN_POINT('Ctrl Pts',(-20.7175920952023,-19.6917722147139,
-4.66622481928063));
#76369=CARTESIAN_POINT('Ctrl Pts',(-20.7225805678527,-19.6781104083805,
-4.66702139913379));
#76370=CARTESIAN_POINT('',(-20.8509999970068,-18.9521080404548,-3.68920542733227));
#76371=CARTESIAN_POINT('Ctrl Pts',(-20.7225805839746,-19.678110364228,-4.44630500845845));
#76372=CARTESIAN_POINT('Ctrl Pts',(-20.7059750529334,-19.7235875234065,
-4.44325060284348));
#76373=CARTESIAN_POINT('Ctrl Pts',(-20.6878139586179,-19.7684827791584,
-4.4401292757464));
#76374=CARTESIAN_POINT('Ctrl Pts',(-20.591907891162,-19.983994763893,-4.42474709701318));
#76375=CARTESIAN_POINT('Ctrl Pts',(-20.4932541629939,-20.1444257471549,
-4.41214843505669));
#76376=CARTESIAN_POINT('Ctrl Pts',(-20.3393458867707,-20.3331927496265,
-4.39674509708733));
#76377=CARTESIAN_POINT('Ctrl Pts',(-20.3022244749473,-20.3752012331731,
-4.39326454066552));
#76378=CARTESIAN_POINT('Ctrl Pts',(-20.2551575499931,-20.42438360834,-4.38912061286533));
#76379=CARTESIAN_POINT('Ctrl Pts',(-20.2467641763983,-20.4330058534641,
-4.38839137665417));
#76380=CARTESIAN_POINT('Ctrl Pts',(-20.2327633547897,-20.4471452342441,
-4.38719077628363));
#76381=CARTESIAN_POINT('Ctrl Pts',(-20.2271979391164,-20.4527034291847,
-4.38671758281733));
#76382=CARTESIAN_POINT('Ctrl Pts',(-20.2170712572065,-20.4627048652255,
-4.38586381042063));
#76383=CARTESIAN_POINT('Ctrl Pts',(-20.2125206967677,-20.4671587687003,
-4.3854827629929));
#76384=CARTESIAN_POINT('Ctrl Pts',(-20.2027146609815,-20.4766702731645,
-4.38466716985252));
#76385=CARTESIAN_POINT('Ctrl Pts',(-20.1974529921072,-20.4817213926687,
-4.3842329096807));
#76386=CARTESIAN_POINT('Ctrl Pts',(-20.1830322987544,-20.4954225290718,
-4.38305178219053));
#76387=CARTESIAN_POINT('Ctrl Pts',(-20.1738219073444,-20.5040182317033,
-4.38230725975863));
#76388=CARTESIAN_POINT('Ctrl Pts',(-20.1246867769961,-20.5490602827635,
-4.378386182477));
#76389=CARTESIAN_POINT('Ctrl Pts',(-20.0834517180678,-20.584051482861,-4.3752714719419));
#76390=CARTESIAN_POINT('Ctrl Pts',(-19.8904571533231,-20.7355010553542,
-4.36137514659493));
#76391=CARTESIAN_POINT('Ctrl Pts',(-19.7247036441514,-20.8326301520677,
-4.3513510585107));
#76392=CARTESIAN_POINT('Ctrl Pts',(-19.5328945419942,-20.9125433624371,
-4.33980005282473));
#76393=CARTESIAN_POINT('Ctrl Pts',(-19.5175474424909,-20.9187272689795,
-4.33887548281398));
#76394=CARTESIAN_POINT('Ctrl Pts',(-19.452565118001,-20.9440296882608,-4.33495319392707));
#76395=CARTESIAN_POINT('Ctrl Pts',(-19.4022951099149,-20.9614523489393,
-4.33190077680262));
#76396=CARTESIAN_POINT('Ctrl Pts',(-19.3430953186911,-20.9795028405317,
-4.32822794047945));
#76397=CARTESIAN_POINT('Ctrl Pts',(-19.3347479195817,-20.981991824327,-4.32770827127453));
#76398=CARTESIAN_POINT('Ctrl Pts',(-19.3220834068493,-20.9856831089112,
-4.32691680809558));
#76399=CARTESIAN_POINT('Ctrl Pts',(-19.3177773277268,-20.9869233675167,
-4.32664717278153));
#76400=CARTESIAN_POINT('Ctrl Pts',(-19.3100396533694,-20.989125430285,-4.32616165788158));
#76401=CARTESIAN_POINT('Ctrl Pts',(-19.3066095412356,-20.9900922486373,
-4.32594607368808));
#76402=CARTESIAN_POINT('Ctrl Pts',(-19.2991494694688,-20.9921746400132,
-4.32547642114468));
#76403=CARTESIAN_POINT('Ctrl Pts',(-19.295118693786,-20.9932869213757,-4.32522217096642));
#76404=CARTESIAN_POINT('Ctrl Pts',(-19.2837834444003,-20.9963787414552,
-4.32450584948313));
#76405=CARTESIAN_POINT('Ctrl Pts',(-19.2764716985071,-20.998331040325,-4.32404224614419));
#76406=CARTESIAN_POINT('Ctrl Pts',(-19.232618159204,-21.0097887625457,-4.32125312336358));
#76407=CARTESIAN_POINT('Ctrl Pts',(-19.1958402651079,-21.0183537503357,
-4.31887850060007));
#76408=CARTESIAN_POINT('Ctrl Pts',(-19.0738755684451,-21.0433388780075,
-4.31093035876734));
#76409=CARTESIAN_POINT('Ctrl Pts',(-18.9879109198764,-21.0555068432524,
-4.30521476113107));
#76410=CARTESIAN_POINT('Ctrl Pts',(-18.7261811852056,-21.0762739786108,
-4.28786797528356));
#76411=CARTESIAN_POINT('Ctrl Pts',(-18.5498271357661,-21.0682951159875,
-4.27632332416896));
#76412=CARTESIAN_POINT('Ctrl Pts',(-18.3538341836113,-21.0347122447921,
-4.26408410894484));
#76413=CARTESIAN_POINT('Ctrl Pts',(-18.3312640457341,-21.0304658185513,
-4.26268226389162));
#76414=CARTESIAN_POINT('Ctrl Pts',(-18.299419550179,-21.0239362625587,-4.26071447593337));
#76415=CARTESIAN_POINT('Ctrl Pts',(-18.2900852985823,-21.0219564695907,
-4.26013890950837));
#76416=CARTESIAN_POINT('Ctrl Pts',(-18.274936970614,-21.0186363318461,-4.25920675779561));
#76417=CARTESIAN_POINT('Ctrl Pts',(-18.2691146907666,-21.0173344144343,
-4.25884894658992));
#76418=CARTESIAN_POINT('Ctrl Pts',(-18.2569360706598,-21.0145570502935,
-4.25810144260337));
#76419=CARTESIAN_POINT('Ctrl Pts',(-18.2505808835106,-21.0130767908245,
-4.25771190874602));
#76420=CARTESIAN_POINT('Ctrl Pts',(-18.2354732802992,-21.0094841855936,
-4.2567871363927));
#76421=CARTESIAN_POINT('Ctrl Pts',(-18.2267272505224,-21.0073453300298,
-4.25625275703224));
#76422=CARTESIAN_POINT('Ctrl Pts',(-18.1972843532456,-20.999945638784,-4.2544569315623));
#76423=CARTESIAN_POINT('Ctrl Pts',(-18.1766530921176,-20.9944273544678,
-4.25320379655168));
#76424=CARTESIAN_POINT('Ctrl Pts',(-18.0646403429302,-20.9626433453724,
-4.24642355657773));
#76425=CARTESIAN_POINT('Ctrl Pts',(-17.9750191843356,-20.930555075165,-4.24109076819345));
#76426=CARTESIAN_POINT('Ctrl Pts',(-17.7316760138036,-20.8244484976068,
-4.22648574375833));
#76427=CARTESIAN_POINT('Ctrl Pts',(-17.5843122092003,-20.7377555286927,
-4.2175229278678));
#76428=CARTESIAN_POINT('Ctrl Pts',(-17.4194338798366,-20.6118144254466,
-4.20567685724372));
#76429=CARTESIAN_POINT('Ctrl Pts',(-17.3905232962856,-20.5885017510247,
-4.20352037051548));
#76430=CARTESIAN_POINT('Ctrl Pts',(-17.3567868496268,-20.5598010600513,
-4.20088718598271));
#76431=CARTESIAN_POINT('Ctrl Pts',(-17.3513546411945,-20.5551319717157,
-4.20045946944414));
#76432=CARTESIAN_POINT('Ctrl Pts',(-17.3425343964042,-20.5474726239438,
-4.19975869027246));
#76433=CARTESIAN_POINT('Ctrl Pts',(-17.3391320035622,-20.5444988826961,
-4.19948682220336));
#76434=CARTESIAN_POINT('Ctrl Pts',(-17.3330613329158,-20.539158647118,-4.19899892069522));
#76435=CARTESIAN_POINT('Ctrl Pts',(-17.3303894915829,-20.5367962835783,
-4.19878319535851));
#76436=CARTESIAN_POINT('Ctrl Pts',(-17.3246190913873,-20.5316682259454,
-4.19831513323318));
#76437=CARTESIAN_POINT('Ctrl Pts',(-17.3215227405428,-20.5289001999034,
-4.19806262490934));
#76438=CARTESIAN_POINT('Ctrl Pts',(-17.3129036055194,-20.5211492499445,
-4.19735600543973));
#76439=CARTESIAN_POINT('Ctrl Pts',(-17.3073989722264,-20.5161463597715,
-4.19690042684133));
#76440=CARTESIAN_POINT('Ctrl Pts',(-17.2757206373601,-20.487049153316,-4.19425429279777));
#76441=CARTESIAN_POINT('Ctrl Pts',(-17.2501328775237,-20.4623286462916,
-4.19202019468405));
#76442=CARTESIAN_POINT('Ctrl Pts',(-17.1701409974656,-20.3810525079773,
-4.18475370112295));
#76443=CARTESIAN_POINT('Ctrl Pts',(-17.1182555550447,-20.3221146949031,
-4.17960301470105));
#76444=CARTESIAN_POINT('Ctrl Pts',(-16.9534976510358,-20.1125549463459,
-4.16200818529868));
#76445=CARTESIAN_POINT('Ctrl Pts',(-16.8574333061634,-19.9497988824915,
-4.14960212188181));
#76446=CARTESIAN_POINT('Ctrl Pts',(-16.7756363194314,-19.7563492369065,
-4.13668902326418));
#76447=CARTESIAN_POINT('Ctrl Pts',(-16.7674421701439,-19.7361022625955,
-4.13535674821671));
#76448=CARTESIAN_POINT('Ctrl Pts',(-16.7565261363091,-19.7078815777027,
-4.1335256874127));
#76449=CARTESIAN_POINT('Ctrl Pts',(-16.753536519592,-19.7000135340097,-4.13301793609186));
#76450=CARTESIAN_POINT('Ctrl Pts',(-16.7484728288283,-19.686443775432,-4.13214690571609));
#76451=CARTESIAN_POINT('Ctrl Pts',(-16.746376212341,-19.6807506340686,-4.1317828754104));
#76452=CARTESIAN_POINT('Ctrl Pts',(-16.7420994336397,-19.6689817292357,
-4.13103321838409));
#76453=CARTESIAN_POINT('Ctrl Pts',(-16.7399225263875,-19.6629048438291,
-4.13064770341623));
#76454=CARTESIAN_POINT('Ctrl Pts',(-16.7349131486048,-19.6487169933402,
-4.12975124249218));
#76455=CARTESIAN_POINT('Ctrl Pts',(-16.7321021768789,-19.6405985167946,
-4.12924101486907));
#76456=CARTESIAN_POINT('Ctrl Pts',(-16.7232307638172,-19.6144631363991,
-4.12760708048881));
#76457=CARTESIAN_POINT('Ctrl Pts',(-16.7173634250955,-19.5963813217992,
-4.12648974845712));
#76458=CARTESIAN_POINT('Ctrl Pts',(-16.6891028975398,-19.5051196249743,
-4.12091263309419));
#76459=CARTESIAN_POINT('Ctrl Pts',(-16.6704446171377,-19.4308386516401,
-4.11657589146647));
#76460=CARTESIAN_POINT('Ctrl Pts',(-16.6348945456058,-19.2478371293008,
-4.10621551847124));
#76461=CARTESIAN_POINT('Ctrl Pts',(-16.6223700923974,-19.1385027329552,
-4.10030128258774));
#76462=CARTESIAN_POINT('Ctrl Pts',(-16.6158499422204,-18.9586296005015,
-4.09049861521862));
#76463=CARTESIAN_POINT('Ctrl Pts',(-16.6167921119604,-18.8884923012791,
-4.08665523106028));
#76464=CARTESIAN_POINT('Ctrl Pts',(-16.6242519040962,-18.7704011489976,
-4.07997133316755));
#76465=CARTESIAN_POINT('Ctrl Pts',(-16.6289363433943,-18.7223885939147,
-4.07719364272327));
#76466=CARTESIAN_POINT('Ctrl Pts',(-16.6362711963348,-18.6668983742835,
-4.07387055095543));
#76467=CARTESIAN_POINT('Ctrl Pts',(-16.6373290194225,-18.6592204485359,
-4.07340822687095));
#76468=CARTESIAN_POINT('Ctrl Pts',(-16.6390882420684,-18.6469503226795,
-4.07266509892751));
#76469=CARTESIAN_POINT('Ctrl Pts',(-16.6397626491681,-18.6423542401508,
-4.07238577830725));
#76470=CARTESIAN_POINT('Ctrl Pts',(-16.6409847634691,-18.6342121878138,
-4.07188918875754));
#76471=CARTESIAN_POINT('Ctrl Pts',(-16.6415263646599,-18.6306653470811,
-4.07167226758135));
#76472=CARTESIAN_POINT('Ctrl Pts',(-16.6426944554599,-18.6231439395748,
-4.0712109783146));
#76473=CARTESIAN_POINT('Ctrl Pts',(-16.6433232501197,-18.6191698391243,
-4.07096648742731));
#76474=CARTESIAN_POINT('Ctrl Pts',(-16.6450531811568,-18.608434704283,-4.07030404437638));
#76475=CARTESIAN_POINT('Ctrl Pts',(-16.6461757994061,-18.6016772504882,
-4.06988490316812));
#76476=CARTESIAN_POINT('Ctrl Pts',(-16.651940782872,-18.5679878934548,-4.06778492686652));
#76477=CARTESIAN_POINT('Ctrl Pts',(-16.6570713312078,-18.5411435506829,
-4.06607862011139));
#76478=CARTESIAN_POINT('Ctrl Pts',(-16.6734618060952,-18.4635616165769,
-4.0610657501009));
#76479=CARTESIAN_POINT('Ctrl Pts',(-16.6860717907079,-18.4131317184198,
-4.05770556997723));
#76480=CARTESIAN_POINT('Ctrl Pts',(-16.7391454266503,-18.2298304943454,
-4.04523014415083));
#76481=CARTESIAN_POINT('Ctrl Pts',(-16.7908028922377,-18.1005525454839,
-4.03594380839722));
#76482=CARTESIAN_POINT('Ctrl Pts',(-16.898623103787,-17.8926792547821,-4.02078720699884));
#76483=CARTESIAN_POINT('Ctrl Pts',(-16.9481619569181,-17.8111425896993,
-4.01476927491229));
#76484=CARTESIAN_POINT('Ctrl Pts',(-17.0110098080695,-17.7218838531483,
-4.00810746113588));
#76485=CARTESIAN_POINT('Ctrl Pts',(-17.019096971541,-17.7106343997278,-4.00726627211872));
#76486=CARTESIAN_POINT('Ctrl Pts',(-17.0322212446878,-17.6927512486061,
-4.00592627440369));
#76487=CARTESIAN_POINT('Ctrl Pts',(-17.0371879774477,-17.6860666237372,
-4.0054247607819));
#76488=CARTESIAN_POINT('Ctrl Pts',(-17.0460632962751,-17.6742675890925,
-4.00453835475868));
#76489=CARTESIAN_POINT('Ctrl Pts',(-17.0499559830554,-17.6691414029297,
-4.00415284763788));
#76490=CARTESIAN_POINT('Ctrl Pts',(-17.058101743891,-17.6585154158186,-4.00335286100862));
#76491=CARTESIAN_POINT('Ctrl Pts',(-17.0623586579445,-17.6530186453811,
-4.00293853933194));
#76492=CARTESIAN_POINT('Ctrl Pts',(-17.073454498603,-17.6388359391721,-4.00186816347282));
#76493=CARTESIAN_POINT('Ctrl Pts',(-17.0803345773694,-17.6301823537766,
-4.00121375332688));
#76494=CARTESIAN_POINT('Ctrl Pts',(-17.1102289631788,-17.5931807114727,
-3.99840935811378));
#76495=CARTESIAN_POINT('Ctrl Pts',(-17.1339075922544,-17.5653757678634,
-3.99628627007465));
#76496=CARTESIAN_POINT('Ctrl Pts',(-17.1984212854729,-17.4934743137192,
-3.99073907288807));
#76497=CARTESIAN_POINT('Ctrl Pts',(-17.2404354309439,-17.4504791556932,
-3.98736295770136));
#76498=CARTESIAN_POINT('Ctrl Pts',(-17.4057125679295,-17.2951547469706,
-3.97480002707343));
#76499=CARTESIAN_POINT('Ctrl Pts',(-17.5402502319539,-17.1957432471182,
-3.96602173154569));
#76500=CARTESIAN_POINT('Ctrl Pts',(-17.7323969635959,-17.0861349624229,
-3.95359315730816));
#76501=CARTESIAN_POINT('Ctrl Pts',(-17.7807716781396,-17.0609643930868,
-3.95046757089726));
#76502=CARTESIAN_POINT('Ctrl Pts',(-17.83798496002,-17.0339481559771,-3.94671321259899));
#76503=CARTESIAN_POINT('Ctrl Pts',(-17.8459339283735,-17.0302548361845,
-3.94619033276576));
#76504=CARTESIAN_POINT('Ctrl Pts',(-17.857991688379,-17.0247432386701,-3.94539493128373));
#76505=CARTESIAN_POINT('Ctrl Pts',(-17.8620838225065,-17.0228884519835,
-3.94512460056052));
#76506=CARTESIAN_POINT('Ctrl Pts',(-17.8694331455228,-17.019585484245,-3.94463834535009));
#76507=CARTESIAN_POINT('Ctrl Pts',(-17.872688113209,-17.018132491626,-3.94442272021774));
#76508=CARTESIAN_POINT('Ctrl Pts',(-17.8797611811931,-17.0149965280794,
-3.94395357670426));
#76509=CARTESIAN_POINT('Ctrl Pts',(-17.8835805411395,-17.0133166444499,
-3.94369987975458));
#76510=CARTESIAN_POINT('Ctrl Pts',(-17.8943035217731,-17.0086380993906,
-3.94298664442694));
#76511=CARTESIAN_POINT('Ctrl Pts',(-17.9012181245005,-17.0056649835608,
-3.94252559469452));
#76512=CARTESIAN_POINT('Ctrl Pts',(-17.9422593749615,-16.9882769531812,
-3.93978303617392));
#76513=CARTESIAN_POINT('Ctrl Pts',(-17.9767415780873,-16.9747239147111,
-3.93745427279839));
#76514=CARTESIAN_POINT('Ctrl Pts',(-18.0904942376852,-16.9334259096005,
-3.92973304932975));
#76515=CARTESIAN_POINT('Ctrl Pts',(-18.1710597367467,-16.9094923620726,
-3.92420662595751));
#76516=CARTESIAN_POINT('Ctrl Pts',(-18.4279500089406,-16.8495345638189,
-3.90678197133828));
#76517=CARTESIAN_POINT('Ctrl Pts',(-18.6076051857285,-16.8311329485589,
-3.89495694896189));
#76518=CARTESIAN_POINT('Ctrl Pts',(-18.8100807322765,-16.8362463906006,
-3.88249451686865));
#76519=CARTESIAN_POINT('Ctrl Pts',(-18.8327045134775,-16.8371810727607,
-3.88111267460419));
#76520=CARTESIAN_POINT('Ctrl Pts',(-18.8647825400151,-16.8390222532311,
-3.87916783765606));
#76521=CARTESIAN_POINT('Ctrl Pts',(-18.8742517772229,-16.8396296549411,
-3.87859552139535));
#76522=CARTESIAN_POINT('Ctrl Pts',(-18.889658208021,-16.840721950844,-3.87766719336879));
#76523=CARTESIAN_POINT('Ctrl Pts',(-18.8955979253899,-16.8411682705131,
-3.87730997557107));
#76524=CARTESIAN_POINT('Ctrl Pts',(-18.9080490546663,-16.8421567315635,
-3.87656256512833));
#76525=CARTESIAN_POINT('Ctrl Pts',(-18.9145600085186,-16.8427039620772,
-3.87617253644228));
#76526=CARTESIAN_POINT('Ctrl Pts',(-18.9300836147993,-16.8440810902564,
-3.87524449652174));
#76527=CARTESIAN_POINT('Ctrl Pts',(-18.9390937311685,-16.8449386626497,
-3.874707360787));
#76528=CARTESIAN_POINT('Ctrl Pts',(-18.9696216472435,-16.8480419476245,
-3.87289236579694));
#76529=CARTESIAN_POINT('Ctrl Pts',(-18.9911108687225,-16.8505597560181,
-3.87162306511117));
#76530=CARTESIAN_POINT('Ctrl Pts',(-19.1091483882639,-16.8662275521552,
-3.86469120335776));
#76531=CARTESIAN_POINT('Ctrl Pts',(-19.2047439228792,-16.8857022471294,
-3.85923328847979));
#76532=CARTESIAN_POINT('Ctrl Pts',(-19.4494677928498,-16.9534311374556,
-3.84527878745208));
#76533=CARTESIAN_POINT('Ctrl Pts',(-19.5951621838004,-17.0117516735864,
-3.8370068749821));
#76534=CARTESIAN_POINT('Ctrl Pts',(-19.774743453748,-17.107881141832,-3.82549065724233));
#76535=CARTESIAN_POINT('Ctrl Pts',(-19.8156366621528,-17.1315652447075,
-3.82276760727552));
#76536=CARTESIAN_POINT('Ctrl Pts',(-19.8627994039801,-17.1610307145722,
-3.81946565200369));
#76537=CARTESIAN_POINT('Ctrl Pts',(-19.8698723625714,-17.1655081734109,
-3.81896606295435));
#76538=CARTESIAN_POINT('Ctrl Pts',(-19.880586834266,-17.1723802023097,-3.81820225254096));
#76539=CARTESIAN_POINT('Ctrl Pts',(-19.8842479096312,-17.1747443238376,
-3.81794000883896));
#76540=CARTESIAN_POINT('Ctrl Pts',(-19.8907254749626,-17.1789555786331,
-3.81747374310823));
#76541=CARTESIAN_POINT('Ctrl Pts',(-19.893544881643,-17.1807981448131,-3.81727002725082));
#76542=CARTESIAN_POINT('Ctrl Pts',(-19.8963810206393,-17.1826613202964,
-3.81706431919753));
#76543=CARTESIAN_POINT('Ctrl Pts',(-19.8964021259494,-17.1826751857768,
-3.81706278836429));
#76544=CARTESIAN_POINT('Ctrl Pts',(-19.8964439371482,-17.1827026554021,
-3.81705975558274));
#76545=CARTESIAN_POINT('Ctrl Pts',(-19.8964646431052,-17.1827162595717,
-3.81705825363111));
#76546=CARTESIAN_POINT('Ctrl Pts',(-19.8965056793506,-17.1827432221214,
-3.81705527689466));
#76547=CARTESIAN_POINT('Ctrl Pts',(-19.8965260095775,-17.1827565804425,
-3.81705380211581));
#76548=CARTESIAN_POINT('Ctrl Pts',(-19.8965663163984,-17.1827830657188,
-3.8170508781309));
#76549=CARTESIAN_POINT('Ctrl Pts',(-19.896586292861,-17.1827961925705,-3.81704942893576));
#76550=CARTESIAN_POINT('Ctrl Pts',(-19.8966259124454,-17.182822228191,-3.81704655465032));
#76551=CARTESIAN_POINT('Ctrl Pts',(-19.8966455555369,-17.182835136924,-3.81704512956349));
#76552=CARTESIAN_POINT('Ctrl Pts',(-19.8966845271922,-17.182860748623,-3.81704230213364));
#76553=CARTESIAN_POINT('Ctrl Pts',(-19.8967038558692,-17.1828734516486,
-3.81704089978359));
#76554=CARTESIAN_POINT('Ctrl Pts',(-19.8967422163445,-17.1828986634879,
-3.81703811655034));
#76555=CARTESIAN_POINT('Ctrl Pts',(-19.8967612482861,-17.182911172382,-3.81703673565787));
#76556=CARTESIAN_POINT('Ctrl Pts',(-19.8967990320516,-17.1829360069337,
-3.81703399412695));
#76557=CARTESIAN_POINT('Ctrl Pts',(-19.8968177838715,-17.182948332576,-3.81703263348984));
#76558=CARTESIAN_POINT('Ctrl Pts',(-19.896855023109,-17.1829728109156,-3.8170299313324));
#76559=CARTESIAN_POINT('Ctrl Pts',(-19.8968735104283,-17.1829849635366,
-3.81702858982017));
#76560=CARTESIAN_POINT('Ctrl Pts',(-19.8969102351793,-17.1830091053395,
-3.81702592486214));
#76561=CARTESIAN_POINT('Ctrl Pts',(-19.8969284726153,-17.1830210945133,
-3.81702460141691));
#76562=CARTESIAN_POINT('Ctrl Pts',(-19.8969647110558,-17.1830449182348,
-3.81702197161905));
#76563=CARTESIAN_POINT('Ctrl Pts',(-19.8969827122019,-17.1830567528652,
-3.81702066525698));
#76564=CARTESIAN_POINT('Ctrl Pts',(-19.8970184914677,-17.1830802762825,
-3.8170180686551));
#76565=CARTESIAN_POINT('Ctrl Pts',(-19.8970362694361,-17.1830919649601,
-3.81701677842706));
#76566=CARTESIAN_POINT('Ctrl Pts',(-19.8970716142431,-17.1831152042646,
-3.81701421323215));
#76567=CARTESIAN_POINT('Ctrl Pts',(-19.8970891811503,-17.1831267549276,
-3.81701293826105));
#76568=CARTESIAN_POINT('Ctrl Pts',(-19.8971241154634,-17.183149725822,-3.81701040273822));
#76569=CARTESIAN_POINT('Ctrl Pts',(-19.897141482875,-17.1831611460488,-3.81700914218676));
#76570=CARTESIAN_POINT('Ctrl Pts',(-19.8971760290475,-17.1831838631808,
-3.81700663471771));
#76571=CARTESIAN_POINT('Ctrl Pts',(-19.8971932078295,-17.1831951600919,
-3.81700538779921));
#76572=CARTESIAN_POINT('Ctrl Pts',(-19.897227387305,-17.1832176375151,-3.81700290683131));
#76573=CARTESIAN_POINT('Ctrl Pts',(-19.8972443878677,-17.1832288179337,
-3.817001672792));
#76574=CARTESIAN_POINT('Ctrl Pts',(-19.8972782207694,-17.1832510688373,
-3.81699921686815));
#76575=CARTESIAN_POINT('Ctrl Pts',(-19.8972950529995,-17.1832621392437,
-3.81699799499209));
#76576=CARTESIAN_POINT('Ctrl Pts',(-19.8973285583645,-17.1832841761064,
-3.81699556273376));
#76577=CARTESIAN_POINT('Ctrl Pts',(-19.897345231592,-17.183295142617,-3.8169943523453));
#76578=CARTESIAN_POINT('Ctrl Pts',(-19.8973784275216,-17.1833169773053,
-3.81699194244158));
#76579=CARTESIAN_POINT('Ctrl Pts',(-19.8973949504846,-17.1833278456486,
-3.81699074290788));
#76580=CARTESIAN_POINT('Ctrl Pts',(-19.8974278547195,-17.1833494897954,
-3.8169883540738));
#76581=CARTESIAN_POINT('Ctrl Pts',(-19.8974442359604,-17.1833602655727,
-3.81698716477612));
#76582=CARTESIAN_POINT('Ctrl Pts',(-19.8974768649881,-17.1833817299893,
-3.81698479581742));
#76583=CARTESIAN_POINT('Ctrl Pts',(-19.8974931126518,-17.1833924185422,
-3.81698361616577));
#76584=CARTESIAN_POINT('Ctrl Pts',(-19.90101725197,-17.1857108491017,-3.81672774259221));
#76585=CARTESIAN_POINT('Ctrl Pts',(-19.9045182350899,-17.1880289992199,
-3.81647234691026));
#76586=CARTESIAN_POINT('Ctrl Pts',(-19.9146081885047,-17.1947532518542,
-3.81573286041144));
#76587=CARTESIAN_POINT('Ctrl Pts',(-19.9211792553152,-17.1991859083652,
-3.81524703302925));
#76588=CARTESIAN_POINT('Ctrl Pts',(-19.9646746055134,-17.2288834234257,
-3.81200380529768));
#76589=CARTESIAN_POINT('Ctrl Pts',(-20.0008121180661,-17.2552745868262,
-3.80917735043901));
#76590=CARTESIAN_POINT('Ctrl Pts',(-20.1294156491835,-17.3555929152385,
-3.79870576291934));
#76591=CARTESIAN_POINT('Ctrl Pts',(-20.216473553393,-17.4360940750762,-3.79081709998143));
#76592=CARTESIAN_POINT('Ctrl Pts',(-20.3960790574005,-17.6325203492072,
-3.77328192696135));
#76593=CARTESIAN_POINT('Ctrl Pts',(-20.4841331800545,-17.7517573356269,
-3.76375301034587));
#76594=CARTESIAN_POINT('Ctrl Pts',(-20.5662675611358,-17.891487325838,-3.75385703836535));
#76595=CARTESIAN_POINT('Ctrl Pts',(-20.5733557627424,-17.9038292404177,
-3.75299259719209));
#76596=CARTESIAN_POINT('Ctrl Pts',(-20.5844473891295,-17.9236009249835,
-3.75162281076882));
#76597=CARTESIAN_POINT('Ctrl Pts',(-20.5885316858317,-17.9309846098627,
-3.75111456735481));
#76598=CARTESIAN_POINT('Ctrl Pts',(-20.5956619115805,-17.9440587412643,
-3.75022037175344));
#76599=CARTESIAN_POINT('Ctrl Pts',(-20.5987261475108,-17.9497390308349,
-3.74983376889326));
#76600=CARTESIAN_POINT('Ctrl Pts',(-20.6050148169184,-17.9615252491383,
-3.74903547104967));
#76601=CARTESIAN_POINT('Ctrl Pts',(-20.6082354533443,-17.9676331251069,
-3.74862391431566));
#76602=CARTESIAN_POINT('Ctrl Pts',(-20.6164350746077,-17.9833696844013,
-3.74756898125616));
#76603=CARTESIAN_POINT('Ctrl Pts',(-20.621370133545,-17.9930211243061,-3.74692715903245));
#76604=CARTESIAN_POINT('Ctrl Pts',(-20.6417352834016,-18.0336152246479,
-3.74424881006918));
#76605=CARTESIAN_POINT('Ctrl Pts',(-20.6564807857285,-18.064896659469,-3.74223621312865));
#76606=CARTESIAN_POINT('Ctrl Pts',(-20.6929644865468,-18.1474813595387,
-3.73704320781428));
#76607=CARTESIAN_POINT('Ctrl Pts',(-20.7134559977444,-18.1993070222144,
-3.73390317844735));
#76608=CARTESIAN_POINT('Ctrl Pts',(-20.7653540629842,-18.3474054561233,
-3.72518160212191));
#76609=CARTESIAN_POINT('Ctrl Pts',(-20.7919349482263,-18.4452075808195,
-3.71971762169302));
#76610=CARTESIAN_POINT('Ctrl Pts',(-20.8347036733654,-18.6632602447623,
-3.70763489487761));
#76611=CARTESIAN_POINT('Ctrl Pts',(-20.847766551041,-18.7837459212227,-3.70102041173113));
#76612=CARTESIAN_POINT('Ctrl Pts',(-20.850728113419,-18.9161735210989,-3.69321415810316));
#76613=CARTESIAN_POINT('Ctrl Pts',(-20.8508915887521,-18.9276806435142,
-3.69253136286732));
#76614=CARTESIAN_POINT('Ctrl Pts',(-20.8509827903195,-18.9427504062806,
-3.69163064214214));
#76615=CARTESIAN_POINT('Ctrl Pts',(-20.8509953572148,-18.9463125920937,
-3.69141725226841));
#76616=CARTESIAN_POINT('Ctrl Pts',(-20.850999717921,-18.9506563959296,-3.69115643925956));
#76617=CARTESIAN_POINT('Ctrl Pts',(-20.8510000697051,-18.9514380271121,
-3.69110948441178));
#76618=CARTESIAN_POINT('Ctrl Pts',(-20.8509999886044,-18.9522196567131,
-3.69106250577301));
#76619=CARTESIAN_POINT('Ctrl Pts',(-20.8509999976816,-18.952099076172,-3.6890562790225));
#76620=CARTESIAN_POINT('Ctrl Pts',(-20.8509997507685,-18.9573749670545,
-3.68873698393553));
#76621=CARTESIAN_POINT('Ctrl Pts',(-20.8509797813958,-18.9626508039048,
-3.68841768884856));
#76622=CARTESIAN_POINT('Ctrl Pts',(-20.8509400905189,-18.9679264921966,
-3.68809839376159));
#76623=CARTESIAN_POINT('Ctrl Pts',(-20.8503947174663,-19.0404171615265,
-3.68371111511894));
#76624=CARTESIAN_POINT('Ctrl Pts',(-20.8461205125485,-19.1130212561315,
-3.67932383647628));
#76625=CARTESIAN_POINT('Ctrl Pts',(-20.8381029246827,-19.1853235571938,
-3.67493655783363));
#76626=CARTESIAN_POINT('Ctrl Pts',(-20.8300957679123,-19.257531791037,-3.67055498715732));
#76627=CARTESIAN_POINT('Ctrl Pts',(-20.8183549391221,-19.3294385348818,
-3.66617341648101));
#76628=CARTESIAN_POINT('Ctrl Pts',(-20.8029178766228,-19.4006288218456,
-3.6617918458047));
#76629=CARTESIAN_POINT('Ctrl Pts',(-20.7874985864907,-19.4717371489208,
-3.65741531953908));
#76630=CARTESIAN_POINT('Ctrl Pts',(-20.7683916165406,-19.542130188401,-3.65303879327345));
#76631=CARTESIAN_POINT('Ctrl Pts',(-20.7456859385557,-19.6114002461458,
-3.64866226700783));
#76632=CARTESIAN_POINT('Ctrl Pts',(-20.7383572889959,-19.6337583531595,
-3.64724966759936));
#76633=CARTESIAN_POINT('Ctrl Pts',(-20.730654129157,-19.6559995449129,-3.64583706819089));
#76634=CARTESIAN_POINT('Ctrl Pts',(-20.7225805821191,-19.6781103693095,
-3.64442446878243));
#76635=CARTESIAN_POINT('Origin',(-18.734,-18.952,0.));
#76636=CARTESIAN_POINT('',(-20.7202230519095,-19.6772708889146,-2.84456322442383));
#76637=CARTESIAN_POINT('',(-20.7225805657411,-19.6781104141636,-3.06515450115675));
#76638=CARTESIAN_POINT('',(-20.7225805821191,-19.6781103693095,0.));
#76639=CARTESIAN_POINT('Ctrl Pts',(-20.7225805657411,-19.6781104141636,
-3.06515450115675));
#76640=CARTESIAN_POINT('Ctrl Pts',(-20.7750121871659,-19.5345172341707,
-3.0751267565293));
#76641=CARTESIAN_POINT('Ctrl Pts',(-20.8117530434534,-19.3856243798708,
-3.08537389662126));
#76642=CARTESIAN_POINT('Ctrl Pts',(-20.8399080668057,-19.17616159463,-3.09899381870072));
#76643=CARTESIAN_POINT('Ctrl Pts',(-20.8452891027995,-19.1180014933404,
-3.10269885507837));
#76644=CARTESIAN_POINT('Ctrl Pts',(-20.8500786753983,-19.0239677445121,
-3.10855854633529));
#76645=CARTESIAN_POINT('Ctrl Pts',(-20.8509926290102,-18.9882045641041,
-3.11075705378731));
#76646=CARTESIAN_POINT('Ctrl Pts',(-20.8510022031607,-18.9414601962185,
-3.11359314044188));
#76647=CARTESIAN_POINT('Ctrl Pts',(-20.8509191302795,-18.9304867805795,
-3.11425623710019));
#76648=CARTESIAN_POINT('Ctrl Pts',(-20.8506443291055,-18.9125808604659,
-3.11533398638087));
#76649=CARTESIAN_POINT('Ctrl Pts',(-20.8505038547663,-18.9056478799212,
-3.11575023684162));
#76650=CARTESIAN_POINT('Ctrl Pts',(-20.8501671510856,-18.8922748000332,
-3.11655117669939));
#76651=CARTESIAN_POINT('Ctrl Pts',(-20.8499755814641,-18.8858346698847,
-3.11693600754339));
#76652=CARTESIAN_POINT('Ctrl Pts',(-20.8494626513867,-18.8708874756035,
-3.1178271791705));
#76653=CARTESIAN_POINT('Ctrl Pts',(-20.8491193705504,-18.8623812375752,
-3.11833282785324));
#76654=CARTESIAN_POINT('Ctrl Pts',(-20.8478634332364,-18.835313502854,-3.11993722523715));
#76655=CARTESIAN_POINT('Ctrl Pts',(-20.8467576626712,-18.8167615275721,
-3.12102992330274));
#76656=CARTESIAN_POINT('Ctrl Pts',(-20.8436139259455,-18.7735961489326,
-3.12355760465782));
#76657=CARTESIAN_POINT('Ctrl Pts',(-20.8413892485388,-18.7489988246942,
-3.12498678499905));
#76658=CARTESIAN_POINT('Ctrl Pts',(-20.8320826356473,-18.6629186365409,
-3.12995537998052));
#76659=CARTESIAN_POINT('Ctrl Pts',(-20.8227356958111,-18.6017103544863,
-3.13342821369199));
#76660=CARTESIAN_POINT('Ctrl Pts',(-20.7831184061431,-18.4015323427769,
-3.14471637276859));
#76661=CARTESIAN_POINT('Ctrl Pts',(-20.7415406505033,-18.2652110975059,
-3.15226989085367));
#76662=CARTESIAN_POINT('Ctrl Pts',(-20.6575308786554,-18.0646525712234,
-3.16430917626056));
#76663=CARTESIAN_POINT('Ctrl Pts',(-20.624765051529,-17.9968238532109,-3.16856377200981));
#76664=CARTESIAN_POINT('Ctrl Pts',(-20.5838855720109,-17.9225815359599,
-3.17358685068925));
#76665=CARTESIAN_POINT('Ctrl Pts',(-20.5792539110375,-17.9143020671391,
-3.17415234859705));
#76666=CARTESIAN_POINT('Ctrl Pts',(-20.5723045530033,-17.9020731754783,
-3.17499594404416));
#76667=CARTESIAN_POINT('Ctrl Pts',(-20.5700293647512,-17.8980995600578,
-3.17527137574389));
#76668=CARTESIAN_POINT('Ctrl Pts',(-20.5659565571533,-17.8910396192182,
-3.1757631411735));
#76669=CARTESIAN_POINT('Ctrl Pts',(-20.5641640012562,-17.8879504310608,
-3.17597914657379));
#76670=CARTESIAN_POINT('Ctrl Pts',(-20.5602911281429,-17.8813148833034,
-3.17644491875611));
#76671=CARTESIAN_POINT('Ctrl Pts',(-20.5582083254959,-17.8777700951956,
-3.17669484162145));
#76672=CARTESIAN_POINT('Ctrl Pts',(-20.5524255212133,-17.8679934733214,
-3.17738713606048));
#76673=CARTESIAN_POINT('Ctrl Pts',(-20.5487038640988,-17.8617746066947,
-3.17783088201754));
#76674=CARTESIAN_POINT('Ctrl Pts',(-20.5280540698229,-17.827667617119,-3.18028270346098));
#76675=CARTESIAN_POINT('Ctrl Pts',(-20.5105159352334,-17.8001561853588,
-3.18232731782027));
#76676=CARTESIAN_POINT('Ctrl Pts',(-20.4017832506917,-17.6379845704622,
-3.19473521305806));
#76677=CARTESIAN_POINT('Ctrl Pts',(-20.2959558316742,-17.5137957579558,
-3.2056869923486));
#76678=CARTESIAN_POINT('Ctrl Pts',(-20.0915015827885,-17.32334492249,-3.22393806664416));
#76679=CARTESIAN_POINT('Ctrl Pts',(-19.9995962773085,-17.250940984881,-3.23137718247265));
#76680=CARTESIAN_POINT('Ctrl Pts',(-19.8902556552171,-17.1785947909833,
-3.23938263451834));
#76681=CARTESIAN_POINT('Ctrl Pts',(-19.8782592703425,-17.1708307453977,
-3.24025058944005));
#76682=CARTESIAN_POINT('Ctrl Pts',(-19.8590411953543,-17.1586671290977,
-3.24162487099198));
#76683=CARTESIAN_POINT('Ctrl Pts',(-19.8518703296846,-17.1541884396987,
-3.2421341255113));
#76684=CARTESIAN_POINT('Ctrl Pts',(-19.8391760166392,-17.1463653023819,
-3.24302949654675));
#76685=CARTESIAN_POINT('Ctrl Pts',(-19.8336637737645,-17.1430029643198,
-3.24341626915737));
#76686=CARTESIAN_POINT('Ctrl Pts',(-19.8222308217142,-17.1361007014649,
-3.2442143391915));
#76687=CARTESIAN_POINT('Ctrl Pts',(-19.8163080139289,-17.132564387381,-3.2446255012173));
#76688=CARTESIAN_POINT('Ctrl Pts',(-19.8010605158282,-17.1235614075287,
-3.24567822398864));
#76689=CARTESIAN_POINT('Ctrl Pts',(-19.7917109790676,-17.1181370492328,
-3.24631824335776));
#76690=CARTESIAN_POINT('Ctrl Pts',(-19.7525150540193,-17.0957960684932,
-3.24897901160294));
#76691=CARTESIAN_POINT('Ctrl Pts',(-19.7223002429932,-17.0795340385118,
-3.25097622941703));
#76692=CARTESIAN_POINT('Ctrl Pts',(-19.6425552389293,-17.0390825099004,
-3.25612059037294));
#76693=CARTESIAN_POINT('Ctrl Pts',(-19.5924513360114,-17.0160795741263,
-3.25922833882827));
#76694=CARTESIAN_POINT('Ctrl Pts',(-19.4404220489694,-16.9533469142707,
-3.26837307984706));
#76695=CARTESIAN_POINT('Ctrl Pts',(-19.336257619456,-16.9195303418129,-3.27426134412098));
#76696=CARTESIAN_POINT('Ctrl Pts',(-19.1852144053711,-16.8831327257681,
-3.28272017749787));
#76697=CARTESIAN_POINT('Ctrl Pts',(-19.1401431065128,-16.8738147887076,
-3.28523616785355));
#76698=CARTESIAN_POINT('Ctrl Pts',(-19.0730021865743,-16.8622018945177,
-3.28901511602901));
#76699=CARTESIAN_POINT('Ctrl Pts',(-19.0511416504121,-16.8587728908796,
-3.29025036235558));
#76700=CARTESIAN_POINT('Ctrl Pts',(-18.9782517117143,-16.8485075153112,
-3.29439654873523));
#76701=CARTESIAN_POINT('Ctrl Pts',(-18.9270309001987,-16.8431904595562,
-3.29735466260615));
#76702=CARTESIAN_POINT('Ctrl Pts',(-18.8670518902524,-16.8391675801266,
-3.30092257068796));
#76703=CARTESIAN_POINT('Ctrl Pts',(-18.8584285234604,-16.83864220333,-3.30143804463868));
#76704=CARTESIAN_POINT('Ctrl Pts',(-18.84534323773,-16.8379253497651,-3.3022243592258));
#76705=CARTESIAN_POINT('Ctrl Pts',(-18.8408834109855,-16.8376951783223,
-3.30249308302644));
#76706=CARTESIAN_POINT('Ctrl Pts',(-18.8328642258223,-16.8373067458879,
-3.3029776318575));
#76707=CARTESIAN_POINT('Ctrl Pts',(-18.8293051702647,-16.8371433574955,
-3.30319316669541));
#76708=CARTESIAN_POINT('Ctrl Pts',(-18.8215561750979,-16.8368072189123,
-3.30366350593958));
#76709=CARTESIAN_POINT('Ctrl Pts',(-18.8173661830889,-16.8366379355352,
-3.30391849652393));
#76710=CARTESIAN_POINT('Ctrl Pts',(-18.8055578570849,-16.8361959951855,
-3.30463895542649));
#76711=CARTESIAN_POINT('Ctrl Pts',(-18.7979386040835,-16.8359520410562,
-3.30510598370228));
#76712=CARTESIAN_POINT('Ctrl Pts',(-18.7515930262247,-16.8347186778891,
-3.30795920468723));
#76713=CARTESIAN_POINT('Ctrl Pts',(-18.7128494621799,-16.8347513305589,
-3.31039710552513));
#76714=CARTESIAN_POINT('Ctrl Pts',(-18.5834881156202,-16.8384111118236,
-3.3186659456236));
#76715=CARTESIAN_POINT('Ctrl Pts',(-18.4931085004704,-16.8467966611819,
-3.32465075205842));
#76716=CARTESIAN_POINT('Ctrl Pts',(-18.3372551817402,-16.8714261675618,
-3.33507774052121));
#76717=CARTESIAN_POINT('Ctrl Pts',(-18.2714928771618,-16.885050162914,-3.33951216991325));
#76718=CARTESIAN_POINT('Ctrl Pts',(-18.0953521885325,-16.9303703012794,
-3.35138319824012));
#76719=CARTESIAN_POINT('Ctrl Pts',(-17.9867125146762,-16.9679570315923,
-3.35868705498082));
#76720=CARTESIAN_POINT('Ctrl Pts',(-17.8685879807642,-17.019914503744,-3.36656631690883));
#76721=CARTESIAN_POINT('Ctrl Pts',(-17.8555936119012,-17.0257875089062,
-3.36743244385989));
#76722=CARTESIAN_POINT('Ctrl Pts',(-17.8349986185777,-17.0353474890338,
-3.368804387101));
#76723=CARTESIAN_POINT('Ctrl Pts',(-17.8273591816184,-17.0389493573703,
-3.36931311579913));
#76724=CARTESIAN_POINT('Ctrl Pts',(-17.8139191417624,-17.0453847044799,
-3.37020787539313));
#76725=CARTESIAN_POINT('Ctrl Pts',(-17.8081095990445,-17.0481991601912,
-3.37059455956325));
#76726=CARTESIAN_POINT('Ctrl Pts',(-17.7961156722072,-17.0540775516699,
-3.37139274724937));
#76727=CARTESIAN_POINT('Ctrl Pts',(-17.7899332089932,-17.0571452488259,
-3.37180411388749));
#76728=CARTESIAN_POINT('Ctrl Pts',(-17.7740927119444,-17.0651019701378,
-3.37285798266288));
#76729=CARTESIAN_POINT('Ctrl Pts',(-17.7644568990954,-17.0700349740666,
-3.37349893683031));
#76730=CARTESIAN_POINT('Ctrl Pts',(-17.7243188278068,-17.0909735445627,
-3.37616880653635));
#76731=CARTESIAN_POINT('Ctrl Pts',(-17.6941706645162,-17.107648978816,-3.37817398504847));
#76732=CARTESIAN_POINT('Ctrl Pts',(-17.6166171846615,-17.1530515004375,
-3.38334350621631));
#76733=CARTESIAN_POINT('Ctrl Pts',(-17.5699084499522,-17.1829178713438,
-3.38646794689538));
#76734=CARTESIAN_POINT('Ctrl Pts',(-17.434470325509,-17.2772089951712,-3.39564179683054));
#76735=CARTESIAN_POINT('Ctrl Pts',(-17.3495146403673,-17.3467263700294,
-3.40154257811789));
#76736=CARTESIAN_POINT('Ctrl Pts',(-17.2253030156092,-17.4655930736365,
-3.41090428151993));
#76737=CARTESIAN_POINT('Ctrl Pts',(-17.182208059007,-17.5106418982638,-3.41431721164908));
#76738=CARTESIAN_POINT('Ctrl Pts',(-17.1041023086802,-17.5998578597279,
-3.4209698238421));
#76739=CARTESIAN_POINT('Ctrl Pts',(-17.0687455816744,-17.6436493600893,
-3.42419174947284));
#76740=CARTESIAN_POINT('Ctrl Pts',(-17.029907751694,-17.6958803306067,-3.42805339840083));
#76741=CARTESIAN_POINT('Ctrl Pts',(-17.024681887737,-17.7030009609612,-3.42858024845712));
#76742=CARTESIAN_POINT('Ctrl Pts',(-17.0168567957713,-17.7138043238606,
-3.42938051768936));
#76743=CARTESIAN_POINT('Ctrl Pts',(-17.0142244454959,-17.7174630999822,
-3.4296517057325));
#76744=CARTESIAN_POINT('Ctrl Pts',(-17.0095306783354,-17.724031241222,-3.4301388774044));
#76745=CARTESIAN_POINT('Ctrl Pts',(-17.0074649100795,-17.7269374314379,
-3.43035455679817));
#76746=CARTESIAN_POINT('Ctrl Pts',(-17.0030039146711,-17.7332470011605,
-3.43082308993311));
#76747=CARTESIAN_POINT('Ctrl Pts',(-17.0006114106405,-17.7366521826266,
-3.43107611829161));
#76748=CARTESIAN_POINT('Ctrl Pts',(-16.9939485295931,-17.7461949631425,
-3.43178562982335));
#76749=CARTESIAN_POINT('Ctrl Pts',(-16.9897006547124,-17.752348093499,-3.43224359956881));
#76750=CARTESIAN_POINT('Ctrl Pts',(-16.9650722077977,-17.7884302411408,
-3.43493133031106));
#76751=CARTESIAN_POINT('Ctrl Pts',(-16.9454309019536,-17.8188537886966,
-3.43720621601769));
#76752=CARTESIAN_POINT('Ctrl Pts',(-16.8845074363521,-17.91875455471,-3.44466644430703));
#76753=CARTESIAN_POINT('Ctrl Pts',(-16.8464214866401,-17.9900932937538,
-3.44997665662514));
#76754=CARTESIAN_POINT('Ctrl Pts',(-16.7350512317748,-18.2309259319501,
-3.46749639804901));
#76755=CARTESIAN_POINT('Ctrl Pts',(-16.6798104289505,-18.4078709953419,
-3.47965146933822));
#76756=CARTESIAN_POINT('Ctrl Pts',(-16.6444212787081,-18.6116428570199,
-3.49237191650146));
#76757=CARTESIAN_POINT('Ctrl Pts',(-16.6409656433381,-18.633582886672,-3.49372698156557));
#76758=CARTESIAN_POINT('Ctrl Pts',(-16.6366691327942,-18.6639651841717,
-3.49558404564725));
#76759=CARTESIAN_POINT('Ctrl Pts',(-16.6355328663374,-18.6723636041767,
-3.4960953457489));
#76760=CARTESIAN_POINT('Ctrl Pts',(-16.6336677996926,-18.6868007522204,
-3.49697084922426));
#76761=CARTESIAN_POINT('Ctrl Pts',(-16.6329145422906,-18.6928361651893,
-3.49733582144025));
#76762=CARTESIAN_POINT('Ctrl Pts',(-16.6314164660555,-18.7052753673423,
-3.49808595291603));
#76763=CARTESIAN_POINT('Ctrl Pts',(-16.630674867349,-18.7116794862016,-3.49847100687257));
#76764=CARTESIAN_POINT('Ctrl Pts',(-16.6290190463627,-18.7265735221345,
-3.49936392526794));
#76765=CARTESIAN_POINT('Ctrl Pts',(-16.6281269086576,-18.7350658198487,
-3.4998710889412));
#76766=CARTESIAN_POINT('Ctrl Pts',(-16.6254426677784,-18.7621960206922,
-3.5014852204105));
#76767=CARTESIAN_POINT('Ctrl Pts',(-16.6238463997406,-18.7808527228416,
-3.50258603174766));
#76768=CARTESIAN_POINT('Ctrl Pts',(-16.6207022632528,-18.8243943390283,
-3.50513524117928));
#76769=CARTESIAN_POINT('Ctrl Pts',(-16.6193460402236,-18.8492905426304,
-3.50657769657541));
#76770=CARTESIAN_POINT('Ctrl Pts',(-16.6161241558677,-18.9369077386372,
-3.51160756551674));
#76771=CARTESIAN_POINT('Ctrl Pts',(-16.6166070346251,-18.9996842644478,
-3.51512648289882));
#76772=CARTESIAN_POINT('Ctrl Pts',(-16.6251169534667,-19.162719350435,-3.5241519935401));
#76773=CARTESIAN_POINT('Ctrl Pts',(-16.6374969846859,-19.262589640145,-3.52956469392171));
#76774=CARTESIAN_POINT('Ctrl Pts',(-16.6713133767545,-19.4342388659572,
-3.53909562781371));
#76775=CARTESIAN_POINT('Ctrl Pts',(-16.6895436984001,-19.5064613544429,
-3.54318108101848));
#76776=CARTESIAN_POINT('Ctrl Pts',(-16.7242464782779,-19.618655404559,-3.549847139363));
#76777=CARTESIAN_POINT('Ctrl Pts',(-16.7382032335146,-19.6593424542716,
-3.55233361274859));
#76778=CARTESIAN_POINT('Ctrl Pts',(-16.7560328997254,-19.7065801780384,
-3.55533297897032));
#76779=CARTESIAN_POINT('Ctrl Pts',(-16.7587148310986,-19.713573103922,-3.55577993859825));
#76780=CARTESIAN_POINT('Ctrl Pts',(-16.7631101361496,-19.724854104536,-3.55650596691035));
#76781=CARTESIAN_POINT('Ctrl Pts',(-16.7648005588927,-19.7291511323694,
-3.55678369356958));
#76782=CARTESIAN_POINT('Ctrl Pts',(-16.7678248317406,-19.736765565053,-3.55727797960094));
#76783=CARTESIAN_POINT('Ctrl Pts',(-16.7691530418488,-19.7400851573319,
-3.55749419764027));
#76784=CARTESIAN_POINT('Ctrl Pts',(-16.7720172825604,-19.7471914956494,
-3.55795864190332));
#76785=CARTESIAN_POINT('Ctrl Pts',(-16.7735558461246,-19.750977106786,-3.55820701483607));
#76786=CARTESIAN_POINT('Ctrl Pts',(-16.7778103862272,-19.7613590572156,
-3.55889076094335));
#76787=CARTESIAN_POINT('Ctrl Pts',(-16.7805487299379,-19.7679460893235,
-3.55932745424807));
#76788=CARTESIAN_POINT('Ctrl Pts',(-16.7953642529426,-19.803082467704,-3.56167177331539));
#76789=CARTESIAN_POINT('Ctrl Pts',(-16.8080334423877,-19.831376205448,-3.56361233621496));
#76790=CARTESIAN_POINT('Ctrl Pts',(-16.8914421534581,-20.0071948713133,
-3.57595985721899));
#76791=CARTESIAN_POINT('Ctrl Pts',(-16.9784616229249,-20.1463786198815,
-3.58697916217434));
#76792=CARTESIAN_POINT('Ctrl Pts',(-17.1541016996981,-20.3660178360548,
-3.60535443711196));
#76793=CARTESIAN_POINT('Ctrl Pts',(-17.2351020366533,-20.4516125960041,
-3.61284962524372));
#76794=CARTESIAN_POINT('Ctrl Pts',(-17.3334673883594,-20.5395773632765,
-3.62090722677531));
#76795=CARTESIAN_POINT('Ctrl Pts',(-17.3442230955028,-20.5490014565223,
-3.62177583862196));
#76796=CARTESIAN_POINT('Ctrl Pts',(-17.3614909775208,-20.5638249013515,
-3.62315096039115));
#76797=CARTESIAN_POINT('Ctrl Pts',(-17.3679413048689,-20.5692953268043,
-3.62366040377535));
#76798=CARTESIAN_POINT('Ctrl Pts',(-17.3793739084945,-20.5788739495618,
-3.62455599451275));
#76799=CARTESIAN_POINT('Ctrl Pts',(-17.3843424904639,-20.5829982538114,
-3.62494279897377));
#76800=CARTESIAN_POINT('Ctrl Pts',(-17.3946567976818,-20.5914805131012,
-3.6257408271769));
#76801=CARTESIAN_POINT('Ctrl Pts',(-17.400005110778,-20.595835211843,-3.62615191605153));
#76802=CARTESIAN_POINT('Ctrl Pts',(-17.4137852881771,-20.6069437519117,
-3.62720422900319));
#76803=CARTESIAN_POINT('Ctrl Pts',(-17.4222478076719,-20.6136593813945,
-3.62784391405927));
#76804=CARTESIAN_POINT('Ctrl Pts',(-17.4577578247429,-20.6413988429035,
-3.63050143480448));
#76805=CARTESIAN_POINT('Ctrl Pts',(-17.4852631032338,-20.6618300789155,
-3.63249581268312));
#76806=CARTESIAN_POINT('Ctrl Pts',(-17.5581870839315,-20.7133000397434,
-3.6376312080087));
#76807=CARTESIAN_POINT('Ctrl Pts',(-17.6043416785304,-20.7432527913602,
-3.64073301059341));
#76808=CARTESIAN_POINT('Ctrl Pts',(-17.7399452826533,-20.8239263784107,
-3.64950725668404));
#76809=CARTESIAN_POINT('Ctrl Pts',(-17.8319897860291,-20.8699759324472,
-3.65505452014676));
#76810=CARTESIAN_POINT('Ctrl Pts',(-17.9865129944676,-20.9336896684191,
-3.6641437014595));
#76811=CARTESIAN_POINT('Ctrl Pts',(-18.0470955714514,-20.9554950339264,
-3.6676573038223));
#76812=CARTESIAN_POINT('Ctrl Pts',(-18.1672384902349,-20.9926471980787,
-3.67468495367161));
#76813=CARTESIAN_POINT('Ctrl Pts',(-18.2266586984968,-21.0082254039323,
-3.67818851473783));
#76814=CARTESIAN_POINT('Ctrl Pts',(-18.2955825262409,-21.0231258648863,
-3.6823707336775));
#76815=CARTESIAN_POINT('Ctrl Pts',(-18.3045117355898,-21.0249959125553,
-3.68291480586106));
#76816=CARTESIAN_POINT('Ctrl Pts',(-18.3178694090414,-21.0277034087792,
-3.68373245776881));
#76817=CARTESIAN_POINT('Ctrl Pts',(-18.3222890479464,-21.0285845518653,
-3.68400360443394));
#76818=CARTESIAN_POINT('Ctrl Pts',(-18.3302104133595,-21.0301375515718,
-3.68449073177888));
#76819=CARTESIAN_POINT('Ctrl Pts',(-18.3337110522616,-21.030814679468,-3.68470640845911));
#76820=CARTESIAN_POINT('Ctrl Pts',(-18.3413018670186,-21.032263084386,-3.68517497062505));
#76821=CARTESIAN_POINT('Ctrl Pts',(-18.3453925563355,-21.0330311333438,
-3.68542803091718));
#76822=CARTESIAN_POINT('Ctrl Pts',(-18.3568404762853,-21.0351456107814,
-3.68613772016426));
#76823=CARTESIAN_POINT('Ctrl Pts',(-18.3642025317645,-21.0364651042164,
-3.68659583686972));
#76824=CARTESIAN_POINT('Ctrl Pts',(-18.4062226472798,-21.0437667120568,
-3.68921981782216));
#76825=CARTESIAN_POINT('Ctrl Pts',(-18.4410163913472,-21.0489230413356,
-3.69142815028951));
#76826=CARTESIAN_POINT('Ctrl Pts',(-18.5527211397596,-21.0626431204196,
-3.6985975852703));
#76827=CARTESIAN_POINT('Ctrl Pts',(-18.6299767610013,-21.0678577332487,
-3.70367415276998));
#76828=CARTESIAN_POINT('Ctrl Pts',(-18.8713067416439,-21.0708972890744,
-3.71960110373368));
#76829=CARTESIAN_POINT('Ctrl Pts',(-19.0349889865895,-21.05390413415,-3.73044991121841));
#76830=CARTESIAN_POINT('Ctrl Pts',(-19.2357062130324,-21.009112618543,-3.74331746309862));
#76831=CARTESIAN_POINT('Ctrl Pts',(-19.2760555607942,-20.9988506547641,
-3.74588521346109));
#76832=CARTESIAN_POINT('Ctrl Pts',(-19.3276857353803,-20.984085626922,-3.74914844971681));
#76833=CARTESIAN_POINT('Ctrl Pts',(-19.3392645955762,-20.9806669333192,
-3.74987882979632));
#76834=CARTESIAN_POINT('Ctrl Pts',(-19.3576800302606,-20.9750580167046,
-3.75103828548124));
#76835=CARTESIAN_POINT('Ctrl Pts',(-19.3645356759786,-20.9729317856853,
-3.75146944321166));
#76836=CARTESIAN_POINT('Ctrl Pts',(-19.3768578510903,-20.9690413421671,
-3.7522435716577));
#76837=CARTESIAN_POINT('Ctrl Pts',(-19.3823282406043,-20.9672896779768,
-3.75258694985607));
#76838=CARTESIAN_POINT('Ctrl Pts',(-19.3951462353479,-20.9631276565673,
-3.75339088208151));
#76839=CARTESIAN_POINT('Ctrl Pts',(-19.4024879291187,-20.9606992523958,
-3.75385083720906));
#76840=CARTESIAN_POINT('Ctrl Pts',(-19.4226688931911,-20.9539011192879,
-3.75511386702412));
#76841=CARTESIAN_POINT('Ctrl Pts',(-19.4354798738525,-20.9494481057738,
-3.75591418571056));
#76842=CARTESIAN_POINT('Ctrl Pts',(-19.5138716712433,-20.9213524067101,
-3.76080383739638));
#76843=CARTESIAN_POINT('Ctrl Pts',(-19.5782981884462,-20.8946041161553,
-3.76478762826629));
#76844=CARTESIAN_POINT('Ctrl Pts',(-19.7647122572798,-20.8061793341797,
-3.7763465812836));
#76845=CARTESIAN_POINT('Ctrl Pts',(-19.8821740152948,-20.7358290647983,
-3.78365452961412));
#76846=CARTESIAN_POINT('Ctrl Pts',(-20.0762780510362,-20.5924110088189,
-3.79684035205429));
#76847=CARTESIAN_POINT('Ctrl Pts',(-20.1557687662013,-20.5240134439716,
-3.80264508842154));
#76848=CARTESIAN_POINT('Ctrl Pts',(-20.2367163588933,-20.4431828791227,
-3.80942238885642));
#76849=CARTESIAN_POINT('Ctrl Pts',(-20.2435237139725,-20.4362914077689,
-3.80999964040408));
#76850=CARTESIAN_POINT('Ctrl Pts',(-20.2535060244761,-20.4260460531825,
-3.81085743565184));
#76851=CARTESIAN_POINT('Ctrl Pts',(-20.2567177954723,-20.42272799652,-3.81113518154812));
#76852=CARTESIAN_POINT('Ctrl Pts',(-20.2623970491556,-20.4168222570494,
-3.81162948880734));
#76853=CARTESIAN_POINT('Ctrl Pts',(-20.2648688595173,-20.4142388038092,
-3.81184570872853));
#76854=CARTESIAN_POINT('Ctrl Pts',(-20.2701515051174,-20.4086894830196,
-3.81231014231393));
#76855=CARTESIAN_POINT('Ctrl Pts',(-20.2729602595526,-20.4057217806305,
-3.81255850261044));
#76856=CARTESIAN_POINT('Ctrl Pts',(-20.2787067622919,-20.3996147637823,
-3.81306952369131));
#76857=CARTESIAN_POINT('Ctrl Pts',(-20.2816435723938,-20.3964745957892,
-3.81333225270047));
#76858=CARTESIAN_POINT('Ctrl Pts',(-20.2951037388432,-20.3819942163683,
-3.81454354142486));
#76859=CARTESIAN_POINT('Ctrl Pts',(-20.3055118358505,-20.3705481521945,
-3.81550032218878));
#76860=CARTESIAN_POINT('Ctrl Pts',(-20.3738183655828,-20.2937552486411,
-3.82190882332335));
#76861=CARTESIAN_POINT('Ctrl Pts',(-20.4277468291377,-20.2250003784039,
-3.82759284987748));
#76862=CARTESIAN_POINT('Ctrl Pts',(-20.5185513242836,-20.0932094601856,
-3.83812777718336));
#76863=CARTESIAN_POINT('Ctrl Pts',(-20.5567150918504,-20.0312091104248,
-3.84295349355964));
#76864=CARTESIAN_POINT('Ctrl Pts',(-20.5939227256405,-19.9631378145699,
-3.84805527367092));
#76865=CARTESIAN_POINT('Ctrl Pts',(-20.596219730547,-19.9589011375566,-3.84837202744986));
#76866=CARTESIAN_POINT('Ctrl Pts',(-20.6464310200096,-19.8655301285701,
-3.85533558745032));
#76867=CARTESIAN_POINT('Ctrl Pts',(-20.6878922366713,-19.7731104590378,
-3.86187259304192));
#76868=CARTESIAN_POINT('Ctrl Pts',(-20.7225805144725,-19.6781105545716,
-3.86819367631211));
#76869=CARTESIAN_POINT('',(-20.8509991606888,-18.9501148891277,-2.8890562790225));
#76870=CARTESIAN_POINT('Ctrl Pts',(-20.7225805821191,-19.6781103693095,
-3.64442446878243));
#76871=CARTESIAN_POINT('Ctrl Pts',(-20.6975861564812,-19.7465619871152,
-3.64005128426942));
#76872=CARTESIAN_POINT('Ctrl Pts',(-20.6690382082784,-19.8137627604839,
-3.63567809975641));
#76873=CARTESIAN_POINT('Ctrl Pts',(-20.6370917484072,-19.8793245371199,
-3.63130491524341));
#76874=CARTESIAN_POINT('Ctrl Pts',(-20.6051516095213,-19.944873341582,-3.62693259601674));
#76875=CARTESIAN_POINT('Ctrl Pts',(-20.5698145058605,-20.0087833599342,
-3.62256027679008));
#76876=CARTESIAN_POINT('Ctrl Pts',(-20.5312826026733,-20.070688627871,-3.61818795756341));
#76877=CARTESIAN_POINT('Ctrl Pts',(-20.4927456129338,-20.1326020678512,
-3.6138150611519));
#76878=CARTESIAN_POINT('Ctrl Pts',(-20.4510132433513,-20.1925098238232,
-3.6094421647404));
#76879=CARTESIAN_POINT('Ctrl Pts',(-20.4063315108142,-20.2500740802966,
-3.60506926832889));
#76880=CARTESIAN_POINT('Ctrl Pts',(-20.3616004942757,-20.3077018302098,
-3.6006915486077));
#76881=CARTESIAN_POINT('Ctrl Pts',(-20.3139139201605,-20.3629805414553,
-3.59631382888651));
#76882=CARTESIAN_POINT('Ctrl Pts',(-20.2635581471404,-20.4156054367611,
-3.59193610916532));
#76883=CARTESIAN_POINT('Ctrl Pts',(-20.2131700667217,-20.4682640952952,
-3.5875555807744));
#76884=CARTESIAN_POINT('Ctrl Pts',(-20.16010973072,-20.5182652193778,-3.58317505238349));
#76885=CARTESIAN_POINT('Ctrl Pts',(-20.1046984520788,-20.5653427265987,
-3.57879452399257));
#76886=CARTESIAN_POINT('Ctrl Pts',(-20.0491943887079,-20.612499063868,-3.57440666052201));
#76887=CARTESIAN_POINT('Ctrl Pts',(-19.9913319107465,-20.6567217240253,
-3.57001879705145));
#76888=CARTESIAN_POINT('Ctrl Pts',(-19.931462615983,-20.6977870097246,-3.56563093358088));
#76889=CARTESIAN_POINT('Ctrl Pts',(-19.9100485962753,-20.7124752207807,
-3.56406148474731));
#76890=CARTESIAN_POINT('Ctrl Pts',(-19.8883780714084,-20.7267599186563,
-3.56249203591374));
#76891=CARTESIAN_POINT('Ctrl Pts',(-19.8664678605235,-20.7406323112595,
-3.56092258708016));
#76892=CARTESIAN_POINT('Ctrl Pts',(-19.8052064921928,-20.7794197860744,
-3.55653437814988));
#76893=CARTESIAN_POINT('Ctrl Pts',(-19.7418305075798,-20.8151319931224,
-3.55214616921959));
#76894=CARTESIAN_POINT('Ctrl Pts',(-19.6766813842659,-20.8475318007774,
-3.54775796028931));
#76895=CARTESIAN_POINT('Ctrl Pts',(-19.611628953053,-20.8798835217459,-3.54337626418866));
#76896=CARTESIAN_POINT('Ctrl Pts',(-19.5448090356316,-20.908932389527,-3.53899456808801));
#76897=CARTESIAN_POINT('Ctrl Pts',(-19.4765908557835,-20.93448526373,-3.53461287198737));
#76898=CARTESIAN_POINT('Ctrl Pts',(-19.4084528377259,-20.9600081112722,
-3.53023632472836));
#76899=CARTESIAN_POINT('Ctrl Pts',(-19.3389202706952,-20.982042957579,-3.52585977746935));
#76900=CARTESIAN_POINT('Ctrl Pts',(-19.2683841301347,-21.0004439463798,
-3.52148323021034));
#76901=CARTESIAN_POINT('Ctrl Pts',(-19.1978927225695,-21.018833265541,-3.517109458494));
#76902=CARTESIAN_POINT('Ctrl Pts',(-19.1263994698856,-21.033593178237,-3.51273568677766));
#76903=CARTESIAN_POINT('Ctrl Pts',(-19.054311001005,-21.0446275021215,-3.50836191506133));
#76904=CARTESIAN_POINT('Ctrl Pts',(-18.9822444688877,-21.0556584682242,
-3.50398947429841));
#76905=CARTESIAN_POINT('Ctrl Pts',(-18.9095835567029,-21.0629660233357,
-3.4996170335355));
#76906=CARTESIAN_POINT('Ctrl Pts',(-18.8367439345943,-21.0665053047709,
-3.49524459277259));
#76907=CARTESIAN_POINT('Ctrl Pts',(-18.7639024499686,-21.0700446767059,
-3.49087204020588));
#76908=CARTESIAN_POINT('Ctrl Pts',(-18.6908827282527,-21.0698155622467,
-3.48649948763918));
#76909=CARTESIAN_POINT('Ctrl Pts',(-18.6181027067733,-21.0658251624538,
-3.48212693507248));
#76910=CARTESIAN_POINT('Ctrl Pts',(-18.5452471514426,-21.0618306212735,
-3.47774984450579));
#76911=CARTESIAN_POINT('Ctrl Pts',(-18.4726322757191,-21.0540670274163,
-3.47337275393911));
#76912=CARTESIAN_POINT('Ctrl Pts',(-18.4006723159509,-21.0425936130789,
-3.46899566337243));
#76913=CARTESIAN_POINT('Ctrl Pts',(-18.3286730561778,-21.0311139326842,
-3.46461618231413));
#76914=CARTESIAN_POINT('Ctrl Pts',(-18.2573298966098,-21.0159204984676,
-3.46023670125583));
#76915=CARTESIAN_POINT('Ctrl Pts',(-18.1870456019981,-20.997123440408,-3.45585722019753));
#76916=CARTESIAN_POINT('Ctrl Pts',(-18.1166367289457,-20.9782930646892,
-3.45146997653845));
#76917=CARTESIAN_POINT('Ctrl Pts',(-18.0472909281431,-20.9558464584345,
-3.44708273287937));
#76918=CARTESIAN_POINT('Ctrl Pts',(-17.9793940004957,-20.9299430693304,
-3.44269548922029));
#76919=CARTESIAN_POINT('Ctrl Pts',(-17.9332306321329,-20.912331260748,-3.43971258627977));
#76920=CARTESIAN_POINT('Ctrl Pts',(-17.8877366290251,-20.8931225055476,
-3.43672968333925));
#76921=CARTESIAN_POINT('Ctrl Pts',(-17.8430266573744,-20.8723789997629,
-3.43374678039873));
#76922=CARTESIAN_POINT('Ctrl Pts',(-17.7772529124841,-20.841862808246,-3.42935857146461));
#76923=CARTESIAN_POINT('Ctrl Pts',(-17.7129203794316,-20.8079039749603,
-3.42497036253048));
#76924=CARTESIAN_POINT('Ctrl Pts',(-17.6504132837259,-20.770661273661,-3.42058215359636));
#76925=CARTESIAN_POINT('Ctrl Pts',(-17.5879989589138,-20.7334738467052,
-3.41620045749186));
#76926=CARTESIAN_POINT('Ctrl Pts',(-17.5274051041874,-20.6930124717674,
-3.41181876138736));
#76927=CARTESIAN_POINT('Ctrl Pts',(-17.4689939738807,-20.6494830643873,
-3.40743706528285));
#76928=CARTESIAN_POINT('Ctrl Pts',(-17.4106514813006,-20.6060048075252,
-3.40306051801998));
#76929=CARTESIAN_POINT('Ctrl Pts',(-17.3544870028669,-20.5594659667512,
-3.39868397075711));
#76930=CARTESIAN_POINT('Ctrl Pts',(-17.300834808213,-20.5101163413077,-3.39430742349424));
#76931=CARTESIAN_POINT('Ctrl Pts',(-17.2472166390012,-20.4607980126794,
-3.38993365177404));
#76932=CARTESIAN_POINT('Ctrl Pts',(-17.1961079465045,-20.4086727619658,
-3.38555988005384));
#76933=CARTESIAN_POINT('Ctrl Pts',(-17.1478097053784,-20.3540304380606,
-3.38118610833364));
#76934=CARTESIAN_POINT('Ctrl Pts',(-17.0995261615695,-20.2994047419982,
-3.37681366756687));
#76935=CARTESIAN_POINT('Ctrl Pts',(-17.0540516905098,-20.2422638546093,
-3.3724412268001));
#76936=CARTESIAN_POINT('Ctrl Pts',(-17.011649008983,-20.1829330053837,-3.36806878603333));
#76937=CARTESIAN_POINT('Ctrl Pts',(-16.9692452432152,-20.1236006390618,
-3.36369623346278));
#76938=CARTESIAN_POINT('Ctrl Pts',(-16.9299137017783,-20.0620785933411,
-3.35932368089223));
#76939=CARTESIAN_POINT('Ctrl Pts',(-16.8938745512684,-19.9987221851716,
-3.35495112832168));
#76940=CARTESIAN_POINT('Ctrl Pts',(-16.8577979979692,-19.9353000233327,
-3.35057403775118));
#76941=CARTESIAN_POINT('Ctrl Pts',(-16.8250208968183,-19.870040118225,-3.34619694718069));
#76942=CARTESIAN_POINT('Ctrl Pts',(-16.7957176611905,-19.8033228383283,
-3.3418198566102));
#76943=CARTESIAN_POINT('Ctrl Pts',(-16.7663984219784,-19.7365691216491,
-3.33744037554812));
#76944=CARTESIAN_POINT('Ctrl Pts',(-16.7405569966193,-19.6683568969041,
-3.33306089448603));
#76945=CARTESIAN_POINT('Ctrl Pts',(-16.7183187921505,-19.5990844367796,
-3.32868141342394));
#76946=CARTESIAN_POINT('Ctrl Pts',(-16.696041170614,-19.5296891916857,-3.32429416976114));
#76947=CARTESIAN_POINT('Ctrl Pts',(-16.6773796475294,-19.4592304251164,
-3.31990692609834));
#76948=CARTESIAN_POINT('Ctrl Pts',(-16.6624089793388,-19.3881188405882,
-3.31551968243554));
#76949=CARTESIAN_POINT('Ctrl Pts',(-16.6522303676446,-19.3397698159047,
-3.31253677952946));
#76950=CARTESIAN_POINT('Ctrl Pts',(-16.6437568500116,-19.2911192245629,
-3.30955387662337));
#76951=CARTESIAN_POINT('Ctrl Pts',(-16.6369981960583,-19.2422971482212,
-3.30657097371729));
#76952=CARTESIAN_POINT('Ctrl Pts',(-16.6270554032346,-19.1704740021266,
-3.30218276479085));
#76953=CARTESIAN_POINT('Ctrl Pts',(-16.6207874279489,-19.0979992504155,
-3.29779455586441));
#76954=CARTESIAN_POINT('Ctrl Pts',(-16.6182687405808,-19.0252819071572,
-3.29340634693797));
#76955=CARTESIAN_POINT('Ctrl Pts',(-16.6157537913624,-18.9526724884929,
-3.28902465084115));
#76956=CARTESIAN_POINT('Ctrl Pts',(-16.6169771002007,-18.8798216711257,
-3.28464295474433));
#76957=CARTESIAN_POINT('Ctrl Pts',(-16.6219616061142,-18.8071455117975,
-3.2802612586475));
#76958=CARTESIAN_POINT('Ctrl Pts',(-16.6269402548367,-18.7345547527397,
-3.27588471139227));
#76959=CARTESIAN_POINT('Ctrl Pts',(-16.6356712880177,-18.6621387228747,
-3.27150816413703));
#76960=CARTESIAN_POINT('Ctrl Pts',(-16.6481255978391,-18.590313701656,-3.2671316168818));
#76961=CARTESIAN_POINT('Ctrl Pts',(-16.6605720093183,-18.5185342308214,
-3.2627578451692));
#76962=CARTESIAN_POINT('Ctrl Pts',(-16.6767369302051,-18.4473454990794,
-3.2583840734566));
#76963=CARTESIAN_POINT('Ctrl Pts',(-16.6965395553225,-18.3771574681928,
-3.254010301744));
#76964=CARTESIAN_POINT('Ctrl Pts',(-16.7163361544347,-18.3069907957591,
-3.24963786098479));
#76965=CARTESIAN_POINT('Ctrl Pts',(-16.7397681292052,-18.2378246835963,
-3.24526542022559));
#76966=CARTESIAN_POINT('Ctrl Pts',(-16.7667042167146,-18.1700560754968,
-3.24089297946638));
#76967=CARTESIAN_POINT('Ctrl Pts',(-16.793640992983,-18.1022857345459,-3.23652042690334));
#76968=CARTESIAN_POINT('Ctrl Pts',(-16.8240818798525,-18.0359134161329,
-3.23214787434029));
#76969=CARTESIAN_POINT('Ctrl Pts',(-16.8578472840016,-17.971316571848,-3.22777532177725));
#76970=CARTESIAN_POINT('Ctrl Pts',(-16.8916477311615,-17.9066526865202,
-3.22339823121414));
#76971=CARTESIAN_POINT('Ctrl Pts',(-16.9287793604406,-17.8437683827164,
-3.21902114065103));
#76972=CARTESIAN_POINT('Ctrl Pts',(-16.9690167487947,-17.7830162007262,
-3.21464405008791));
#76973=CARTESIAN_POINT('Ctrl Pts',(-17.0092761122804,-17.7222308397138,
-3.21026456903314));
#76974=CARTESIAN_POINT('Ctrl Pts',(-17.0526443249034,-17.6635803070146,
-3.20588508797837));
#76975=CARTESIAN_POINT('Ctrl Pts',(-17.0988543828141,-17.6073856275506,
-3.2015056069236));
#76976=CARTESIAN_POINT('Ctrl Pts',(-17.1451463477434,-17.5510913433929,
-3.19711836326793));
#76977=CARTESIAN_POINT('Ctrl Pts',(-17.194289891427,-17.4972619617608,-3.19273111961227));
#76978=CARTESIAN_POINT('Ctrl Pts',(-17.2459801414474,-17.4461826470143,
-3.1883438759566));
#76979=CARTESIAN_POINT('Ctrl Pts',(-17.2811245310897,-17.4114536344943,
-3.18536097298302));
#76980=CARTESIAN_POINT('Ctrl Pts',(-17.3174454256972,-17.3779951039873,
-3.18237807000944));
#76981=CARTESIAN_POINT('Ctrl Pts',(-17.3548387352824,-17.345885680936,-3.17939516703586));
#76982=CARTESIAN_POINT('Ctrl Pts',(-17.4098487897263,-17.2986488589,-3.17500695810765));
#76983=CARTESIAN_POINT('Ctrl Pts',(-17.4673958504111,-17.2541492751002,
-3.17061874917943));
#76984=CARTESIAN_POINT('Ctrl Pts',(-17.5271763106365,-17.2126709388989,
-3.16623054025122));
#76985=CARTESIAN_POINT('Ctrl Pts',(-17.5868680467463,-17.1712541634263,
-3.16184884415269));
#76986=CARTESIAN_POINT('Ctrl Pts',(-17.6487862091489,-17.1328500068486,
-3.15746714805417));
#76987=CARTESIAN_POINT('Ctrl Pts',(-17.7125933764223,-17.0977029608739,
-3.15308545195564));
#76988=CARTESIAN_POINT('Ctrl Pts',(-17.7763255651952,-17.062597215476,-3.14870890469881));
#76989=CARTESIAN_POINT('Ctrl Pts',(-17.8419419289074,-17.0307412091789,
-3.14433235744198));
#76990=CARTESIAN_POINT('Ctrl Pts',(-17.9090766869066,-17.0023357910874,
-3.13995581018516));
#76991=CARTESIAN_POINT('Ctrl Pts',(-17.9761688690172,-16.9739483872994,
-3.13558203847104));
#76992=CARTESIAN_POINT('Ctrl Pts',(-18.044777091654,-16.9490074173241,-3.13120826675692));
#76993=CARTESIAN_POINT('Ctrl Pts',(-18.1145129035424,-16.9276668413222,
-3.1268344950428));
#76994=CARTESIAN_POINT('Ctrl Pts',(-18.1842274945885,-16.9063327593294,
-3.12246205428213));
#76995=CARTESIAN_POINT('Ctrl Pts',(-18.2550685326835,-16.8885970372536,
-3.11808961352147));
#76996=CARTESIAN_POINT('Ctrl Pts',(-18.3266312007869,-16.8745641618987,
-3.11371717276081));
#76997=CARTESIAN_POINT('Ctrl Pts',(-18.3981956987552,-16.8605309277218,
-3.10934462019639));
#76998=CARTESIAN_POINT('Ctrl Pts',(-18.4704813896195,-16.8502008191088,
-3.10497206763197));
#76999=CARTESIAN_POINT('Ctrl Pts',(-18.543073685867,-16.8436271338846,-3.10059951506755));
#77000=CARTESIAN_POINT('Ctrl Pts',(-18.6157413211371,-16.837046626242,-3.09622242450318));
#77001=CARTESIAN_POINT('Ctrl Pts',(-18.6887157156715,-16.8342303693191,
-3.09184533393881));
#77002=CARTESIAN_POINT('Ctrl Pts',(-18.7615784216589,-16.8351796413822,
-3.08746824337444));
#77003=CARTESIAN_POINT('Ctrl Pts',(-18.8344809206741,-16.8361294318779,
-3.08308876231848));
#77004=CARTESIAN_POINT('Ctrl Pts',(-18.9072711279966,-16.8408488145899,
-3.07870928126251));
#77005=CARTESIAN_POINT('Ctrl Pts',(-18.9795345883502,-16.8492870462368,
-3.07432980020655));
#77006=CARTESIAN_POINT('Ctrl Pts',(-19.0519261352023,-16.8577402345926,
-3.06994255654981));
#77007=CARTESIAN_POINT('Ctrl Pts',(-19.1237885946052,-16.8699253543973,
-3.06555531289307));
#77008=CARTESIAN_POINT('Ctrl Pts',(-19.194717166803,-16.885740410255,-3.06116806923633));
#77009=CARTESIAN_POINT('Ctrl Pts',(-19.2429417616867,-16.8964931244035,
-3.05818516627569));
#77010=CARTESIAN_POINT('Ctrl Pts',(-19.2907349020831,-16.9089227808444,
-3.05520226331506));
#77011=CARTESIAN_POINT('Ctrl Pts',(-19.3379741345032,-16.9229844148329,
-3.05221936035442));
#77012=CARTESIAN_POINT('Ctrl Pts',(-19.4074687259721,-16.9436707693596,
-3.04783115140139));
#77013=CARTESIAN_POINT('Ctrl Pts',(-19.4760349665996,-16.9679719598249,
-3.04344294244835));
#77014=CARTESIAN_POINT('Ctrl Pts',(-19.5432697129059,-16.995786429918,-3.03905473349532));
#77015=CARTESIAN_POINT('Ctrl Pts',(-19.6104046717026,-17.0235596187263,
-3.03467303737184));
#77016=CARTESIAN_POINT('Ctrl Pts',(-19.6762116170654,-17.054835553211,-3.03029134124837));
#77017=CARTESIAN_POINT('Ctrl Pts',(-19.7403023303408,-17.0894628540749,
-3.02590964512489));
#77018=CARTESIAN_POINT('Ctrl Pts',(-19.8043177319278,-17.1240494651048,
-3.02153309784305));
#77019=CARTESIAN_POINT('Ctrl Pts',(-19.8666204853438,-17.1619793912516,
-3.0171565505612));
#77020=CARTESIAN_POINT('Ctrl Pts',(-19.9268437181447,-17.2030537846799,
-3.01278000327936));
#77021=CARTESIAN_POINT('Ctrl Pts',(-19.9870287582467,-17.2441021293248,
-3.00840623154019));
#77022=CARTESIAN_POINT('Ctrl Pts',(-20.0451364968745,-17.2882907134169,
-3.00403245980103));
#77023=CARTESIAN_POINT('Ctrl Pts',(-20.100827216588,-17.3353762466194,-2.99965868806186));
#77024=CARTESIAN_POINT('Ctrl Pts',(-20.156500989428,-17.3824474515356,-2.99528624727616));
#77025=CARTESIAN_POINT('Ctrl Pts',(-20.2097588354208,-17.4324135441543,
-2.99091380649046));
#77026=CARTESIAN_POINT('Ctrl Pts',(-20.2602937779114,-17.48499069413,-2.98654136570476));
#77027=CARTESIAN_POINT('Ctrl Pts',(-20.3108300125851,-17.5375691885083,
-2.98216881311535));
#77028=CARTESIAN_POINT('Ctrl Pts',(-20.3586428726932,-17.5927585236335,
-2.97779626052593));
#77029=CARTESIAN_POINT('Ctrl Pts',(-20.40346313484,-17.6502389461156,-2.97342370793652));
#77030=CARTESIAN_POINT('Ctrl Pts',(-20.4483299131425,-17.7077790239444,
-2.96904661734739));
#77031=CARTESIAN_POINT('Ctrl Pts',(-20.4901975952304,-17.7676145553053,
-2.96466952675826));
#77032=CARTESIAN_POINT('Ctrl Pts',(-20.5288386084183,-17.8293943837077,
-2.96029243616913));
#77033=CARTESIAN_POINT('Ctrl Pts',(-20.5675007248966,-17.8912079523656,
-2.9559129550885));
#77034=CARTESIAN_POINT('Ctrl Pts',(-20.6029324294701,-17.9549675102643,
-2.95153347400787));
#77035=CARTESIAN_POINT('Ctrl Pts',(-20.6349520524258,-18.0202970997264,
-2.94715399292724));
#77036=CARTESIAN_POINT('Ctrl Pts',(-20.6670284299448,-18.0857424854403,
-2.94276674924626));
#77037=CARTESIAN_POINT('Ctrl Pts',(-20.695680458665,-18.1527630160604,-2.93837950556528));
#77038=CARTESIAN_POINT('Ctrl Pts',(-20.7207747901411,-18.2209631108763,
-2.9339922618843));
#77039=CARTESIAN_POINT('Ctrl Pts',(-20.7378365162473,-18.2673326003074,
-2.9310093591472));
#77040=CARTESIAN_POINT('Ctrl Pts',(-20.7532546613818,-18.3142470017661,
-2.92802645641009));
#77041=CARTESIAN_POINT('Ctrl Pts',(-20.767000752034,-18.3615790127128,-2.92504355367299));
#77042=CARTESIAN_POINT('Ctrl Pts',(-20.7921933233422,-18.4483247712785,
-2.91957676374621));
#77043=CARTESIAN_POINT('Ctrl Pts',(-20.8118478930265,-18.5367464915126,
-2.91410997381944));
#77044=CARTESIAN_POINT('Ctrl Pts',(-20.8257819138148,-18.6262126076147,
-2.90864318389266));
#77045=CARTESIAN_POINT('Ctrl Pts',(-20.8394880731057,-18.7142156942372,
-2.90326579177559));
#77046=CARTESIAN_POINT('Ctrl Pts',(-20.8476592207529,-18.8032293912446,
-2.89788839965851));
#77047=CARTESIAN_POINT('Ctrl Pts',(-20.8501673751625,-18.8926313188794,
-2.89251100754144));
#77048=CARTESIAN_POINT('Ctrl Pts',(-20.8507044999979,-18.911776868886,-2.89135943136846));
#77049=CARTESIAN_POINT('Ctrl Pts',(-20.8509820862726,-18.9309401417771,
-2.89020785519548));
#77050=CARTESIAN_POINT('Ctrl Pts',(-20.8509991606888,-18.9501148891277,
-2.8890562790225));
#77051=CARTESIAN_POINT('Ctrl Pts',(-20.849962012661,-18.9501158126703,-2.8890562790225));
#77052=CARTESIAN_POINT('Ctrl Pts',(-20.8478498624177,-19.1969462894927,
-2.87422526082294));
#77053=CARTESIAN_POINT('Ctrl Pts',(-20.8034779929369,-19.4444419793215,
-2.85939424262338));
#77054=CARTESIAN_POINT('Ctrl Pts',(-20.7202230519095,-19.6772708889146,
-2.84456322442383));
#77055=CARTESIAN_POINT('Origin',(-18.734,-18.952,0.));
#77056=CARTESIAN_POINT('',(-20.7225805826894,-19.6781103677477,-2.04625070052543));
#77057=CARTESIAN_POINT('',(-20.7225805820961,-19.6781103693727,-2.26547392846891));
#77058=CARTESIAN_POINT('',(-20.7225805821191,-19.6781103693095,0.));
#77059=CARTESIAN_POINT('',(-20.8509992561133,-18.9537747157296,-2.31031853654595));
#77060=CARTESIAN_POINT('Ctrl Pts',(-20.7225805820961,-19.6781103693727,
-2.26547392846891));
#77061=CARTESIAN_POINT('Ctrl Pts',(-20.7575267620676,-19.5824041271247,
-2.2710458239064));
#77062=CARTESIAN_POINT('Ctrl Pts',(-20.7855141340195,-19.4843107263304,
-2.27670326525148));
#77063=CARTESIAN_POINT('Ctrl Pts',(-20.8083091787163,-19.3751126538042,
-2.2833121262572));
#77064=CARTESIAN_POINT('Ctrl Pts',(-20.8102239943213,-19.3656143180092,
-2.28388953700015));
#77065=CARTESIAN_POINT('Ctrl Pts',(-20.8129550917444,-19.3515698395547,
-2.2847475243896));
#77066=CARTESIAN_POINT('Ctrl Pts',(-20.8138218385678,-19.3470334784062,
-2.28502530142322));
#77067=CARTESIAN_POINT('Ctrl Pts',(-20.8153332698376,-19.3389801091439,
-2.28551964303392));
#77068=CARTESIAN_POINT('Ctrl Pts',(-20.8159838956222,-19.3354642658266,
-2.2857358659928));
#77069=CARTESIAN_POINT('Ctrl Pts',(-20.8173589190641,-19.3279272645982,
-2.2862002822975));
#77070=CARTESIAN_POINT('Ctrl Pts',(-20.8180805726934,-19.3239057135641,
-2.28644862215127));
#77071=CARTESIAN_POINT('Ctrl Pts',(-20.819537639316,-19.3156485071271,-2.28695959356709));
#77072=CARTESIAN_POINT('Ctrl Pts',(-20.8202718006576,-19.3114126525071,
-2.28722229330262));
#77073=CARTESIAN_POINT('Ctrl Pts',(-20.8220971202441,-19.3006871419385,
-2.28788887808368));
#77074=CARTESIAN_POINT('Ctrl Pts',(-20.823170921096,-19.2941946323735,-2.28829368782551));
#77075=CARTESIAN_POINT('Ctrl Pts',(-20.8419517333718,-19.1772561807361,
-2.29560698829358));
#77076=CARTESIAN_POINT('Ctrl Pts',(-20.8509055123085,-19.0655985766051,
-2.30293678580813));
#77077=CARTESIAN_POINT('Ctrl Pts',(-20.8509992561133,-18.9537747157296,
-2.31031853654595));
#77078=CARTESIAN_POINT('Ctrl Pts',(-20.8509992546724,-18.9537764337049,
-2.31031842313845));
#77079=CARTESIAN_POINT('Ctrl Pts',(-20.8510843034766,-18.8524226625882,
-2.31700901865283));
#77080=CARTESIAN_POINT('Ctrl Pts',(-20.8438905426111,-18.7511845230255,
-2.32372474899395));
#77081=CARTESIAN_POINT('Ctrl Pts',(-20.8169301667289,-18.563591183208,-2.33599520132961));
#77082=CARTESIAN_POINT('Ctrl Pts',(-20.7989516822577,-18.4771974729164,
-2.34157662375898));
#77083=CARTESIAN_POINT('Ctrl Pts',(-20.7702116745163,-18.3723866086643,
-2.34824632884448));
#77084=CARTESIAN_POINT('Ctrl Pts',(-20.7645005235169,-18.3526859443344,
-2.34949575392107));
#77085=CARTESIAN_POINT('Ctrl Pts',(-20.75591384801,-18.3245991161562,-2.35127147777804));
#77086=CARTESIAN_POINT('Ctrl Pts',(-20.7532707044411,-18.3161436453596,
-2.35180533073409));
#77087=CARTESIAN_POINT('Ctrl Pts',(-20.7485964764223,-18.3015138128981,
-2.3527278285672));
#77088=CARTESIAN_POINT('Ctrl Pts',(-20.7465899039902,-18.2953318020169,
-2.3531172723558));
#77089=CARTESIAN_POINT('Ctrl Pts',(-20.7426769449974,-18.2834628625813,
-2.35386429785767));
#77090=CARTESIAN_POINT('Ctrl Pts',(-20.7407748004187,-18.2777746111156,
-2.35422201494289));
#77091=CARTESIAN_POINT('Ctrl Pts',(-20.7357282855469,-18.2628938705469,
-2.35515707901907));
#77092=CARTESIAN_POINT('Ctrl Pts',(-20.7325447424454,-18.2537147402154,
-2.3557331260957));
#77093=CARTESIAN_POINT('Ctrl Pts',(-20.7212756715466,-18.2219310080391,
-2.35772543262704));
#77094=CARTESIAN_POINT('Ctrl Pts',(-20.712868733493,-18.1994417414467,-2.35913101792212));
#77095=CARTESIAN_POINT('Ctrl Pts',(-20.6489791070301,-18.0370108868283,
-2.36926326534927));
#77096=CARTESIAN_POINT('Ctrl Pts',(-20.579092299269,-17.9031953293941,-2.37746165698123));
#77097=CARTESIAN_POINT('Ctrl Pts',(-20.4589031767015,-17.7228643216449,
-2.38923025126843));
#77098=CARTESIAN_POINT('Ctrl Pts',(-20.419654497017,-17.6695671941733,-2.39281850192715));
#77099=CARTESIAN_POINT('Ctrl Pts',(-20.3433815131489,-17.5755570867321,
-2.39950740498086));
#77100=CARTESIAN_POINT('Ctrl Pts',(-20.3071431999893,-17.5342822619525,
-2.40258503118372));
#77101=CARTESIAN_POINT('Ctrl Pts',(-20.2498839317676,-17.4739662245475,
-2.40738294988533));
#77102=CARTESIAN_POINT('Ctrl Pts',(-20.2300158975193,-17.4538597547527,
-2.40903691680933));
#77103=CARTESIAN_POINT('Ctrl Pts',(-20.204871379837,-17.4294124884789,-2.41112625537063));
#77104=CARTESIAN_POINT('Ctrl Pts',(-20.1999675447591,-17.4246904370405,
-2.41153355304756));
#77105=CARTESIAN_POINT('Ctrl Pts',(-20.1920749587726,-17.4171634568076,
-2.41218897213734));
#77106=CARTESIAN_POINT('Ctrl Pts',(-20.189100642402,-17.4143433674762,-2.41243594049324));
#77107=CARTESIAN_POINT('Ctrl Pts',(-20.183517820333,-17.4090807347955,-2.41289949705779));
#77108=CARTESIAN_POINT('Ctrl Pts',(-20.1809113134251,-17.4066361526108,
-2.41311592397766));
#77109=CARTESIAN_POINT('Ctrl Pts',(-20.1749367418387,-17.4010611070537,
-2.41361200686093));
#77110=CARTESIAN_POINT('Ctrl Pts',(-20.1715646701594,-17.3979350200772,
-2.41389199041614));
#77111=CARTESIAN_POINT('Ctrl Pts',(-20.1611317026697,-17.3883261251821,
-2.4147581416011));
#77112=CARTESIAN_POINT('Ctrl Pts',(-20.1540370547588,-17.3818803743891,
-2.41534700356176));
#77113=CARTESIAN_POINT('Ctrl Pts',(-20.0609538422547,-17.2984577440783,
-2.42306828895633));
#77114=CARTESIAN_POINT('Ctrl Pts',(-19.9688635983804,-17.2285980909303,
-2.43064533735236));
#77115=CARTESIAN_POINT('Ctrl Pts',(-19.7568270044209,-17.093500790107,-2.44724911310532));
#77116=CARTESIAN_POINT('Ctrl Pts',(-19.6353076822509,-17.0316232020963,
-2.45624208495786));
#77117=CARTESIAN_POINT('Ctrl Pts',(-19.4515627171354,-16.9593736994179,
-2.46876543184455));
#77118=CARTESIAN_POINT('Ctrl Pts',(-19.3934914252173,-16.9394076171203,
-2.47258367441128));
#77119=CARTESIAN_POINT('Ctrl Pts',(-19.3220865375304,-16.9182806677852,
-2.47711488452111));
#77120=CARTESIAN_POINT('Ctrl Pts',(-19.3095092614356,-16.9146857876376,
-2.47790702471601));
#77121=CARTESIAN_POINT('Ctrl Pts',(-19.2897662094287,-16.9092401825917,
-2.47914131244906));
#77122=CARTESIAN_POINT('Ctrl Pts',(-19.2826228345554,-16.907310111843,-2.47958603105056));
#77123=CARTESIAN_POINT('Ctrl Pts',(-19.2699384595304,-16.9039541752115,
-2.48037244931891));
#77124=CARTESIAN_POINT('Ctrl Pts',(-19.2644015525042,-16.9025132528038,
-2.48071463394917));
#77125=CARTESIAN_POINT('Ctrl Pts',(-19.2516307390168,-16.8992450012206,
-2.48150138269828));
#77126=CARTESIAN_POINT('Ctrl Pts',(-19.2443928501979,-16.8974334258437,
-2.48194543380327));
#77127=CARTESIAN_POINT('Ctrl Pts',(-19.2245130458354,-16.8925692331332,
-2.4831601256031));
#77128=CARTESIAN_POINT('Ctrl Pts',(-19.2118522090242,-16.889594751431,-2.48392824569442));
#77129=CARTESIAN_POINT('Ctrl Pts',(-19.1470884397097,-16.8750078389006,
-2.48783049991296));
#77130=CARTESIAN_POINT('Ctrl Pts',(-19.0945845827141,-16.8652518239961,
-2.49090477702753));
#77131=CARTESIAN_POINT('Ctrl Pts',(-19.0090766668656,-16.8526873990585,
-2.49579929498177));
#77132=CARTESIAN_POINT('Ctrl Pts',(-18.976279893557,-16.8486500167908,-2.49765037755845));
#77133=CARTESIAN_POINT('Ctrl Pts',(-18.7852284832504,-16.8296592150614,
-2.50831766663554));
#77134=CARTESIAN_POINT('Ctrl Pts',(-18.6257996033672,-16.8318011326506,
-2.51671730677738));
#77135=CARTESIAN_POINT('Ctrl Pts',(-18.4217059616401,-16.8576384862318,
-2.5281621761271));
#77136=CARTESIAN_POINT('Ctrl Pts',(-18.3755031033387,-16.8650507602765,
-2.53080323672204));
#77137=CARTESIAN_POINT('Ctrl Pts',(-18.3129815181106,-16.8772184166345,
-2.5344906560672));
#77138=CARTESIAN_POINT('Ctrl Pts',(-18.2964160470553,-16.8806488882883,
-2.53547864972362));
#77139=CARTESIAN_POINT('Ctrl Pts',(-18.2681428715129,-16.886858144027,-2.53718650104151));
#77140=CARTESIAN_POINT('Ctrl Pts',(-18.2564142548678,-16.8895389481557,
-2.53790137165594));
#77141=CARTESIAN_POINT('Ctrl Pts',(-18.2398024748614,-16.8934851850898,
-2.53892379564829));
#77142=CARTESIAN_POINT('Ctrl Pts',(-18.2348997548702,-16.8946683832762,
-2.53922677982418));
#77143=CARTESIAN_POINT('Ctrl Pts',(-18.2264687918622,-16.8967349801915,
-2.53975000037692));
#77144=CARTESIAN_POINT('Ctrl Pts',(-18.2229384733949,-16.8976099823181,
-2.53996975392649));
#77145=CARTESIAN_POINT('Ctrl Pts',(-18.2161063943996,-16.8993220380594,
-2.54039634791947));
#77146=CARTESIAN_POINT('Ctrl Pts',(-18.2128043905838,-16.9001579645345,
-2.54060311726895));
#77147=CARTESIAN_POINT('Ctrl Pts',(-18.2039189563164,-16.9024302097678,
-2.54116108719151));
#77148=CARTESIAN_POINT('Ctrl Pts',(-18.1983393998172,-16.9038813614615,
-2.5415131323691));
#77149=CARTESIAN_POINT('Ctrl Pts',(-18.1777566817011,-16.9093244500454,
-2.542817808868));
#77150=CARTESIAN_POINT('Ctrl Pts',(-18.1627920600465,-16.9134584898482,
-2.54377816205421));
#77151=CARTESIAN_POINT('Ctrl Pts',(-18.014865766124,-16.9560803968292,-2.55337931936512));
#77152=CARTESIAN_POINT('Ctrl Pts',(-17.8859477015773,-17.0073534823636,
-2.56259251617903));
#77153=CARTESIAN_POINT('Ctrl Pts',(-17.6236863361639,-17.1427291877668,
-2.58207676758641));
#77154=CARTESIAN_POINT('Ctrl Pts',(-17.4927956980432,-17.229883024082,-2.59224665750888));
#77155=CARTESIAN_POINT('Ctrl Pts',(-17.3584531866092,-17.342681320773,-2.60299063285758));
#77156=CARTESIAN_POINT('Ctrl Pts',(-17.3443525729114,-17.3548413634553,
-2.60412330254172));
#77157=CARTESIAN_POINT('Ctrl Pts',(-17.3240360895543,-17.3728346027039,
-2.60576305051107));
#77158=CARTESIAN_POINT('Ctrl Pts',(-17.3176924123458,-17.3785215599685,
-2.60627618129264));
#77159=CARTESIAN_POINT('Ctrl Pts',(-17.3066111321943,-17.3885769787169,
-2.60717459364726));
#77160=CARTESIAN_POINT('Ctrl Pts',(-17.3018588554306,-17.3929290372567,
-2.607560559442));
#77161=CARTESIAN_POINT('Ctrl Pts',(-17.2926555280229,-17.4014348846445,
-2.608309382641));
#77162=CARTESIAN_POINT('Ctrl Pts',(-17.2882023832658,-17.4055863048676,
-2.60867233520964));
#77163=CARTESIAN_POINT('Ctrl Pts',(-17.2775771800516,-17.4155776081885,
-2.60953988495517));
#77164=CARTESIAN_POINT('Ctrl Pts',(-17.271422219591,-17.4214355825454,-2.61004369956364));
#77165=CARTESIAN_POINT('Ctrl Pts',(-17.2492045896015,-17.4428375816475,
-2.61186711747284));
#77166=CARTESIAN_POINT('Ctrl Pts',(-17.2333527291824,-17.4585990356322,
-2.61317725984456));
#77167=CARTESIAN_POINT('Ctrl Pts',(-17.0899891072817,-17.6057331846057,
-2.62512213612595));
#77168=CARTESIAN_POINT('Ctrl Pts',(-16.9797754269409,-17.7528717634576,
-2.63492742701779));
#77169=CARTESIAN_POINT('Ctrl Pts',(-16.8496864969737,-17.9836282922652,
-2.6493606634437));
#77170=CARTESIAN_POINT('Ctrl Pts',(-16.8136801494142,-18.0571532449666,
-2.65385439815567));
#77171=CARTESIAN_POINT('Ctrl Pts',(-16.76790205596,-18.1662021164378,-2.66061627690045));
#77172=CARTESIAN_POINT('Ctrl Pts',(-16.7546560641544,-18.2001910733189,
-2.66273718358911));
#77173=CARTESIAN_POINT('Ctrl Pts',(-16.7397559652177,-18.2415523418886,
-2.66535332811062));
#77174=CARTESIAN_POINT('Ctrl Pts',(-16.7372539102181,-18.2486151876004,
-2.66580128276438));
#77175=CARTESIAN_POINT('Ctrl Pts',(-16.7334194712451,-18.2596244541528,
-2.66650165103914));
#77176=CARTESIAN_POINT('Ctrl Pts',(-16.7320611220711,-18.2635618569029,
-2.66675255321516));
#77177=CARTESIAN_POINT('Ctrl Pts',(-16.7295616245501,-18.270877022409,-2.66721951788925));
#77178=CARTESIAN_POINT('Ctrl Pts',(-16.7284173860902,-18.2742536685736,
-2.66743539468765));
#77179=CARTESIAN_POINT('Ctrl Pts',(-16.7258473618599,-18.2819013087203,
-2.66792506252116));
#77180=CARTESIAN_POINT('Ctrl Pts',(-16.7244266766088,-18.2861739482626,
-2.66819914837998));
#77181=CARTESIAN_POINT('Ctrl Pts',(-16.7201749544556,-18.2990983578693,
-2.66902972057012));
#77182=CARTESIAN_POINT('Ctrl Pts',(-16.7173861244278,-18.307763755766,-2.66958859654811));
#77183=CARTESIAN_POINT('Ctrl Pts',(-16.6964027866544,-18.3744342186201,
-2.67390241390562));
#77184=CARTESIAN_POINT('Ctrl Pts',(-16.6806602016957,-18.433175512017,-2.67778311973229));
#77185=CARTESIAN_POINT('Ctrl Pts',(-16.6544953518538,-18.5508495944172,
-2.68560931693323));
#77186=CARTESIAN_POINT('Ctrl Pts',(-16.6439997300583,-18.6097141394462,
-2.68954919806779));
#77187=CARTESIAN_POINT('Ctrl Pts',(-16.6214547373713,-18.776814584,-2.7006885988515));
#77188=CARTESIAN_POINT('Ctrl Pts',(-16.6152410173306,-18.8856579376055,
-2.70788290331176));
#77189=CARTESIAN_POINT('Ctrl Pts',(-16.6189294810739,-19.0693393875393,
-2.71968573748178));
#77190=CARTESIAN_POINT('Ctrl Pts',(-16.6244003470743,-19.1440501695098,
-2.72439467406062));
#77191=CARTESIAN_POINT('Ctrl Pts',(-16.6361815638864,-19.2369554518382,
-2.7301315167553));
#77192=CARTESIAN_POINT('Ctrl Pts',(-16.6387924334566,-19.2555573903308,
-2.73127433200432));
#77193=CARTESIAN_POINT('Ctrl Pts',(-16.6429515323512,-19.2825728436937,
-2.73292595535522));
#77194=CARTESIAN_POINT('Ctrl Pts',(-16.644303662991,-19.2910152230879,-2.73344094020871));
#77195=CARTESIAN_POINT('Ctrl Pts',(-16.6467652682766,-19.3058103417579,
-2.73434148848935));
#77196=CARTESIAN_POINT('Ctrl Pts',(-16.6478526870343,-19.3121665910108,
-2.73472774629328));
#77197=CARTESIAN_POINT('Ctrl Pts',(-16.6500215868135,-19.3245049348253,
-2.73547632877471));
#77198=CARTESIAN_POINT('Ctrl Pts',(-16.6510998235812,-19.3304875286672,
-2.73583875240774));
#77199=CARTESIAN_POINT('Ctrl Pts',(-16.653740677822,-19.3447871760181,-2.73670375035126));
#77200=CARTESIAN_POINT('Ctrl Pts',(-16.6553274331522,-19.3530997084849,
-2.73720555256272));
#77201=CARTESIAN_POINT('Ctrl Pts',(-16.6612435667179,-19.3831142283741,
-2.73901389463681));
#77202=CARTESIAN_POINT('Ctrl Pts',(-16.6658634084498,-19.4047579958013,
-2.7403111798372));
#77203=CARTESIAN_POINT('Ctrl Pts',(-16.712356256267,-19.6069881747458,-2.75237946205574));
#77204=CARTESIAN_POINT('Ctrl Pts',(-16.7774363137221,-19.7814079276443,
-2.76229617748199));
#77205=CARTESIAN_POINT('Ctrl Pts',(-16.9020687769329,-20.0160309433708,
-2.77677838677597));
#77206=CARTESIAN_POINT('Ctrl Pts',(-16.9437294307967,-20.0847237656925,
-2.78119283318351));
#77207=CARTESIAN_POINT('Ctrl Pts',(-17.0096109285556,-20.1806057863731,
-2.78784702134053));
#77208=CARTESIAN_POINT('Ctrl Pts',(-17.0307911844307,-20.2098033347825,
-2.78994486071768));
#77209=CARTESIAN_POINT('Ctrl Pts',(-17.0572437469074,-20.24437504082,-2.79253541732834));
#77210=CARTESIAN_POINT('Ctrl Pts',(-17.0618134287027,-20.250282267237,-2.79298192428639));
#77211=CARTESIAN_POINT('Ctrl Pts',(-17.0689768229347,-20.2594418242843,
-2.79368051603599));
#77212=CARTESIAN_POINT('Ctrl Pts',(-17.0715490783351,-20.262710966012,-2.79393110174537));
#77213=CARTESIAN_POINT('Ctrl Pts',(-17.0763441711972,-20.2687683427906,
-2.79439778391963));
#77214=CARTESIAN_POINT('Ctrl Pts',(-17.0785644240464,-20.2715585506529,
-2.79461369662171));
#77215=CARTESIAN_POINT('Ctrl Pts',(-17.0836087264691,-20.2778649943719,
-2.79510384257887));
#77216=CARTESIAN_POINT('Ctrl Pts',(-17.0864369547359,-20.2813778056135,
-2.79537837313561));
#77217=CARTESIAN_POINT('Ctrl Pts',(-17.0937678546657,-20.2904238493259,
-2.79608918027847));
#77218=CARTESIAN_POINT('Ctrl Pts',(-17.0982872670438,-20.2959433555661,
-2.79652662278851));
#77219=CARTESIAN_POINT('Ctrl Pts',(-17.1262020155252,-20.3296859324566,
-2.79922333626872));
#77220=CARTESIAN_POINT('Ctrl Pts',(-17.1502977877338,-20.3573184041027,
-2.80152877697819));
#77221=CARTESIAN_POINT('Ctrl Pts',(-17.2905198459883,-20.5099338860497,
-2.81475506622014));
#77222=CARTESIAN_POINT('Ctrl Pts',(-17.4207027263043,-20.6211453908159,
-2.82626658314038));
#77223=CARTESIAN_POINT('Ctrl Pts',(-17.6422309411859,-20.7682641858778,
-2.84354790066166));
#77224=CARTESIAN_POINT('Ctrl Pts',(-17.7251161516467,-20.8155806649673,
-2.84960399158042));
#77225=CARTESIAN_POINT('Ctrl Pts',(-17.8301635393875,-20.8664779788826,
-2.85677403699184));
#77226=CARTESIAN_POINT('Ctrl Pts',(-17.8495484397734,-20.8755102727644,
-2.85807747242254));
#77227=CARTESIAN_POINT('Ctrl Pts',(-17.8772897908168,-20.8879281420314,
-2.85991560516654));
#77228=CARTESIAN_POINT('Ctrl Pts',(-17.8855356458991,-20.8915562372278,
-2.86045860440219));
#77229=CARTESIAN_POINT('Ctrl Pts',(-17.8997946371104,-20.8977217176929,
-2.86139185880284));
#77230=CARTESIAN_POINT('Ctrl Pts',(-17.9057967607741,-20.900284113314,-2.8617829644363));
#77231=CARTESIAN_POINT('Ctrl Pts',(-17.9173074120821,-20.9051353761622,
-2.86252973492477));
#77232=CARTESIAN_POINT('Ctrl Pts',(-17.9228139434107,-20.9074287927441,
-2.86288555160323));
#77233=CARTESIAN_POINT('Ctrl Pts',(-17.9371485581939,-20.91332804874,-2.86380815248949));
#77234=CARTESIAN_POINT('Ctrl Pts',(-17.9459915056895,-20.9168975933875,
-2.8643737045856));
#77235=CARTESIAN_POINT('Ctrl Pts',(-17.9761783563008,-20.928846254373,-2.86629235026561));
#77236=CARTESIAN_POINT('Ctrl Pts',(-17.9976346070627,-20.9369384941645,
-2.86763581300588));
#77237=CARTESIAN_POINT('Ctrl Pts',(-18.1851701243143,-21.0042081119377,
-2.87921379355666));
#77238=CARTESIAN_POINT('Ctrl Pts',(-18.3579047976642,-21.0427729255352,
-2.88868917458312));
#77239=CARTESIAN_POINT('Ctrl Pts',(-18.6194739823872,-21.0676659669617,
-2.90298760447507));
#77240=CARTESIAN_POINT('Ctrl Pts',(-18.7059267822595,-21.0705769340084,
-2.9077208684055));
#77241=CARTESIAN_POINT('Ctrl Pts',(-18.8299702073384,-21.0671591569455,
-2.91480681872399));
#77242=CARTESIAN_POINT('Ctrl Pts',(-18.8675956958097,-21.065116261605,-2.91699559974952));
#77243=CARTESIAN_POINT('Ctrl Pts',(-18.9126825053349,-21.0614593540092,
-2.91968700219917));
#77244=CARTESIAN_POINT('Ctrl Pts',(-18.9202176178737,-21.0608075300537,
-2.92013910931319));
#77245=CARTESIAN_POINT('Ctrl Pts',(-18.9319118510765,-21.0597327571016,
-2.92084457189483));
#77246=CARTESIAN_POINT('Ctrl Pts',(-18.9360735719884,-21.0593378340849,
-2.9210963802099));
#77247=CARTESIAN_POINT('Ctrl Pts',(-18.9437810432223,-21.0585833986757,
-2.92156416115829));
#77248=CARTESIAN_POINT('Ctrl Pts',(-18.9473270656625,-21.0582272584276,
-2.92177994256916));
#77249=CARTESIAN_POINT('Ctrl Pts',(-18.9553310718424,-21.0574029660065,
-2.92226827503101));
#77250=CARTESIAN_POINT('Ctrl Pts',(-18.9597884524445,-21.056929610823,-2.92254111395026));
#77251=CARTESIAN_POINT('Ctrl Pts',(-18.9729092891475,-21.0554940773037,
-2.9233468012166));
#77252=CARTESIAN_POINT('Ctrl Pts',(-18.9815682219235,-21.0544925567489,
-2.92388178430716));
#77253=CARTESIAN_POINT('Ctrl Pts',(-19.0431247851564,-21.0469871916588,
-2.92770715323812));
#77254=CARTESIAN_POINT('Ctrl Pts',(-19.0957619578154,-21.0385418084244,
-2.93109442716222));
#77255=CARTESIAN_POINT('Ctrl Pts',(-19.165639585287,-21.0246068341795,-2.93569932437968));
#77256=CARTESIAN_POINT('Ctrl Pts',(-19.183214058549,-21.0208688998034,-2.93686677563015));
#77257=CARTESIAN_POINT('Ctrl Pts',(-19.2477667355174,-21.0062778284428,
-2.94118471749289));
#77258=CARTESIAN_POINT('Ctrl Pts',(-19.2944169913585,-20.9940446170198,
-2.94436322108441));
#77259=CARTESIAN_POINT('Ctrl Pts',(-19.4454006226561,-20.9488880873146,
-2.95477330183771));
#77260=CARTESIAN_POINT('Ctrl Pts',(-19.5476151913201,-20.909469454547,-2.96200586331425));
#77261=CARTESIAN_POINT('Ctrl Pts',(-19.7146198451544,-20.8297115769728,
-2.97390182191414));
#77262=CARTESIAN_POINT('Ctrl Pts',(-19.7811168240447,-20.7934571956495,
-2.9786646070532));
#77263=CARTESIAN_POINT('Ctrl Pts',(-19.8616163856955,-20.7437944328501,
-2.98445954348771));
#77264=CARTESIAN_POINT('Ctrl Pts',(-19.8775638003171,-20.7336587422455,
-2.98560923791801));
#77265=CARTESIAN_POINT('Ctrl Pts',(-19.9005446269231,-20.7186171297813,
-2.9872689067531));
#77266=CARTESIAN_POINT('Ctrl Pts',(-19.907686968211,-20.7138800622817,-2.98778514283673));
#77267=CARTESIAN_POINT('Ctrl Pts',(-19.9201552917799,-20.7055011399917,
-2.98868713489284));
#77268=CARTESIAN_POINT('Ctrl Pts',(-19.9254937215573,-20.7018780920649,
-2.98907359210613));
#77269=CARTESIAN_POINT('Ctrl Pts',(-19.9358248392117,-20.6947974454344,
-2.98982202182923));
#77270=CARTESIAN_POINT('Ctrl Pts',(-19.9408193702581,-20.6913426599469,
-2.9901840958295));
#77271=CARTESIAN_POINT('Ctrl Pts',(-19.9527192190574,-20.6830354394547,
-2.99104740250487));
#77272=CARTESIAN_POINT('Ctrl Pts',(-19.9596105557258,-20.6781630851042,
-2.99154787000295));
#77273=CARTESIAN_POINT('Ctrl Pts',(-19.9843472197686,-20.6604508010163,
-2.99334636737155));
#77274=CARTESIAN_POINT('Ctrl Pts',(-20.0020218091838,-20.6473740160565,
-2.99463527563848));
#77275=CARTESIAN_POINT('Ctrl Pts',(-20.1679063249765,-20.5205964570162,
-3.00677962427125));
#77276=CARTESIAN_POINT('Ctrl Pts',(-20.3006543344855,-20.3880300454364,
-3.01676515693063));
#77277=CARTESIAN_POINT('Ctrl Pts',(-20.462557625633,-20.1767749022675,-3.03127852268068));
#77278=CARTESIAN_POINT('Ctrl Pts',(-20.5072414949363,-20.1111366026836,
-3.03564445976581));
#77279=CARTESIAN_POINT('Ctrl Pts',(-20.5665926592175,-20.0124602166786,
-3.04223265684119));
#77280=CARTESIAN_POINT('Ctrl Pts',(-20.5842695945084,-19.9813074422148,
-3.04431623325168));
#77281=CARTESIAN_POINT('Ctrl Pts',(-20.604659326247,-19.9431499558446,-3.04689096520608));
#77282=CARTESIAN_POINT('Ctrl Pts',(-20.6081371447691,-19.9365580270833,
-3.04733656748382));
#77283=CARTESIAN_POINT('Ctrl Pts',(-20.6135001055998,-19.9262615815686,
-3.04803404893226));
#77284=CARTESIAN_POINT('Ctrl Pts',(-20.6154093082858,-19.9225695700379,
-3.04828443672385));
#77285=CARTESIAN_POINT('Ctrl Pts',(-20.618936353984,-19.9156994651866,-3.04875094291312));
#77286=CARTESIAN_POINT('Ctrl Pts',(-20.6205570438794,-19.9125228978802,
-3.04896687876149));
#77287=CARTESIAN_POINT('Ctrl Pts',(-20.6242111978435,-19.9053157963717,
-3.04945732687813));
#77288=CARTESIAN_POINT('Ctrl Pts',(-20.6262397902928,-19.9012828636525,
-3.04973213801056));
#77289=CARTESIAN_POINT('Ctrl Pts',(-20.6322139769686,-19.8893106729462,
-3.05054896180295));
#77290=CARTESIAN_POINT('Ctrl Pts',(-20.6361225578581,-19.8813531990358,
-3.05109319647717));
#77291=CARTESIAN_POINT('Ctrl Pts',(-20.6648568363037,-19.8219124810826,
-3.05516702627434));
#77292=CARTESIAN_POINT('Ctrl Pts',(-20.6876362395481,-19.7694717412689,
-3.05880796392093));
#77293=CARTESIAN_POINT('Ctrl Pts',(-20.7131593808188,-19.703532466891,-3.06338860271513));
#77294=CARTESIAN_POINT('Ctrl Pts',(-20.7179316577104,-19.6908422631791,
-3.06427030004251));
#77295=CARTESIAN_POINT('Ctrl Pts',(-20.7225805657411,-19.6781104141636,
-3.06515450115675));
#77296=CARTESIAN_POINT('',(-20.8479141126547,-18.952828455763,-2.0890042932752));
#77297=CARTESIAN_POINT('Ctrl Pts',(-20.7202230519095,-19.6772708889146,
-2.84456322442383));
#77298=CARTESIAN_POINT('Ctrl Pts',(-20.6328469601815,-19.9216249165611,
-2.82899806527974));
#77299=CARTESIAN_POINT('Ctrl Pts',(-20.1480308925685,-20.7713282564288,
-2.77104097057519));
#77300=CARTESIAN_POINT('Ctrl Pts',(-18.3741968385222,-21.4292710094645,
-2.67069194031011));
#77301=CARTESIAN_POINT('Ctrl Pts',(-16.4562524857842,-19.9903623098931,
-2.54351613362868));
#77302=CARTESIAN_POINT('Ctrl Pts',(-16.6280001024638,-17.5988205946497,
-2.41634032694725));
#77303=CARTESIAN_POINT('Ctrl Pts',(-18.7318719157381,-16.448737081536,-2.28916452026583));
#77304=CARTESIAN_POINT('Ctrl Pts',(-20.5383021468591,-17.4322383264222,
-2.18006983762423));
#77305=CARTESIAN_POINT('Ctrl Pts',(-20.8463943934263,-18.5471996728808,
-2.11336709054313));
#77306=CARTESIAN_POINT('Ctrl Pts',(-20.8478239065824,-18.9528314138757,
-2.0890562790225));
#77307=CARTESIAN_POINT('Ctrl Pts',(-20.8509998750793,-18.9527272648688,
-2.08722596880618));
#77308=CARTESIAN_POINT('Ctrl Pts',(-20.8509329970117,-19.1474030521012,
-2.07601660755437));
#77309=CARTESIAN_POINT('Ctrl Pts',(-20.8240164192313,-19.3411372216795,
-2.0657352891835));
#77310=CARTESIAN_POINT('Ctrl Pts',(-20.7567161848195,-19.5789442372845,
-2.05215238229222));
#77311=CARTESIAN_POINT('Ctrl Pts',(-20.7405652872149,-19.6288561003616,
-2.04923741397087));
#77312=CARTESIAN_POINT('Ctrl Pts',(-20.7225805826894,-19.6781103677477,
-2.04625070052543));
#77313=CARTESIAN_POINT('Origin',(-18.734,-18.952,0.));
#77314=CARTESIAN_POINT('',(-20.7225806439552,-19.6781101999605,-1.24458624895941));
#77315=CARTESIAN_POINT('',(-20.7225805819607,-19.6781103697435,-1.46829802089257));
#77316=CARTESIAN_POINT('',(-20.7225805821191,-19.6781103693095,0.));
#77317=CARTESIAN_POINT('Ctrl Pts',(-20.7225805819607,-19.6781103697434,
-1.46829802089257));
#77318=CARTESIAN_POINT('Ctrl Pts',(-20.7720931560047,-19.5425115029463,
-1.47674759264403));
#77319=CARTESIAN_POINT('Ctrl Pts',(-20.8076106549703,-19.4021955091639,
-1.48469159119666));
#77320=CARTESIAN_POINT('Ctrl Pts',(-20.8435716231799,-19.1571126846671,
-1.4981609862824));
#77321=CARTESIAN_POINT('Ctrl Pts',(-20.8510665767008,-19.0539337997499,
-1.50372418439499));
#77322=CARTESIAN_POINT('Ctrl Pts',(-20.8509605931235,-18.8905719691387,
-1.51286258178651));
#77323=CARTESIAN_POINT('Ctrl Pts',(-20.8483662197456,-18.8305518846646,
-1.51629231097292));
#77324=CARTESIAN_POINT('Ctrl Pts',(-20.8424571653604,-18.7617954033505,
-1.52038555277385));
#77325=CARTESIAN_POINT('Ctrl Pts',(-20.8416326174778,-18.7528665018886,
-1.52092031606078));
#77326=CARTESIAN_POINT('Ctrl Pts',(-20.8403055944572,-18.7394292637794,
-1.52173027738312));
#77327=CARTESIAN_POINT('Ctrl Pts',(-20.8398453004456,-18.7349167329088,
-1.52200316307499));
#77328=CARTESIAN_POINT('Ctrl Pts',(-20.8389970510928,-18.7268575017177,
-1.52249215995441));
#77329=CARTESIAN_POINT('Ctrl Pts',(-20.8386146291968,-18.7233102714294,
-1.52270795724757));
#77330=CARTESIAN_POINT('Ctrl Pts',(-20.8377689773509,-18.715648065319,-1.52317533193935));
#77331=CARTESIAN_POINT('Ctrl Pts',(-20.8373026471316,-18.7115335345996,
-1.52342707634132));
#77332=CARTESIAN_POINT('Ctrl Pts',(-20.8359714183482,-18.700088014928,-1.52412945106569));
#77333=CARTESIAN_POINT('Ctrl Pts',(-20.8350802524046,-18.6927602248131,
-1.52458152096667));
#77334=CARTESIAN_POINT('Ctrl Pts',(-20.8297855243033,-18.6510449721524,
-1.52716806677283));
#77335=CARTESIAN_POINT('Ctrl Pts',(-20.8245763700799,-18.6167672271824,
-1.52934386967377));
#77336=CARTESIAN_POINT('Ctrl Pts',(-20.805407203348,-18.5085850836545,-1.53633896031892));
#77337=CARTESIAN_POINT('Ctrl Pts',(-20.7883503689925,-18.4352915707807,
-1.5412675751516));
#77338=CARTESIAN_POINT('Ctrl Pts',(-20.7136651896318,-18.1774233514788,
-1.55897631652309));
#77339=CARTESIAN_POINT('Ctrl Pts',(-20.6347145051753,-17.9999712102452,
-1.57174497002659));
#77340=CARTESIAN_POINT('Ctrl Pts',(-20.5215596546255,-17.8176409598084,
-1.58493005964286));
#77341=CARTESIAN_POINT('Ctrl Pts',(-20.5100907444826,-17.7997666599859,
-1.5862249121803));
#77342=CARTESIAN_POINT('Ctrl Pts',(-20.4937578044299,-17.7751352437741,
-1.58801303729796));
#77343=CARTESIAN_POINT('Ctrl Pts',(-20.4891202512924,-17.7682301358412,
-1.58851473814774));
#77344=CARTESIAN_POINT('Ctrl Pts',(-20.4810444540192,-17.7563574238619,
-1.58937815825898));
#77345=CARTESIAN_POINT('Ctrl Pts',(-20.4776254463123,-17.7513769124568,
-1.58974059901217));
#77346=CARTESIAN_POINT('Ctrl Pts',(-20.4705005725153,-17.7410926446403,
-1.59048953820632));
#77347=CARTESIAN_POINT('Ctrl Pts',(-20.4667916131035,-17.7357910999329,
-1.59087591362798));
#77348=CARTESIAN_POINT('Ctrl Pts',(-20.4580471971384,-17.7234131324265,
-1.59177876182168));
#77349=CARTESIAN_POINT('Ctrl Pts',(-20.4529923593877,-17.716350494303,-1.59229448462309));
#77350=CARTESIAN_POINT('Ctrl Pts',(-20.4364321359028,-17.6935107857039,
-1.5939643184017));
#77351=CARTESIAN_POINT('Ctrl Pts',(-20.4247516920709,-17.6778614544143,
-1.59511164885719));
#77352=CARTESIAN_POINT('Ctrl Pts',(-20.3638543848995,-17.5985842527767,
-1.6009440987315));
#77353=CARTESIAN_POINT('Ctrl Pts',(-20.3112537720283,-17.537633684328,-1.60549259413782));
#77354=CARTESIAN_POINT('Ctrl Pts',(-20.1384828374626,-17.3590974186498,
-1.61926744787057));
#77355=CARTESIAN_POINT('Ctrl Pts',(-20.0077162434858,-17.2527206740547,
-1.62810931945867));
#77356=CARTESIAN_POINT('Ctrl Pts',(-19.8645504722943,-17.1621545623342,
-1.63762197913388));
#77357=CARTESIAN_POINT('Ctrl Pts',(-19.8633364114307,-17.1613882802404,
-1.63770263978496));
#77358=CARTESIAN_POINT('Ctrl Pts',(-19.8165501446093,-17.1319245750012,
-1.6408107992702));
#77359=CARTESIAN_POINT('Ctrl Pts',(-19.769904206213,-17.1049778566222,-1.64389995115153));
#77360=CARTESIAN_POINT('Ctrl Pts',(-19.7145580901597,-17.0757614222467,
-1.64761374906773));
#77361=CARTESIAN_POINT('Ctrl Pts',(-19.7068048260349,-17.071729771199,-1.64813508316971));
#77362=CARTESIAN_POINT('Ctrl Pts',(-19.6950330254656,-17.0657008032327,
-1.64892859080482));
#77363=CARTESIAN_POINT('Ctrl Pts',(-19.6910326250181,-17.0636680139448,
-1.64919858901596));
#77364=CARTESIAN_POINT('Ctrl Pts',(-19.6838431557468,-17.0600434245146,
-1.64968449156431));
#77365=CARTESIAN_POINT('Ctrl Pts',(-19.680656505283,-17.0584469469397,-1.6499000984515));
#77366=CARTESIAN_POINT('Ctrl Pts',(-19.6737267013854,-17.0549970552061,
-1.65036948900504));
#77367=CARTESIAN_POINT('Ctrl Pts',(-19.6699821394481,-17.0531466934511,
-1.65062345280078));
#77368=CARTESIAN_POINT('Ctrl Pts',(-19.65945663646,-17.0479842528489,-1.65133817465765));
#77369=CARTESIAN_POINT('Ctrl Pts',(-19.6526635046141,-17.0446973725394,
-1.65180045401116));
#77370=CARTESIAN_POINT('Ctrl Pts',(-19.6121122934695,-17.0253434237479,
-1.65456529495592));
#77371=CARTESIAN_POINT('Ctrl Pts',(-19.5779531778002,-17.010137646603,-1.6569159911075));
#77372=CARTESIAN_POINT('Ctrl Pts',(-19.4646002505116,-16.9632348036155,
-1.66474517783172));
#77373=CARTESIAN_POINT('Ctrl Pts',(-19.3838947010915,-16.935419047224,-1.67036146853556));
#77374=CARTESIAN_POINT('Ctrl Pts',(-19.1303439587519,-16.8648362097004,
-1.68774849196257));
#77375=CARTESIAN_POINT('Ctrl Pts',(-18.9535825726714,-16.8389100513405,
-1.69943933765766));
#77376=CARTESIAN_POINT('Ctrl Pts',(-18.7528413217338,-16.8349610585024,
-1.71179541625068));
#77377=CARTESIAN_POINT('Ctrl Pts',(-18.7300385391062,-16.8348809089096,
-1.71318715496088));
#77378=CARTESIAN_POINT('Ctrl Pts',(-18.6977241054554,-16.8352894407271,
-1.71514335073775));
#77379=CARTESIAN_POINT('Ctrl Pts',(-18.6882108216452,-16.8354738631353,
-1.71571727820927));
#77380=CARTESIAN_POINT('Ctrl Pts',(-18.6727398788415,-16.8358781385027,
-1.71664750104682));
#77381=CARTESIAN_POINT('Ctrl Pts',(-18.6667814139094,-16.8360590277692,
-1.71700501229205));
#77382=CARTESIAN_POINT('Ctrl Pts',(-18.6542981447292,-16.8364907826573,
-1.71775246541144));
#77383=CARTESIAN_POINT('Ctrl Pts',(-18.6477735683102,-16.8367466727726,
-1.71814224583394));
#77384=CARTESIAN_POINT('Ctrl Pts',(-18.6322317703546,-16.8374282428006,
-1.71906865220709));
#77385=CARTESIAN_POINT('Ctrl Pts',(-18.6232158351792,-16.8378814220628,
-1.71960441083953));
#77386=CARTESIAN_POINT('Ctrl Pts',(-18.5927430277503,-16.8396085883,-1.72140981157502));
#77387=CARTESIAN_POINT('Ctrl Pts',(-18.5713023058927,-16.8411517063428,
-1.7226710194346));
#77388=CARTESIAN_POINT('Ctrl Pts',(-18.3711113374509,-16.8586281824042,
-1.7343712045856));
#77389=CARTESIAN_POINT('Ctrl Pts',(-18.1950470064643,-16.8969013635447,
-1.74401336695471));
#77390=CARTESIAN_POINT('Ctrl Pts',(-17.9123555806182,-16.9972345763578,
-1.76033857027388));
#77391=CARTESIAN_POINT('Ctrl Pts',(-17.8024670832392,-17.0471521413233,
-1.76694910621919));
#77392=CARTESIAN_POINT('Ctrl Pts',(-17.689157312473,-17.1107822137987,-1.77465096526347));
#77393=CARTESIAN_POINT('Ctrl Pts',(-17.6809088778169,-17.1154874738563,
-1.77521700333436));
#77394=CARTESIAN_POINT('Ctrl Pts',(-17.6687290579812,-17.1225443971041,
-1.77606125136031));
#77395=CARTESIAN_POINT('Ctrl Pts',(-17.6647730693753,-17.1248536586254,
-1.77633678946594));
#77396=CARTESIAN_POINT('Ctrl Pts',(-17.657745774603,-17.1289863960063,-1.77682867067709));
#77397=CARTESIAN_POINT('Ctrl Pts',(-17.6546715578725,-17.1308048232506,
-1.7770446848463));
#77398=CARTESIAN_POINT('Ctrl Pts',(-17.6480695597411,-17.1347325533149,
-1.77751039119574));
#77399=CARTESIAN_POINT('Ctrl Pts',(-17.6445433666054,-17.136844321511,-1.77776023901127));
#77400=CARTESIAN_POINT('Ctrl Pts',(-17.6348212205239,-17.1427052597282,
-1.77845212054551));
#77401=CARTESIAN_POINT('Ctrl Pts',(-17.628638389739,-17.1464759338364,-1.77889552601222));
#77402=CARTESIAN_POINT('Ctrl Pts',(-17.5947783719678,-17.1673649810112,
-1.78134203262665));
#77403=CARTESIAN_POINT('Ctrl Pts',(-17.5674810060627,-17.1850870886606,
-1.78338149012634));
#77404=CARTESIAN_POINT('Ctrl Pts',(-17.4062222837481,-17.2951458252544,
-1.79578761632431));
#77405=CARTESIAN_POINT('Ctrl Pts',(-17.2828639885251,-17.4020439918414,
-1.80674408137016));
#77406=CARTESIAN_POINT('Ctrl Pts',(-17.0940640645746,-17.6081460680513,
-1.82500120375695));
#77407=CARTESIAN_POINT('Ctrl Pts',(-17.0224165578849,-17.7006714304132,
-1.83244184753139));
#77408=CARTESIAN_POINT('Ctrl Pts',(-16.9509757340412,-17.8106334283907,
-1.84044872018204));
#77409=CARTESIAN_POINT('Ctrl Pts',(-16.9433122522029,-17.8226946429811,
-1.84131669273718));
#77410=CARTESIAN_POINT('Ctrl Pts',(-16.9313097879687,-17.842014199276,-1.84269099629933));
#77411=CARTESIAN_POINT('Ctrl Pts',(-16.9268912599426,-17.8492223781695,
-1.84320025535469));
#77412=CARTESIAN_POINT('Ctrl Pts',(-16.9191746503873,-17.8619818169293,
-1.8440956310349));
#77413=CARTESIAN_POINT('Ctrl Pts',(-16.9158585847764,-17.8675220220293,
-1.84448240378293));
#77414=CARTESIAN_POINT('Ctrl Pts',(-16.909052320419,-17.8790123254048,-1.84528047090647));
#77415=CARTESIAN_POINT('Ctrl Pts',(-16.9055657493798,-17.8849644917192,
-1.84569162990037));
#77416=CARTESIAN_POINT('Ctrl Pts',(-16.8966908776356,-17.9002866285896,
-1.84674433828627));
#77417=CARTESIAN_POINT('Ctrl Pts',(-16.8913450888508,-17.9096810892519,
-1.84738434637507));
#77418=CARTESIAN_POINT('Ctrl Pts',(-16.8693339283149,-17.9490611758034,
-1.85004501217718));
#77419=CARTESIAN_POINT('Ctrl Pts',(-16.8533261471882,-17.9794096957476,
-1.85204214106567));
#77420=CARTESIAN_POINT('Ctrl Pts',(-16.8135457661922,-18.0594860747149,
-1.85718622303641));
#77421=CARTESIAN_POINT('Ctrl Pts',(-16.7909643176087,-18.1097776105255,
-1.86029378691145));
#77422=CARTESIAN_POINT('Ctrl Pts',(-16.7295080505817,-18.2623206019634,
-1.86943820421793));
#77423=CARTESIAN_POINT('Ctrl Pts',(-16.6965647403786,-18.3667615068895,
-1.87532632806816));
#77424=CARTESIAN_POINT('Ctrl Pts',(-16.6614948457228,-18.5178305125628,
-1.88376987107214));
#77425=CARTESIAN_POINT('Ctrl Pts',(-16.6525992748352,-18.5627037860073,
-1.88627060963726));
#77426=CARTESIAN_POINT('Ctrl Pts',(-16.6414615163854,-18.6303007519883,
-1.89006945553716));
#77427=CARTESIAN_POINT('Ctrl Pts',(-16.6381218045566,-18.6528307339971,
-1.89134087530487));
#77428=CARTESIAN_POINT('Ctrl Pts',(-16.6350173565239,-18.6763882500269,
-1.89267965899724));
#77429=CARTESIAN_POINT('Ctrl Pts',(-16.6348890764467,-18.6773669631099,
-1.89273529654612));
#77430=CARTESIAN_POINT('Ctrl Pts',(-16.6324974615984,-18.6957133628997,
-1.89377856834965));
#77431=CARTESIAN_POINT('Ctrl Pts',(-16.6304491159064,-18.7131079602769,
-1.89477311962891));
#77432=CARTESIAN_POINT('Ctrl Pts',(-16.6250305537704,-18.7646179557352,
-1.89773935511748));
#77433=CARTESIAN_POINT('Ctrl Pts',(-16.6222730658847,-18.7987903068576,
-1.89973448825879));
#77434=CARTESIAN_POINT('Ctrl Pts',(-16.6199541902419,-18.8399819454601,
-1.90218822447091));
#77435=CARTESIAN_POINT('Ctrl Pts',(-16.619596315564,-18.8469534080429,-1.9026051854378));
#77436=CARTESIAN_POINT('Ctrl Pts',(-16.6190661743308,-18.8583846602077,
-1.90329182261017));
#77437=CARTESIAN_POINT('Ctrl Pts',(-16.6188735170734,-18.8628435129217,
-1.90356038335881));
#77438=CARTESIAN_POINT('Ctrl Pts',(-16.6185524253135,-18.8708627600133,
-1.90404475977978));
#77439=CARTESIAN_POINT('Ctrl Pts',(-16.6184188776031,-18.8744228950945,
-1.90426028618967));
#77440=CARTESIAN_POINT('Ctrl Pts',(-16.6181476248048,-18.8821764398172,
-1.90473075032974));
#77441=CARTESIAN_POINT('Ctrl Pts',(-16.6180134005704,-18.8863698734934,
-1.90498587502555));
#77442=CARTESIAN_POINT('Ctrl Pts',(-16.6176701236929,-18.8981936700985,
-1.90570708368143));
#77443=CARTESIAN_POINT('Ctrl Pts',(-16.6174898759185,-18.905824713597,-1.90617473268144));
#77444=CARTESIAN_POINT('Ctrl Pts',(-16.6166422978356,-18.9523701010658,
-1.9090397744387));
#77445=CARTESIAN_POINT('Ctrl Pts',(-16.6170069957211,-18.991293154584,-1.91148936322848));
#77446=CARTESIAN_POINT('Ctrl Pts',(-16.624432178869,-19.192216446517,-1.92433805849365));
#77447=CARTESIAN_POINT('Ctrl Pts',(-16.6490153671944,-19.3530249496497,
-1.93525759681636));
#77448=CARTESIAN_POINT('Ctrl Pts',(-16.720801572638,-19.6160210132374,-1.95302136151426));
#77449=CARTESIAN_POINT('Ctrl Pts',(-16.7581895162412,-19.7201610518911,
-1.96004026467851));
#77450=CARTESIAN_POINT('Ctrl Pts',(-16.809364870051,-19.8338558992318,-1.9676522676726));
#77451=CARTESIAN_POINT('Ctrl Pts',(-16.8153170027438,-19.8467322403145,
-1.96851381223093));
#77452=CARTESIAN_POINT('Ctrl Pts',(-16.8250096346055,-19.8671588670269,
-1.96987989211645));
#77453=CARTESIAN_POINT('Ctrl Pts',(-16.828666484445,-19.8747481589113,-1.97038730120075));
#77454=CARTESIAN_POINT('Ctrl Pts',(-16.8352038190521,-19.888110938308,-1.97128052825651));
#77455=CARTESIAN_POINT('Ctrl Pts',(-16.8380655604922,-19.8938934271563,
-1.9716669924283));
#77456=CARTESIAN_POINT('Ctrl Pts',(-16.8440471794529,-19.9058422781841,
-1.97246548443794));
#77457=CARTESIAN_POINT('Ctrl Pts',(-16.8471709088992,-19.9120066344886,
-1.97287737165393));
#77458=CARTESIAN_POINT('Ctrl Pts',(-16.8552835589183,-19.9278235453769,
-1.97393415242114));
#77459=CARTESIAN_POINT('Ctrl Pts',(-16.8603167474348,-19.9374532629306,
-1.97457748121119));
#77460=CARTESIAN_POINT('Ctrl Pts',(-16.8817820617469,-19.9777626112148,
-1.97727060546021));
#77461=CARTESIAN_POINT('Ctrl Pts',(-16.8988958476915,-20.008074419974,-1.97929613321528));
#77462=CARTESIAN_POINT('Ctrl Pts',(-16.9455837646253,-20.0862027630167,
-1.98453016001506));
#77463=CARTESIAN_POINT('Ctrl Pts',(-16.9763291082887,-20.1332883872032,
-1.98769743867443));
#77464=CARTESIAN_POINT('Ctrl Pts',(-17.0817706984249,-20.2815209961167,
-1.9978032875194));
#77465=CARTESIAN_POINT('Ctrl Pts',(-17.1636028273967,-20.3772510786442,
-2.00452990898683));
#77466=CARTESIAN_POINT('Ctrl Pts',(-17.3250192108307,-20.5351897250686,
-2.01688751694712));
#77467=CARTESIAN_POINT('Ctrl Pts',(-17.401463959395,-20.6000470132183,-2.02245412321344));
#77468=CARTESIAN_POINT('Ctrl Pts',(-17.4900160570699,-20.6649760445418,
-2.02895946080841));
#77469=CARTESIAN_POINT('Ctrl Pts',(-17.4978730895972,-20.6706544832367,
-2.02953715294625));
#77470=CARTESIAN_POINT('Ctrl Pts',(-17.5095311331976,-20.6789586946519,
-2.03039548033192));
#77471=CARTESIAN_POINT('Ctrl Pts',(-17.5133023117823,-20.681626402393,-2.03067331277748));
#77472=CARTESIAN_POINT('Ctrl Pts',(-17.5200080570562,-20.6863371495187,
-2.03116771579227));
#77473=CARTESIAN_POINT('Ctrl Pts',(-17.5229391003863,-20.6883851194223,
-2.03138394443113));
#77474=CARTESIAN_POINT('Ctrl Pts',(-17.5292300518527,-20.6927570368103,
-2.03184833071061));
#77475=CARTESIAN_POINT('Ctrl Pts',(-17.5325914517094,-20.6950786524439,
-2.03209663463902));
#77476=CARTESIAN_POINT('Ctrl Pts',(-17.5418367574082,-20.7014246538077,
-2.03278000064794));
#77477=CARTESIAN_POINT('Ctrl Pts',(-17.5477342403474,-20.7054290292111,
-2.03321638046797));
#77478=CARTESIAN_POINT('Ctrl Pts',(-17.5793268591596,-20.7266479998233,
-2.03555605303473));
#77479=CARTESIAN_POINT('Ctrl Pts',(-17.6053752782282,-20.7433267679299,
-2.03749213161147));
#77480=CARTESIAN_POINT('Ctrl Pts',(-17.6853208634728,-20.7920799048843,
-2.04343315903331));
#77481=CARTESIAN_POINT('Ctrl Pts',(-17.7402846192009,-20.8223343632513,
-2.04751558425808));
#77482=CARTESIAN_POINT('Ctrl Pts',(-17.9269437673714,-20.9145274204903,
-2.06119652295239));
#77483=CARTESIAN_POINT('Ctrl Pts',(-18.0636913134972,-20.9653423845116,
-2.07089652908973));
#77484=CARTESIAN_POINT('Ctrl Pts',(-18.2773306865386,-21.020523315321,-2.08502433209331));
#77485=CARTESIAN_POINT('Ctrl Pts',(-18.3510416139255,-21.0354300157609,
-2.08973101563419));
#77486=CARTESIAN_POINT('Ctrl Pts',(-18.4383920181184,-21.0483008988569,
-2.095113975572));
#77487=CARTESIAN_POINT('Ctrl Pts',(-18.4514048216643,-21.0500947344908,
-2.09591096010546));
#77488=CARTESIAN_POINT('Ctrl Pts',(-18.4725698737199,-21.0528118852477,
-2.09719942659657));
#77489=CARTESIAN_POINT('Ctrl Pts',(-18.4807121246604,-21.0538091120003,
-2.09769323066074));
#77490=CARTESIAN_POINT('Ctrl Pts',(-18.4952174439366,-21.0555001441856,
-2.09856966623564));
#77491=CARTESIAN_POINT('Ctrl Pts',(-18.5015782129253,-21.0562124607454,
-2.09895287706902));
#77492=CARTESIAN_POINT('Ctrl Pts',(-18.5149835319341,-21.0576521411115,
-2.09975817978));
#77493=CARTESIAN_POINT('Ctrl Pts',(-18.5220287095392,-21.058373026447,-2.10018006312557));
#77494=CARTESIAN_POINT('Ctrl Pts',(-18.5406629914278,-21.0601853086807,
-2.10129245268935));
#77495=CARTESIAN_POINT('Ctrl Pts',(-18.5522578105289,-21.061216508412,-2.10198106081862));
#77496=CARTESIAN_POINT('Ctrl Pts',(-18.6060541942796,-21.0655540526629,
-2.10516016387081));
#77497=CARTESIAN_POINT('Ctrl Pts',(-18.6483421141709,-21.0676899465985,
-2.10761379689482));
#77498=CARTESIAN_POINT('Ctrl Pts',(-18.7648645872267,-21.0700755020006,
-2.11427452492477));
#77499=CARTESIAN_POINT('Ctrl Pts',(-18.8390937832549,-21.0676921010481,
-2.11840428181186));
#77500=CARTESIAN_POINT('Ctrl Pts',(-19.0791534827002,-21.0473156275731,
-2.13162883027534));
#77501=CARTESIAN_POINT('Ctrl Pts',(-19.2429910353896,-21.0136485769753,
-2.14041564688287));
#77502=CARTESIAN_POINT('Ctrl Pts',(-19.434565167532,-20.9500330449553,-2.15196475350744));
#77503=CARTESIAN_POINT('Ctrl Pts',(-19.4676816584993,-20.9381114023114,
-2.15401157799856));
#77504=CARTESIAN_POINT('Ctrl Pts',(-19.5070465388779,-20.9228215601371,
-2.15652283454657));
#77505=CARTESIAN_POINT('Ctrl Pts',(-19.5135968095329,-20.9202396664534,
-2.15694334048251));
#77506=CARTESIAN_POINT('Ctrl Pts',(-19.5242950041681,-20.9159610204893,
-2.15763464107657));
#77507=CARTESIAN_POINT('Ctrl Pts',(-19.5284506947994,-20.914283663566,-2.15790429446698));
#77508=CARTESIAN_POINT('Ctrl Pts',(-19.5359015412223,-20.9112487384921,
-2.15838982847879));
#77509=CARTESIAN_POINT('Ctrl Pts',(-19.5391986201502,-20.9098960347546,
-2.15860541360415));
#77510=CARTESIAN_POINT('Ctrl Pts',(-19.54635659736,-20.906938168159,-2.15907505243277));
#77511=CARTESIAN_POINT('Ctrl Pts',(-19.5502161101035,-20.9053299115891,
-2.15932928787843));
#77512=CARTESIAN_POINT('Ctrl Pts',(-19.5609065938249,-20.9008379776625,
-2.16003625065996));
#77513=CARTESIAN_POINT('Ctrl Pts',(-19.5677271404579,-20.8979298624608,
-2.16049042168676));
#77514=CARTESIAN_POINT('Ctrl Pts',(-19.6072724394993,-20.8808226394272,
-2.16314130578718));
#77515=CARTESIAN_POINT('Ctrl Pts',(-19.6396473324771,-20.8658349168796,
-2.16538179422692));
#77516=CARTESIAN_POINT('Ctrl Pts',(-19.7424836811496,-20.8150340173786,
-2.17269150338552));
#77517=CARTESIAN_POINT('Ctrl Pts',(-19.8113211986012,-20.7760922234604,
-2.17788069750092));
#77518=CARTESIAN_POINT('Ctrl Pts',(-19.9507806423674,-20.6865468243716,
-2.18882077245553));
#77519=CARTESIAN_POINT('Ctrl Pts',(-20.0208012369451,-20.6352562117291,
-2.19456593442936));
#77520=CARTESIAN_POINT('Ctrl Pts',(-20.1722642798111,-20.5093190955114,
-2.20740013127517));
#77521=CARTESIAN_POINT('Ctrl Pts',(-20.2514210750559,-20.4322995660472,
-2.21440553909444));
#77522=CARTESIAN_POINT('Ctrl Pts',(-20.333587503665,-20.33879844327,-2.22200484823458));
#77523=CARTESIAN_POINT('Ctrl Pts',(-20.3428414896205,-20.3280520269145,
-2.22286616210404));
#77524=CARTESIAN_POINT('Ctrl Pts',(-20.3574188713835,-20.3107755946574,
-2.22423194628946));
#77525=CARTESIAN_POINT('Ctrl Pts',(-20.3628123594039,-20.3043055311788,
-2.22473928843057));
#77526=CARTESIAN_POINT('Ctrl Pts',(-20.3722685160257,-20.2928232145257,
-2.22563243727655));
#77527=CARTESIAN_POINT('Ctrl Pts',(-20.3763471297789,-20.2878242885755,
-2.22601888982665));
#77528=CARTESIAN_POINT('Ctrl Pts',(-20.3847473016138,-20.2774320457245,
-2.2268173959899));
#77529=CARTESIAN_POINT('Ctrl Pts',(-20.3890654343432,-20.2720360492813,
-2.22722930879292));
#77530=CARTESIAN_POINT('Ctrl Pts',(-20.4001056081468,-20.2581007634803,
-2.22828623475696));
#77531=CARTESIAN_POINT('Ctrl Pts',(-20.4067885119983,-20.2495306172316,
-2.22892968230987));
#77532=CARTESIAN_POINT('Ctrl Pts',(-20.4346053675792,-20.2132861943621,
-2.23162398089347));
#77533=CARTESIAN_POINT('Ctrl Pts',(-20.4551215893789,-20.1851432034442,
-2.23365053718074));
#77534=CARTESIAN_POINT('Ctrl Pts',(-20.5323186411735,-20.0735662598666,
-2.2414529178018));
#77535=CARTESIAN_POINT('Ctrl Pts',(-20.5837048545482,-19.9866283045965,
-2.2470334705779));
#77536=CARTESIAN_POINT('Ctrl Pts',(-20.663586701512,-19.8263570355579,-2.25680806958959));
#77537=CARTESIAN_POINT('Ctrl Pts',(-20.6945668143561,-19.7544852992699,
-2.26102665247313));
#77538=CARTESIAN_POINT('Ctrl Pts',(-20.7218604140742,-19.6800804036127,
-2.26535923033235));
#77539=CARTESIAN_POINT('Ctrl Pts',(-20.7222208667441,-19.6790955129461,
-2.26541657466571));
#77540=CARTESIAN_POINT('Ctrl Pts',(-20.7225805820961,-19.6781103693727,
-2.2654739284689));
#77541=CARTESIAN_POINT('Ctrl Pts',(-20.7225805826894,-19.6781103677477,
-2.04625070052543));
#77542=CARTESIAN_POINT('Ctrl Pts',(-20.7190678195543,-19.6877306856393,
-2.04566733720848));
#77543=CARTESIAN_POINT('Ctrl Pts',(-20.7154850976113,-19.6973259159891,
-2.04508122692791));
#77544=CARTESIAN_POINT('Ctrl Pts',(-20.7008062983039,-19.7357845066084,
-2.04271342574978));
#77545=CARTESIAN_POINT('Ctrl Pts',(-20.6891489348871,-19.7644269710652,
-2.04090765878723));
#77546=CARTESIAN_POINT('Ctrl Pts',(-20.6740381866449,-19.7993438756357,
-2.03864177403879));
#77547=CARTESIAN_POINT('Ctrl Pts',(-20.6711741826596,-19.8058711799589,
-2.03821537891728));
#77548=CARTESIAN_POINT('Ctrl Pts',(-20.6666170552106,-19.8161163151558,
-2.03754149041164));
#77549=CARTESIAN_POINT('Ctrl Pts',(-20.6649460105186,-19.8198439906011,
-2.03729532896267));
#77550=CARTESIAN_POINT('Ctrl Pts',(-20.6617920753461,-19.8268254112321,
-2.03683244207514));
#77551=CARTESIAN_POINT('Ctrl Pts',(-20.6603117271752,-19.8300802440396,
-2.03661587282193));
#77552=CARTESIAN_POINT('Ctrl Pts',(-20.6568999800089,-19.8375314827844,
-2.03611833908501));
#77553=CARTESIAN_POINT('Ctrl Pts',(-20.6549630922218,-19.8417253157622,
-2.03583703971688));
#77554=CARTESIAN_POINT('Ctrl Pts',(-20.6489187125119,-19.8547011241648,
-2.03496283317336));
#77555=CARTESIAN_POINT('Ctrl Pts',(-20.6447646756307,-19.863461102436,-2.0343671601292));
#77556=CARTESIAN_POINT('Ctrl Pts',(-20.5974979055914,-19.9613933702837,
-2.02764856428545));
#77557=CARTESIAN_POINT('Ctrl Pts',(-20.5482428284132,-20.0474532047992,
-2.02119626990881));
#77558=CARTESIAN_POINT('Ctrl Pts',(-20.3994673093771,-20.2696747704616,
-2.003579541899));
#77559=CARTESIAN_POINT('Ctrl Pts',(-20.2894008237162,-20.3979575619853,
-1.99239225570726));
#77560=CARTESIAN_POINT('Ctrl Pts',(-20.1424108759181,-20.532832482389,-1.97986538399193));
#77561=CARTESIAN_POINT('Ctrl Pts',(-20.1190797257721,-20.5533140988938,
-1.97793603921231));
#77562=CARTESIAN_POINT('Ctrl Pts',(-20.0837081766672,-20.5830138448141,
-1.97509657056978));
#77563=CARTESIAN_POINT('Ctrl Pts',(-20.07200638745,-20.5926270904666,-1.97417061497426));
#77564=CARTESIAN_POINT('Ctrl Pts',(-20.053101282801,-20.6078211857509,-1.97269574460927));
#77565=CARTESIAN_POINT('Ctrl Pts',(-20.0459635052767,-20.6134823978489,
-1.9721436156328));
#77566=CARTESIAN_POINT('Ctrl Pts',(-20.0322804493069,-20.6241917331012,
-1.97109407224112));
#77567=CARTESIAN_POINT('Ctrl Pts',(-20.0257417314927,-20.629247930227,-1.97059634135207));
#77568=CARTESIAN_POINT('Ctrl Pts',(-20.0142131900203,-20.6380552045011,
-1.96972538585768));
#77569=CARTESIAN_POINT('Ctrl Pts',(-20.0092361076183,-20.6418227231423,
-1.96935151439972));
#77570=CARTESIAN_POINT('Ctrl Pts',(-19.9993807200469,-20.6492146492863,
-1.96861535962426));
#77571=CARTESIAN_POINT('Ctrl Pts',(-19.9945033299632,-20.6528401714315,
-1.96825303480688));
#77572=CARTESIAN_POINT('Ctrl Pts',(-19.9828022176899,-20.6614600099083,
-1.96738851373889));
#77573=CARTESIAN_POINT('Ctrl Pts',(-19.9759640172694,-20.6664345678222,
-1.96688708763631));
#77574=CARTESIAN_POINT('Ctrl Pts',(-19.951156598313,-20.6842548049735,-1.96508152989753));
#77575=CARTESIAN_POINT('Ctrl Pts',(-19.9330160197317,-20.6968603189806,
-1.96378661516836));
#77576=CARTESIAN_POINT('Ctrl Pts',(-19.7605316039865,-20.8127557130371,
-1.95170046419682));
#77577=CARTESIAN_POINT('Ctrl Pts',(-19.5934291011689,-20.8955963013441,
-1.94176724924772));
#77578=CARTESIAN_POINT('Ctrl Pts',(-19.3418755601045,-20.9814300818394,
-1.92727730385095));
#77579=CARTESIAN_POINT('Ctrl Pts',(-19.2647017150212,-21.0029638809598,
-1.92287411277622));
#77580=CARTESIAN_POINT('Ctrl Pts',(-19.1513240644229,-21.0277712470727,
-1.91623522899354));
#77581=CARTESIAN_POINT('Ctrl Pts',(-19.1159589849224,-21.0345687577443,
-1.91414068824534));
#77582=CARTESIAN_POINT('Ctrl Pts',(-19.0730758941525,-21.0416823356312,
-1.91155379071));
#77583=CARTESIAN_POINT('Ctrl Pts',(-19.0657052693835,-21.0428649732448,
-1.91110749168472));
#77584=CARTESIAN_POINT('Ctrl Pts',(-19.0542187151086,-21.0446457588916,
-1.91040915479717));
#77585=CARTESIAN_POINT('Ctrl Pts',(-19.0501069330924,-21.0452708147491,
-1.9101586142393));
#77586=CARTESIAN_POINT('Ctrl Pts',(-19.0424663468632,-21.0464092792429,
-1.90969197025716));
#77587=CARTESIAN_POINT('Ctrl Pts',(-19.0389380777652,-21.046925889918,-1.90947605030773));
#77588=CARTESIAN_POINT('Ctrl Pts',(-19.0309434826086,-21.0480758376547,
-1.90898582900953));
#77589=CARTESIAN_POINT('Ctrl Pts',(-19.026476449865,-21.0487038118119,-1.90871122998497));
#77590=CARTESIAN_POINT('Ctrl Pts',(-19.0149365151976,-21.0502884968433,
-1.9080001362419));
#77591=CARTESIAN_POINT('Ctrl Pts',(-19.0078607872201,-21.0512237154404,
-1.90756247410033));
#77592=CARTESIAN_POINT('Ctrl Pts',(-18.9643580473622,-21.056749908699,-1.90486206382203));
#77593=CARTESIAN_POINT('Ctrl Pts',(-18.9278237679634,-21.0604280827711,
-1.90255300475009));
#77594=CARTESIAN_POINT('Ctrl Pts',(-18.7213462194097,-21.075804206797,-1.88933906323761));
#77595=CARTESIAN_POINT('Ctrl Pts',(-18.5505732804184,-21.0679069289307,
-1.87784579016391));
#77596=CARTESIAN_POINT('Ctrl Pts',(-18.288426158339,-21.0237796023901,-1.86056924249069));
#77597=CARTESIAN_POINT('Ctrl Pts',(-18.1954346426859,-21.00157517292,-1.85450219355194));
#77598=CARTESIAN_POINT('Ctrl Pts',(-18.0838141290484,-20.966796629113,-1.84732064884633));
#77599=CARTESIAN_POINT('Ctrl Pts',(-18.0634764335022,-20.9601198477793,
-1.84601599339661));
#77600=CARTESIAN_POINT('Ctrl Pts',(-18.0347242032187,-20.9501950792171,
-1.84417645125597));
#77601=CARTESIAN_POINT('Ctrl Pts',(-18.0262242790272,-20.94720017725,-1.84363324546491));
#77602=CARTESIAN_POINT('Ctrl Pts',(-18.0116017707027,-20.941942812525,-1.84269974461762));
#77603=CARTESIAN_POINT('Ctrl Pts',(-18.0054700997176,-20.9397061615559,
-1.84230859794233));
#77604=CARTESIAN_POINT('Ctrl Pts',(-17.9937551270939,-20.935371397761,-1.84156182277498));
#77605=CARTESIAN_POINT('Ctrl Pts',(-17.9881701658856,-20.9332779797359,
-1.84120604210323));
#77606=CARTESIAN_POINT('Ctrl Pts',(-17.9736824205417,-20.9277775794377,
-1.84028369350109));
#77607=CARTESIAN_POINT('Ctrl Pts',(-17.9647936043243,-20.9243339956537,
-1.83971835628536));
#77608=CARTESIAN_POINT('Ctrl Pts',(-17.9346247699119,-20.9124114260076,
-1.83780125513713));
#77609=CARTESIAN_POINT('Ctrl Pts',(-17.9134587713652,-20.9036469634844,
-1.8364591005122));
#77610=CARTESIAN_POINT('Ctrl Pts',(-17.730397719994,-20.8243399290242,-1.82486537947046));
#77611=CARTESIAN_POINT('Ctrl Pts',(-17.577778751225,-20.734142928077,-1.8153758609545));
#77612=CARTESIAN_POINT('Ctrl Pts',(-17.3699361942469,-20.5732507793918,
-1.80107191152797));
#77613=CARTESIAN_POINT('Ctrl Pts',(-17.3050449697912,-20.5163558826288,
-1.7963489923218));
#77614=CARTESIAN_POINT('Ctrl Pts',(-17.2170838455513,-20.4291831592641,
-1.78927699853988));
#77615=CARTESIAN_POINT('Ctrl Pts',(-17.1910715232213,-20.4019917336887,
-1.7870910913466));
#77616=CARTESIAN_POINT('Ctrl Pts',(-17.1607205265127,-20.3685231584339,
-1.78440287333128));
#77617=CARTESIAN_POINT('Ctrl Pts',(-17.1556718303541,-20.3628955826249,
-1.78395093746037));
#77618=CARTESIAN_POINT('Ctrl Pts',(-17.1478789475879,-20.3541150017325,
-1.78324568424477));
#77619=CARTESIAN_POINT('Ctrl Pts',(-17.1451137141005,-20.3509806434598,
-1.78299391256094));
#77620=CARTESIAN_POINT('Ctrl Pts',(-17.1400079158395,-20.3451586189318,
-1.78252616633747));
#77621=CARTESIAN_POINT('Ctrl Pts',(-17.1376648487835,-20.342473223862,-1.78231038280618));
#77622=CARTESIAN_POINT('Ctrl Pts',(-17.1323896226924,-20.3363963661908,
-1.78182200170695));
#77623=CARTESIAN_POINT('Ctrl Pts',(-17.1294614661708,-20.3330015177484,
-1.78154911600803));
#77624=CARTESIAN_POINT('Ctrl Pts',(-17.1208694787161,-20.3229759179436,
-1.78074315403428));
#77625=CARTESIAN_POINT('Ctrl Pts',(-17.115235889878,-20.3163195359043,-1.78020794081838));
#77626=CARTESIAN_POINT('Ctrl Pts',(-17.0754251888519,-20.2686873928663,
-1.77637848201504));
#77627=CARTESIAN_POINT('Ctrl Pts',(-17.0427697643961,-20.226470614844,-1.77298712418771));
#77628=CARTESIAN_POINT('Ctrl Pts',(-17.0014762191369,-20.168701394637,-1.76839776225945));
#77629=CARTESIAN_POINT('Ctrl Pts',(-16.9913860734998,-20.1542053126184,
-1.76725022502634));
#77630=CARTESIAN_POINT('Ctrl Pts',(-16.9543026867097,-20.0994812912088,
-1.76293769807455));
#77631=CARTESIAN_POINT('Ctrl Pts',(-16.9285119216045,-20.058457591769,-1.75974409731762));
#77632=CARTESIAN_POINT('Ctrl Pts',(-16.849146026128,-19.9220407382868,-1.74931865084814));
#77633=CARTESIAN_POINT('Ctrl Pts',(-16.8015463320435,-19.8233666414338,
-1.742085863055));
#77634=CARTESIAN_POINT('Ctrl Pts',(-16.7417568175448,-19.6701171705583,
-1.73151222865472));
#77635=CARTESIAN_POINT('Ctrl Pts',(-16.7237400582286,-19.6180187356863,
-1.72802300287674));
#77636=CARTESIAN_POINT('Ctrl Pts',(-16.6978381781391,-19.5324401562204,
-1.72246531640385));
#77637=CARTESIAN_POINT('Ctrl Pts',(-16.6886998391823,-19.4993693526762,
-1.72035841402675));
#77638=CARTESIAN_POINT('Ctrl Pts',(-16.6777441292952,-19.4556046220498,
-1.71762185256941));
#77639=CARTESIAN_POINT('Ctrl Pts',(-16.6751997329276,-19.4450996737436,
-1.71696885089705));
#77640=CARTESIAN_POINT('Ctrl Pts',(-16.6711634629899,-19.4278592259875,
-1.71590335916471));
#77641=CARTESIAN_POINT('Ctrl Pts',(-16.6696238845251,-19.4211352011839,
-1.7154893396334));
#77642=CARTESIAN_POINT('Ctrl Pts',(-16.6667069027187,-19.4081029904322,
-1.71468983673421));
#77643=CARTESIAN_POINT('Ctrl Pts',(-16.6653254418001,-19.4017957999248,
-1.71430422701255));
#77644=CARTESIAN_POINT('Ctrl Pts',(-16.6622017609047,-19.3872155026155,
-1.7134158266876));
#77645=CARTESIAN_POINT('Ctrl Pts',(-16.6604801942873,-19.378938046695,-1.71291370211267));
#77646=CARTESIAN_POINT('Ctrl Pts',(-16.6559824447547,-19.3566433286995,
-1.71156713494216));
#77647=CARTESIAN_POINT('Ctrl Pts',(-16.6532984879279,-19.3426077520206,
-1.710725633561));
#77648=CARTESIAN_POINT('Ctrl Pts',(-16.6299803466818,-19.2135999198293,
-1.70304546140456));
#77649=CARTESIAN_POINT('Ctrl Pts',(-16.6187512461435,-19.0971247379113,
-1.69652331624241));
#77650=CARTESIAN_POINT('Ctrl Pts',(-16.6150141574696,-18.8176357478624,
-1.68122134773218));
#77651=CARTESIAN_POINT('Ctrl Pts',(-16.6315967213824,-18.6552789540971,
-1.67262441655658));
#77652=CARTESIAN_POINT('Ctrl Pts',(-16.6736069919899,-18.4646285363578,
-1.6614158197078));
#77653=CARTESIAN_POINT('Ctrl Pts',(-16.6813503331717,-18.4329822994738,
-1.65951585324633));
#77654=CARTESIAN_POINT('Ctrl Pts',(-16.6917038813867,-18.3945342674246,
-1.6571450963628));
#77655=CARTESIAN_POINT('Ctrl Pts',(-16.693623420371,-18.3875490376032,-1.65671183579415));
#77656=CARTESIAN_POINT('Ctrl Pts',(-16.6966883047469,-18.376615820509,-1.65602951244593));
#77657=CARTESIAN_POINT('Ctrl Pts',(-16.697809383091,-18.3726610072034,-1.65578183773681));
#77658=CARTESIAN_POINT('Ctrl Pts',(-16.6999260702594,-18.3652760396696,
-1.6553176910471));
#77659=CARTESIAN_POINT('Ctrl Pts',(-16.7009188438121,-18.3618451313637,
-1.6551013848204));
#77660=CARTESIAN_POINT('Ctrl Pts',(-16.7032044325518,-18.3540206205047,
-1.65460654986977));
#77661=CARTESIAN_POINT('Ctrl Pts',(-16.7045028212763,-18.3496287061034,
-1.65432769981613));
#77662=CARTESIAN_POINT('Ctrl Pts',(-16.7085359774964,-18.3361472639435,
-1.65346843807196));
#77663=CARTESIAN_POINT('Ctrl Pts',(-16.7113175908226,-18.3270720338653,
-1.65288539238236));
#77664=CARTESIAN_POINT('Ctrl Pts',(-16.7367707030987,-18.2459797455049,
-1.64763601863469));
#77665=CARTESIAN_POINT('Ctrl Pts',(-16.7632164951043,-18.1752121733009,
-1.64277665110504));
#77666=CARTESIAN_POINT('Ctrl Pts',(-16.8475005998302,-17.9818711473493,
-1.62898457159768));
#77667=CARTESIAN_POINT('Ctrl Pts',(-16.9134127660971,-17.863195252135,-1.61993219658966));
#77668=CARTESIAN_POINT('Ctrl Pts',(-17.041206518941,-17.6775479604834,-1.6053260997555));
#77669=CARTESIAN_POINT('Ctrl Pts',(-17.0968763104419,-17.6067835132174,
-1.59962665350095));
#77670=CARTESIAN_POINT('Ctrl Pts',(-17.170716119228,-17.5243227584686,-1.59283208250353));
#77671=CARTESIAN_POINT('Ctrl Pts',(-17.1847724627518,-17.5090818167031,
-1.59156897800392));
#77672=CARTESIAN_POINT('Ctrl Pts',(-17.2051781508662,-17.4875984456937,
-1.58977741907538));
#77673=CARTESIAN_POINT('Ctrl Pts',(-17.2113461565476,-17.4811861316128,
-1.58924122423206));
#77674=CARTESIAN_POINT('Ctrl Pts',(-17.2220942905375,-17.4701523507733,
-1.58831597872501));
#77675=CARTESIAN_POINT('Ctrl Pts',(-17.2266556019151,-17.4655127996336,
-1.58792611600589));
#77676=CARTESIAN_POINT('Ctrl Pts',(-17.2354566220657,-17.4566429815126,
-1.58717918400606));
#77677=CARTESIAN_POINT('Ctrl Pts',(-17.2396930294272,-17.4524095402002,
-1.58682197507435));
#77678=CARTESIAN_POINT('Ctrl Pts',(-17.2508148454768,-17.4413894403611,
-1.58589021910236));
#77679=CARTESIAN_POINT('Ctrl Pts',(-17.2577289288232,-17.434631819693,-1.58531695388658));
#77680=CARTESIAN_POINT('Ctrl Pts',(-17.2817684682588,-17.4114561361086,
-1.58334401763752));
#77681=CARTESIAN_POINT('Ctrl Pts',(-17.2991238359299,-17.3952783553431,
-1.58195474199971));
#77682=CARTESIAN_POINT('Ctrl Pts',(-17.4372484007768,-17.2707986906363,
-1.57115794072198));
#77683=CARTESIAN_POINT('Ctrl Pts',(-17.5698311025968,-17.1764098680476,
-1.56237647059935));
#77684=CARTESIAN_POINT('Ctrl Pts',(-17.8260773644939,-17.0351372980038,
-1.54648015492268));
#77685=CARTESIAN_POINT('Ctrl Pts',(-17.9458033605028,-16.9828828586032,
-1.53938988112134));
#77686=CARTESIAN_POINT('Ctrl Pts',(-18.0808437687644,-16.9382429733636,
-1.53099659419024));
#77687=CARTESIAN_POINT('Ctrl Pts',(-18.0921660077211,-16.9346057558173,
-1.53028986634222));
#77688=CARTESIAN_POINT('Ctrl Pts',(-18.1083101308925,-16.9295691884824,
-1.52927710045089));
#77689=CARTESIAN_POINT('Ctrl Pts',(-18.1131075134792,-16.9280912276785,
-1.528975515019));
#77690=CARTESIAN_POINT('Ctrl Pts',(-18.1213859413958,-16.925573042289,-1.52845393404589));
#77691=CARTESIAN_POINT('Ctrl Pts',(-18.1248645276573,-16.9245246793309,
-1.52823441316264));
#77692=CARTESIAN_POINT('Ctrl Pts',(-18.1316161213705,-16.9225088541225,
-1.52780763364235));
#77693=CARTESIAN_POINT('Ctrl Pts',(-18.1348887764096,-16.9215403501145,
-1.52760044324629));
#77694=CARTESIAN_POINT('Ctrl Pts',(-18.1437280857569,-16.9189476905458,
-1.52703999354796));
#77695=CARTESIAN_POINT('Ctrl Pts',(-18.1492990466822,-16.9173385001205,
-1.52668587665264));
#77696=CARTESIAN_POINT('Ctrl Pts',(-18.1700200047351,-16.9114453104256,
-1.52536561859706));
#77697=CARTESIAN_POINT('Ctrl Pts',(-18.1852106047553,-16.9073075922571,
-1.52439152156402));
#77698=CARTESIAN_POINT('Ctrl Pts',(-18.3278408526358,-16.870160864034,-1.51519649801879));
#77699=CARTESIAN_POINT('Ctrl Pts',(-18.4580418341895,-16.8489402244129,
-1.50645731733271));
#77700=CARTESIAN_POINT('Ctrl Pts',(-18.7482991390137,-16.8290619672997,
-1.487239119146));
#77701=CARTESIAN_POINT('Ctrl Pts',(-18.9079913130624,-16.8361513367251,
-1.47686732231346));
#77702=CARTESIAN_POINT('Ctrl Pts',(-19.0864171272193,-16.8644310703918,
-1.46577186590442));
#77703=CARTESIAN_POINT('Ctrl Pts',(-19.1073845944292,-16.8680792088082,
-1.46447482370769));
#77704=CARTESIAN_POINT('Ctrl Pts',(-19.1371281389595,-16.8737176447483,
-1.46264404197272));
#77705=CARTESIAN_POINT('Ctrl Pts',(-19.1459515159648,-16.8754485807078,
-1.46210209142977));
#77706=CARTESIAN_POINT('Ctrl Pts',(-19.1611568616866,-16.8785322358493,
-1.46117005519189));
#77707=CARTESIAN_POINT('Ctrl Pts',(-19.1675440460578,-16.8798583264978,
-1.46077912511099));
#77708=CARTESIAN_POINT('Ctrl Pts',(-19.179763779525,-16.8824543295307,-1.46003229214783));
#77709=CARTESIAN_POINT('Ctrl Pts',(-19.185597277295,-16.8837194267803,-1.45967623934523));
#77710=CARTESIAN_POINT('Ctrl Pts',(-19.2007565986014,-16.8870741869795,
-1.45875216575367));
#77711=CARTESIAN_POINT('Ctrl Pts',(-19.2100738278235,-16.8892023728368,
-1.45818538481364));
#77712=CARTESIAN_POINT('Ctrl Pts',(-19.2418171654502,-16.8966795253776,
-1.45625815048359));
#77713=CARTESIAN_POINT('Ctrl Pts',(-19.2641706545985,-16.9023318157934,
-1.45490744634196));
#77714=CARTESIAN_POINT('Ctrl Pts',(-19.4549976985346,-16.953915070331,-1.44342150463895));
#77715=CARTESIAN_POINT('Ctrl Pts',(-19.6172807621166,-17.0201607465475,
-1.43402853690495));
#77716=CARTESIAN_POINT('Ctrl Pts',(-19.8460091767101,-17.1484479468382,
-1.41976125585502));
#77717=CARTESIAN_POINT('Ctrl Pts',(-19.9196806860506,-17.1960036168401,
-1.41496687862995));
#77718=CARTESIAN_POINT('Ctrl Pts',(-20.0207562178372,-17.2705156446807,
-1.40779853363121));
#77719=CARTESIAN_POINT('Ctrl Pts',(-20.050710172864,-17.2938669781061,-1.40559284897915));
#77720=CARTESIAN_POINT('Ctrl Pts',(-20.0858688090117,-17.3228292943661,
-1.40288270525609));
#77721=CARTESIAN_POINT('Ctrl Pts',(-20.0916937757686,-17.3276804279405,
-1.40242958083281));
#77722=CARTESIAN_POINT('Ctrl Pts',(-20.1006932809881,-17.3352576013287,
-1.40172286696889));
#77723=CARTESIAN_POINT('Ctrl Pts',(-20.1038860708932,-17.3379620016751,
-1.40147083342189));
#77724=CARTESIAN_POINT('Ctrl Pts',(-20.1097830114752,-17.342987009666,-1.40100286219437));
#77725=CARTESIAN_POINT('Ctrl Pts',(-20.1124893284976,-17.3453049858886,
-1.40078711718446));
#77726=CARTESIAN_POINT('Ctrl Pts',(-20.118582736565,-17.3505507532902,-1.40029915277496));
#77727=CARTESIAN_POINT('Ctrl Pts',(-20.1219663794784,-17.3534824452741,
-1.4000266473414));
#77728=CARTESIAN_POINT('Ctrl Pts',(-20.1318927169114,-17.3621382059273,
-1.3992227406268));
#77729=CARTESIAN_POINT('Ctrl Pts',(-20.138409390065,-17.367891786714,-1.39868921784563));
#77730=CARTESIAN_POINT('Ctrl Pts',(-20.1842716029898,-17.4088890282016,
-1.39489468584104));
#77731=CARTESIAN_POINT('Ctrl Pts',(-20.2223180985812,-17.4455513876767,
-1.39153847472474));
#77732=CARTESIAN_POINT('Ctrl Pts',(-20.2724921201232,-17.4976574855266,
-1.38686505684447));
#77733=CARTESIAN_POINT('Ctrl Pts',(-20.2858384035778,-17.5119070552806,
-1.38559624901655));
#77734=CARTESIAN_POINT('Ctrl Pts',(-20.397595909335,-17.6345861820864,-1.37476371728557));
#77735=CARTESIAN_POINT('Ctrl Pts',(-20.4847190246882,-17.7527841633212,
-1.3649584311791));
#77736=CARTESIAN_POINT('Ctrl Pts',(-20.5902290778054,-17.9322388444991,
-1.35150933953882));
#77737=CARTESIAN_POINT('Ctrl Pts',(-20.6191743280918,-17.9867963515892,
-1.34758323029188));
#77738=CARTESIAN_POINT('Ctrl Pts',(-20.6616864855659,-18.0761579328442,
-1.34141723280114));
#77739=CARTESIAN_POINT('Ctrl Pts',(-20.6767885701733,-18.1101880490366,
-1.3391275721287));
#77740=CARTESIAN_POINT('Ctrl Pts',(-20.6952311453368,-18.1548894204109,
-1.33619300060901));
#77741=CARTESIAN_POINT('Ctrl Pts',(-20.6993949332349,-18.1652118167138,
-1.33552031141605));
#77742=CARTESIAN_POINT('Ctrl Pts',(-20.7060328960241,-18.1820494725962,
-1.33443094956885));
#77743=CARTESIAN_POINT('Ctrl Pts',(-20.7085566090558,-18.1885448558746,
-1.3340126126734));
#77744=CARTESIAN_POINT('Ctrl Pts',(-20.7133473748445,-18.2010577141666,
-1.33321032421712));
#77745=CARTESIAN_POINT('Ctrl Pts',(-20.7156191687908,-18.207073279949,-1.33282621705269));
#77746=CARTESIAN_POINT('Ctrl Pts',(-20.7207568509151,-18.2208673638336,
-1.33194903142352));
#77747=CARTESIAN_POINT('Ctrl Pts',(-20.7236045418523,-18.2286525825372,
-1.33145656532494));
#77748=CARTESIAN_POINT('Ctrl Pts',(-20.7310458567812,-18.2493726096214,
-1.33015267371095));
#77749=CARTESIAN_POINT('Ctrl Pts',(-20.7355595833636,-18.262335841672,-1.32934390222874));
#77750=CARTESIAN_POINT('Ctrl Pts',(-20.768858789551,-18.3610511026393,-1.32323614162636));
#77751=CARTESIAN_POINT('Ctrl Pts',(-20.7922497677207,-18.4485303721536,
-1.31812045243364));
#77752=CARTESIAN_POINT('Ctrl Pts',(-20.8373639019983,-18.6743412751769,
-1.30537420899799));
#77753=CARTESIAN_POINT('Ctrl Pts',(-20.8511051846576,-18.813805234618,-1.29793914602196));
#77754=CARTESIAN_POINT('Ctrl Pts',(-20.850984040619,-18.9738904697264,-1.28909422412968));
#77755=CARTESIAN_POINT('Ctrl Pts',(-20.8506770343583,-18.9941772551681,
-1.28796714642275));
#77756=CARTESIAN_POINT('Ctrl Pts',(-20.8483264232153,-19.0738184747613,
-1.2835078783363));
#77757=CARTESIAN_POINT('Ctrl Pts',(-20.8440773310445,-19.1330752901755,
-1.28011463463512));
#77758=CARTESIAN_POINT('Ctrl Pts',(-20.836329718907,-19.2009553113883,-1.27606208409883));
#77759=CARTESIAN_POINT('Ctrl Pts',(-20.8352591869441,-19.209834863776,-1.27552867654599));
#77760=CARTESIAN_POINT('Ctrl Pts',(-20.8335616366235,-19.2232018844552,
-1.27472039173358));
#77761=CARTESIAN_POINT('Ctrl Pts',(-20.8329764090901,-19.2276946885955,
-1.27444781320648));
#77762=CARTESIAN_POINT('Ctrl Pts',(-20.831904658458,-19.2357212866073,-1.2739591658741));
#77763=CARTESIAN_POINT('Ctrl Pts',(-20.8314236225286,-19.2392557603419,
-1.27374340933918));
#77764=CARTESIAN_POINT('Ctrl Pts',(-20.830364447558,-19.2468936671231,-1.27327589048336));
#77765=CARTESIAN_POINT('Ctrl Pts',(-20.8297832007567,-19.2509965662683,
-1.27302395992035));
#77766=CARTESIAN_POINT('Ctrl Pts',(-20.8281309522132,-19.2624178821841,
-1.27232050370401));
#77767=CARTESIAN_POINT('Ctrl Pts',(-20.8270336493153,-19.2697323491824,
-1.2718675311357));
#77768=CARTESIAN_POINT('Ctrl Pts',(-20.8205389602655,-19.3115308797211,
-1.26926550463275));
#77769=CARTESIAN_POINT('Ctrl Pts',(-20.8143280491217,-19.3458809039005,
-1.26707454839359));
#77770=CARTESIAN_POINT('Ctrl Pts',(-20.791895818292,-19.4545296439919,-1.26000957896572));
#77771=CARTESIAN_POINT('Ctrl Pts',(-20.7725200301541,-19.5281126177893,
-1.25502394121134));
#77772=CARTESIAN_POINT('Ctrl Pts',(-20.7408447920318,-19.6265459931844,
-1.24820178648662));
#77773=CARTESIAN_POINT('Ctrl Pts',(-20.7319594894793,-19.6524245799638,
-1.2463931639016));
#77774=CARTESIAN_POINT('Ctrl Pts',(-20.7225806439552,-19.6781101999604,
-1.24458624895942));
#77775=CARTESIAN_POINT('Origin',(-18.734,-18.952,0.));
#77776=CARTESIAN_POINT('',(-20.7225805821191,-19.6781103693095,-0.444429623604461));
#77777=CARTESIAN_POINT('',(-20.7225805821191,-19.6781103693095,-0.666446455478431));
#77778=CARTESIAN_POINT('',(-20.7225805821191,-19.6781103693095,0.));
#77779=CARTESIAN_POINT('',(-17.1140743056112,-17.5890877707427,0.));
#77780=CARTESIAN_POINT('Ctrl Pts',(-20.7225805821191,-19.6781103693095,
-0.444429623604461));
#77781=CARTESIAN_POINT('Ctrl Pts',(-20.6978890887291,-19.7457323540302,
-0.440115259735745));
#77782=CARTESIAN_POINT('Ctrl Pts',(-20.66973990691,-19.8121053494161,-0.435800895867028));
#77783=CARTESIAN_POINT('Ctrl Pts',(-20.6382937703335,-19.8768536296458,
-0.431486531998312));
#77784=CARTESIAN_POINT('Ctrl Pts',(-20.6068209446005,-19.94165686343,-0.427168506416429));
#77785=CARTESIAN_POINT('Ctrl Pts',(-20.5720457909348,-20.00483217924,-0.422850480834545));
#77786=CARTESIAN_POINT('Ctrl Pts',(-20.5341758415686,-20.0660269024726,
-0.418532455252662));
#77787=CARTESIAN_POINT('Ctrl Pts',(-20.4962904232958,-20.127246622186,-0.41421266586766));
#77788=CARTESIAN_POINT('Ctrl Pts',(-20.4553079752336,-20.1864837294646,
-0.409892876482659));
#77789=CARTESIAN_POINT('Ctrl Pts',(-20.4114787744278,-20.2434154874959,
-0.405573087097658));
#77790=CARTESIAN_POINT('Ctrl Pts',(-20.3675728005617,-20.3004469695743,
-0.401245730988999));
#77791=CARTESIAN_POINT('Ctrl Pts',(-20.3208104379345,-20.3551646589689,
-0.39691837488034));
#77792=CARTESIAN_POINT('Ctrl Pts',(-20.271481107869,-20.4072803313953,-0.392591018771681));
#77793=CARTESIAN_POINT('Ctrl Pts',(-20.2294415884618,-20.4516944318802,
-0.388903152529222));
#77794=CARTESIAN_POINT('Ctrl Pts',(-20.1855384971826,-20.4942192435085,
-0.385215286286762));
#77795=CARTESIAN_POINT('Ctrl Pts',(-20.1399695482849,-20.534699791273,-0.381527420044303));
#77796=CARTESIAN_POINT('Ctrl Pts',(-20.0856805306588,-20.5829266919205,
-0.377133844149252));
#77797=CARTESIAN_POINT('Ctrl Pts',(-20.0288042210985,-20.628448612849,-0.372740268254202));
#77798=CARTESIAN_POINT('Ctrl Pts',(-19.9696409341316,-20.6709765797993,
-0.368346692359152));
#77799=CARTESIAN_POINT('Ctrl Pts',(-19.9105639455,-20.7134425134695,-0.363959525139234));
#77800=CARTESIAN_POINT('Ctrl Pts',(-19.8492069897094,-20.7529228848838,
-0.359572357919316));
#77801=CARTESIAN_POINT('Ctrl Pts',(-19.7859047362903,-20.7891677728967,
-0.355185190699398));
#77802=CARTESIAN_POINT('Ctrl Pts',(-19.722674949545,-20.8253711687613,-0.350803045787515));
#77803=CARTESIAN_POINT('Ctrl Pts',(-19.65750470457,-20.8583462016274,-0.346420900875633));
#77804=CARTESIAN_POINT('Ctrl Pts',(-19.5907576513137,-20.8878861864571,
-0.34203875596375));
#77805=CARTESIAN_POINT('Ctrl Pts',(-19.5240517390545,-20.9174079636751,
-0.337659312082134));
#77806=CARTESIAN_POINT('Ctrl Pts',(-19.4557713858207,-20.9434987000513,
-0.333279868200517));
#77807=CARTESIAN_POINT('Ctrl Pts',(-19.38630358708,-20.9659982696821,-0.328900424318901));
#77808=CARTESIAN_POINT('Ctrl Pts',(-19.3168558633838,-20.9884913373096,
-0.324522246024118));
#77809=CARTESIAN_POINT('Ctrl Pts',(-19.2462218327665,-21.0073951506619,
-0.320144067729335));
#77810=CARTESIAN_POINT('Ctrl Pts',(-19.1748055877232,-21.0225988104488,
-0.315765889434552));
#77811=CARTESIAN_POINT('Ctrl Pts',(-19.1033866007398,-21.0378030539618,
-0.311387543044916));
#77812=CARTESIAN_POINT('Ctrl Pts',(-19.0311858104649,-21.0493067636484,
-0.30700919665528));
#77813=CARTESIAN_POINT('Ctrl Pts',(-18.9586178566871,-21.0570500750475,
-0.302630850265644));
#77814=CARTESIAN_POINT('Ctrl Pts',(-18.8859739522816,-21.0648014907037,
-0.298247921437905));
#77815=CARTESIAN_POINT('Ctrl Pts',(-18.8129625963386,-21.0687845992062,
-0.293864992610166));
#77816=CARTESIAN_POINT('Ctrl Pts',(-18.7400030989877,-21.0689914885995,
-0.289482063782427));
#77817=CARTESIAN_POINT('Ctrl Pts',(-18.6670032476661,-21.0691984924235,
-0.285096710752382));
#77818=CARTESIAN_POINT('Ctrl Pts',(-18.5940557926886,-21.0656251419751,
-0.280711357722337));
#77819=CARTESIAN_POINT('Ctrl Pts',(-18.5215768813659,-21.0583156028169,
-0.276326004692292));
#77820=CARTESIAN_POINT('Ctrl Pts',(-18.4489698822544,-21.0509931459328,
-0.271932901681429));
#77821=CARTESIAN_POINT('Ctrl Pts',(-18.3768335560974,-21.039921387774,-0.267539798670566));
#77822=CARTESIAN_POINT('Ctrl Pts',(-18.3055752234051,-21.0251958930115,
-0.263146695659703));
#77823=CARTESIAN_POINT('Ctrl Pts',(-18.2580216757331,-21.0153689788707,
-0.260215001560758));
#77824=CARTESIAN_POINT('Ctrl Pts',(-18.210858896598,-21.0039159582902,-0.257283307461813));
#77825=CARTESIAN_POINT('Ctrl Pts',(-18.164203666426,-20.9908774210937,-0.254351613362869));
#77826=CARTESIAN_POINT('Ctrl Pts',(-18.0951064200439,-20.9715671098208,
-0.250009720959284));
#77827=CARTESIAN_POINT('Ctrl Pts',(-18.0268407868783,-20.9486978630522,
-0.245667828555699));
#77828=CARTESIAN_POINT('Ctrl Pts',(-17.9598054524231,-20.922358292926,-0.241325936152114));
#77829=CARTESIAN_POINT('Ctrl Pts',(-17.8928710627946,-20.8960583861112,
-0.236990581965715));
#77830=CARTESIAN_POINT('Ctrl Pts',(-17.8271637514137,-20.8662987014601,
-0.232655227779317));
#77831=CARTESIAN_POINT('Ctrl Pts',(-17.763068724128,-20.8332180781434,-0.228319873592918));
#77832=CARTESIAN_POINT('Ctrl Pts',(-17.699047363678,-20.8001754756366,-0.223989502192827));
#77833=CARTESIAN_POINT('Ctrl Pts',(-17.6366350451716,-20.7638197356247,
-0.219659130792735));
#77834=CARTESIAN_POINT('Ctrl Pts',(-17.5761969042586,-20.7243377193672,
-0.215328759392644));
#77835=CARTESIAN_POINT('Ctrl Pts',(-17.5157959073165,-20.6848799679007,
-0.211001049344912));
#77836=CARTESIAN_POINT('Ctrl Pts',(-17.457367094634,-20.6423000184136,-0.206673339297181));
#77837=CARTESIAN_POINT('Ctrl Pts',(-17.4012494835622,-20.5968297969501,
-0.202345629249449));
#77838=CARTESIAN_POINT('Ctrl Pts',(-17.3451469193491,-20.5513717674523,
-0.198019079593976));
#77839=CARTESIAN_POINT('Ctrl Pts',(-17.2913547105839,-20.5030253137849,
-0.193692529938503));
#77840=CARTESIAN_POINT('Ctrl Pts',(-17.2401799611388,-20.4520635624855,
-0.18936598028303));
#77841=CARTESIAN_POINT('Ctrl Pts',(-17.1890012037485,-20.4010978199226,
-0.185039091777358));
#77842=CARTESIAN_POINT('Ctrl Pts',(-17.1404406606225,-20.3475167229364,
-0.180712203271685));
#77843=CARTESIAN_POINT('Ctrl Pts',(-17.0947683110377,-20.2916299749938,
-0.176385314766013));
#77844=CARTESIAN_POINT('Ctrl Pts',(-17.0490411502534,-20.2356761575941,
-0.172053233579186));
#77845=CARTESIAN_POINT('Ctrl Pts',(-17.0062094147358,-20.1774115489121,
-0.167721152392358));
#77846=CARTESIAN_POINT('Ctrl Pts',(-16.9665019464716,-20.1171779395326,
-0.16338907120553));
#77847=CARTESIAN_POINT('Ctrl Pts',(-16.9267699714228,-20.0569071549778,
-0.159054316330717));
#77848=CARTESIAN_POINT('Ctrl Pts',(-16.8901663478009,-19.9946653786934,
-0.154719561455904));
#77849=CARTESIAN_POINT('Ctrl Pts',(-16.8568742859376,-19.9308197247736,
-0.150384806581091));
#77850=CARTESIAN_POINT('Ctrl Pts',(-16.8235151748393,-19.8668454875814,
-0.146041321637236));
#77851=CARTESIAN_POINT('Ctrl Pts',(-16.793481145719,-19.8012613727176,-0.141697836693382));
#77852=CARTESIAN_POINT('Ctrl Pts',(-16.7669073048299,-19.7344546815047,
-0.137354351749528));
#77853=CARTESIAN_POINT('Ctrl Pts',(-16.7461495461317,-19.6822696330047,
-0.133961503393496));
#77854=CARTESIAN_POINT('Ctrl Pts',(-16.7275021235515,-19.6293390357121,
-0.130568655037465));
#77855=CARTESIAN_POINT('Ctrl Pts',(-16.7110078198973,-19.5758522575445,
-0.127175806681434));
#77856=CARTESIAN_POINT('Ctrl Pts',(-16.6890805816263,-19.5047478718232,
-0.122665413525099));
#77857=CARTESIAN_POINT('Ctrl Pts',(-16.670871275646,-19.4323727566685,-0.118155020368764));
#77858=CARTESIAN_POINT('Ctrl Pts',(-16.6565191765188,-19.3591393226743,
-0.113644627212429));
#77859=CARTESIAN_POINT('Ctrl Pts',(-16.641451763523,-19.2822559075513,-0.108909434411911));
#77860=CARTESIAN_POINT('Ctrl Pts',(-16.6306362897029,-19.2044268305763,
-0.104174241611394));
#77861=CARTESIAN_POINT('Ctrl Pts',(-16.6241750766647,-19.1261487664996,
-0.0994390488108757));
#77862=CARTESIAN_POINT('Ctrl Pts',(-16.618041066305,-19.0518347865785,-0.0949436511940506));
#77863=CARTESIAN_POINT('Ctrl Pts',(-16.6158311203138,-18.9771167035359,
-0.0904482535772255));
#77864=CARTESIAN_POINT('Ctrl Pts',(-16.6175804393308,-18.9024294117756,
-0.0859528559604003));
#77865=CARTESIAN_POINT('Ctrl Pts',(-16.6193281134804,-18.8278123477383,
-0.0814616853215709));
#77866=CARTESIAN_POINT('Ctrl Pts',(-16.6250276422425,-18.7532264655291,
-0.0769705146827415));
#77867=CARTESIAN_POINT('Ctrl Pts',(-16.6346622154624,-18.6791083247648,
-0.0724793440439121));
#77868=CARTESIAN_POINT('Ctrl Pts',(-16.6442902465126,-18.6050405124837,
-0.0679912230472238));
#77869=CARTESIAN_POINT('Ctrl Pts',(-16.6578479512151,-18.5314402553688,
-0.0635031020505355));
#77870=CARTESIAN_POINT('Ctrl Pts',(-16.6752666606882,-18.458739381659,-0.0590149810538472));
#77871=CARTESIAN_POINT('Ctrl Pts',(-16.6926780888339,-18.3860688981953,
-0.0545287361708016));
#77872=CARTESIAN_POINT('Ctrl Pts',(-16.7139472060124,-18.3142974872696,
-0.0500424912877559));
#77873=CARTESIAN_POINT('Ctrl Pts',(-16.738954437569,-18.2438459180203,-0.0455562464047103));
#77874=CARTESIAN_POINT('Ctrl Pts',(-16.7639647762088,-18.1733855953477,
-0.0410694441174684));
#77875=CARTESIAN_POINT('Ctrl Pts',(-16.7927140135935,-18.1042458686283,
-0.0365826418302264));
#77876=CARTESIAN_POINT('Ctrl Pts',(-16.8250332584604,-18.0368306278641,
-0.0320958395429845));
#77877=CARTESIAN_POINT('Ctrl Pts',(-16.8573540573157,-17.9694121456102,
-0.0276088215193051));
#77878=CARTESIAN_POINT('Ctrl Pts',(-16.893245003916,-17.9037187169574,-0.0231218034956257));
#77879=CARTESIAN_POINT('Ctrl Pts',(-16.9324905209222,-17.8401310343422,
-0.0186347854719464));
#77880=CARTESIAN_POINT('Ctrl Pts',(-16.971763121732,-17.776499469102,-0.0141446709031355));
#77881=CARTESIAN_POINT('Ctrl Pts',(-17.0143946720501,-17.7149769304511,
-0.00965455633432465));
#77882=CARTESIAN_POINT('Ctrl Pts',(-17.0601258387639,-17.65591578501,-0.00516444176551379));
#77883=CARTESIAN_POINT('Ctrl Pts',(-17.0776588692871,-17.6332721277373,
-0.00344296117700913));
#77884=CARTESIAN_POINT('Ctrl Pts',(-17.0956470822643,-17.6109899387145,
-0.00172148058850446));
#77885=CARTESIAN_POINT('Ctrl Pts',(-17.1140743056112,-17.5890877707427,
2.02192933296002E-16));
#77886=CARTESIAN_POINT('',(-20.3539400851898,-17.5891048754966,-2.19119258500671E-7));
#77887=CARTESIAN_POINT('Origin',(-18.734,-18.952,0.));
#77888=CARTESIAN_POINT('Ctrl Pts',(-20.3539400851898,-17.5891048754965,
-2.19119258500671E-7));
#77889=CARTESIAN_POINT('Ctrl Pts',(-20.3072931859159,-17.5336602703872,
-0.00438523983104841));
#77890=CARTESIAN_POINT('Ctrl Pts',(-20.2577048501402,-17.4805043431566,
-0.00877026054283832));
#77891=CARTESIAN_POINT('Ctrl Pts',(-20.2054284583706,-17.4299660674291,
-0.0131552812546282));
#77892=CARTESIAN_POINT('Ctrl Pts',(-20.1532296863998,-17.3795028307521,
-0.0175337911033991));
#77893=CARTESIAN_POINT('Ctrl Pts',(-20.0983511257708,-17.3316498632894,
-0.02191230095217));
#77894=CARTESIAN_POINT('Ctrl Pts',(-20.0410859170621,-17.2867026075148,
-0.0262908108009409));
#77895=CARTESIAN_POINT('Ctrl Pts',(-19.9838881021844,-17.2418082489151,
-0.0306641677032834));
#77896=CARTESIAN_POINT('Ctrl Pts',(-19.9243095970085,-17.1998131057542,
-0.0350375246056259));
#77897=CARTESIAN_POINT('Ctrl Pts',(-19.8626785748432,-17.1609741278558,
-0.0394108815079684));
#77898=CARTESIAN_POINT('Ctrl Pts',(-19.8010865494232,-17.1221597251417,
-0.0437814711888771));
#77899=CARTESIAN_POINT('Ctrl Pts',(-19.7374449915698,-17.0864977823033,
-0.0481520608697857));
#77900=CARTESIAN_POINT('Ctrl Pts',(-19.6721120099389,-17.054202630203,-0.0525226505506944));
#77901=CARTESIAN_POINT('Ctrl Pts',(-19.6067987309428,-17.0219172174346,
-0.0568919221816712));
#77902=CARTESIAN_POINT('Ctrl Pts',(-19.5397954737535,-16.9929967935617,
-0.061261193812648));
#77903=CARTESIAN_POINT('Ctrl Pts',(-19.471484467114,-16.9676094989228,-0.0656304654436248));
#77904=CARTESIAN_POINT('Ctrl Pts',(-19.4031714390131,-16.9422214530222,
-0.0699998663702223));
#77905=CARTESIAN_POINT('Ctrl Pts',(-19.3335510382758,-16.9203669101753,
-0.0743692672968198));
#77906=CARTESIAN_POINT('Ctrl Pts',(-19.2630233707281,-16.9021650619566,
-0.0787386682234172));
#77907=CARTESIAN_POINT('Ctrl Pts',(-19.1924239083035,-16.883944684847,-0.0831125170583778));
#77908=CARTESIAN_POINT('Ctrl Pts',(-19.1209158041551,-16.8693845460033,
-0.0874863658933384));
#77909=CARTESIAN_POINT('Ctrl Pts',(-19.0489112989914,-16.8585531117873,
-0.091860214728299));
#77910=CARTESIAN_POINT('Ctrl Pts',(-18.9768669711116,-16.8477156871527,
-0.0962364825582915));
#77911=CARTESIAN_POINT('Ctrl Pts',(-18.9043261767331,-16.8406111195394,
-0.100612750388284));
#77912=CARTESIAN_POINT('Ctrl Pts',(-18.8317055633236,-16.8372558965928,
-0.104989018218277));
#77913=CARTESIAN_POINT('Ctrl Pts',(-18.7589608117349,-16.8338949382048,
-0.109372766870793));
#77914=CARTESIAN_POINT('Ctrl Pts',(-18.6861364519369,-16.8342961174985,
-0.113756515523309));
#77915=CARTESIAN_POINT('Ctrl Pts',(-18.6136477260046,-16.8384238054558,
-0.118140264175825));
#77916=CARTESIAN_POINT('Ctrl Pts',(-18.5716413935224,-16.8408157502787,
-0.120680593048316));
#77917=CARTESIAN_POINT('Ctrl Pts',(-18.5297476644013,-16.8444581093918,
-0.123220921920807));
#77918=CARTESIAN_POINT('Ctrl Pts',(-18.4880458342194,-16.8493360828855,
-0.125761250793298));
#77919=CARTESIAN_POINT('Ctrl Pts',(-18.4158851594457,-16.8577769080795,
-0.130157025386072));
#77920=CARTESIAN_POINT('Ctrl Pts',(-18.3440241643562,-16.8699525372844,
-0.134552799978846));
#77921=CARTESIAN_POINT('Ctrl Pts',(-18.2728786958473,-16.8858305628878,
-0.138948574571619));
#77922=CARTESIAN_POINT('Ctrl Pts',(-18.2018360533927,-16.9016856400904,
-0.143337995981728));
#77923=CARTESIAN_POINT('Ctrl Pts',(-18.1315073495763,-16.9212323858817,
-0.147727417391837));
#77924=CARTESIAN_POINT('Ctrl Pts',(-18.0623020683667,-16.9443867681649,
-0.152116838801945));
#77925=CARTESIAN_POINT('Ctrl Pts',(-17.9931748039694,-16.9675150479445,
-0.156501311909554));
#77926=CARTESIAN_POINT('Ctrl Pts',(-17.9251688996743,-16.9942427328983,
-0.160885785017163));
#77927=CARTESIAN_POINT('Ctrl Pts',(-17.8586807914584,-17.0244354010415,
-0.165270258124772));
#77928=CARTESIAN_POINT('Ctrl Pts',(-17.7922329666599,-17.0546097762315,
-0.169652074794037));
#77929=CARTESIAN_POINT('Ctrl Pts',(-17.7273015495518,-17.088244770482,-0.174033891463303));
#77930=CARTESIAN_POINT('Ctrl Pts',(-17.664263699225,-17.1251575747197,-0.178415708132568));
#77931=CARTESIAN_POINT('Ctrl Pts',(-17.601243455081,-17.1620600693801,-0.182796300980502));
#77932=CARTESIAN_POINT('Ctrl Pts',(-17.5401161419552,-17.2022383136031,
-0.187176893828435));
#77933=CARTESIAN_POINT('Ctrl Pts',(-17.481233502117,-17.2454640051315,-0.191557486676369));
#77934=CARTESIAN_POINT('Ctrl Pts',(-17.4223480788122,-17.2886917400001,
-0.195938286601192));
#77935=CARTESIAN_POINT('Ctrl Pts',(-17.3657079255823,-17.3349669223205,
-0.200319086526015));
#77936=CARTESIAN_POINT('Ctrl Pts',(-17.3116336689764,-17.3840194451555,
-0.204699886450839));
#77937=CARTESIAN_POINT('Ctrl Pts',(-17.2575022929462,-17.4331237828844,
-0.20908531387839));
#77938=CARTESIAN_POINT('Ctrl Pts',(-17.2059425814251,-17.4850109948883,
-0.213470741305941));
#77939=CARTESIAN_POINT('Ctrl Pts',(-17.1572394598231,-17.5393729441424,
-0.217856168733492));
#77940=CARTESIAN_POINT('Ctrl Pts',(-17.1085090930288,-17.5937653042143,
-0.222244049429123));
#77941=CARTESIAN_POINT('Ctrl Pts',(-17.0626387997765,-17.6506347838423,
-0.226631930124753));
#77942=CARTESIAN_POINT('Ctrl Pts',(-17.019872504564,-17.7096409820867,-0.231019810820383));
#77943=CARTESIAN_POINT('Ctrl Pts',(-16.9770304728485,-17.7687516767129,
-0.235415462185369));
#77944=CARTESIAN_POINT('Ctrl Pts',(-16.9373036781403,-17.8300062430901,
-0.239811113550354));
#77945=CARTESIAN_POINT('Ctrl Pts',(-16.9008917879239,-17.8930366942999,
-0.24420676491534));
#77946=CARTESIAN_POINT('Ctrl Pts',(-16.8767856560651,-17.9347653812468,
-0.247116862435137));
#77947=CARTESIAN_POINT('Ctrl Pts',(-16.8541314891368,-17.9772719122011,
-0.250026959954935));
#77948=CARTESIAN_POINT('Ctrl Pts',(-16.8329756005513,-18.0204447237546,
-0.252937057474732));
#77949=CARTESIAN_POINT('Ctrl Pts',(-16.8011149915786,-18.0854626529992,
-0.257319642435692));
#77950=CARTESIAN_POINT('Ctrl Pts',(-16.7725300877984,-18.1522470560443,
-0.261702227396653));
#77951=CARTESIAN_POINT('Ctrl Pts',(-16.7474199512368,-18.2204340700553,
-0.266084812357613));
#77952=CARTESIAN_POINT('Ctrl Pts',(-16.7223475943392,-18.2885184927293,
-0.27046080346405));
#77953=CARTESIAN_POINT('Ctrl Pts',(-16.7007397931117,-18.3580008874103,
-0.274836794570486));
#77954=CARTESIAN_POINT('Ctrl Pts',(-16.6827489310325,-18.4284944584252,
-0.279212785676922));
#77955=CARTESIAN_POINT('Ctrl Pts',(-16.6647796228869,-18.4989035746903,
-0.283583534131739));
#77956=CARTESIAN_POINT('Ctrl Pts',(-16.6504187653927,-18.5703209945558,
-0.287954282586557));
#77957=CARTESIAN_POINT('Ctrl Pts',(-16.6397694152316,-18.6423433226609,
-0.292325031041374));
#77958=CARTESIAN_POINT('Ctrl Pts',(-16.6291269614596,-18.714319009986,-0.296692949052881));
#77959=CARTESIAN_POINT('Ctrl Pts',(-16.6221913171743,-18.7868983510167,
-0.301060867064388));
#77960=CARTESIAN_POINT('Ctrl Pts',(-16.6190144817355,-18.8596676788374,
-0.305428785075896));
#77961=CARTESIAN_POINT('Ctrl Pts',(-16.6158386481743,-18.9324140574164,
-0.309795325578372));
#77962=CARTESIAN_POINT('Ctrl Pts',(-16.616419291388,-19.0053498208129,-0.314161866080849));
#77963=CARTESIAN_POINT('Ctrl Pts',(-16.6207564193529,-19.0780577996553,
-0.318528406583326));
#77964=CARTESIAN_POINT('Ctrl Pts',(-16.6250936203624,-19.1507670030232,
-0.322895020625736));
#77965=CARTESIAN_POINT('Ctrl Pts',(-16.6331874009118,-19.2232479313927,
-0.327261634668147));
#77966=CARTESIAN_POINT('Ctrl Pts',(-16.6449857626134,-19.2950867470421,
-0.331628248710558));
#77967=CARTESIAN_POINT('Ctrl Pts',(-16.6567963363639,-19.3669999203992,
-0.335999382474065));
#77968=CARTESIAN_POINT('Ctrl Pts',(-16.6723190685484,-19.4382691756095,
-0.340370516237573));
#77969=CARTESIAN_POINT('Ctrl Pts',(-16.6914506293117,-19.5084899534591,
-0.34474165000108));
#77970=CARTESIAN_POINT('Ctrl Pts',(-16.7105925668403,-19.578748818349,-0.349115154623359));
#77971=CARTESIAN_POINT('Ctrl Pts',(-16.7333470785607,-19.6479576138077,
-0.353488659245638));
#77972=CARTESIAN_POINT('Ctrl Pts',(-16.7595614725531,-19.715728683063,-0.357862163867917));
#77973=CARTESIAN_POINT('Ctrl Pts',(-16.7858226024992,-19.7836205769906,
-0.362243465729766));
#77974=CARTESIAN_POINT('Ctrl Pts',(-16.815555734801,-19.8500691841256,-0.366624767591615));
#77975=CARTESIAN_POINT('Ctrl Pts',(-16.8485609817508,-19.9147090466302,
-0.371006069453464));
#77976=CARTESIAN_POINT('Ctrl Pts',(-16.871428766834,-19.9594949706928,-0.374041667687698));
#77977=CARTESIAN_POINT('Ctrl Pts',(-16.8958663395961,-20.0034131234881,
-0.377077265921932));
#77978=CARTESIAN_POINT('Ctrl Pts',(-16.9217951774031,-20.0463503465328,
-0.380112864156166));
#77979=CARTESIAN_POINT('Ctrl Pts',(-16.9592871194148,-20.108435654348,-0.384502203694482));
#77980=CARTESIAN_POINT('Ctrl Pts',(-17.0000462087351,-20.1687128298791,
-0.388891543232798));
#77981=CARTESIAN_POINT('Ctrl Pts',(-17.0438726579669,-20.2268170722547,
-0.393280882771115));
#77982=CARTESIAN_POINT('Ctrl Pts',(-17.0876341208282,-20.2848351569816,
-0.39766371374554));
#77983=CARTESIAN_POINT('Ctrl Pts',(-17.1344536264988,-20.3406863231545,
-0.402046544719966));
#77984=CARTESIAN_POINT('Ctrl Pts',(-17.1840869213949,-20.3940327488545,
-0.406429375694392));
#77985=CARTESIAN_POINT('Ctrl Pts',(-17.233661916773,-20.4473165135744,-0.410807058573503));
#77986=CARTESIAN_POINT('Ctrl Pts',(-17.286043808912,-20.4981010311795,-0.415184741452614));
#77987=CARTESIAN_POINT('Ctrl Pts',(-17.3409477702608,-20.5460810786214,
-0.419562424331725));
#77988=CARTESIAN_POINT('Ctrl Pts',(-17.3958169194767,-20.5940307040728,
-0.423937331518979));
#77989=CARTESIAN_POINT('Ctrl Pts',(-17.4532046028362,-20.6391790711338,
-0.428312238706232));
#77990=CARTESIAN_POINT('Ctrl Pts',(-17.512789805683,-20.6812584136838,-0.432687145893485));
#77991=CARTESIAN_POINT('Ctrl Pts',(-17.5723568562233,-20.7233249369921,
-0.437060720289174));
#77992=CARTESIAN_POINT('Ctrl Pts',(-17.6341197035788,-20.7623240140803,
-0.441434294684862));
#77993=CARTESIAN_POINT('Ctrl Pts',(-17.6977263244878,-20.7980297585468,
-0.44580786908055));
#77994=CARTESIAN_POINT('Ctrl Pts',(-17.7613345200932,-20.8337363869733,
-0.450181551751953));
#77995=CARTESIAN_POINT('Ctrl Pts',(-17.8267861585153,-20.8661492866598,
-0.454555234423356));
#77996=CARTESIAN_POINT('Ctrl Pts',(-17.893703933171,-20.8950881400677,-0.458928917094759));
#77997=CARTESIAN_POINT('Ctrl Pts',(-17.9606909349874,-20.9240569310321,
-0.463307124388127));
#77998=CARTESIAN_POINT('Ctrl Pts',(-18.0291466578796,-20.9495443083808,
-0.467685331681495));
#77999=CARTESIAN_POINT('Ctrl Pts',(-18.0986738647243,-20.9714181592319,
-0.472063538974863));
#78000=CARTESIAN_POINT('Ctrl Pts',(-18.168238941735,-20.9933039243595,-0.476444130995652));
#78001=CARTESIAN_POINT('Ctrl Pts',(-18.2388761976448,-21.0115721233672,
-0.480824723016442));
#78002=CARTESIAN_POINT('Ctrl Pts',(-18.3101759171464,-21.026141303478,-0.485205315037232));
#78003=CARTESIAN_POINT('Ctrl Pts',(-18.381601628856,-21.040736228475,-0.4895936479084));
#78004=CARTESIAN_POINT('Ctrl Pts',(-18.4536916647472,-21.0516190094181,
-0.493981980779569));
#78005=CARTESIAN_POINT('Ctrl Pts',(-18.5260294507968,-21.0587598939281,
-0.498370313650738));
#78006=CARTESIAN_POINT('Ctrl Pts',(-18.5750331942105,-21.063597339078,-0.501343099379692));
#78007=CARTESIAN_POINT('Ctrl Pts',(-18.6241505410346,-21.0667186770647,
-0.504315885108646));
#78008=CARTESIAN_POINT('Ctrl Pts',(-18.6732524746729,-21.0681282423725,
-0.5072886708376));
#78009=CARTESIAN_POINT('Ctrl Pts',(-18.7457477477536,-21.0702093584171,
-0.511677763023227));
#78010=CARTESIAN_POINT('Ctrl Pts',(-18.8184909227825,-21.068564845846,-0.516066855208853));
#78011=CARTESIAN_POINT('Ctrl Pts',(-18.8910671418926,-21.063165297398,-0.520455947394479));
#78012=CARTESIAN_POINT('Ctrl Pts',(-18.9635359951035,-21.0577737367921,
-0.524838546560291));
#78013=CARTESIAN_POINT('Ctrl Pts',(-19.035837905828,-21.0486382034475,-0.529221145726102));
#78014=CARTESIAN_POINT('Ctrl Pts',(-19.1075566421874,-21.0357812829272,
-0.533603744891914));
#78015=CARTESIAN_POINT('Ctrl Pts',(-19.1791915341236,-21.0229393930828,
-0.537981220480295));
#78016=CARTESIAN_POINT('Ctrl Pts',(-19.2502441338016,-21.0063848432238,
-0.542358696068677));
#78017=CARTESIAN_POINT('Ctrl Pts',(-19.32030366582,-20.9861919799876,-0.546736171657058));
#78018=CARTESIAN_POINT('Ctrl Pts',(-19.3903190177729,-20.9660118505222,
-0.551110886776556));
#78019=CARTESIAN_POINT('Ctrl Pts',(-19.4593420824551,-20.9421980932421,
-0.555485601896053));
#78020=CARTESIAN_POINT('Ctrl Pts',(-19.5269740036053,-20.91487575501,-0.559860317015551));
#78021=CARTESIAN_POINT('Ctrl Pts',(-19.5945855605349,-20.8875616436346,
-0.564233714892222));
#78022=CARTESIAN_POINT('Ctrl Pts',(-19.6608063587657,-20.8567412292127,
-0.568607112768892));
#78023=CARTESIAN_POINT('Ctrl Pts',(-19.7252559833366,-20.8225882966328,
-0.572980510645563));
#78024=CARTESIAN_POINT('Ctrl Pts',(-19.7897074377076,-20.7884343944112,
-0.577354032688112));
#78025=CARTESIAN_POINT('Ctrl Pts',(-19.8523871934859,-20.750948013708,-0.581727554730662));
#78026=CARTESIAN_POINT('Ctrl Pts',(-19.91293947795,-20.7103488582563,-0.586101076773212));
#78027=CARTESIAN_POINT('Ctrl Pts',(-19.973554763754,-20.6697074616039,-0.590479149226235));
#78028=CARTESIAN_POINT('Ctrl Pts',(-20.0320377575058,-20.6259470930868,
-0.594857221679259));
#78029=CARTESIAN_POINT('Ctrl Pts',(-20.0880624400642,-20.5793303009554,
-0.599235294132282));
#78030=CARTESIAN_POINT('Ctrl Pts',(-20.144117821258,-20.532687965227,-0.603615765543122));
#78031=CARTESIAN_POINT('Ctrl Pts',(-20.1977118548976,-20.4831864169908,
-0.607996236953962));
#78032=CARTESIAN_POINT('Ctrl Pts',(-20.2485543758913,-20.4311261076962,
-0.612376708364801));
#78033=CARTESIAN_POINT('Ctrl Pts',(-20.2994870261127,-20.3789735103841,
-0.616764945096826));
#78034=CARTESIAN_POINT('Ctrl Pts',(-20.3476581043646,-20.3242534561184,
-0.62115318182885));
#78035=CARTESIAN_POINT('Ctrl Pts',(-20.3928172134661,-20.2673001377285,
-0.625541418560875));
#78036=CARTESIAN_POINT('Ctrl Pts',(-20.4234261206891,-20.2286970989767,
-0.628515771546929));
#78037=CARTESIAN_POINT('Ctrl Pts',(-20.4526521510532,-20.1890687322311,
-0.631490124532982));
#78038=CARTESIAN_POINT('Ctrl Pts',(-20.4804290435443,-20.1485260531492,
-0.634464477519035));
#78039=CARTESIAN_POINT('Ctrl Pts',(-20.5219934354816,-20.0878593747552,
-0.6389151976027));
#78040=CARTESIAN_POINT('Ctrl Pts',(-20.5604705838686,-20.0249114796293,
-0.643365917686366));
#78041=CARTESIAN_POINT('Ctrl Pts',(-20.5956057938581,-19.9600242399239,
-0.647816637770031));
#78042=CARTESIAN_POINT('Ctrl Pts',(-20.6306759070159,-19.8952572201836,
-0.652259111773021));
#78043=CARTESIAN_POINT('Ctrl Pts',(-20.6624161699,-19.8285584030127,-0.656701585776012));
#78044=CARTESIAN_POINT('Ctrl Pts',(-20.6906149824499,-19.760298713628,-0.661144059779002));
#78045=CARTESIAN_POINT('Ctrl Pts',(-20.7018340510959,-19.7331411820968,
-0.662911525012145));
#78046=CARTESIAN_POINT('Ctrl Pts',(-20.7124930319529,-19.7057368944626,
-0.664678990245288));
#78047=CARTESIAN_POINT('Ctrl Pts',(-20.7225805821191,-19.6781103693095,
-0.666446455478431));
#78048=CARTESIAN_POINT('Origin',(18.734,-18.952,0.));
#78049=CARTESIAN_POINT('',(16.745419449923,-19.6781104570625,-21.2464098137458));
#78050=CARTESIAN_POINT('',(16.7454194499919,-19.678110457251,-21.4658225324418));
#78051=CARTESIAN_POINT('',(16.7454194499637,-19.6781104571739,0.));
#78052=CARTESIAN_POINT('',(16.6170006158577,-18.953614788214,-21.5109437210328));
#78053=CARTESIAN_POINT('Ctrl Pts',(16.7454194499919,-19.678110457251,-21.4658225324418));
#78054=CARTESIAN_POINT('Ctrl Pts',(16.7444838645978,-19.6755481929303,-21.4659708416694));
#78055=CARTESIAN_POINT('Ctrl Pts',(16.7435532220733,-19.672984094887,-21.466119187511));
#78056=CARTESIAN_POINT('Ctrl Pts',(16.7287348633895,-19.6319093107387,-21.4684945478173));
#78057=CARTESIAN_POINT('Ctrl Pts',(16.7159624561017,-19.5930064377761,-21.4707298068511));
#78058=CARTESIAN_POINT('Ctrl Pts',(16.6989527891759,-19.5356344857477,-21.4740350315673));
#78059=CARTESIAN_POINT('Ctrl Pts',(16.6938224023506,-19.5174393926652,-21.4750845544372));
#78060=CARTESIAN_POINT('Ctrl Pts',(16.67330414272,-19.4407529854473,-21.479522275393));
#78061=CARTESIAN_POINT('Ctrl Pts',(16.6601842244916,-19.3816901056815,-21.4829746671899));
#78062=CARTESIAN_POINT('Ctrl Pts',(16.6480276539524,-19.3132345736383,-21.4870987991129));
#78063=CARTESIAN_POINT('Ctrl Pts',(16.6465011846899,-19.3043063086001,-21.4876390674732));
#78064=CARTESIAN_POINT('Ctrl Pts',(16.644305726321,-19.2909496980064,-21.4884512303201));
#78065=CARTESIAN_POINT('Ctrl Pts',(16.6435933949815,-19.286528444333,-21.4887207108556));
#78066=CARTESIAN_POINT('Ctrl Pts',(16.6423404404213,-19.2785913960363,-21.4892056875075));
#78067=CARTESIAN_POINT('Ctrl Pts',(16.6417946456356,-19.2750764736216,-21.4894208862796));
#78068=CARTESIAN_POINT('Ctrl Pts',(16.6407480030303,-19.2682221989107,-21.4898413667536));
#78069=CARTESIAN_POINT('Ctrl Pts',(16.640246287296,-19.2648830325719,-21.4900465921491));
#78070=CARTESIAN_POINT('Ctrl Pts',(16.6391505446239,-19.2574696572128,-21.4905030441399));
#78071=CARTESIAN_POINT('Ctrl Pts',(16.6385604120744,-19.2533948985467,-21.4907544855749));
#78072=CARTESIAN_POINT('Ctrl Pts',(16.637120554269,-19.2432442762658,-21.4913821828982));
#78073=CARTESIAN_POINT('Ctrl Pts',(16.6362853529834,-19.2371664356149,-21.4917592136064));
#78074=CARTESIAN_POINT('Ctrl Pts',(16.6323978968592,-19.2079355069642,-21.4935779411442));
#78075=CARTESIAN_POINT('Ctrl Pts',(16.6297026110604,-19.1847375792239,-21.4950376377215));
#78076=CARTESIAN_POINT('Ctrl Pts',(16.6205187442238,-19.0923904497098,-21.5009009048513));
#78077=CARTESIAN_POINT('Ctrl Pts',(16.6170514757345,-19.0229900275189,-21.5054225881123));
#78078=CARTESIAN_POINT('Ctrl Pts',(16.6170005689161,-18.9535520277953,-21.5099894676286));
#78079=CARTESIAN_POINT('',(20.3539256943886,-20.3149122292574,-22.));
#78080=CARTESIAN_POINT('Ctrl Pts',(16.6170006158577,-18.953614788214,-21.5109437210328));
#78081=CARTESIAN_POINT('Ctrl Pts',(16.6169439842755,-18.879370361958,-21.5154240901546));
#78082=CARTESIAN_POINT('Ctrl Pts',(16.620797918379,-18.8049814529217,-21.5199044592764));
#78083=CARTESIAN_POINT('Ctrl Pts',(16.6285774617411,-18.730900621006,-21.5243848283982));
#78084=CARTESIAN_POINT('Ctrl Pts',(16.6360763262784,-18.6594925578986,-21.5287035498909));
#78085=CARTESIAN_POINT('Ctrl Pts',(16.6472223388839,-18.5883712693749,-21.5330222713836));
#78086=CARTESIAN_POINT('Ctrl Pts',(16.6619760550115,-18.5179426634713,-21.5373409928764));
#78087=CARTESIAN_POINT('Ctrl Pts',(16.6767199425897,-18.4475609753088,-21.541656837347));
#78088=CARTESIAN_POINT('Ctrl Pts',(16.6950666675508,-18.3778715396864,-21.5459726818176));
#78089=CARTESIAN_POINT('Ctrl Pts',(16.7169252861184,-18.3092725316128,-21.5502885262882));
#78090=CARTESIAN_POINT('Ctrl Pts',(16.738777013927,-18.2406951488414,-21.5546030102225));
#78091=CARTESIAN_POINT('Ctrl Pts',(16.7641382879759,-18.1732079844748,-21.5589174941569));
#78092=CARTESIAN_POINT('Ctrl Pts',(16.792868144003,-18.1071946273647,-21.5632319780912));
#78093=CARTESIAN_POINT('Ctrl Pts',(16.8215990247681,-18.0411789156865,-21.5675466159148));
#78094=CARTESIAN_POINT('Ctrl Pts',(16.8536985247398,-17.9766375696395,-21.5718612537383));
#78095=CARTESIAN_POINT('Ctrl Pts',(16.8889780706294,-17.9139330078739,-21.5761758915619));
#78096=CARTESIAN_POINT('Ctrl Pts',(16.9242925056221,-17.8511664355052,-21.5804947962727));
#78097=CARTESIAN_POINT('Ctrl Pts',(16.9627930151098,-17.7902407038457,-21.5848137009835));
#78098=CARTESIAN_POINT('Ctrl Pts',(17.0042462802129,-17.7314914711963,-21.5891326056943));
#78099=CARTESIAN_POINT('Ctrl Pts',(17.0457242009246,-17.6727072956277,-21.593454079207));
#78100=CARTESIAN_POINT('Ctrl Pts',(17.0901580619222,-17.6161025825292,-21.5977755527196));
#78101=CARTESIAN_POINT('Ctrl Pts',(17.1372743754074,-17.5619797556261,-21.6020970262323));
#78102=CARTESIAN_POINT('Ctrl Pts',(17.1844652778813,-17.5077712478488,-21.606425340992));
#78103=CARTESIAN_POINT('Ctrl Pts',(17.2343467552723,-17.4560528156038,-21.6107536557517));
#78104=CARTESIAN_POINT('Ctrl Pts',(17.2866094559726,-17.4070891245576,-21.6150819705114));
#78105=CARTESIAN_POINT('Ctrl Pts',(17.3002562150789,-17.3943037979728,-21.6162121736595));
#78106=CARTESIAN_POINT('Ctrl Pts',(17.3140651673995,-17.3817060763086,-21.6173423768076));
#78107=CARTESIAN_POINT('Ctrl Pts',(17.3280304696825,-17.3693001927659,-21.6184725799558));
#78108=CARTESIAN_POINT('Ctrl Pts',(17.3823193529476,-17.3210734125788,-21.6228661452028));
#78109=CARTESIAN_POINT('Ctrl Pts',(17.4391955190593,-17.2755515953447,-21.6272597104498));
#78110=CARTESIAN_POINT('Ctrl Pts',(17.4983586556721,-17.2330237150596,-21.6316532756968));
#78111=CARTESIAN_POINT('Ctrl Pts',(17.5574354931409,-17.1905578686671,-21.6360404322079));
#78112=CARTESIAN_POINT('Ctrl Pts',(17.6187922908035,-17.1510775674503,-21.640427588719));
#78113=CARTESIAN_POINT('Ctrl Pts',(17.6820943811751,-17.1148327324153,-21.64481474523));
#78114=CARTESIAN_POINT('Ctrl Pts',(17.7453240043386,-17.0786293898806,-21.6491968793954));
#78115=CARTESIAN_POINT('Ctrl Pts',(17.810494080778,-17.0456543930935,-21.6535790135607));
#78116=CARTESIAN_POINT('Ctrl Pts',(17.8772409624661,-17.0161144270376,-21.6579611477261));
#78117=CARTESIAN_POINT('Ctrl Pts',(17.9439467029022,-16.9865926687415,-21.6623405808441));
#78118=CARTESIAN_POINT('Ctrl Pts',(18.0122268812651,-16.9605019339683,-21.6667200139621));
#78119=CARTESIAN_POINT('Ctrl Pts',(18.0816945039053,-16.9380023486199,-21.6710994470801));
#78120=CARTESIAN_POINT('Ctrl Pts',(18.1511420514884,-16.9155092652999,-21.6754776146104));
#78121=CARTESIAN_POINT('Ctrl Pts',(18.2217759047592,-16.8966054189395,-21.6798557821407));
#78122=CARTESIAN_POINT('Ctrl Pts',(18.2931919729642,-16.881401708853,-21.684233949671));
#78123=CARTESIAN_POINT('Ctrl Pts',(18.364610783359,-16.866197414984,-21.6886122853114));
#78124=CARTESIAN_POINT('Ctrl Pts',(18.4368113975566,-16.8546936376761,-21.6929906209519));
#78125=CARTESIAN_POINT('Ctrl Pts',(18.5093791774671,-16.8469502414231,-21.6973689565923));
#78126=CARTESIAN_POINT('Ctrl Pts',(18.5820229096485,-16.8391987406294,-21.7017518747697));
#78127=CARTESIAN_POINT('Ctrl Pts',(18.6550340955975,-16.8352155299105,-21.7061347929472));
#78128=CARTESIAN_POINT('Ctrl Pts',(18.7279934268567,-16.835008521255,-21.7105177111246));
#78129=CARTESIAN_POINT('Ctrl Pts',(18.8009931127498,-16.8348013981006,-21.7149030535438));
#78130=CARTESIAN_POINT('Ctrl Pts',(18.8739404062014,-16.8383746122317,-21.719288395963));
#78131=CARTESIAN_POINT('Ctrl Pts',(18.9464191616025,-16.845683998118,-21.7236737383821));
#78132=CARTESIAN_POINT('Ctrl Pts',(19.019026007826,-16.8530063017931,-21.7280668309636));
#78133=CARTESIAN_POINT('Ctrl Pts',(19.0911621866738,-16.8640778900689,-21.7324599235451));
#78134=CARTESIAN_POINT('Ctrl Pts',(19.1624203793687,-16.8788031983091,-21.7368530161266));
#78135=CARTESIAN_POINT('Ctrl Pts',(19.2099755048328,-16.8886303333286,-21.7397848062968));
#78136=CARTESIAN_POINT('Ctrl Pts',(19.2571398375277,-16.9000836817304,-21.742716596467));
#78137=CARTESIAN_POINT('Ctrl Pts',(19.3037965853284,-16.9131226492631,-21.7456483866372));
#78138=CARTESIAN_POINT('Ctrl Pts',(19.3728941566259,-16.932433060537,-21.7499903005052));
#78139=CARTESIAN_POINT('Ctrl Pts',(19.4411600971652,-16.9553024383045,-21.7543322143732));
#78140=CARTESIAN_POINT('Ctrl Pts',(19.5081957188875,-16.9816421673066,-21.7586741282413));
#78141=CARTESIAN_POINT('Ctrl Pts',(19.5751303969638,-17.007942233392,-21.7630095039643));
#78142=CARTESIAN_POINT('Ctrl Pts',(19.6408379766924,-17.0377021052713,-21.7673448796873));
#78143=CARTESIAN_POINT('Ctrl Pts',(19.7049332499917,-17.0707829407374,-21.7716802554104));
#78144=CARTESIAN_POINT('Ctrl Pts',(19.7689548569736,-17.1038257555634,-21.7760106483765));
#78145=CARTESIAN_POINT('Ctrl Pts',(19.8313673996942,-17.1401817328403,-21.7803410413427));
#78146=CARTESIAN_POINT('Ctrl Pts',(19.8918057405323,-17.1796640083804,-21.7846714343088));
#78147=CARTESIAN_POINT('Ctrl Pts',(19.9522069377095,-17.2191220192527,-21.7889991659403));
#78148=CARTESIAN_POINT('Ctrl Pts',(20.0106359263449,-17.2617022501812,-21.7933268975719));
#78149=CARTESIAN_POINT('Ctrl Pts',(20.0667536873044,-17.307172772302,-21.7976546292034));
#78150=CARTESIAN_POINT('Ctrl Pts',(20.1228564014125,-17.3526311024149,-21.8019812004406));
#78151=CARTESIAN_POINT('Ctrl Pts',(20.1766487340221,-17.4009778759096,-21.8063077716777));
#78152=CARTESIAN_POINT('Ctrl Pts',(20.2278235795987,-17.4519399635232,-21.8106343429149));
#78153=CARTESIAN_POINT('Ctrl Pts',(20.2790024328481,-17.5029060421478,-21.8149612529802));
#78154=CARTESIAN_POINT('Ctrl Pts',(20.3275630441483,-17.5564874916594,-21.8192881630456));
#78155=CARTESIAN_POINT('Ctrl Pts',(20.3732354326212,-17.6123746059293,-21.823615073111));
#78156=CARTESIAN_POINT('Ctrl Pts',(20.4189626303271,-17.6683287876325,-21.8279471756927));
#78157=CARTESIAN_POINT('Ctrl Pts',(20.4617943736678,-17.7265937742531,-21.8322792782743));
#78158=CARTESIAN_POINT('Ctrl Pts',(20.5015018190868,-17.7868277725912,-21.836611380856));
#78159=CARTESIAN_POINT('Ctrl Pts',(20.5412337707152,-17.8470989454934,-21.8409461570777));
#78160=CARTESIAN_POINT('Ctrl Pts',(20.5778373403004,-17.9093411211074,-21.8452809332993));
#78161=CARTESIAN_POINT('Ctrl Pts',(20.6111293159145,-17.973187182688,-21.8496157095209));
#78162=CARTESIAN_POINT('Ctrl Pts',(20.6444883378172,-18.0371618230444,-21.8539592154936));
#78163=CARTESIAN_POINT('Ctrl Pts',(20.674522245953,-18.1027463491743,-21.8583027214662));
#78164=CARTESIAN_POINT('Ctrl Pts',(20.7010959324481,-18.1695534570681,-21.8626462274389));
#78165=CARTESIAN_POINT('Ctrl Pts',(20.7218522888838,-18.2217356089171,-21.8660388827321));
#78166=CARTESIAN_POINT('Ctrl Pts',(20.7404985496073,-18.2746632207694,-21.8694315380253));
#78167=CARTESIAN_POINT('Ctrl Pts',(20.7569919383483,-18.3281469585088,-21.8728241933186));
#78168=CARTESIAN_POINT('Ctrl Pts',(20.7789191314163,-18.3992510998001,-21.8773345707065));
#78169=CARTESIAN_POINT('Ctrl Pts',(20.7971284192367,-18.4716259697097,-21.8818449480945));
#78170=CARTESIAN_POINT('Ctrl Pts',(20.8114805262578,-18.5448591607076,-21.8863553254824));
#78171=CARTESIAN_POINT('Ctrl Pts',(20.8265480064888,-18.621742621512,-21.891090520254));
#78172=CARTESIAN_POINT('Ctrl Pts',(20.8373635429458,-18.6995717540552,-21.8958257150255));
#78173=CARTESIAN_POINT('Ctrl Pts',(20.843824811693,-18.7778498809511,-21.9005609097971));
#78174=CARTESIAN_POINT('Ctrl Pts',(20.8499588507186,-18.8521636270621,-21.9050562915339));
#78175=CARTESIAN_POINT('Ctrl Pts',(20.8521688501583,-18.9268814796183,-21.9095516732707));
#78176=CARTESIAN_POINT('Ctrl Pts',(20.8504196084828,-19.0015685467751,-21.9140470550075));
#78177=CARTESIAN_POINT('Ctrl Pts',(20.8486720115918,-19.0761853868609,-21.9185382098078));
#78178=CARTESIAN_POINT('Ctrl Pts',(20.8429725838885,-19.1507710509859,-21.9230293646081));
#78179=CARTESIAN_POINT('Ctrl Pts',(20.8333381346341,-19.2248889819521,-21.9275205194084));
#78180=CARTESIAN_POINT('Ctrl Pts',(20.8237102273003,-19.2989565858473,-21.9320086246542));
#78181=CARTESIAN_POINT('Ctrl Pts',(20.8101526690551,-19.3725566428308,-21.9364967299001));
#78182=CARTESIAN_POINT('Ctrl Pts',(20.7927341278966,-19.4452573269945,-21.9409848351459));
#78183=CARTESIAN_POINT('Ctrl Pts',(20.7753228675005,-19.5179276230559,-21.9454710644121));
#78184=CARTESIAN_POINT('Ctrl Pts',(20.7540539396924,-19.5896988571003,-21.9499572936783));
#78185=CARTESIAN_POINT('Ctrl Pts',(20.7290469182522,-19.6601502622835,-21.9544435229445));
#78186=CARTESIAN_POINT('Ctrl Pts',(20.7040367879202,-19.7306104260392,-21.9589303099422));
#78187=CARTESIAN_POINT('Ctrl Pts',(20.6752877790479,-19.7997500064623,-21.9634170969398));
#78188=CARTESIAN_POINT('Ctrl Pts',(20.6429687820359,-19.8671651158193,-21.9679038839375));
#78189=CARTESIAN_POINT('Ctrl Pts',(20.6106482296079,-19.9345834696624,-21.9723908868707));
#78190=CARTESIAN_POINT('Ctrl Pts',(20.5747575484645,-20.0002767846379,-21.9768778898039));
#78191=CARTESIAN_POINT('Ctrl Pts',(20.5355123150534,-20.0638643706455,-21.9813648927371));
#78192=CARTESIAN_POINT('Ctrl Pts',(20.4962399941625,-20.1274958454851,-21.9858549926477));
#78193=CARTESIAN_POINT('Ctrl Pts',(20.4536087412679,-20.1890183104101,-21.9903450925584));
#78194=CARTESIAN_POINT('Ctrl Pts',(20.407877888554,-20.2480794011981,-21.994835192469));
#78195=CARTESIAN_POINT('Ctrl Pts',(20.3903436794274,-20.2707247151527,-21.9965567949793));
#78196=CARTESIAN_POINT('Ctrl Pts',(20.372354222822,-20.2930085100904,-21.9982783974897));
#78197=CARTESIAN_POINT('Ctrl Pts',(20.3539256943887,-20.3149122292573,-22.));
#78198=CARTESIAN_POINT('',(17.1140599642913,-20.3148951833168,-21.9999997809128));
#78199=CARTESIAN_POINT('Origin',(18.734,-18.952,-22.));
#78200=CARTESIAN_POINT('',(16.6170002905213,-18.9531090839331,-21.2890562790225));
#78201=CARTESIAN_POINT('Ctrl Pts',(17.1140599642913,-20.3148951833168,-21.9999997809128));
#78202=CARTESIAN_POINT('Ctrl Pts',(17.1607068994597,-20.3703398270043,-21.9956147572469));
#78203=CARTESIAN_POINT('Ctrl Pts',(17.210295274204,-20.4234957880638,-21.9912297335811));
#78204=CARTESIAN_POINT('Ctrl Pts',(17.2625717073312,-20.4740340927633,-21.9868447099152));
#78205=CARTESIAN_POINT('Ctrl Pts',(17.3147705210273,-20.5244973587843,-21.9824661970807));
#78206=CARTESIAN_POINT('Ctrl Pts',(17.3696491258074,-20.5723503507068,-21.9780876842462));
#78207=CARTESIAN_POINT('Ctrl Pts',(17.4269143804502,-20.6172976260014,-21.9737091714118));
#78208=CARTESIAN_POINT('Ctrl Pts',(17.4841122416856,-20.6621920044732,-21.9693358114907));
#78209=CARTESIAN_POINT('Ctrl Pts',(17.5436907950378,-20.7041871625307,-21.9649624515697));
#78210=CARTESIAN_POINT('Ctrl Pts',(17.605321866596,-20.7430261503327,-21.9605890916486));
#78211=CARTESIAN_POINT('Ctrl Pts',(17.6669139416705,-20.7818405631288,-21.9562184989301));
#78212=CARTESIAN_POINT('Ctrl Pts',(17.7305555504131,-20.8175025110335,-21.9518479062116));
#78213=CARTESIAN_POINT('Ctrl Pts',(17.7958885836047,-20.8497976631951,-21.9474773134931));
#78214=CARTESIAN_POINT('Ctrl Pts',(17.8612019143776,-20.8820830761394,-21.94310803881));
#78215=CARTESIAN_POINT('Ctrl Pts',(17.9282052240273,-20.9110034951629,-21.9387387641268));
#78216=CARTESIAN_POINT('Ctrl Pts',(17.9965162832812,-20.9363907799561,-21.9343694894437));
#78217=CARTESIAN_POINT('Ctrl Pts',(18.0648293641575,-20.9617788160697,-21.9300000854546));
#78218=CARTESIAN_POINT('Ctrl Pts',(18.1344498178311,-20.9836333441171,-21.9256306814655));
#78219=CARTESIAN_POINT('Ctrl Pts',(18.2049775379727,-21.0018351725616,-21.9212612774765));
#78220=CARTESIAN_POINT('Ctrl Pts',(18.2755770529193,-21.0200555298444,-21.9168874255837));
#78221=CARTESIAN_POINT('Ctrl Pts',(18.347085209244,-21.0346156438901,-21.912513573691));
#78222=CARTESIAN_POINT('Ctrl Pts',(18.4190897657556,-21.0454470483793,-21.9081397217982));
#78223=CARTESIAN_POINT('Ctrl Pts',(18.4911341450163,-21.0562844432714,-21.9037634509084));
#78224=CARTESIAN_POINT('Ctrl Pts',(18.5636749899472,-21.0633889762076,-21.8993871800187));
#78225=CARTESIAN_POINT('Ctrl Pts',(18.6362956526055,-21.0667441595853,-21.8950109091289));
#78226=CARTESIAN_POINT('Ctrl Pts',(18.7090404529568,-21.0701050783104,-21.8906271574457));
#78227=CARTESIAN_POINT('Ctrl Pts',(18.7818648602089,-21.0697038545041,-21.8862434057626));
#78228=CARTESIAN_POINT('Ctrl Pts',(18.8543536318168,-21.0655761172261,-21.8818596540794));
#78229=CARTESIAN_POINT('Ctrl Pts',(18.896359511156,-21.063184171133,-21.8793193524552));
#78230=CARTESIAN_POINT('Ctrl Pts',(18.9382527891111,-21.0595418376991,-21.8767790508309));
#78231=CARTESIAN_POINT('Ctrl Pts',(18.979954172718,-21.054663916303,-21.8742387492067));
#78232=CARTESIAN_POINT('Ctrl Pts',(19.0521148572584,-21.0462230897252,-21.8698429740959));
#78233=CARTESIAN_POINT('Ctrl Pts',(19.1239758615628,-21.0340474581782,-21.8654471989851));
#78234=CARTESIAN_POINT('Ctrl Pts',(19.1951213386526,-21.0181694294126,-21.8610514238743));
#78235=CARTESIAN_POINT('Ctrl Pts',(19.2661639899332,-21.0023143489949,-21.856662001931));
#78236=CARTESIAN_POINT('Ctrl Pts',(19.3364927019385,-20.9827675991443,-21.8522725799877));
#78237=CARTESIAN_POINT('Ctrl Pts',(19.4056979906368,-20.959613212094,-21.8478831580444));
#78238=CARTESIAN_POINT('Ctrl Pts',(19.4748252628419,-20.936484927443,-21.8434986843834));
#78239=CARTESIAN_POINT('Ctrl Pts',(19.5428311742357,-20.9097572368777,-21.8391142107225));
#78240=CARTESIAN_POINT('Ctrl Pts',(19.6093192887935,-20.8795645625156,-21.8347297370615));
#78241=CARTESIAN_POINT('Ctrl Pts',(19.675767120119,-20.8493901810247,-21.8303479198267));
#78242=CARTESIAN_POINT('Ctrl Pts',(19.7406985429898,-20.8157551798471,-21.825966102592));
#78243=CARTESIAN_POINT('Ctrl Pts',(19.803736398282,-20.7788423681836,-21.8215842853572));
#78244=CARTESIAN_POINT('Ctrl Pts',(19.8667566475552,-20.7419398660025,-21.8172036919325));
#78245=CARTESIAN_POINT('Ctrl Pts',(19.9278839650038,-20.7017616137434,-21.8128230985077));
#78246=CARTESIAN_POINT('Ctrl Pts',(19.9867666083377,-20.6585359137838,-21.808442505083));
#78247=CARTESIAN_POINT('Ctrl Pts',(20.0456520352798,-20.6153081703798,-21.8040617045708));
#78248=CARTESIAN_POINT('Ctrl Pts',(20.1022921913093,-20.5690329791144,-21.7996809040586));
#78249=CARTESIAN_POINT('Ctrl Pts',(20.1563664498668,-20.519980447038,-21.7953001035464));
#78250=CARTESIAN_POINT('Ctrl Pts',(20.2104978279948,-20.4708760999272,-21.7909146755192));
#78251=CARTESIAN_POINT('Ctrl Pts',(20.2620575407503,-20.4189888782294,-21.786529247492));
#78252=CARTESIAN_POINT('Ctrl Pts',(20.3107606627202,-20.364626919076,-21.7821438194648));
#78253=CARTESIAN_POINT('Ctrl Pts',(20.3594910299654,-20.3102345490068,-21.7777559381617));
#78254=CARTESIAN_POINT('Ctrl Pts',(20.4053613227915,-20.2533650591673,-21.7733680568587));
#78255=CARTESIAN_POINT('Ctrl Pts',(20.4481276167033,-20.1943588505964,-21.7689801755556));
#78256=CARTESIAN_POINT('Ctrl Pts',(20.4909696471634,-20.1352481455596,-21.7645845235772));
#78257=CARTESIAN_POINT('Ctrl Pts',(20.5306964397318,-20.0739935686515,-21.7601888715988));
#78258=CARTESIAN_POINT('Ctrl Pts',(20.5671083269304,-20.0109631068826,-21.7557932196204));
#78259=CARTESIAN_POINT('Ctrl Pts',(20.5912144107273,-19.969234492684,-21.7528831272554));
#78260=CARTESIAN_POINT('Ctrl Pts',(20.613868534761,-19.9267280374392,-21.7499730348904));
#78261=CARTESIAN_POINT('Ctrl Pts',(20.6350243858782,-19.8835553039387,-21.7470629425253));
#78262=CARTESIAN_POINT('Ctrl Pts',(20.6668849852277,-19.8185373967291,-21.7426803588893));
#78263=CARTESIAN_POINT('Ctrl Pts',(20.6954698819653,-19.7517530160599,-21.7382977752533));
#78264=CARTESIAN_POINT('Ctrl Pts',(20.7205800139613,-19.6835660244499,-21.7339151916173));
#78265=CARTESIAN_POINT('Ctrl Pts',(20.7456523661794,-19.6154816244714,-21.7295392018549));
#78266=CARTESIAN_POINT('Ctrl Pts',(20.7672601652298,-19.5459992525245,-21.7251632120926));
#78267=CARTESIAN_POINT('Ctrl Pts',(20.7852510275153,-19.4755057039971,-21.7207872223302));
#78268=CARTESIAN_POINT('Ctrl Pts',(20.8032203357683,-19.4050966105787,-21.7164164752418));
#78269=CARTESIAN_POINT('Ctrl Pts',(20.8175811957868,-19.3336792133251,-21.7120457281534));
#78270=CARTESIAN_POINT('Ctrl Pts',(20.8282305507602,-19.2616569073388,-21.707674981065));
#78271=CARTESIAN_POINT('Ctrl Pts',(20.8388730093072,-19.1896812423493,-21.7033070644331));
#78272=CARTESIAN_POINT('Ctrl Pts',(20.845808660676,-19.1171019231659,-21.6989391478011));
#78273=CARTESIAN_POINT('Ctrl Pts',(20.8489855053725,-19.0443326164712,-21.6945712311692));
#78274=CARTESIAN_POINT('Ctrl Pts',(20.8521613481799,-18.9715862592065,-21.6902046920575));
#78275=CARTESIAN_POINT('Ctrl Pts',(20.8515807164049,-18.8986505164049,-21.6858381529459));
#78276=CARTESIAN_POINT('Ctrl Pts',(20.8472436019355,-18.8259425572265,-21.6814716138342));
#78277=CARTESIAN_POINT('Ctrl Pts',(20.8429064144311,-18.753233373679,-21.677105001192));
#78278=CARTESIAN_POINT('Ctrl Pts',(20.8348126494595,-18.6807524641984,-21.6727383885499));
#78279=CARTESIAN_POINT('Ctrl Pts',(20.8230143052733,-18.6089136663121,-21.6683717759077));
#78280=CARTESIAN_POINT('Ctrl Pts',(20.8112037490663,-18.5370005107965,-21.6640006435495));
#78281=CARTESIAN_POINT('Ctrl Pts',(20.7956810363731,-18.4657312722987,-21.6596295111913));
#78282=CARTESIAN_POINT('Ctrl Pts',(20.7765494969166,-18.3955105098514,-21.6552583788331));
#78283=CARTESIAN_POINT('Ctrl Pts',(20.7574075807255,-18.3252516604421,-21.6508848756213));
#78284=CARTESIAN_POINT('Ctrl Pts',(20.734653092167,-18.2560428791505,-21.6465113724094));
#78285=CARTESIAN_POINT('Ctrl Pts',(20.7084387230319,-18.1882718225755,-21.6421378691975));
#78286=CARTESIAN_POINT('Ctrl Pts',(20.6821776179286,-18.1203799411991,-21.6377565687388));
#78287=CARTESIAN_POINT('Ctrl Pts',(20.6524445121555,-18.0539313451297,-21.6333752682801));
#78288=CARTESIAN_POINT('Ctrl Pts',(20.619439293294,-17.9892914920377,-21.6289939678214));
#78289=CARTESIAN_POINT('Ctrl Pts',(20.5965714267485,-17.9445053768408,-21.6259583571622));
#78290=CARTESIAN_POINT('Ctrl Pts',(20.57213375941,-17.9005870397827,-21.622922746503));
#78291=CARTESIAN_POINT('Ctrl Pts',(20.546204814931,-17.8576496407728,-21.6198871358438));
#78292=CARTESIAN_POINT('Ctrl Pts',(20.5087128672688,-17.7955643245834,-21.6154977957359));
#78293=CARTESIAN_POINT('Ctrl Pts',(20.4679537715697,-17.7352871414802,-21.6111084556279));
#78294=CARTESIAN_POINT('Ctrl Pts',(20.4241273153556,-17.6771828923768,-21.60671911552));
#78295=CARTESIAN_POINT('Ctrl Pts',(20.3803658454572,-17.6191648008458,-21.6023362839703));
#78296=CARTESIAN_POINT('Ctrl Pts',(20.3335463321389,-17.5633136287167,-21.5979534524206));
#78297=CARTESIAN_POINT('Ctrl Pts',(20.283913029103,-17.5099671979401,-21.5935706208709));
#78298=CARTESIAN_POINT('Ctrl Pts',(20.2343380255226,-17.456683428072,-21.5891929374108));
#78299=CARTESIAN_POINT('Ctrl Pts',(20.1819561246821,-17.4058989062031,-21.5848152539507));
#78300=CARTESIAN_POINT('Ctrl Pts',(20.1270521542449,-17.3579188554049,-21.5804375704906));
#78301=CARTESIAN_POINT('Ctrl Pts',(20.0721829959018,-17.3099692265604,-21.5760626627192));
#78302=CARTESIAN_POINT('Ctrl Pts',(20.0147953030245,-17.2648208570169,-21.5716877549478));
#78303=CARTESIAN_POINT('Ctrl Pts',(19.9552100903752,-17.222741512912,-21.5673128471764));
#78304=CARTESIAN_POINT('Ctrl Pts',(19.8956430300011,-17.1806749880252,-21.5629392721942));
#78305=CARTESIAN_POINT('Ctrl Pts',(19.8338801725247,-17.1416759102888,-21.558565697212));
#78306=CARTESIAN_POINT('Ctrl Pts',(19.7702735413081,-17.1059701661173,-21.5541921222299));
#78307=CARTESIAN_POINT('Ctrl Pts',(19.7066653353733,-17.0702635379739,-21.5498184389705));
#78308=CARTESIAN_POINT('Ctrl Pts',(19.6412136864337,-17.0378506395157,-21.5454447557111));
#78309=CARTESIAN_POINT('Ctrl Pts',(19.5742959011684,-17.0089117882917,-21.5410710724518));
#78310=CARTESIAN_POINT('Ctrl Pts',(19.5073088887682,-16.9799429995295,-21.5366928645722));
#78311=CARTESIAN_POINT('Ctrl Pts',(19.4388531552012,-16.9544556253366,-21.5323146566927));
#78312=CARTESIAN_POINT('Ctrl Pts',(19.3693259376834,-16.9325817786039,-21.5279364488132));
#78313=CARTESIAN_POINT('Ctrl Pts',(19.2997608500006,-16.9106960175991,-21.5235558562063));
#78314=CARTESIAN_POINT('Ctrl Pts',(19.2291235834203,-16.8924278236772,-21.5191752635995));
#78315=CARTESIAN_POINT('Ctrl Pts',(19.1578238533414,-16.8778586496242,-21.5147946709926));
#78316=CARTESIAN_POINT('Ctrl Pts',(19.0863981311614,-16.8632637307212,-21.5104063375421));
#78317=CARTESIAN_POINT('Ctrl Pts',(19.0143080848955,-16.8523809568344,-21.5060180040915));
#78318=CARTESIAN_POINT('Ctrl Pts',(18.9419702886576,-16.8452400803519,-21.5016296706409));
#78319=CARTESIAN_POINT('Ctrl Pts',(18.8929666311248,-16.8404026497993,-21.4986568901481));
#78320=CARTESIAN_POINT('Ctrl Pts',(18.8438493706969,-16.8372813203535,-21.4956841096553));
#78321=CARTESIAN_POINT('Ctrl Pts',(18.7947475232676,-16.8358717575684,-21.4927113291624));
#78322=CARTESIAN_POINT('Ctrl Pts',(18.7222522474693,-16.8337906415164,-21.488322236837));
#78323=CARTESIAN_POINT('Ctrl Pts',(18.6495090698324,-16.8354351543627,-21.4839331445116));
#78324=CARTESIAN_POINT('Ctrl Pts',(18.5769328482517,-16.8408347033352,-21.4795440521862));
#78325=CARTESIAN_POINT('Ctrl Pts',(18.5044639925059,-16.8462262644699,-21.4751614528767));
#78326=CARTESIAN_POINT('Ctrl Pts',(18.4321620793838,-16.8553617985987,-21.4707788535672));
#78327=CARTESIAN_POINT('Ctrl Pts',(18.3604433407868,-16.868218720125,-21.4663962542577));
#78328=CARTESIAN_POINT('Ctrl Pts',(18.2888084465286,-16.8810606109898,-21.4620187785205));
#78329=CARTESIAN_POINT('Ctrl Pts',(18.2177558446894,-16.8976151620993,-21.4576413027833));
#78330=CARTESIAN_POINT('Ctrl Pts',(18.1476963106892,-16.917808026783,-21.4532638270461));
#78331=CARTESIAN_POINT('Ctrl Pts',(18.0776809567047,-16.9379881577097,-21.4488891117746));
#78332=CARTESIAN_POINT('Ctrl Pts',(18.0086578901714,-16.9618019166529,-21.4445143965032));
#78333=CARTESIAN_POINT('Ctrl Pts',(17.9410259673652,-16.9891242567175,-21.4401396812318));
#78334=CARTESIAN_POINT('Ctrl Pts',(17.8734144087345,-17.0164383699432,-21.4357662832003));
#78335=CARTESIAN_POINT('Ctrl Pts',(17.8071936089994,-17.0472587863894,-21.4313928851688));
#78336=CARTESIAN_POINT('Ctrl Pts',(17.7427439831315,-17.0814117211363,-21.4270194871373));
#78337=CARTESIAN_POINT('Ctrl Pts',(17.6782925274241,-17.1155656255459,-21.4226459649373));
#78338=CARTESIAN_POINT('Ctrl Pts',(17.6156127705188,-17.1530520085839,-21.4182724427373));
#78339=CARTESIAN_POINT('Ctrl Pts',(17.5550604851453,-17.1936511664877,-21.4138989205372));
#78340=CARTESIAN_POINT('Ctrl Pts',(17.4944451983904,-17.2342925656217,-21.4095208479236));
#78341=CARTESIAN_POINT('Ctrl Pts',(17.4359622039086,-17.2780529367419,-21.4051427753101));
#78342=CARTESIAN_POINT('Ctrl Pts',(17.3799375208464,-17.32466973157,-21.4007647026965));
#78343=CARTESIAN_POINT('Ctrl Pts',(17.3238821391245,-17.3713120700165,-21.3963842311231));
#78344=CARTESIAN_POINT('Ctrl Pts',(17.2702881051855,-17.4208136210669,-21.3920037595497));
#78345=CARTESIAN_POINT('Ctrl Pts',(17.2194455841251,-17.4728739332451,-21.3876232879764));
#78346=CARTESIAN_POINT('Ctrl Pts',(17.1685129338238,-17.5250265334594,-21.3832350510804));
#78347=CARTESIAN_POINT('Ctrl Pts',(17.120341855727,-17.5797465906982,-21.3788468141844));
#78348=CARTESIAN_POINT('Ctrl Pts',(17.0751827470182,-17.6366999121076,-21.3744585772885));
#78349=CARTESIAN_POINT('Ctrl Pts',(17.0445738554429,-17.6753029335072,-21.371484225686));
#78350=CARTESIAN_POINT('Ctrl Pts',(17.015347839445,-17.7149312818909,-21.3685098740835));
#78351=CARTESIAN_POINT('Ctrl Pts',(16.9875709599417,-17.7554739417626,-21.365535522481));
#78352=CARTESIAN_POINT('Ctrl Pts',(16.9460128347077,-17.8161314730044,-21.3610854734259));
#78353=CARTESIAN_POINT('Ctrl Pts',(16.9075410210167,-17.8790695324529,-21.3566354243708));
#78354=CARTESIAN_POINT('Ctrl Pts',(16.8724101016156,-17.9439464050791,-21.3521853753158));
#78355=CARTESIAN_POINT('Ctrl Pts',(16.8373354751619,-18.0087193205517,-21.3477424569132));
#78356=CARTESIAN_POINT('Ctrl Pts',(16.8055913305909,-18.0754244744595,-21.3432995385106));
#78357=CARTESIAN_POINT('Ctrl Pts',(16.77738933593,-18.1436908331291,-21.338856620108));
#78358=CARTESIAN_POINT('Ctrl Pts',(16.7492306468634,-18.2118523653399,-21.3344205240321));
#78359=CARTESIAN_POINT('Ctrl Pts',(16.7246034679416,-18.2815699082597,-21.3299844279563));
#78360=CARTESIAN_POINT('Ctrl Pts',(16.703673027533,-18.3524490139505,-21.3255483318804));
#78361=CARTESIAN_POINT('Ctrl Pts',(16.6827615762291,-18.4232638146991,-21.3211162604448));
#78362=CARTESIAN_POINT('Ctrl Pts',(16.6655403334367,-18.495237641409,-21.3166841890092));
#78363=CARTESIAN_POINT('Ctrl Pts',(16.6521256163152,-18.5679582697712,-21.3122521175736));
#78364=CARTESIAN_POINT('Ctrl Pts',(16.6387184414623,-18.6406380118066,-21.3078225380185));
#78365=CARTESIAN_POINT('Ctrl Pts',(16.6291136269053,-18.7140632656555,-21.3033929584635));
#78366=CARTESIAN_POINT('Ctrl Pts',(16.6233766956374,-18.7878102710847,-21.2989633789084));
#78367=CARTESIAN_POINT('Ctrl Pts',(16.6190996643447,-18.8427905794111,-21.2956610122798));
#78368=CARTESIAN_POINT('Ctrl Pts',(16.6169713926958,-18.8979494279291,-21.2923586456512));
#78369=CARTESIAN_POINT('Ctrl Pts',(16.6170002905213,-18.9531090839331,-21.2890562790225));
#78370=CARTESIAN_POINT('Ctrl Pts',(16.6170002427961,-18.9530139027121,-21.2873807947792));
#78371=CARTESIAN_POINT('Ctrl Pts',(16.6170353681744,-19.0263546841816,-21.283214403805));
#78372=CARTESIAN_POINT('Ctrl Pts',(16.620881643312,-19.099649181836,-21.2791526234396));
#78373=CARTESIAN_POINT('Ctrl Pts',(16.6454736247964,-19.3343610415228,-21.2662365927548));
#78374=CARTESIAN_POINT('Ctrl Pts',(16.6810044211168,-19.4936083875884,-21.257642580014));
#78375=CARTESIAN_POINT('Ctrl Pts',(16.7379955393082,-19.6575316163442,-21.2476766099661));
#78376=CARTESIAN_POINT('Ctrl Pts',(16.7416677446335,-19.6678357556093,-21.2470450721877));
#78377=CARTESIAN_POINT('Ctrl Pts',(16.745419449923,-19.6781104570625,-21.2464098137458));
#78378=CARTESIAN_POINT('Origin',(18.734,-18.952,0.));
#78379=CARTESIAN_POINT('',(16.7454193204094,-19.6781101023667,-20.4442392291799));
#78380=CARTESIAN_POINT('',(16.7454194499653,-19.6781104571783,-20.6683679347509));
#78381=CARTESIAN_POINT('',(16.7454194499637,-19.6781104571739,0.));
#78382=CARTESIAN_POINT('Ctrl Pts',(16.7454194499653,-19.6781104571783,-20.6683679347509));
#78383=CARTESIAN_POINT('Ctrl Pts',(16.7441348064984,-19.6745922362427,-20.668590378304));
#78384=CARTESIAN_POINT('Ctrl Pts',(16.7428594929539,-19.6710705874846,-20.6688125127429));
#78385=CARTESIAN_POINT('Ctrl Pts',(16.7369541278903,-19.6546273468838,-20.6698472702451));
#78386=CARTESIAN_POINT('Ctrl Pts',(16.7324404003774,-19.6416641112149,-20.6706560419502));
#78387=CARTESIAN_POINT('Ctrl Pts',(16.6991411812999,-19.5429488037885,-20.6767638054007));
#78388=CARTESIAN_POINT('Ctrl Pts',(16.6757501965837,-19.4554694899014,-20.6818794970702));
#78389=CARTESIAN_POINT('Ctrl Pts',(16.6306360858101,-19.2296586008703,-20.6946257394849));
#78390=CARTESIAN_POINT('Ctrl Pts',(16.6168948154608,-19.0901947037234,-20.7020607995078));
#78391=CARTESIAN_POINT('Ctrl Pts',(16.6170159593102,-18.9301096100918,-20.7109057137875));
#78392=CARTESIAN_POINT('Ctrl Pts',(16.6173229632374,-18.9098229033623,-20.7120327871212));
#78393=CARTESIAN_POINT('Ctrl Pts',(16.6196735652514,-18.830181690397,-20.7164920546507));
#78394=CARTESIAN_POINT('Ctrl Pts',(16.6239226589396,-18.7709248029925,-20.719885302315));
#78395=CARTESIAN_POINT('Ctrl Pts',(16.6316702790211,-18.7030447059488,-20.7239378573419));
#78396=CARTESIAN_POINT('Ctrl Pts',(16.6327408114508,-18.6941651491509,-20.7244712651555));
#78397=CARTESIAN_POINT('Ctrl Pts',(16.634438362504,-18.6807981222699,-20.7252795503377));
#78398=CARTESIAN_POINT('Ctrl Pts',(16.6350235902586,-18.6763053163335,-20.7255521289721));
#78399=CARTESIAN_POINT('Ctrl Pts',(16.636095341283,-18.6682787152921,-20.7260407764863));
#78400=CARTESIAN_POINT('Ctrl Pts',(16.6365763773781,-18.6647442403234,-20.7262565330954));
#78401=CARTESIAN_POINT('Ctrl Pts',(16.6376355527075,-18.6571063309708,-20.7267240521063));
#78402=CARTESIAN_POINT('Ctrl Pts',(16.6382167997036,-18.6530034304865,-20.7269759827503));
#78403=CARTESIAN_POINT('Ctrl Pts',(16.6398690487733,-18.6415821111098,-20.7276794391765));
#78404=CARTESIAN_POINT('Ctrl Pts',(16.6409663520168,-18.6342676419927,-20.7281324118739));
#78405=CARTESIAN_POINT('Ctrl Pts',(16.6474610426461,-18.5924691027289,-20.7307344389076));
#78406=CARTESIAN_POINT('Ctrl Pts',(16.6536719553288,-18.5581190719979,-20.7329253955482));
#78407=CARTESIAN_POINT('Ctrl Pts',(16.6761041931998,-18.4494703058947,-20.739990366585));
#78408=CARTESIAN_POINT('Ctrl Pts',(16.6954799886247,-18.3758873130994,-20.7449760055384));
#78409=CARTESIAN_POINT('Ctrl Pts',(16.7775784089416,-18.1207598411494,-20.7626582096691));
#78410=CARTESIAN_POINT('Ctrl Pts',(16.8609882798593,-17.9468118002398,-20.7753361225597));
#78411=CARTESIAN_POINT('Ctrl Pts',(16.9785112585037,-17.7686123322985,-20.7884543812594));
#78412=CARTESIAN_POINT('Ctrl Pts',(16.9905654135348,-17.7509242367354,-20.7897596025357));
#78413=CARTESIAN_POINT('Ctrl Pts',(17.0076899876059,-17.7265970495096,-20.7915596575448));
#78414=CARTESIAN_POINT('Ctrl Pts',(17.0125342438745,-17.7198010292286,-20.7920630665967));
#78415=CARTESIAN_POINT('Ctrl Pts',(17.020958416024,-17.7081293818748,-20.7929286403344));
#78416=CARTESIAN_POINT('Ctrl Pts',(17.024519245586,-17.7032401613862,-20.793291534835));
#78417=CARTESIAN_POINT('Ctrl Pts',(17.0319299155845,-17.6931559926561,-20.7940406860232));
#78418=CARTESIAN_POINT('Ctrl Pts',(17.0357827044739,-17.6879632815084,-20.7944268228754));
#78419=CARTESIAN_POINT('Ctrl Pts',(17.0448502384326,-17.6758585304046,-20.7953278661294));
#78420=CARTESIAN_POINT('Ctrl Pts',(17.0500837422373,-17.6689606367444,-20.7958420316204));
#78421=CARTESIAN_POINT('Ctrl Pts',(17.0671665414274,-17.6467296366344,-20.7975015884365));
#78422=CARTESIAN_POINT('Ctrl Pts',(17.0791842933618,-17.6315267840458,-20.7986403172642));
#78423=CARTESIAN_POINT('Ctrl Pts',(17.1414401067977,-17.5549561348447,-20.8043989609493));
#78424=CARTESIAN_POINT('Ctrl Pts',(17.1948920696731,-17.4962777335467,-20.8088862716222));
#78425=CARTESIAN_POINT('Ctrl Pts',(17.3679310293639,-17.3265344580812,-20.8223348122778));
#78426=CARTESIAN_POINT('Ctrl Pts',(17.4971413356927,-17.2261791559357,-20.8309358352439));
#78427=CARTESIAN_POINT('Ctrl Pts',(17.6888224651241,-17.1099834120811,-20.8434650927113));
#78428=CARTESIAN_POINT('Ctrl Pts',(17.7424062160291,-17.0805937133456,-20.8469515463375));
#78429=CARTESIAN_POINT('Ctrl Pts',(17.8053528508124,-17.0495314623582,-20.8511147112887));
#78430=CARTESIAN_POINT('Ctrl Pts',(17.8135516627711,-17.0455512290744,-20.8516582496761));
#78431=CARTESIAN_POINT('Ctrl Pts',(17.8258413198441,-17.0396827906079,-20.8524752803578));
#78432=CARTESIAN_POINT('Ctrl Pts',(17.829913030924,-17.0377544438696,-20.8527463458961));
#78433=CARTESIAN_POINT('Ctrl Pts',(17.837219177645,-17.0343227909233,-20.8532334596924));
#78434=CARTESIAN_POINT('Ctrl Pts',(17.8404512827568,-17.0328146490828,-20.8534492048724));
#78435=CARTESIAN_POINT('Ctrl Pts',(17.8474674131497,-17.0295623982225,-20.8539181004368));
#78436=CARTESIAN_POINT('Ctrl Pts',(17.8512527308801,-17.027821313275,-20.8541714267524));
#78437=CARTESIAN_POINT('Ctrl Pts',(17.8618590201682,-17.0229807559241,-20.8548821606054));
#78438=CARTESIAN_POINT('Ctrl Pts',(17.8686912632587,-17.0199063379374,-20.8553410607026));
#78439=CARTESIAN_POINT('Ctrl Pts',(17.9088201517114,-17.0021044161471,-20.8580420077365));
#78440=CARTESIAN_POINT('Ctrl Pts',(17.9424738266147,-16.9882025261106,-20.8603296450267));
#78441=CARTESIAN_POINT('Ctrl Pts',(18.0526121619314,-16.9459967134346,-20.8678505797909));
#78442=CARTESIAN_POINT('Ctrl Pts',(18.1303751010118,-16.9212430486737,-20.8732107040317));
#78443=CARTESIAN_POINT('Ctrl Pts',(18.3869084934598,-16.8556220732748,-20.8906947769685));
#78444=CARTESIAN_POINT('Ctrl Pts',(18.5696370356424,-16.8334428624919,-20.9027594149921));
#78445=CARTESIAN_POINT('Ctrl Pts',(18.7752757176076,-16.8352847894356,-20.9154088510647));
#78446=CARTESIAN_POINT('Ctrl Pts',(18.7975860889257,-16.8358374739657,-20.9167705181314));
#78447=CARTESIAN_POINT('Ctrl Pts',(18.828370448187,-16.8370873888204,-20.9186352166078));
#78448=CARTESIAN_POINT('Ctrl Pts',(18.8368545988943,-16.8374830175211,-20.9191476427989));
#78449=CARTESIAN_POINT('Ctrl Pts',(18.8514163840271,-16.8382499051485,-20.920024659769));
#78450=CARTESIAN_POINT('Ctrl Pts',(18.8574951702196,-16.8385963436061,-20.9203900242773));
#78451=CARTESIAN_POINT('Ctrl Pts',(18.8700077345155,-16.8393636221401,-20.9211405879507));
#78452=CARTESIAN_POINT('Ctrl Pts',(18.876441259797,-16.8397876390306,-20.921525683414));
#78453=CARTESIAN_POINT('Ctrl Pts',(18.8913807799879,-16.8408408313187,-20.9224180718585));
#78454=CARTESIAN_POINT('Ctrl Pts',(18.8998851476281,-16.8414920359164,-20.9229246681711));
#78455=CARTESIAN_POINT('Ctrl Pts',(18.926981877434,-16.8437317094449,-20.9245344936403));
#78456=CARTESIAN_POINT('Ctrl Pts',(18.9455575972416,-16.8455146318989,-20.9256316173553));
#78457=CARTESIAN_POINT('Ctrl Pts',(19.1238293861668,-16.8650074144962,-20.936104584212));
#78458=CARTESIAN_POINT('Ctrl Pts',(19.2810467987769,-16.9005973171631,-20.944851943207));
#78459=CARTESIAN_POINT('Ctrl Pts',(19.5595112982897,-16.9979642147191,-20.9608716902572));
#78460=CARTESIAN_POINT('Ctrl Pts',(19.6817599775027,-17.0542471539759,-20.9681342243965));
#78461=CARTESIAN_POINT('Ctrl Pts',(19.8113925966665,-17.1295949860951,-20.9769255599056));
#78462=CARTESIAN_POINT('Ctrl Pts',(19.8248600163339,-17.1376242852256,-20.9778530720793));
#78463=CARTESIAN_POINT('Ctrl Pts',(19.843175667546,-17.1488217361748,-20.9791357894353));
#78464=CARTESIAN_POINT('Ctrl Pts',(19.8481023036346,-17.1518615142572,-20.9794829568611));
#78465=CARTESIAN_POINT('Ctrl Pts',(19.8559119558499,-17.1567244782742,-20.9800367880161));
#78466=CARTESIAN_POINT('Ctrl Pts',(19.858803181974,-17.1585345174698,-20.9802425906215));
#78467=CARTESIAN_POINT('Ctrl Pts',(19.8647630702242,-17.1622857591029,-20.9806684406013));
#78468=CARTESIAN_POINT('Ctrl Pts',(19.8678311048603,-17.1642278640955,-20.9808885509505));
#78469=CARTESIAN_POINT('Ctrl Pts',(19.8751297553507,-17.1688743472511,-20.9814142824791));
#78470=CARTESIAN_POINT('Ctrl Pts',(19.8793557607971,-17.1715858930986,-20.9817203767317));
#78471=CARTESIAN_POINT('Ctrl Pts',(19.8935799345559,-17.1807841979277,-20.9827562531188));
#78472=CARTESIAN_POINT('Ctrl Pts',(19.9035327475494,-17.1873402085578,-20.9834904469937));
#78473=CARTESIAN_POINT('Ctrl Pts',(19.9273112382603,-17.20329284101,-20.9852661632181));
#78474=CARTESIAN_POINT('Ctrl Pts',(19.9410818220879,-17.2127697457847,-20.9863123317198));
#78475=CARTESIAN_POINT('Ctrl Pts',(19.9923064800113,-17.248923887959,-20.9902670048094));
#78476=CARTESIAN_POINT('Ctrl Pts',(20.0289984831854,-17.2766547150036,-20.9932278203942));
#78477=CARTESIAN_POINT('Ctrl Pts',(20.1225696448146,-17.3522846175853,-21.0010639595944));
#78478=CARTESIAN_POINT('Ctrl Pts',(20.17788036306,-17.4020245455899,-21.0059870821838));
#78479=CARTESIAN_POINT('Ctrl Pts',(20.340265877829,-17.564304632727,-21.0211539576285));
#78480=CARTESIAN_POINT('Ctrl Pts',(20.4376882469793,-17.6858043470796,-21.031270219651));
#78481=CARTESIAN_POINT('Ctrl Pts',(20.5337906378363,-17.8370938509968,-21.0423125609111));
#78482=CARTESIAN_POINT('Ctrl Pts',(20.5462830395389,-17.8575173278558,-21.0437748160134));
#78483=CARTESIAN_POINT('Ctrl Pts',(20.5633463525542,-17.8865071637873,-21.0458116441825));
#78484=CARTESIAN_POINT('Ctrl Pts',(20.5682085162694,-17.894899160264,-21.0463967903385));
#78485=CARTESIAN_POINT('Ctrl Pts',(20.5759804390449,-17.9085284141976,-21.0473399870257));
#78486=CARTESIAN_POINT('Ctrl Pts',(20.5789258966666,-17.9137450577254,-21.047699324951));
#78487=CARTESIAN_POINT('Ctrl Pts',(20.585018155475,-17.9246427286944,-21.048446539027));
#78488=CARTESIAN_POINT('Ctrl Pts',(20.5881610425254,-17.9303258813913,-21.0488342716484));
#78489=CARTESIAN_POINT('Ctrl Pts',(20.5955279171313,-17.9437930548324,-21.0497485408661));
#78490=CARTESIAN_POINT('Ctrl Pts',(20.5997293309015,-17.9515893353267,-21.0502742671338));
#78491=CARTESIAN_POINT('Ctrl Pts',(20.6135045226626,-17.9775396546421,-21.0520126166771));
#78492=CARTESIAN_POINT('Ctrl Pts',(20.6228634135764,-17.9958068898118,-21.0532176350391));
#78493=CARTESIAN_POINT('Ctrl Pts',(20.6710804835961,-18.0933912503387,-21.0595612182483));
#78494=CARTESIAN_POINT('Ctrl Pts',(20.705214392142,-18.1749503421696,-21.0645333127584));
#78495=CARTESIAN_POINT('Ctrl Pts',(20.7770394327539,-18.3820778355627,-21.0766340371412));
#78496=CARTESIAN_POINT('Ctrl Pts',(20.8083599893668,-18.5094499401615,-21.0836114699341));
#78497=CARTESIAN_POINT('Ctrl Pts',(20.833296192086,-18.6761974614834,-21.0929116951813));
#78498=CARTESIAN_POINT('Ctrl Pts',(20.8378764044661,-18.713640216961,-21.0950120356838));
#78499=CARTESIAN_POINT('Ctrl Pts',(20.8458049312631,-18.7968456367883,-21.0997433823018));
#78500=CARTESIAN_POINT('Ctrl Pts',(20.8486704702366,-18.842633321617,-21.1023896304583));
#78501=CARTESIAN_POINT('Ctrl Pts',(20.8502755294736,-18.8960977918028,-21.1055661138367));
#78502=CARTESIAN_POINT('Ctrl Pts',(20.8504631957338,-18.9037225656617,-21.1060211766074));
#78503=CARTESIAN_POINT('Ctrl Pts',(20.8506981199302,-18.9159542766341,-21.1067547192797));
#78504=CARTESIAN_POINT('Ctrl Pts',(20.8507715502729,-18.9205607232214,-21.1070317729793));
#78505=CARTESIAN_POINT('Ctrl Pts',(20.8508753357168,-18.9287483570312,-21.1075257003794));
#78506=CARTESIAN_POINT('Ctrl Pts',(20.8509116405735,-18.9323294209292,-21.1077422381226));
#78507=CARTESIAN_POINT('Ctrl Pts',(20.8509695834459,-18.9399531742319,-21.1082043236871));
#78508=CARTESIAN_POINT('Ctrl Pts',(20.8509887281269,-18.9439957762768,-21.1084500024256));
#78509=CARTESIAN_POINT('Ctrl Pts',(20.8510092759738,-18.9549760307021,-21.1091190226478));
#78510=CARTESIAN_POINT('Ctrl Pts',(20.8509881550678,-18.9619136038538,-21.1095435935371));
#78511=CARTESIAN_POINT('Ctrl Pts',(20.8507067513094,-18.9972657303104,-21.1117161927685));
#78512=CARTESIAN_POINT('Ctrl Pts',(20.8499084969048,-19.0256716116516,-21.1134918173908));
#78513=CARTESIAN_POINT('Ctrl Pts',(20.8458833591939,-19.1090740112288,-21.1187766106147));
#78514=CARTESIAN_POINT('Ctrl Pts',(20.841081398104,-19.1639686715603,-21.1223459901169));
#78515=CARTESIAN_POINT('Ctrl Pts',(20.8165236137624,-19.3574160321671,-21.1351168642238));
#78516=CARTESIAN_POINT('Ctrl Pts',(20.7851821639716,-19.4941470826533,-21.1444681992938));
#78517=CARTESIAN_POINT('Ctrl Pts',(20.7117607576932,-19.7124765734288,-21.1593417742929));
#78518=CARTESIAN_POINT('Ctrl Pts',(20.6774820193082,-19.7962414439341,-21.1650403526591));
#78519=CARTESIAN_POINT('Ctrl Pts',(20.6319427774607,-19.8899183348006,-21.1713958232838));
#78520=CARTESIAN_POINT('Ctrl Pts',(20.625818564718,-19.9022105668768,-21.1722295668832));
#78521=CARTESIAN_POINT('Ctrl Pts',(20.6158042833255,-19.9218301055949,-21.1735601516639));
#78522=CARTESIAN_POINT('Ctrl Pts',(20.6119900834166,-19.9291954994298,-21.1740596352053));
#78523=CARTESIAN_POINT('Ctrl Pts',(20.6051403519625,-19.9422344075863,-21.1749438714527));
#78524=CARTESIAN_POINT('Ctrl Pts',(20.602122073986,-19.9479168222362,-21.1753292269818));
#78525=CARTESIAN_POINT('Ctrl Pts',(20.5957788408268,-19.9597287192617,-21.1761302977887));
#78526=CARTESIAN_POINT('Ctrl Pts',(20.5924494089736,-19.9658557194433,-21.1765458481905));
#78527=CARTESIAN_POINT('Ctrl Pts',(20.5837231444416,-19.9817268370587,-21.1776224012723));
#78528=CARTESIAN_POINT('Ctrl Pts',(20.578279529071,-19.9914450903525,-21.1782817260884));
#78529=CARTESIAN_POINT('Ctrl Pts',(20.5542939886397,-20.0334837843617,-21.1811348734192));
#78530=CARTESIAN_POINT('Ctrl Pts',(20.5349766166401,-20.0653556740046,-21.1833006274091));
#78531=CARTESIAN_POINT('Ctrl Pts',(20.4814022596282,-20.1487019246783,-21.1889868978582));
#78532=CARTESIAN_POINT('Ctrl Pts',(20.4457144124919,-20.1992148099006,-21.1924562679554));
#78533=CARTESIAN_POINT('Ctrl Pts',(20.3212188357911,-20.3599966382228,-21.203706746279));
#78534=CARTESIAN_POINT('Ctrl Pts',(20.2235750955592,-20.4629208706177,-21.2112292798062));
#78535=CARTESIAN_POINT('Ctrl Pts',(20.0589846054194,-20.6048312739061,-21.2232594631871));
#78536=CARTESIAN_POINT('Ctrl Pts',(19.9989617028074,-20.6512070870442,-21.2275423201506));
#78537=CARTESIAN_POINT('Ctrl Pts',(19.9287634567381,-20.6996612096779,-21.232597429934));
#78538=CARTESIAN_POINT('Ctrl Pts',(19.9209015376318,-20.7050100267027,-21.2331642151306));
#78539=CARTESIAN_POINT('Ctrl Pts',(19.9091942263251,-20.7128601792525,-21.2340095820793));
#78540=CARTESIAN_POINT('Ctrl Pts',(19.9053761836469,-20.715402357927,-21.2342854892835));
#78541=CARTESIAN_POINT('Ctrl Pts',(19.8985629713055,-20.7199069285266,-21.2347782736967));
#78542=CARTESIAN_POINT('Ctrl Pts',(19.8955710575026,-20.7218741481059,-21.2349948230819));
#78543=CARTESIAN_POINT('Ctrl Pts',(19.8891185625986,-20.7260933326153,-21.2354621790106));
#78544=CARTESIAN_POINT('Ctrl Pts',(19.8856564244501,-20.7283427388438,-21.2357131445364));
#78545=CARTESIAN_POINT('Ctrl Pts',(19.8760732416528,-20.734529292701,-21.2364083233809));
#78546=CARTESIAN_POINT('Ctrl Pts',(19.8699385072232,-20.7384449817777,-21.236853916029));
#78547=CARTESIAN_POINT('Ctrl Pts',(19.8360663291079,-20.759819958445,-21.239316789699));
#78548=CARTESIAN_POINT('Ctrl Pts',(19.8079481125203,-20.7766639072493,-21.2413707537187));
#78549=CARTESIAN_POINT('Ctrl Pts',(19.637133811473,-20.8736725923874,-21.253852858953));
#78550=CARTESIAN_POINT('Ctrl Pts',(19.4859266550713,-20.9377197301571,-21.2648703773371));
#78551=CARTESIAN_POINT('Ctrl Pts',(19.219052034435,-21.0158563298912,-21.2830111543928));
#78552=CARTESIAN_POINT('Ctrl Pts',(19.1068139143064,-21.0390542714415,-21.2902909846396));
#78553=CARTESIAN_POINT('Ctrl Pts',(18.9790747482339,-21.0548149962688,-21.2981493777544));
#78554=CARTESIAN_POINT('Ctrl Pts',(18.9648977846834,-21.0564188673792,-21.2990159480795));
#78555=CARTESIAN_POINT('Ctrl Pts',(18.9422913718601,-21.0587451792277,-21.3003891073552));
#78556=CARTESIAN_POINT('Ctrl Pts',(18.933872123076,-21.0595606001829,-21.3008986009188));
#78557=CARTESIAN_POINT('Ctrl Pts',(18.9190045968664,-21.0609106572923,-21.301795011777));
#78558=CARTESIAN_POINT('Ctrl Pts',(18.9125583738391,-21.0614662286638,-21.3021825812551));
#78559=CARTESIAN_POINT('Ctrl Pts',(18.8992101478361,-21.0625550281615,-21.3029828981746));
#78560=CARTESIAN_POINT('Ctrl Pts',(18.8923078657119,-21.0630839730446,-21.3033955068471));
#78561=CARTESIAN_POINT('Ctrl Pts',(18.8745625674112,-21.0643563347267,-21.3044532004385));
#78562=CARTESIAN_POINT('Ctrl Pts',(18.8637161113918,-21.0650501312834,-21.3050967260024));
#78563=CARTESIAN_POINT('Ctrl Pts',(18.8182383210541,-21.0676076382278,-21.307782974265));
#78564=CARTESIAN_POINT('Ctrl Pts',(18.7835680456845,-21.0687038019414,-21.3098016620234));
#78565=CARTESIAN_POINT('Ctrl Pts',(18.6930029358653,-21.0693405949672,-21.3150107968876));
#78566=CARTESIAN_POINT('Ctrl Pts',(18.637124726158,-21.0675206934193,-21.3181606462064));
#78567=CARTESIAN_POINT('Ctrl Pts',(18.3834490253179,-21.0491849388313,-21.3322947223814));
#78568=CARTESIAN_POINT('Ctrl Pts',(18.1885432697126,-21.007122439283,-21.3426052567678));
#78569=CARTESIAN_POINT('Ctrl Pts',(17.9724265963165,-20.9275285600448,-21.3558294338989));
#78570=CARTESIAN_POINT('Ctrl Pts',(17.9427393213528,-20.9158262226672,-21.3576899849543));
#78571=CARTESIAN_POINT('Ctrl Pts',(17.9070443376312,-20.9008149796076,-21.3599939051993));
#78572=CARTESIAN_POINT('Ctrl Pts',(17.9007719012643,-20.8981414195499,-21.3604012976031));
#78573=CARTESIAN_POINT('Ctrl Pts',(17.8904606766489,-20.8936873824995,-21.3610753741911));
#78574=CARTESIAN_POINT('Ctrl Pts',(17.8864142923849,-20.8919244698782,-21.3613410118751));
#78575=CARTESIAN_POINT('Ctrl Pts',(17.8791233500635,-20.8887208152821,-21.3618217113354));
#78576=CARTESIAN_POINT('Ctrl Pts',(17.8758768732385,-20.8872845532682,-21.362036496941));
#78577=CARTESIAN_POINT('Ctrl Pts',(17.8695652741977,-20.8844732572644,-21.3624555348091));
#78578=CARTESIAN_POINT('Ctrl Pts',(17.8664998554812,-20.8830991129689,-21.3626597245703));
#78579=CARTESIAN_POINT('Ctrl Pts',(17.8574561994662,-20.8790192075954,-21.3632640852242));
#78580=CARTESIAN_POINT('Ctrl Pts',(17.8514873236632,-20.8762929699415,-21.3636654975209));
#78581=CARTESIAN_POINT('Ctrl Pts',(17.8231312490501,-20.8631818732934,-21.3655841969521));
#78582=CARTESIAN_POINT('Ctrl Pts',(17.8009151237192,-20.8524342987479,-21.3671223449005));
#78583=CARTESIAN_POINT('Ctrl Pts',(17.7387161835997,-20.8209905937864,-21.3715175782383));
#78584=CARTESIAN_POINT('Ctrl Pts',(17.6991998507323,-20.7994046232302,-21.3744154243017));
#78585=CARTESIAN_POINT('Ctrl Pts',(17.5784756444411,-20.7283695383323,-21.3835372013532));
#78586=CARTESIAN_POINT('Ctrl Pts',(17.4998886812953,-20.6746996142006,-21.3898623194032));
#78587=CARTESIAN_POINT('Ctrl Pts',(17.3073656436015,-20.523263804994,-21.4060185095361));
#78588=CARTESIAN_POINT('Ctrl Pts',(17.1997104958011,-20.4183312382949,-21.4156928955309));
#78589=CARTESIAN_POINT('Ctrl Pts',(17.095014197546,-20.2920052958014,-21.4257089375579));
#78590=CARTESIAN_POINT('Ctrl Pts',(17.0861067224719,-20.2810358966566,-21.4265670572121));
#78591=CARTESIAN_POINT('Ctrl Pts',(17.0720934640097,-20.2634213138756,-21.4279268883053));
#78592=CARTESIAN_POINT('Ctrl Pts',(17.0669162730053,-20.2568337239732,-21.4284314759978));
#78593=CARTESIAN_POINT('Ctrl Pts',(17.0578483390237,-20.2451533856107,-21.4293192434309));
#78594=CARTESIAN_POINT('Ctrl Pts',(17.0539413835426,-20.2400734124992,-21.4297030690241));
#78595=CARTESIAN_POINT('Ctrl Pts',(17.045902570356,-20.2295222394312,-21.4304956168759));
#78596=CARTESIAN_POINT('Ctrl Pts',(17.041774097975,-20.2240485456295,-21.4309042020828));
#78597=CARTESIAN_POINT('Ctrl Pts',(17.0312338007196,-20.2099316687941,-21.4319514451176));
#78598=CARTESIAN_POINT('Ctrl Pts',(17.0248611085845,-20.2012594082619,-21.4325885617407));
#78599=CARTESIAN_POINT('Ctrl Pts',(16.998453023494,-20.1647417077541,-21.4352459079932));
#78600=CARTESIAN_POINT('Ctrl Pts',(16.9790291445457,-20.1364590544198,-21.4372424437986));
#78601=CARTESIAN_POINT('Ctrl Pts',(16.9301557786891,-20.0614521293199,-21.4423912249897));
#78602=CARTESIAN_POINT('Ctrl Pts',(16.9018314005475,-20.0140248948994,-21.4455035981185));
#78603=CARTESIAN_POINT('Ctrl Pts',(16.8405504664467,-19.9016494245699,-21.4526165630114));
#78604=CARTESIAN_POINT('Ctrl Pts',(16.809025281103,-19.8360012188719,-21.4565793344688));
#78605=CARTESIAN_POINT('Ctrl Pts',(16.7684068302387,-19.7388850155352,-21.4622948397039));
#78606=CARTESIAN_POINT('Ctrl Pts',(16.7565625548255,-19.7086277997814,-21.4640561247131));
#78607=CARTESIAN_POINT('Ctrl Pts',(16.7454194499919,-19.678110457251,-21.4658225324418));
#78608=CARTESIAN_POINT('Ctrl Pts',(16.745419449923,-19.6781104570625,-21.2464098137458));
#78609=CARTESIAN_POINT('Ctrl Pts',(16.7527636255383,-19.6982237671557,-21.2451662593623));
#78610=CARTESIAN_POINT('Ctrl Pts',(16.7604124473736,-19.7182242707579,-21.2439084485296));
#78611=CARTESIAN_POINT('Ctrl Pts',(16.7710457043463,-19.7448124735101,-21.2422034349802));
#78612=CARTESIAN_POINT('Ctrl Pts',(16.7737624299642,-19.7515060040884,-21.241771382987));
#78613=CARTESIAN_POINT('Ctrl Pts',(16.7780760232234,-19.7619797753612,-21.241090700836));
#78614=CARTESIAN_POINT('Ctrl Pts',(16.7796497446164,-19.7657695730657,-21.2408434511686));
#78615=CARTESIAN_POINT('Ctrl Pts',(16.7826135719917,-19.7728488054705,-21.2403797672208));
#78616=CARTESIAN_POINT('Ctrl Pts',(16.7840009862905,-19.7761393078273,-21.2401634966048));
#78617=CARTESIAN_POINT('Ctrl Pts',(16.7871885268885,-19.7836460214901,-21.2396684192655));
#78618=CARTESIAN_POINT('Ctrl Pts',(16.7889940230661,-19.7878598959617,-21.2393892888697));
#78619=CARTESIAN_POINT('Ctrl Pts',(16.7945883559339,-19.8008003200464,-21.2385284233604));
#78620=CARTESIAN_POINT('Ctrl Pts',(16.798422280582,-19.809507080309,-21.2379440407997));
#78621=CARTESIAN_POINT('Ctrl Pts',(16.851424787907,-19.927708005361,-21.2299430499284));
#78622=CARTESIAN_POINT('Ctrl Pts',(16.9097546367613,-20.0328412114739,-21.222046249565));
#78623=CARTESIAN_POINT('Ctrl Pts',(17.0373577043262,-20.2228030219735,-21.2069280582549));
#78624=CARTESIAN_POINT('Ctrl Pts',(17.1049303948756,-20.3083447574048,-21.1997344815819));
#78625=CARTESIAN_POINT('Ctrl Pts',(17.2157356654224,-20.4283225590371,-21.1892424346618));
#78626=CARTESIAN_POINT('Ctrl Pts',(17.2542172143822,-20.4668922699957,-21.1857953784389));
#78627=CARTESIAN_POINT('Ctrl Pts',(17.310715173096,-20.5193098408933,-21.1810061335353));
#78628=CARTESIAN_POINT('Ctrl Pts',(17.327529678,-20.5344162318493,-21.1796125375574));
#78629=CARTESIAN_POINT('Ctrl Pts',(17.3536852690417,-20.5571684568501,-21.1774922913361));
#78630=CARTESIAN_POINT('Ctrl Pts',(17.3628547924315,-20.5650081712708,-21.1767576852892));
#78631=CARTESIAN_POINT('Ctrl Pts',(17.3799883106688,-20.579405219871,-21.1754009323345));
#78632=CARTESIAN_POINT('Ctrl Pts',(17.3879341446112,-20.5859835137969,-21.1747779378894));
#78633=CARTESIAN_POINT('Ctrl Pts',(17.401101328972,-20.5967232909328,-21.1737556316717));
#78634=CARTESIAN_POINT('Ctrl Pts',(17.40629478113,-20.6009185620697,-21.1733549545101));
#78635=CARTESIAN_POINT('Ctrl Pts',(17.4165517911981,-20.6091242977851,-21.1725685706118));
#78636=CARTESIAN_POINT('Ctrl Pts',(17.4216140267495,-20.6131362917674,-21.1721828049434));
#78637=CARTESIAN_POINT('Ctrl Pts',(17.4333466046785,-20.6223476493514,-21.1712940795849));
#78638=CARTESIAN_POINT('Ctrl Pts',(17.4400299285359,-20.6275303583568,-21.1707917859344));
#78639=CARTESIAN_POINT('Ctrl Pts',(17.4580911914217,-20.6413637847229,-21.1694448336001));
#78640=CARTESIAN_POINT('Ctrl Pts',(17.4695261004689,-20.6499396506526,-21.1686031158945));
#78641=CARTESIAN_POINT('Ctrl Pts',(17.5749932258708,-20.7273806910733,-21.160937700305));
#78642=CARTESIAN_POINT('Ctrl Pts',(17.6744809196387,-20.7884906340283,-21.1544288556416));
#78643=CARTESIAN_POINT('Ctrl Pts',(17.924069777241,-20.9147306291121,-21.1391142841543));
#78644=CARTESIAN_POINT('Ctrl Pts',(18.0776371463879,-20.9712756947479,-21.1304943329389));
#78645=CARTESIAN_POINT('Ctrl Pts',(18.2675045627371,-21.0172146651587,-21.1192744585072));
#78646=CARTESIAN_POINT('Ctrl Pts',(18.2990256928423,-21.0240826969062,-21.1173926007298));
#78647=CARTESIAN_POINT('Ctrl Pts',(18.3377825562967,-21.0316040355389,-21.1150418377291));
#78648=CARTESIAN_POINT('Ctrl Pts',(18.3448825713782,-21.0329442161303,-21.1146096851959));
#78649=CARTESIAN_POINT('Ctrl Pts',(18.3560299249902,-21.0349893181378,-21.1139286267818));
#78650=CARTESIAN_POINT('Ctrl Pts',(18.3600727685966,-21.035718863483,-21.1136810984186));
#78651=CARTESIAN_POINT('Ctrl Pts',(18.3676364747793,-21.0370610396962,-21.1132169728438));
#78652=CARTESIAN_POINT('Ctrl Pts',(18.371156773337,-21.0376765243169,-21.1130005399103));
#78653=CARTESIAN_POINT('Ctrl Pts',(18.3792007882109,-21.0390619483075,-21.1125050327027));
#78654=CARTESIAN_POINT('Ctrl Pts',(18.3837254427443,-21.0398260919873,-21.1122256346616));
#78655=CARTESIAN_POINT('Ctrl Pts',(18.3955457486324,-21.0417828521001,-21.1114940145469));
#78656=CARTESIAN_POINT('Ctrl Pts',(18.4028451529991,-21.0429519633025,-21.111040513112));
#78657=CARTESIAN_POINT('Ctrl Pts',(18.4508057912219,-21.0503761594953,-21.1080502836029));
#78658=CARTESIAN_POINT('Ctrl Pts',(18.4916330076758,-21.0554826346607,-21.1054554074111));
#78659=CARTESIAN_POINT('Ctrl Pts',(18.6965047503879,-21.0750638190948,-21.0922721036984));
#78660=CARTESIAN_POINT('Ctrl Pts',(18.8616967296209,-21.0715523984599,-21.0811771138372));
#78661=CARTESIAN_POINT('Ctrl Pts',(19.1200097550326,-21.0357277959425,-21.0642237547855));
#78662=CARTESIAN_POINT('Ctrl Pts',(19.214203247993,-21.0160577126116,-21.0581157048154));
#78663=CARTESIAN_POINT('Ctrl Pts',(19.3274215847616,-20.9842404114641,-21.0508911665999));
#78664=CARTESIAN_POINT('Ctrl Pts',(19.3480087226243,-20.9781153987704,-21.0495819749366));
#78665=CARTESIAN_POINT('Ctrl Pts',(19.3771092351514,-20.9689732153594,-21.0477371963725));
#78666=CARTESIAN_POINT('Ctrl Pts',(19.3857014885393,-20.9662133982257,-21.0471932264209));
#78667=CARTESIAN_POINT('Ctrl Pts',(19.4004794163168,-20.9613622912994,-21.0462588160613));
#78668=CARTESIAN_POINT('Ctrl Pts',(19.4066734945251,-20.9592971880905,-21.0458675197625));
#78669=CARTESIAN_POINT('Ctrl Pts',(19.418505085799,-20.9552916244121,-21.0451207326991));
#78670=CARTESIAN_POINT('Ctrl Pts',(19.4241441400081,-20.9533559433685,-21.0447650884325));
#78671=CARTESIAN_POINT('Ctrl Pts',(19.4387648011857,-20.9482680628082,-21.04384368301));
#78672=CARTESIAN_POINT('Ctrl Pts',(19.4477335235512,-20.9450790414422,-21.0432791473921));
#78673=CARTESIAN_POINT('Ctrl Pts',(19.4781319616414,-20.9340387192806,-21.0413677901164));
#78674=CARTESIAN_POINT('Ctrl Pts',(19.4994565717454,-20.925901253218,-21.0400304982196));
#78675=CARTESIAN_POINT('Ctrl Pts',(19.6856656302613,-20.8513723491884,-21.0283736817803));
#78676=CARTESIAN_POINT('Ctrl Pts',(19.8417083679873,-20.7648076439597,-21.0188279067583));
#78677=CARTESIAN_POINT('Ctrl Pts',(20.0540512763229,-20.609244020643,-21.0045003305619));
#78678=CARTESIAN_POINT('Ctrl Pts',(20.1198668693067,-20.5546115656391,-20.9998169422385));
#78679=CARTESIAN_POINT('Ctrl Pts',(20.2094976760322,-20.4705508503281,-20.9927982572618));
#78680=CARTESIAN_POINT('Ctrl Pts',(20.2361143414899,-20.4442272596,-20.9906233506109));
#78681=CARTESIAN_POINT('Ctrl Pts',(20.2672420844694,-20.4117652877376,-20.9879473431042));
#78682=CARTESIAN_POINT('Ctrl Pts',(20.2724374979456,-20.4062888454141,-20.9874960908837));
#78683=CARTESIAN_POINT('Ctrl Pts',(20.2804620690263,-20.3977390903764,-20.9867916868579));
#78684=CARTESIAN_POINT('Ctrl Pts',(20.2833116672582,-20.3946849293539,-20.9865400749659));
#78685=CARTESIAN_POINT('Ctrl Pts',(20.2885756885573,-20.3890094395748,-20.986072495382));
#78686=CARTESIAN_POINT('Ctrl Pts',(20.2909925384615,-20.3863904403859,-20.9858567178472));
#78687=CARTESIAN_POINT('Ctrl Pts',(20.2964366074389,-20.3804610496373,-20.9853681829381));
#78688=CARTESIAN_POINT('Ctrl Pts',(20.2994599073349,-20.3771471503904,-20.9850951364374));
#78689=CARTESIAN_POINT('Ctrl Pts',(20.3083384151675,-20.3673529006457,-20.9842881916601));
#78690=CARTESIAN_POINT('Ctrl Pts',(20.3141639959375,-20.3608459882982,-20.9837521483915));
#78691=CARTESIAN_POINT('Ctrl Pts',(20.35555109441,-20.3140388342587,-20.9798977671729));
#78692=CARTESIAN_POINT('Ctrl Pts',(20.3896037507722,-20.272436632768,-20.9764808890683));
#78693=CARTESIAN_POINT('Ctrl Pts',(20.5153555542102,-20.1062850790474,-20.963010250249));
#78694=CARTESIAN_POINT('Ctrl Pts',(20.5948877805355,-19.9731278325685,-20.9526197441071));
#78695=CARTESIAN_POINT('Ctrl Pts',(20.6978946004503,-19.7479012118729,-20.9365438462385));
#78696=CARTESIAN_POINT('Ctrl Pts',(20.7309677614263,-19.6608472764353,-20.930640761115));
#78697=CARTESIAN_POINT('Ctrl Pts',(20.7643902521413,-19.5517081693673,-20.9236315561303));
#78698=CARTESIAN_POINT('Ctrl Pts',(20.7702684340306,-19.5314353972673,-20.9223453115321));
#78699=CARTESIAN_POINT('Ctrl Pts',(20.7782090523954,-19.5024349587697,-20.9205270526351));
#78700=CARTESIAN_POINT('Ctrl Pts',(20.7805206049522,-19.4937773630344,-20.9199869767051));
#78701=CARTESIAN_POINT('Ctrl Pts',(20.7844182241569,-19.4787984199277,-20.9190572054619));
#78702=CARTESIAN_POINT('Ctrl Pts',(20.786030185184,-19.4724839956821,-20.9186666759323));
#78703=CARTESIAN_POINT('Ctrl Pts',(20.7890639105027,-19.4603670061292,-20.9179199535675));
#78704=CARTESIAN_POINT('Ctrl Pts',(20.7904903183595,-19.4545656780874,-20.917563613984));
#78705=CARTESIAN_POINT('Ctrl Pts',(20.7941422189614,-19.439437159926,-20.9166373747414));
#78706=CARTESIAN_POINT('Ctrl Pts',(20.7963289478639,-19.4301006825188,-20.9160687273879));
#78707=CARTESIAN_POINT('Ctrl Pts',(20.8036013246229,-19.3980719070197,-20.9141279054184));
#78708=CARTESIAN_POINT('Ctrl Pts',(20.8083765840992,-19.3753103346977,-20.9127656733812));
#78709=CARTESIAN_POINT('Ctrl Pts',(20.8452419952168,-19.1839497769598,-20.9014445826094));
#78710=CARTESIAN_POINT('Ctrl Pts',(20.8570962745385,-19.0121042519913,-20.8921988008969));
#78711=CARTESIAN_POINT('Ctrl Pts',(20.8433537383876,-18.7510767321435,-20.8779847795815));
#78712=CARTESIAN_POINT('Ctrl Pts',(20.8329414366662,-18.6618523809092,-20.8730801985421));
#78713=CARTESIAN_POINT('Ctrl Pts',(20.8100173192434,-18.5356780504849,-20.8657635877288));
#78714=CARTESIAN_POINT('Ctrl Pts',(20.8021016158896,-18.497987707128,-20.8635279236192));
#78715=CARTESIAN_POINT('Ctrl Pts',(20.7913965946638,-18.4531351286419,-20.8607845954464));
#78716=CARTESIAN_POINT('Ctrl Pts',(20.7895901299587,-18.4457430284501,-20.8603297510928));
#78717=CARTESIAN_POINT('Ctrl Pts',(20.786727235976,-18.4342959800424,-20.8596209514185));
#78718=CARTESIAN_POINT('Ctrl Pts',(20.785698533698,-18.4302340719048,-20.8593685673205));
#78719=CARTESIAN_POINT('Ctrl Pts',(20.783772814819,-18.4227239828828,-20.8589002740831));
#78720=CARTESIAN_POINT('Ctrl Pts',(20.7828791498592,-18.4192750021244,-20.8586845597255));
#78721=CARTESIAN_POINT('Ctrl Pts',(20.7808448361325,-18.4115046792871,-20.8581971019553));
#78722=CARTESIAN_POINT('Ctrl Pts',(20.7796992137111,-18.4071847092005,-20.8579250751033));
#78723=CARTESIAN_POINT('Ctrl Pts',(20.7762947715889,-18.3945092076618,-20.8571239696015));
#78724=CARTESIAN_POINT('Ctrl Pts',(20.7739984095908,-18.3861639808309,-20.8565927917065));
#78725=CARTESIAN_POINT('Ctrl Pts',(20.7575867030867,-18.3279207456179,-20.8528604603406));
#78726=CARTESIAN_POINT('Ctrl Pts',(20.7416944489696,-18.2785461417397,-20.8495675614366));
#78727=CARTESIAN_POINT('Ctrl Pts',(20.7166531857815,-18.2095445505901,-20.8448281378035));
#78728=CARTESIAN_POINT('Ctrl Pts',(20.7089899557182,-18.1893936925551,-20.8434269961101));
#78729=CARTESIAN_POINT('Ctrl Pts',(20.6839298885056,-18.1264095481897,-20.839000316131));
#78730=CARTESIAN_POINT('Ctrl Pts',(20.6654372282101,-18.0840275359166,-20.8359523796574));
#78731=CARTESIAN_POINT('Ctrl Pts',(20.5985795379597,-17.9435401747494,-20.8256748341888));
#78732=CARTESIAN_POINT('Ctrl Pts',(20.5440021712157,-17.8485763827665,-20.8184438751073));
#78733=CARTESIAN_POINT('Ctrl Pts',(20.4512734533136,-17.7127688611721,-20.8078740102934));
#78734=CARTESIAN_POINT('Ctrl Pts',(20.4184542417522,-17.6685138660085,-20.8043867223197));
#78735=CARTESIAN_POINT('Ctrl Pts',(20.3624588554348,-17.5988604549313,-20.798831714606));
#78736=CARTESIAN_POINT('Ctrl Pts',(20.3403266229736,-17.5726596255167,-20.7967256035217));
#78737=CARTESIAN_POINT('Ctrl Pts',(20.3103939648875,-17.5389225539677,-20.7939898698394));
#78738=CARTESIAN_POINT('Ctrl Pts',(20.3031594613637,-17.5308932508023,-20.7933369250034));
#78739=CARTESIAN_POINT('Ctrl Pts',(20.2912071369385,-17.5178303740107,-20.7922714805455));
#78740=CARTESIAN_POINT('Ctrl Pts',(20.2865257041073,-17.5127639098186,-20.791857452064));
#78741=CARTESIAN_POINT('Ctrl Pts',(20.2774141969953,-17.5029992018415,-20.791057900251));
#78742=CARTESIAN_POINT('Ctrl Pts',(20.2729872313962,-17.4982981737729,-20.7906722507226));
#78743=CARTESIAN_POINT('Ctrl Pts',(20.2627134842322,-17.4874879351667,-20.7897837131695));
#78744=CARTESIAN_POINT('Ctrl Pts',(20.2568514447301,-17.4813933274447,-20.7892814915424));
#78745=CARTESIAN_POINT('Ctrl Pts',(20.2409826754627,-17.4650916208797,-20.7879345617977));
#78746=CARTESIAN_POINT('Ctrl Pts',(20.2309087182202,-17.4549503627865,-20.7870927968686));
#78747=CARTESIAN_POINT('Ctrl Pts',(20.1373585324325,-17.3626637221725,-20.7793944133068));
#78748=CARTESIAN_POINT('Ctrl Pts',(20.0472983860005,-17.2874707532506,-20.772856086988));
#78749=CARTESIAN_POINT('Ctrl Pts',(19.8174082193721,-17.1258649205835,-20.7574736519427));
#78750=CARTESIAN_POINT('Ctrl Pts',(19.6728755528101,-17.0475202675859,-20.7488161747321));
#78751=CARTESIAN_POINT('Ctrl Pts',(19.4917873481704,-16.9750269574099,-20.7376001066905));
#78752=CARTESIAN_POINT('Ctrl Pts',(19.4625462434253,-16.96406533958,-20.7357770075369));
#78753=CARTESIAN_POINT('Ctrl Pts',(19.4263259399395,-16.9513938616092,-20.7334917899725));
#78754=CARTESIAN_POINT('Ctrl Pts',(19.4195648475323,-16.9490669096079,-20.733064074883));
#78755=CARTESIAN_POINT('Ctrl Pts',(19.4089178832912,-16.9454627884744,-20.7323885498455));
#78756=CARTESIAN_POINT('Ctrl Pts',(19.4050398047849,-16.9441625289466,-20.7321420823351));
#78757=CARTESIAN_POINT('Ctrl Pts',(19.3977650651089,-16.9417468517903,-20.7316789284496));
#78758=CARTESIAN_POINT('Ctrl Pts',(19.3943693385109,-16.9406287966596,-20.7314624001223));
#78759=CARTESIAN_POINT('Ctrl Pts',(19.3865863945297,-16.9380880681282,-20.730965362684));
#78760=CARTESIAN_POINT('Ctrl Pts',(19.3821973626667,-16.9366711311145,-20.7306845213098));
#78761=CARTESIAN_POINT('Ctrl Pts',(19.3686045361586,-16.9323318755351,-20.729813141699));
#78762=CARTESIAN_POINT('Ctrl Pts',(19.3593855013232,-16.9294582286346,-20.7292198629124));
#78763=CARTESIAN_POINT('Ctrl Pts',(19.2481011210076,-16.8956035861596,-20.7220335718439));
#78764=CARTESIAN_POINT('Ctrl Pts',(19.143866171573,-16.8723196181018,-20.7150595624586));
#78765=CARTESIAN_POINT('Ctrl Pts',(18.9301039790352,-16.8412670820782,-20.7008100918327));
#78766=CARTESIAN_POINT('Ctrl Pts',(18.8208096022208,-16.8339544122939,-20.6935551844458));
#78767=CARTESIAN_POINT('Ctrl Pts',(18.6488221980256,-16.8357876682644,-20.6824362378933));
#78768=CARTESIAN_POINT('Ctrl Pts',(18.5862650049345,-16.8392327544126,-20.6784512271599));
#78769=CARTESIAN_POINT('Ctrl Pts',(18.4991746732176,-16.8479168578278,-20.6729961131759));
#78770=CARTESIAN_POINT('Ctrl Pts',(18.4744464032588,-16.8508239445997,-20.6714575295445));
#78771=CARTESIAN_POINT('Ctrl Pts',(18.4312406014699,-16.8566776976592,-20.6687868410496));
#78772=CARTESIAN_POINT('Ctrl Pts',(18.4127405261699,-16.8594343045438,-20.6676489548771));
#78773=CARTESIAN_POINT('Ctrl Pts',(18.3858544828323,-16.8638054338338,-20.6660030997113));
#78774=CARTESIAN_POINT('Ctrl Pts',(18.3774382982314,-16.8652260296202,-20.665489014493));
#78775=CARTESIAN_POINT('Ctrl Pts',(18.3626811148188,-16.8678088284576,-20.6645895033053));
#78776=CARTESIAN_POINT('Ctrl Pts',(18.356336447432,-16.8689491613225,-20.6642033878881));
#78777=CARTESIAN_POINT('Ctrl Pts',(18.3440146591901,-16.8712219146808,-20.6634546912562));
#78778=CARTESIAN_POINT('Ctrl Pts',(18.3380370223699,-16.8723511527362,-20.6630920129195));
#78779=CARTESIAN_POINT('Ctrl Pts',(18.3237394707411,-16.8751159896875,-20.6622257846882));
#78780=CARTESIAN_POINT('Ctrl Pts',(18.3154243103936,-16.8767758459848,-20.6617230119399));
#78781=CARTESIAN_POINT('Ctrl Pts',(18.2853398289162,-16.8829694302244,-20.6599074343806));
#78782=CARTESIAN_POINT('Ctrl Pts',(18.2636318237767,-16.8877962111729,-20.6586039828981));
#78783=CARTESIAN_POINT('Ctrl Pts',(18.0627480347725,-16.9357964304618,-20.6465932324424));
#78784=CARTESIAN_POINT('Ctrl Pts',(17.8898576569068,-17.0018497835049,-20.6367285525924));
#78785=CARTESIAN_POINT('Ctrl Pts',(17.6564347876173,-17.1279653232637,-20.6222691800986));
#78786=CARTESIAN_POINT('Ctrl Pts',(17.5874485019967,-17.1705211486931,-20.6178175296491));
#78787=CARTESIAN_POINT('Ctrl Pts',(17.4913574344798,-17.2376945439702,-20.6111127763509));
#78788=CARTESIAN_POINT('Ctrl Pts',(17.4621800954307,-17.2592278600716,-20.6090040722916));
#78789=CARTESIAN_POINT('Ctrl Pts',(17.4276696901645,-17.2860930182023,-20.6064014668105));
#78790=CARTESIAN_POINT('Ctrl Pts',(17.4217917968494,-17.2907189948134,-20.6059542803094));
#78791=CARTESIAN_POINT('Ctrl Pts',(17.412681517766,-17.2979674147469,-20.6052548570601));
#78792=CARTESIAN_POINT('Ctrl Pts',(17.4094320752328,-17.300568458408,-20.6050041252277));
#78793=CARTESIAN_POINT('Ctrl Pts',(17.4034133424525,-17.3054153954806,-20.6045373169608));
#78794=CARTESIAN_POINT('Ctrl Pts',(17.4006420477552,-17.3076587082765,-20.6043214252069));
#78795=CARTESIAN_POINT('Ctrl Pts',(17.3943809871138,-17.3127531584176,-20.6038315160248));
#78796=CARTESIAN_POINT('Ctrl Pts',(17.3908946677011,-17.3156084292549,-20.6035572024839));
#78797=CARTESIAN_POINT('Ctrl Pts',(17.3806055013101,-17.3240902151048,-20.6027431824962));
#78798=CARTESIAN_POINT('Ctrl Pts',(17.3738288014987,-17.3297480955845,-20.6022012760981));
#78799=CARTESIAN_POINT('Ctrl Pts',(17.3242100279993,-17.3717043760233,-20.5981920227039));
#78800=CARTESIAN_POINT('Ctrl Pts',(17.2827955738554,-17.4096490180562,-20.5946171851587));
#78801=CARTESIAN_POINT('Ctrl Pts',(17.1985927881025,-17.4931933656554,-20.5869375005044));
#78802=CARTESIAN_POINT('Ctrl Pts',(17.1562146413819,-17.5391359405585,-20.5828222616848));
#78803=CARTESIAN_POINT('Ctrl Pts',(17.0452480438396,-17.670664243137,-20.5714553749442));
#78804=CARTESIAN_POINT('Ctrl Pts',(16.9811726594501,-17.7598153394788,-20.5642057657625));
#78805=CARTESIAN_POINT('Ctrl Pts',(16.8955510661131,-17.9008760083811,-20.5535967706378));
#78806=CARTESIAN_POINT('Ctrl Pts',(16.868681749659,-17.9493311682977,-20.5500891263359));
#78807=CARTESIAN_POINT('Ctrl Pts',(16.8282391527538,-18.0295304688711,-20.5445055504034));
#78808=CARTESIAN_POINT('Ctrl Pts',(16.8134880190854,-18.0606479973414,-20.5423907290272));
#78809=CARTESIAN_POINT('Ctrl Pts',(16.7951057144783,-18.1020028912704,-20.5396455447155));
#78810=CARTESIAN_POINT('Ctrl Pts',(16.7907854902543,-18.1119264846431,-20.5389916547816));
#78811=CARTESIAN_POINT('Ctrl Pts',(16.7838354324334,-18.1282313523914,-20.5379250851755));
#78812=CARTESIAN_POINT('Ctrl Pts',(16.7811604048282,-18.134593037307,-20.5375108700528));
#78813=CARTESIAN_POINT('Ctrl Pts',(16.7760434384849,-18.1469305777582,-20.5367112457338));
#78814=CARTESIAN_POINT('Ctrl Pts',(16.773597634443,-18.152904737874,-20.5363257088402));
#78815=CARTESIAN_POINT('Ctrl Pts',(16.768014752243,-18.1667214821484,-20.5354378421266));
#78816=CARTESIAN_POINT('Ctrl Pts',(16.7648971947904,-18.1745718742755,-20.5349361757676));
#78817=CARTESIAN_POINT('Ctrl Pts',(16.7566421279101,-18.1957273913413,-20.5335916482684));
#78818=CARTESIAN_POINT('Ctrl Pts',(16.7515918944921,-18.2090662674463,-20.5327517142581));
#78819=CARTESIAN_POINT('Ctrl Pts',(16.6965077126158,-18.3591188847362,-20.5233871995423));
#78820=CARTESIAN_POINT('Ctrl Pts',(16.6605663579691,-18.5005981038488,-20.5153746929697));
#78821=CARTESIAN_POINT('Ctrl Pts',(16.6244283768297,-18.7468873155227,-20.5018389966347));
#78822=CARTESIAN_POINT('Ctrl Pts',(16.6169334233456,-18.8500661998662,-20.4962757985682));
#78823=CARTESIAN_POINT('Ctrl Pts',(16.6170394068497,-19.0134280313683,-20.4871374011508));
#78824=CARTESIAN_POINT('Ctrl Pts',(16.6196337803259,-19.0734481173039,-20.4837076718875));
#78825=CARTESIAN_POINT('Ctrl Pts',(16.6255428349298,-19.1422045998558,-20.4796144300126));
#78826=CARTESIAN_POINT('Ctrl Pts',(16.6263673828061,-19.1511335011068,-20.4790796667383));
#78827=CARTESIAN_POINT('Ctrl Pts',(16.6276944058085,-19.1645707388497,-20.478269705438));
#78828=CARTESIAN_POINT('Ctrl Pts',(16.6281546998097,-19.1690832695645,-20.4779968197555));
#78829=CARTESIAN_POINT('Ctrl Pts',(16.6290029491409,-19.1771425004653,-20.4775078228937));
#78830=CARTESIAN_POINT('Ctrl Pts',(16.629385371026,-19.1806897306192,-20.4772920256087));
#78831=CARTESIAN_POINT('Ctrl Pts',(16.6302310228456,-19.1883519364266,-20.4768246509355));
#78832=CARTESIAN_POINT('Ctrl Pts',(16.6306973530491,-19.192466466978,-20.4765729065439));
#78833=CARTESIAN_POINT('Ctrl Pts',(16.6320285817753,-19.2039119860905,-20.475870531854));
#78834=CARTESIAN_POINT('Ctrl Pts',(16.6329197476738,-19.2112397758109,-20.4754184619776));
#78835=CARTESIAN_POINT('Ctrl Pts',(16.6382144752587,-19.2529550243667,-20.4728319164278));
#78836=CARTESIAN_POINT('Ctrl Pts',(16.643423628833,-19.2872327656516,-20.4706561137669));
#78837=CARTESIAN_POINT('Ctrl Pts',(16.6625927921858,-19.3954148933767,-20.4636610241718));
#78838=CARTESIAN_POINT('Ctrl Pts',(16.6796496226979,-19.4687083943756,-20.45873241018));
#78839=CARTESIAN_POINT('Ctrl Pts',(16.7139659294228,-19.5871935575331,-20.4505956064325));
#78840=CARTESIAN_POINT('Ctrl Pts',(16.7289275848391,-19.6329445735838,-20.4474103338749));
#78841=CARTESIAN_POINT('Ctrl Pts',(16.7454193204093,-19.6781101023665,-20.4442392291799));
#78842=CARTESIAN_POINT('Origin',(18.734,-18.952,0.));
#78843=CARTESIAN_POINT('',(16.7454194498907,-19.678110456974,-19.6425235871583));
#78844=CARTESIAN_POINT('',(16.7452305273115,-19.6781794125984,-19.8664843216556));
#78845=CARTESIAN_POINT('',(16.7454194499637,-19.6781104571739,0.));
#78846=CARTESIAN_POINT('',(16.6200797572234,-18.9511717419853,-19.9109991808971));
#78847=CARTESIAN_POINT('Ctrl Pts',(16.7452305273115,-19.6781794125984,-19.8664843216556));
#78848=CARTESIAN_POINT('Ctrl Pts',(16.6631151187494,-19.4459846869538,-19.8813041214296));
#78849=CARTESIAN_POINT('Ctrl Pts',(16.6210474187959,-19.1984405238965,-19.8961239212035));
#78850=CARTESIAN_POINT('Ctrl Pts',(16.6201759917111,-18.9511685861839,-19.9109437209775));
#78851=CARTESIAN_POINT('Ctrl Pts',(16.6170001249218,-18.9512727318511,-19.9127739724915));
#78852=CARTESIAN_POINT('Ctrl Pts',(16.6170670032748,-18.7565969919401,-19.9239833310404));
#78853=CARTESIAN_POINT('Ctrl Pts',(16.6439835682874,-18.5628628690705,-19.9342646472684));
#78854=CARTESIAN_POINT('Ctrl Pts',(16.7140733703376,-18.3151987866819,-19.9484105632264));
#78855=CARTESIAN_POINT('Ctrl Pts',(16.7338151550543,-18.2556675991902,-19.951902303785));
#78856=CARTESIAN_POINT('Ctrl Pts',(16.7671936907326,-18.1682155204606,-19.9572865138648));
#78857=CARTESIAN_POINT('Ctrl Pts',(16.7788510580608,-18.139573045479,-19.9590922814678));
#78858=CARTESIAN_POINT('Ctrl Pts',(16.793961811212,-18.1046561292592,-19.9613581669638));
#78859=CARTESIAN_POINT('Ctrl Pts',(16.7968258157541,-18.0981288236282,-19.9617845621696));
#78860=CARTESIAN_POINT('Ctrl Pts',(16.8013829440265,-18.0878836865476,-19.962458450798));
#78861=CARTESIAN_POINT('Ctrl Pts',(16.8030539889759,-18.0841560105205,-19.9627046122851));
#78862=CARTESIAN_POINT('Ctrl Pts',(16.8062079245958,-18.0771745888939,-19.9631674992383));
#78863=CARTESIAN_POINT('Ctrl Pts',(16.8076882729554,-18.0739197556721,-19.963384068519));
#78864=CARTESIAN_POINT('Ctrl Pts',(16.8111000205154,-18.0664685160747,-19.9638816023128));
#78865=CARTESIAN_POINT('Ctrl Pts',(16.8130369085069,-18.062274682662,-19.9641629017101));
#78866=CARTESIAN_POINT('Ctrl Pts',(16.8190812886983,-18.0492988732612,-19.9650371083213));
#78867=CARTESIAN_POINT('Ctrl Pts',(16.8232353258609,-18.0405388944304,-19.9656327814039));
#78868=CARTESIAN_POINT('Ctrl Pts',(16.8705046782861,-17.9426012766077,-19.9723517442861));
#78869=CARTESIAN_POINT('Ctrl Pts',(16.9197630785505,-17.8565364755763,-19.9788044444127));
#78870=CARTESIAN_POINT('Ctrl Pts',(17.0685517912955,-17.6342992449471,-19.9964225358484));
#78871=CARTESIAN_POINT('Ctrl Pts',(17.1786301555595,-17.5060074329291,-20.007610743824));
#78872=CARTESIAN_POINT('Ctrl Pts',(17.3256262175747,-17.3711346946008,-20.0201376411174));
#78873=CARTESIAN_POINT('Ctrl Pts',(17.3489492164882,-17.350661088638,-20.0220662574656));
#78874=CARTESIAN_POINT('Ctrl Pts',(17.3843093416891,-17.3209716955516,-20.0249047609683));
#78875=CARTESIAN_POINT('Ctrl Pts',(17.3960081347465,-17.3113611030345,-20.025830467425));
#78876=CARTESIAN_POINT('Ctrl Pts',(17.414908947366,-17.2961706735294,-20.0273049894154));
#78877=CARTESIAN_POINT('Ctrl Pts',(17.4220454704626,-17.2905105236463,-20.027857017166));
#78878=CARTESIAN_POINT('Ctrl Pts',(17.4357263538302,-17.2798029908296,-20.0289063875791));
#78879=CARTESIAN_POINT('Ctrl Pts',(17.4422641581444,-17.2747475396626,-20.029404046488));
#78880=CARTESIAN_POINT('Ctrl Pts',(17.4537916361757,-17.2659411317145,-20.0302749183255));
#78881=CARTESIAN_POINT('Ctrl Pts',(17.4587685760821,-17.2621737429912,-20.0306487777281));
#78882=CARTESIAN_POINT('Ctrl Pts',(17.4686241248444,-17.2547817372316,-20.0313849420241));
#78883=CARTESIAN_POINT('Ctrl Pts',(17.473501821549,-17.2511560094449,-20.0317472882647));
#78884=CARTESIAN_POINT('Ctrl Pts',(17.4852043815327,-17.2425351623169,-20.0326119127962));
#78885=CARTESIAN_POINT('Ctrl Pts',(17.492043730996,-17.2375598123545,-20.0331134205157));
#78886=CARTESIAN_POINT('Ctrl Pts',(17.5168596014723,-17.2197336990024,-20.034919581753));
#78887=CARTESIAN_POINT('Ctrl Pts',(17.5350076330159,-17.2071233151211,-20.0362150101887));
#78888=CARTESIAN_POINT('Ctrl Pts',(17.7074294876819,-17.0912744087843,-20.0482965234404));
#78889=CARTESIAN_POINT('Ctrl Pts',(17.8744496948748,-17.0084655834537,-20.0582255373285));
#78890=CARTESIAN_POINT('Ctrl Pts',(18.1259660093946,-16.9226151349315,-20.072713585799));
#78891=CARTESIAN_POINT('Ctrl Pts',(18.2031933790864,-16.9010610467242,-20.0771197353448));
#78892=CARTESIAN_POINT('Ctrl Pts',(18.3166409704104,-16.876235516632,-20.0837626423482));
#78893=CARTESIAN_POINT('Ctrl Pts',(18.3520210311286,-16.8694346423479,-20.0858580509248));
#78894=CARTESIAN_POINT('Ctrl Pts',(18.3949201538196,-16.8623183023126,-20.0884459112971));
#78895=CARTESIAN_POINT('Ctrl Pts',(18.4022916952279,-16.8611355049851,-20.0888922652693));
#78896=CARTESIAN_POINT('Ctrl Pts',(18.4137793677927,-16.8593545340618,-20.0895906696082));
#78897=CARTESIAN_POINT('Ctrl Pts',(18.4178913501114,-16.8587294441031,-20.0898412222025));
#78898=CARTESIAN_POINT('Ctrl Pts',(18.4255321164967,-16.8575909471096,-20.0903078769221));
#78899=CARTESIAN_POINT('Ctrl Pts',(18.4290603652509,-16.857074336752,-20.0905237954991));
#78900=CARTESIAN_POINT('Ctrl Pts',(18.4370546676644,-16.8559244249816,-20.091013998559));
#78901=CARTESIAN_POINT('Ctrl Pts',(18.4415214277539,-16.8552964848385,-20.0912885806234));
#78902=CARTESIAN_POINT('Ctrl Pts',(18.4530601951649,-16.8537119466705,-20.0919996018318));
#78903=CARTESIAN_POINT('Ctrl Pts',(18.4601350276012,-16.8527768336195,-20.0924372080098));
#78904=CARTESIAN_POINT('Ctrl Pts',(18.5036224153015,-16.8472524836331,-20.0951366607305));
#78905=CARTESIAN_POINT('Ctrl Pts',(18.5401421550111,-16.843575303544,-20.0974447813846));
#78906=CARTESIAN_POINT('Ctrl Pts',(18.7466342443177,-16.828193311188,-20.1106595079955));
#78907=CARTESIAN_POINT('Ctrl Pts',(18.9174369828871,-16.8360915855324,-20.122154853729));
#78908=CARTESIAN_POINT('Ctrl Pts',(19.1796012984132,-16.8802268205788,-20.1394324934186));
#78909=CARTESIAN_POINT('Ctrl Pts',(19.2725816120223,-16.9024296220449,-20.1454987964668));
#78910=CARTESIAN_POINT('Ctrl Pts',(19.3841900256898,-16.9372047258563,-20.1526795589692));
#78911=CARTESIAN_POINT('Ctrl Pts',(19.404526438532,-16.9438811254705,-20.1539841317236));
#78912=CARTESIAN_POINT('Ctrl Pts',(19.4332771835243,-16.9538054070952,-20.1558235785827));
#78913=CARTESIAN_POINT('Ctrl Pts',(19.4417768933293,-16.9568002396486,-20.1563667706154));
#78914=CARTESIAN_POINT('Ctrl Pts',(19.4563991489929,-16.9620575214803,-20.1573002552613));
#78915=CARTESIAN_POINT('Ctrl Pts',(19.462530780882,-16.964294161333,-20.1576913994153));
#78916=CARTESIAN_POINT('Ctrl Pts',(19.4742457579964,-16.9686289324353,-20.1584381748218));
#78917=CARTESIAN_POINT('Ctrl Pts',(19.4798307625224,-16.9707223696108,-20.1587939582294));
#78918=CARTESIAN_POINT('Ctrl Pts',(19.4943187914687,-16.9762228857185,-20.1597163248234));
#78919=CARTESIAN_POINT('Ctrl Pts',(19.5032078468509,-16.9796665690507,-20.1602816771984));
#78920=CARTESIAN_POINT('Ctrl Pts',(19.5333783743245,-16.991589837711,-20.1621988857278));
#78921=CARTESIAN_POINT('Ctrl Pts',(19.554545808818,-17.000354943732,-20.1635411310891));
#78922=CARTESIAN_POINT('Ctrl Pts',(19.7375892096665,-17.0796550024494,-20.1751337316173));
#78923=CARTESIAN_POINT('Ctrl Pts',(19.8901913225283,-17.1698396917425,-20.1846222462391));
#78924=CARTESIAN_POINT('Ctrl Pts',(20.0980331049384,-17.3307226306215,-20.1989258069311));
#78925=CARTESIAN_POINT('Ctrl Pts',(20.1629359992613,-17.3876259465707,-20.2036494651612));
#78926=CARTESIAN_POINT('Ctrl Pts',(20.2509103524937,-17.4748107899274,-20.210722456218));
#78927=CARTESIAN_POINT('Ctrl Pts',(20.2769252789562,-17.5020047690118,-20.2129085690859));
#78928=CARTESIAN_POINT('Ctrl Pts',(20.3072788812218,-17.5354761826385,-20.2155970151179));
#78929=CARTESIAN_POINT('Ctrl Pts',(20.3123277196757,-17.5411039128815,-20.216048963388));
#78930=CARTESIAN_POINT('Ctrl Pts',(20.3201207742068,-17.5498846834153,-20.2167542318291));
#78931=CARTESIAN_POINT('Ctrl Pts',(20.3228860386396,-17.5530190755787,-20.2170060062323));
#78932=CARTESIAN_POINT('Ctrl Pts',(20.3279918658094,-17.558841131249,-20.2174737549519));
#78933=CARTESIAN_POINT('Ctrl Pts',(20.3303349310455,-17.5615265233791,-20.2176895382437));
#78934=CARTESIAN_POINT('Ctrl Pts',(20.3356101175626,-17.5676033334991,-20.2181779155151));
#78935=CARTESIAN_POINT('Ctrl Pts',(20.3385382365935,-17.5709981370934,-20.2184507976054));
#78936=CARTESIAN_POINT('Ctrl Pts',(20.347130010663,-17.5810234829829,-20.2192567391577));
#78937=CARTESIAN_POINT('Ctrl Pts',(20.3527634259066,-17.5876796540211,-20.2197919354018));
#78938=CARTESIAN_POINT('Ctrl Pts',(20.3925711869254,-17.6353082184688,-20.223621106529));
#78939=CARTESIAN_POINT('Ctrl Pts',(20.4252240993812,-17.6775214247544,-20.2270121780518));
#78940=CARTESIAN_POINT('Ctrl Pts',(20.4665317681763,-17.7353095726767,-20.2316030525249));
#78941=CARTESIAN_POINT('Ctrl Pts',(20.476637704108,-17.7498287429233,-20.2327524135595));
#78942=CARTESIAN_POINT('Ctrl Pts',(20.5137223988464,-17.804558563249,-20.2370653467181));
#78943=CARTESIAN_POINT('Ctrl Pts',(20.5395005206388,-17.8455636931513,-20.240257472366));
#78944=CARTESIAN_POINT('Ctrl Pts',(20.6188548644469,-17.9819610211768,-20.2506814207805));
#78945=CARTESIAN_POINT('Ctrl Pts',(20.6664543604433,-18.0806349266119,-20.257914189928));
#78946=CARTESIAN_POINT('Ctrl Pts',(20.7262435630295,-18.2338839091239,-20.2684877851117));
#78947=CARTESIAN_POINT('Ctrl Pts',(20.7442601962116,-18.2859820580437,-20.2719769904407));
#78948=CARTESIAN_POINT('Ctrl Pts',(20.7701619245909,-18.3715602124066,-20.2775346482309));
#78949=CARTESIAN_POINT('Ctrl Pts',(20.7793002214434,-18.404630882613,-20.2796415418738));
#78950=CARTESIAN_POINT('Ctrl Pts',(20.7902558916234,-18.448395463685,-20.2823780938825));
#78951=CARTESIAN_POINT('Ctrl Pts',(20.7928002840516,-18.4589003974776,-20.2830310946352));
#78952=CARTESIAN_POINT('Ctrl Pts',(20.7968365494926,-18.476140828162,-20.2840965852931));
#78953=CARTESIAN_POINT('Ctrl Pts',(20.7983761272019,-18.4828648504576,-20.2845106046632));
#78954=CARTESIAN_POINT('Ctrl Pts',(20.8012931086656,-18.4958970611322,-20.2853101075458));
#78955=CARTESIAN_POINT('Ctrl Pts',(20.8026745699498,-18.5022042540793,-20.2856957174105));
#78956=CARTESIAN_POINT('Ctrl Pts',(20.8057982531238,-18.5167845639653,-20.2865841184869));
#78957=CARTESIAN_POINT('Ctrl Pts',(20.8075198215551,-18.5250620300429,-20.287086243667));
#78958=CARTESIAN_POINT('Ctrl Pts',(20.812017578788,-18.547356791025,-20.2884328133981));
#78959=CARTESIAN_POINT('Ctrl Pts',(20.8147015409593,-18.5613924006362,-20.2892743167176));
#78960=CARTESIAN_POINT('Ctrl Pts',(20.8380201065115,-18.690402646008,-20.2969546320946));
#78961=CARTESIAN_POINT('Ctrl Pts',(20.8492492306908,-18.8068802661364,-20.3034769044381));
#78962=CARTESIAN_POINT('Ctrl Pts',(20.8529854711163,-19.086379167592,-20.3187794026293));
#78963=CARTESIAN_POINT('Ctrl Pts',(20.8364007118598,-19.2487433283176,-20.3273767148595));
#78964=CARTESIAN_POINT('Ctrl Pts',(20.7943880542967,-19.4393918140765,-20.3385853422936));
#78965=CARTESIAN_POINT('Ctrl Pts',(20.7866465694543,-19.4710293951073,-20.3404848059556));
#78966=CARTESIAN_POINT('Ctrl Pts',(20.776295418608,-19.5094682892352,-20.3428550035646));
#78967=CARTESIAN_POINT('Ctrl Pts',(20.7743760315172,-19.5164529359754,-20.3432882285365));
#78968=CARTESIAN_POINT('Ctrl Pts',(20.7713113379336,-19.5273854437378,-20.3439705081739));
#78969=CARTESIAN_POINT('Ctrl Pts',(20.7701902932699,-19.5313401293462,-20.3442181750627));
#78970=CARTESIAN_POINT('Ctrl Pts',(20.7680736334476,-19.5387249876467,-20.3446823151683));
#78971=CARTESIAN_POINT('Ctrl Pts',(20.7670808527248,-19.5421559141823,-20.3448986226805));
#78972=CARTESIAN_POINT('Ctrl Pts',(20.7647951982406,-19.5499806348931,-20.3453934712168));
#78973=CARTESIAN_POINT('Ctrl Pts',(20.7634967497832,-19.5543727405959,-20.3456723336393));
#78974=CARTESIAN_POINT('Ctrl Pts',(20.7594632334565,-19.5678553468216,-20.3465316703975));
#78975=CARTESIAN_POINT('Ctrl Pts',(20.7566813079152,-19.5769315460023,-20.3471147793858));
#78976=CARTESIAN_POINT('Ctrl Pts',(20.731215296637,-19.6580642910096,-20.3523667852692));
#78977=CARTESIAN_POINT('Ctrl Pts',(20.7047527302255,-19.7288699272416,-20.3572289299204));
#78978=CARTESIAN_POINT('Ctrl Pts',(20.6204510971423,-19.9222190009485,-20.3710221902335));
#78979=CARTESIAN_POINT('Ctrl Pts',(20.5545471961497,-20.0408683284741,-20.3800726728836));
#78980=CARTESIAN_POINT('Ctrl Pts',(20.4267722956368,-20.2264792167476,-20.3946760285343));
#78981=CARTESIAN_POINT('Ctrl Pts',(20.3711100367118,-20.2972321902289,-20.4003745739396));
#78982=CARTESIAN_POINT('Ctrl Pts',(20.2972801652681,-20.3796812855696,-20.4071681931084));
#78983=CARTESIAN_POINT('Ctrl Pts',(20.2832249262702,-20.3949209625224,-20.4084311939097));
#78984=CARTESIAN_POINT('Ctrl Pts',(20.2628205713741,-20.4164028865192,-20.4102226329144));
#78985=CARTESIAN_POINT('Ctrl Pts',(20.2566527608454,-20.4228149874029,-20.4107588101116));
#78986=CARTESIAN_POINT('Ctrl Pts',(20.2459048569644,-20.4338485187958,-20.411684034936));
#78987=CARTESIAN_POINT('Ctrl Pts',(20.2413435782436,-20.4384880314903,-20.4120738945192));
#78988=CARTESIAN_POINT('Ctrl Pts',(20.232542542238,-20.447357856229,-20.4128208272488));
#78989=CARTESIAN_POINT('Ctrl Pts',(20.2283060856346,-20.4515913418839,-20.413178040014));
#78990=CARTESIAN_POINT('Ctrl Pts',(20.2171839624836,-20.4626117323176,-20.4141098208219));
#78991=CARTESIAN_POINT('Ctrl Pts',(20.2102696182567,-20.4693695961458,-20.4146831069051));
#78992=CARTESIAN_POINT('Ctrl Pts',(20.1862282668145,-20.4925469743607,-20.41665618853));
#78993=CARTESIAN_POINT('Ctrl Pts',(20.1688713023723,-20.5087261581908,-20.4180455865978));
#78994=CARTESIAN_POINT('Ctrl Pts',(20.0307849583594,-20.6331703426115,-20.4288393372118));
#78995=CARTESIAN_POINT('Ctrl Pts',(19.8982501185042,-20.7275319192425,-20.4376181142168));
#78996=CARTESIAN_POINT('Ctrl Pts',(19.6420170131075,-20.8688214622892,-20.4535141852791));
#78997=CARTESIAN_POINT('Ctrl Pts',(19.5222459529865,-20.9211007722441,-20.4606069961755));
#78998=CARTESIAN_POINT('Ctrl Pts',(19.3871569990757,-20.9657567789928,-20.4690032984038));
#78999=CARTESIAN_POINT('Ctrl Pts',(19.3758345350771,-20.9693940728918,-20.4697100401756));
#79000=CARTESIAN_POINT('Ctrl Pts',(19.3596901468902,-20.9744307256799,-20.4707228226114));
#79001=CARTESIAN_POINT('Ctrl Pts',(19.354892725446,-20.9759086991256,-20.4710244104664));
#79002=CARTESIAN_POINT('Ctrl Pts',(19.3466142517837,-20.9784268993233,-20.4715459942964));
#79003=CARTESIAN_POINT('Ctrl Pts',(19.3431356587079,-20.9794752646904,-20.4717655155993));
#79004=CARTESIAN_POINT('Ctrl Pts',(19.3363840691346,-20.9814910893136,-20.4721922948394));
#79005=CARTESIAN_POINT('Ctrl Pts',(19.3331114250735,-20.9824595904165,-20.4723994845306));
#79006=CARTESIAN_POINT('Ctrl Pts',(19.3242721818198,-20.9850522316033,-20.4729599300098));
#79007=CARTESIAN_POINT('Ctrl Pts',(19.3187012761245,-20.9866614069513,-20.4733140433683));
#79008=CARTESIAN_POINT('Ctrl Pts',(19.2979807360501,-20.9925544819296,-20.4746342746687));
#79009=CARTESIAN_POINT('Ctrl Pts',(19.2827905008595,-20.996692108103,-20.4756083480782));
#79010=CARTESIAN_POINT('Ctrl Pts',(19.140118424596,-21.0338498396404,-20.4848060651902));
#79011=CARTESIAN_POINT('Ctrl Pts',(19.0098734654943,-21.0550736190206,-20.4935482954804));
#79012=CARTESIAN_POINT('Ctrl Pts',(18.7196143114129,-21.0749342222452,-20.512766475312));
#79013=CARTESIAN_POINT('Ctrl Pts',(18.5599657294328,-21.0678418905443,-20.523135291233));
#79014=CARTESIAN_POINT('Ctrl Pts',(18.3815824983642,-21.0395688654763,-20.534228098973));
#79015=CARTESIAN_POINT('Ctrl Pts',(18.360615121053,-21.0359207392878,-20.5355251355653));
#79016=CARTESIAN_POINT('Ctrl Pts',(18.330871681186,-21.0302823202987,-20.5373559108369));
#79017=CARTESIAN_POINT('Ctrl Pts',(18.3220483193726,-21.0285513865597,-20.5378978604425));
#79018=CARTESIAN_POINT('Ctrl Pts',(18.3068429916011,-21.0254677339177,-20.5388298955764));
#79019=CARTESIAN_POINT('Ctrl Pts',(18.3004558100196,-21.0241416433813,-20.5392208254853));
#79020=CARTESIAN_POINT('Ctrl Pts',(18.2882360762416,-21.0215456394119,-20.5399676584656));
#79021=CARTESIAN_POINT('Ctrl Pts',(18.282402575381,-21.0202805410617,-20.5403237114558));
#79022=CARTESIAN_POINT('Ctrl Pts',(18.2672432337545,-21.0169257752085,-20.5412477862828));
#79023=CARTESIAN_POINT('Ctrl Pts',(18.2579259873522,-21.01479758459,-20.541814568264));
#79024=CARTESIAN_POINT('Ctrl Pts',(18.2261825279712,-21.0073204000864,-20.5437418099668));
#79025=CARTESIAN_POINT('Ctrl Pts',(18.2038289350488,-21.0016680792794,-20.5450925203369));
#79026=CARTESIAN_POINT('Ctrl Pts',(18.013003279222,-20.9500851485518,-20.556578377997));
#79027=CARTESIAN_POINT('Ctrl Pts',(17.850721595277,-20.8838401927936,-20.5659712706361));
#79028=CARTESIAN_POINT('Ctrl Pts',(17.6219933391388,-20.7555536562888,-20.5802385231723));
#79029=CARTESIAN_POINT('Ctrl Pts',(17.5483208739786,-20.7079974898499,-20.5850329556423));
#79030=CARTESIAN_POINT('Ctrl Pts',(17.4472442349054,-20.6334847078711,-20.5922013750864));
#79031=CARTESIAN_POINT('Ctrl Pts',(17.4172900622693,-20.6101332147852,-20.594407074953));
#79032=CARTESIAN_POINT('Ctrl Pts',(17.3821312054603,-20.5811707177156,-20.59711723556));
#79033=CARTESIAN_POINT('Ctrl Pts',(17.3763062266334,-20.5763195741404,-20.5975703609094));
#79034=CARTESIAN_POINT('Ctrl Pts',(17.367306706735,-20.5687423883025,-20.5982770759198));
#79035=CARTESIAN_POINT('Ctrl Pts',(17.3641139141255,-20.5660379856191,-20.5985291096791));
#79036=CARTESIAN_POINT('Ctrl Pts',(17.3582169705406,-20.5610129749576,-20.5989970811449));
#79037=CARTESIAN_POINT('Ctrl Pts',(17.3555106532072,-20.5586949984157,-20.5992128261797));
#79038=CARTESIAN_POINT('Ctrl Pts',(17.3494172470552,-20.5534492325401,-20.5997007904362));
#79039=CARTESIAN_POINT('Ctrl Pts',(17.3460336063529,-20.5505175424153,-20.5999732956908));
#79040=CARTESIAN_POINT('Ctrl Pts',(17.3361072837873,-20.5418617945954,-20.6007772011956));
#79041=CARTESIAN_POINT('Ctrl Pts',(17.3295906231659,-20.5361082249202,-20.6013107229349));
#79042=CARTESIAN_POINT('Ctrl Pts',(17.2837289770084,-20.4951114914313,-20.6051052078611));
#79043=CARTESIAN_POINT('Ctrl Pts',(17.2456829977284,-20.4584496693645,-20.6084613702442));
#79044=CARTESIAN_POINT('Ctrl Pts',(17.1955082977119,-20.406342978521,-20.6131348438562));
#79045=CARTESIAN_POINT('Ctrl Pts',(17.1821608933518,-20.3920922093448,-20.6144037584559));
#79046=CARTESIAN_POINT('Ctrl Pts',(17.0704030636719,-20.2694124175078,-20.6252363405281));
#79047=CARTESIAN_POINT('Ctrl Pts',(16.98328057628,-20.1512151403582,-20.6350415616551));
#79048=CARTESIAN_POINT('Ctrl Pts',(16.8777709685967,-19.9717612418561,-20.6484905953123));
#79049=CARTESIAN_POINT('Ctrl Pts',(16.8488257015203,-19.9172037082465,-20.6524167066091));
#79050=CARTESIAN_POINT('Ctrl Pts',(16.8063135223856,-19.8278420853232,-20.658582707094));
#79051=CARTESIAN_POINT('Ctrl Pts',(16.7912114312221,-19.7938119548773,-20.6608723687523));
#79052=CARTESIAN_POINT('Ctrl Pts',(16.7727688488821,-19.7491105654178,-20.6638069414725));
#79053=CARTESIAN_POINT('Ctrl Pts',(16.7686050596556,-19.7387881655802,-20.6644796308978));
#79054=CARTESIAN_POINT('Ctrl Pts',(16.7619670948561,-19.7219505040658,-20.6655689931111));
#79055=CARTESIAN_POINT('Ctrl Pts',(16.759443381107,-19.7154551187033,-20.6659873301411));
#79056=CARTESIAN_POINT('Ctrl Pts',(16.754652614013,-19.7029422564804,-20.6667896188495));
#79057=CARTESIAN_POINT('Ctrl Pts',(16.7523808194749,-19.6969266888527,-20.6671737261315));
#79058=CARTESIAN_POINT('Ctrl Pts',(16.7485503985575,-19.6866424499954,-20.6678277156676));
#79059=CARTESIAN_POINT('Ctrl Pts',(16.7469780574314,-19.6823789764672,-20.668098052724));
#79060=CARTESIAN_POINT('Ctrl Pts',(16.7454194499653,-19.6781104571783,-20.6683679347509));
#79061=CARTESIAN_POINT('',(16.6170007438877,-18.9502252831514,-19.6896814464532));
#79062=CARTESIAN_POINT('Ctrl Pts',(16.7454193204093,-19.6781101023665,-20.4442392291799));
#79063=CARTESIAN_POINT('Ctrl Pts',(16.7951094568911,-19.8141953118298,-20.4346845874371));
#79064=CARTESIAN_POINT('Ctrl Pts',(16.8586919906538,-19.9449671407128,-20.425294583569));
#79065=CARTESIAN_POINT('Ctrl Pts',(16.946440352571,-20.086359051481,-20.4150699224721));
#79066=CARTESIAN_POINT('Ctrl Pts',(16.9579092613415,-20.1042333489413,-20.4137750701033));
#79067=CARTESIAN_POINT('Ctrl Pts',(16.9742421996514,-20.1288647623245,-20.411986945188));
#79068=CARTESIAN_POINT('Ctrl Pts',(16.9788797524813,-20.1357698697497,-20.4114852443744));
#79069=CARTESIAN_POINT('Ctrl Pts',(16.986955549305,-20.1476425809939,-20.4106218243152));
#79070=CARTESIAN_POINT('Ctrl Pts',(16.990374556875,-20.1526230921707,-20.4102593835781));
#79071=CARTESIAN_POINT('Ctrl Pts',(16.9974994304709,-20.1629073596413,-20.409510444408));
#79072=CARTESIAN_POINT('Ctrl Pts',(17.0012083898193,-20.1682089042307,-20.4091240689944));
#79073=CARTESIAN_POINT('Ctrl Pts',(17.0099528057864,-20.1805868716784,-20.4082212208037));
#79074=CARTESIAN_POINT('Ctrl Pts',(17.0150076436039,-20.1876495098593,-20.4077054979974));
#79075=CARTESIAN_POINT('Ctrl Pts',(17.0315678679638,-20.210489219547,-20.4060356641367));
#79076=CARTESIAN_POINT('Ctrl Pts',(17.0432483126324,-20.226138551847,-20.4048883336052));
#79077=CARTESIAN_POINT('Ctrl Pts',(17.1041456281408,-20.3054157636292,-20.3990558829732));
#79078=CARTESIAN_POINT('Ctrl Pts',(17.1567462495226,-20.366366340377,-20.3945073869285));
#79079=CARTESIAN_POINT('Ctrl Pts',(17.3295172146883,-20.544902630157,-20.3807325311516));
#79080=CARTESIAN_POINT('Ctrl Pts',(17.4602838339007,-20.6512793865957,-20.3718906582591));
#79081=CARTESIAN_POINT('Ctrl Pts',(17.6034503023981,-20.7418459276332,-20.3623779523032));
#79082=CARTESIAN_POINT('Ctrl Pts',(17.6046650335289,-20.7426126317282,-20.362297247125));
#79083=CARTESIAN_POINT('Ctrl Pts',(17.6514513430175,-20.7720762866521,-20.359189085107));
#79084=CARTESIAN_POINT('Ctrl Pts',(17.6980966198759,-20.7990225838782,-20.3560999764049));
#79085=CARTESIAN_POINT('Ctrl Pts',(17.7534420180738,-20.8282386341709,-20.3523862265652));
#79086=CARTESIAN_POINT('Ctrl Pts',(17.7611952543453,-20.8322702702407,-20.3518648943258));
#79087=CARTESIAN_POINT('Ctrl Pts',(17.7729670208209,-20.838299220333,-20.3510713889796));
#79088=CARTESIAN_POINT('Ctrl Pts',(17.7769674151895,-20.8403320064167,-20.350801391176));
#79089=CARTESIAN_POINT('Ctrl Pts',(17.7841568778917,-20.8439565923724,-20.3503154890676));
#79090=CARTESIAN_POINT('Ctrl Pts',(17.7873435278836,-20.8455530696404,-20.3500998822104));
#79091=CARTESIAN_POINT('Ctrl Pts',(17.7942733358218,-20.8490029632364,-20.3496304913794));
#79092=CARTESIAN_POINT('Ctrl Pts',(17.7980179022851,-20.850853327131,-20.3493765272743));
#79093=CARTESIAN_POINT('Ctrl Pts',(17.8085434309242,-20.8560157799964,-20.348661803668));
#79094=CARTESIAN_POINT('Ctrl Pts',(17.8153365839922,-20.859302670231,-20.3481995228626));
#79095=CARTESIAN_POINT('Ctrl Pts',(17.8558881851492,-20.8786568022995,-20.3454346552672));
#79096=CARTESIAN_POINT('Ctrl Pts',(17.8900476785133,-20.8938627334018,-20.343083932858));
#79097=CARTESIAN_POINT('Ctrl Pts',(18.0034024770103,-20.9407662663708,-20.3352546161963));
#79098=CARTESIAN_POINT('Ctrl Pts',(18.0841095782876,-20.9685823989571,-20.3296382171641));
#79099=CARTESIAN_POINT('Ctrl Pts',(18.3376598380881,-21.0391643154831,-20.3122512383248));
#79100=CARTESIAN_POINT('Ctrl Pts',(18.5144189555838,-21.0650899138362,-20.3005605532114));
#79101=CARTESIAN_POINT('Ctrl Pts',(18.7151580919771,-21.0690389382767,-20.2882046024328));
#79102=CARTESIAN_POINT('Ctrl Pts',(18.7379610600611,-21.0691190938378,-20.2868128522382));
#79103=CARTESIAN_POINT('Ctrl Pts',(18.770275709497,-21.0687105625804,-20.2848566432985));
#79104=CARTESIAN_POINT('Ctrl Pts',(18.7797890236273,-21.0685261403483,-20.2842827139751));
#79105=CARTESIAN_POINT('Ctrl Pts',(18.7952600020699,-21.0681218649598,-20.283352488968));
#79106=CARTESIAN_POINT('Ctrl Pts',(18.8012184723263,-21.0679409758598,-20.2829949773939));
#79107=CARTESIAN_POINT('Ctrl Pts',(18.8137017416473,-21.0675092216074,-20.2822475242478));
#79108=CARTESIAN_POINT('Ctrl Pts',(18.8202263128847,-21.0672533320544,-20.2818577441247));
#79109=CARTESIAN_POINT('Ctrl Pts',(18.8357680782531,-21.0665717643682,-20.2809313396686));
#79110=CARTESIAN_POINT('Ctrl Pts',(18.8447839860368,-21.0661185871886,-20.2803955826443));
#79111=CARTESIAN_POINT('Ctrl Pts',(18.875256604488,-21.0643914346441,-20.2785901930243));
#79112=CARTESIAN_POINT('Ctrl Pts',(18.8966971650678,-21.0628483327842,-20.2773289945289));
#79113=CARTESIAN_POINT('Ctrl Pts',(19.0968825238194,-21.0453724124202,-20.2656291356277));
#79114=CARTESIAN_POINT('Ctrl Pts',(19.2729416028154,-21.0071011457111,-20.2559872354047));
#79115=CARTESIAN_POINT('Ctrl Pts',(19.5556343147672,-20.9067700395057,-20.2396620219451));
#79116=CARTESIAN_POINT('Ctrl Pts',(19.6655284762268,-20.8568504082491,-20.2330511826679));
#79117=CARTESIAN_POINT('Ctrl Pts',(19.7788432733866,-20.7932174527959,-20.2253489775442));
#79118=CARTESIAN_POINT('Ctrl Pts',(19.7870915475381,-20.7885122812894,-20.2247829502586));
#79119=CARTESIAN_POINT('Ctrl Pts',(19.7992711765382,-20.7814554662475,-20.2239387152781));
#79120=CARTESIAN_POINT('Ctrl Pts',(19.8032271336972,-20.7791462224482,-20.223663179313));
#79121=CARTESIAN_POINT('Ctrl Pts',(19.810254393918,-20.7750135044969,-20.22317130045));
#79122=CARTESIAN_POINT('Ctrl Pts',(19.8133286074333,-20.7731950787742,-20.2229552864762));
#79123=CARTESIAN_POINT('Ctrl Pts',(19.8199306225379,-20.7692673378157,-20.222489578866));
#79124=CARTESIAN_POINT('Ctrl Pts',(19.8234568357825,-20.7671555570695,-20.2222397295855));
#79125=CARTESIAN_POINT('Ctrl Pts',(19.8331790941365,-20.7612945495431,-20.2215478399339));
#79126=CARTESIAN_POINT('Ctrl Pts',(19.8393620165736,-20.7575238178486,-20.2211044277628));
#79127=CARTESIAN_POINT('Ctrl Pts',(19.8732234723351,-20.7366338706383,-20.2186578162648));
#79128=CARTESIAN_POINT('Ctrl Pts',(19.9005221458512,-20.7189108596778,-20.2166182569852));
#79129=CARTESIAN_POINT('Ctrl Pts',(20.0617807904764,-20.6088515790043,-20.2042120968778));
#79130=CARTESIAN_POINT('Ctrl Pts',(20.185137890794,-20.5019541075133,-20.1932557254062));
#79131=CARTESIAN_POINT('Ctrl Pts',(20.3739364858185,-20.2958532227758,-20.1749987219105));
#79132=CARTESIAN_POINT('Ctrl Pts',(20.4455836971107,-20.2033281804784,-20.1675581068973));
#79133=CARTESIAN_POINT('Ctrl Pts',(20.5170242806521,-20.0933665485799,-20.1595512610459));
#79134=CARTESIAN_POINT('Ctrl Pts',(20.5246877590987,-20.0813053390216,-20.1586832888641));
#79135=CARTESIAN_POINT('Ctrl Pts',(20.5366902189829,-20.0619857894196,-20.1573089857889));
#79136=CARTESIAN_POINT('Ctrl Pts',(20.5411087459664,-20.0547776121328,-20.1567997268503));
#79137=CARTESIAN_POINT('Ctrl Pts',(20.548825354215,-20.0420181754053,-20.1559043513171));
#79138=CARTESIAN_POINT('Ctrl Pts',(20.5521414195464,-20.0364779707204,-20.1555175785997));
#79139=CARTESIAN_POINT('Ctrl Pts',(20.5589476838088,-20.024987667407,-20.1547195114838));
#79140=CARTESIAN_POINT('Ctrl Pts',(20.5624342550248,-20.0190355007357,-20.1543083524671));
#79141=CARTESIAN_POINT('Ctrl Pts',(20.5713091281875,-20.003713361264,-20.1532556439074));
#79142=CARTESIAN_POINT('Ctrl Pts',(20.5766549181833,-19.9943188983395,-20.1526156356688));
#79143=CARTESIAN_POINT('Ctrl Pts',(20.5986660915895,-19.9549387880268,-20.1499549682845));
#79144=CARTESIAN_POINT('Ctrl Pts',(20.6146738833644,-19.9245902460364,-20.1479578380001));
#79145=CARTESIAN_POINT('Ctrl Pts',(20.6544542961342,-19.8445137945479,-20.1428137515898));
#79146=CARTESIAN_POINT('Ctrl Pts',(20.677035763032,-19.7942222070087,-20.1397061847616));
#79147=CARTESIAN_POINT('Ctrl Pts',(20.738492048994,-19.641679115766,-20.1305617623255));
#79148=CARTESIAN_POINT('Ctrl Pts',(20.7714353569377,-19.5372381627218,-20.1246736362835));
#79149=CARTESIAN_POINT('Ctrl Pts',(20.8065062231099,-19.3861648461232,-20.1162298524835));
#79150=CARTESIAN_POINT('Ctrl Pts',(20.8154024978397,-19.3412872499354,-20.1137288737193));
#79151=CARTESIAN_POINT('Ctrl Pts',(20.8265388435982,-19.2736961695852,-20.1099303523099));
#79152=CARTESIAN_POINT('Ctrl Pts',(20.8298770511543,-19.2511764901954,-20.1086595135307));
#79153=CARTESIAN_POINT('Ctrl Pts',(20.8329763866112,-19.2276592897455,-20.1073230258424));
#79154=CARTESIAN_POINT('Ctrl Pts',(20.8331007664771,-19.2267105526645,-20.1072690930572));
#79155=CARTESIAN_POINT('Ctrl Pts',(20.835414482207,-19.2089688153357,-20.1062602282928));
#79156=CARTESIAN_POINT('Ctrl Pts',(20.8374028260142,-19.192150623561,-20.105298830823));
#79157=CARTESIAN_POINT('Ctrl Pts',(20.8428628448425,-19.1406780920217,-20.1023362274941));
#79158=CARTESIAN_POINT('Ctrl Pts',(20.8456811406815,-19.1059622224045,-20.1003101554433));
#79159=CARTESIAN_POINT('Ctrl Pts',(20.8480368528763,-19.0641892209831,-20.0978219876125));
#79160=CARTESIAN_POINT('Ctrl Pts',(20.8483970894526,-19.0571816601472,-20.0974028934515));
#79161=CARTESIAN_POINT('Ctrl Pts',(20.8489299572372,-19.0457032225027,-20.0967134499008));
#79162=CARTESIAN_POINT('Ctrl Pts',(20.8491232672893,-19.0412332967747,-20.0964442314703));
#79163=CARTESIAN_POINT('Ctrl Pts',(20.8494450792549,-19.0332023054611,-20.0959591591568));
#79164=CARTESIAN_POINT('Ctrl Pts',(20.8495787611597,-19.0296415016763,-20.0957435982898));
#79165=CARTESIAN_POINT('Ctrl Pts',(20.8498499661962,-19.0218959990634,-20.0952736348228));
#79166=CARTESIAN_POINT('Ctrl Pts',(20.8499840635673,-19.0177112788362,-20.0950190484162));
#79167=CARTESIAN_POINT('Ctrl Pts',(20.8503264209045,-19.00593639317,-20.094300849607));
#79168=CARTESIAN_POINT('Ctrl Pts',(20.8505062579293,-18.9983455549318,-20.0938356925313));
#79169=CARTESIAN_POINT('Ctrl Pts',(20.8513445290428,-18.9525613666721,-20.0910177338244));
#79170=CARTESIAN_POINT('Ctrl Pts',(20.8510099044863,-18.9143594262355,-20.0886146656814));
#79171=CARTESIAN_POINT('Ctrl Pts',(20.8464731240225,-18.7877501482996,-20.0805234784596));
#79172=CARTESIAN_POINT('Ctrl Pts',(20.8377617606703,-18.6996010815258,-20.0746880681203));
#79173=CARTESIAN_POINT('Ctrl Pts',(20.7957454093421,-18.4411791377453,-20.0573881260028));
#79174=CARTESIAN_POINT('Ctrl Pts',(20.7470176745464,-18.2741249616737,-20.0460171671181));
#79175=CARTESIAN_POINT('Ctrl Pts',(20.6693002344558,-18.0936075860013,-20.0339182115918));
#79176=CARTESIAN_POINT('Ctrl Pts',(20.6598010428807,-18.0725030165807,-20.0325053599962));
#79177=CARTESIAN_POINT('Ctrl Pts',(20.6458865243582,-18.0428957593003,-20.0305249464703));
#79178=CARTESIAN_POINT('Ctrl Pts',(20.6417568959298,-18.0342613480849,-20.0299475930393));
#79179=CARTESIAN_POINT('Ctrl Pts',(20.6349559097492,-18.0202858347727,-20.0290133369963));
#79180=CARTESIAN_POINT('Ctrl Pts',(20.6323202933435,-18.0149275793667,-20.0286551974926));
#79181=CARTESIAN_POINT('Ctrl Pts',(20.6267592450396,-18.0037416180122,-20.0279076308146));
#79182=CARTESIAN_POINT('Ctrl Pts',(20.623829484195,-17.9979161248468,-20.0275183598308));
#79183=CARTESIAN_POINT('Ctrl Pts',(20.6168018773392,-17.9841019165005,-20.0265953404202));
#79184=CARTESIAN_POINT('Ctrl Pts',(20.6126800130813,-17.976125509307,-20.0260624423581));
#79185=CARTESIAN_POINT('Ctrl Pts',(20.5986527563105,-17.9493989976437,-20.0242768600043));
#79186=CARTESIAN_POINT('Ctrl Pts',(20.5885162192826,-17.9307711754583,-20.0230323561497));
#79187=CARTESIAN_POINT('Ctrl Pts',(20.5320177019306,-17.8305607171013,-20.016332306278));
#79188=CARTESIAN_POINT('Ctrl Pts',(20.4805481446169,-17.7519723921545,-20.0110657388705));
#79189=CARTESIAN_POINT('Ctrl Pts',(20.3279480334004,-17.549690934078,-19.9971172333309));
#79190=CARTESIAN_POINT('Ctrl Pts',(20.2177889895693,-17.4336115924511,-19.9886941392892));
#79191=CARTESIAN_POINT('Ctrl Pts',(20.0890806216629,-17.3254948106074,-19.9791997111178));
#79192=CARTESIAN_POINT('Ctrl Pts',(20.0824772395814,-17.3200160070786,-19.9787133535409));
#79193=CARTESIAN_POINT('Ctrl Pts',(20.0445540837438,-17.2889386032625,-19.9759233255696));
#79194=CARTESIAN_POINT('Ctrl Pts',(20.0125411923671,-17.2642034608607,-19.9735802302566));
#79195=CARTESIAN_POINT('Ctrl Pts',(19.9738960313434,-17.23607432669,-19.9707399083838));
#79196=CARTESIAN_POINT('Ctrl Pts',(19.9679277020679,-17.2317774831808,-19.9703009269887));
#79197=CARTESIAN_POINT('Ctrl Pts',(19.9582089751464,-17.2248571766077,-19.9695853584113));
#79198=CARTESIAN_POINT('Ctrl Pts',(19.9544721870562,-17.2222145835555,-19.9693100511876));
#79199=CARTESIAN_POINT('Ctrl Pts',(19.9478042275556,-17.2175314783284,-19.968818421559));
#79200=CARTESIAN_POINT('Ctrl Pts',(19.9448764332441,-17.2154862457548,-19.9686024267764));
#79201=CARTESIAN_POINT('Ctrl Pts',(19.938565837533,-17.2111016518852,-19.9681365787778));
#79202=CARTESIAN_POINT('Ctrl Pts',(19.9351814397367,-17.2087647710112,-19.9678865689566));
#79203=CARTESIAN_POINT('Ctrl Pts',(19.9258091288351,-17.2023335691307,-19.9671937942238));
#79204=CARTESIAN_POINT('Ctrl Pts',(19.9198070145729,-17.1982601847573,-19.9667496518529));
#79205=CARTESIAN_POINT('Ctrl Pts',(19.886617890084,-17.17598438511,-19.9642916133847));
#79206=CARTESIAN_POINT('Ctrl Pts',(19.859034239654,-17.1583843357344,-19.962240964186));
#79207=CARTESIAN_POINT('Ctrl Pts',(19.6920336853364,-17.0571957160218,-19.9498310162141));
#79208=CARTESIAN_POINT('Ctrl Pts',(19.5437766951488,-16.9892535887587,-19.9388847359663));
#79209=CARTESIAN_POINT('Ctrl Pts',(19.2781805894784,-16.9028076619477,-19.9206407205647));
#79210=CARTESIAN_POINT('Ctrl Pts',(19.1643411956418,-16.8759132956713,-19.913203361494));
#79211=CARTESIAN_POINT('Ctrl Pts',(19.034717565091,-16.8564184311949,-19.9051995451461));
#79212=CARTESIAN_POINT('Ctrl Pts',(19.0205664076742,-16.8544364431137,-19.9043316120189));
#79213=CARTESIAN_POINT('Ctrl Pts',(18.9980119584396,-16.8515100187934,-19.9029573584115));
#79214=CARTESIAN_POINT('Ctrl Pts',(18.9896213922512,-16.8504724169283,-19.9024481102261));
#79215=CARTESIAN_POINT('Ctrl Pts',(18.9748122342812,-16.8487310783971,-19.9015527466365));
#79216=CARTESIAN_POINT('Ctrl Pts',(18.9683962590684,-16.8480063964148,-19.9011659751714));
#79217=CARTESIAN_POINT('Ctrl Pts',(18.9551189912645,-16.8465682210066,-19.9003679039678));
#79218=CARTESIAN_POINT('Ctrl Pts',(18.948257318076,-16.8458588870458,-19.8999567396444));
#79219=CARTESIAN_POINT('Ctrl Pts',(18.9306352119817,-16.8441241904971,-19.8989040036792));
#79220=CARTESIAN_POINT('Ctrl Pts',(18.9198700873584,-16.8431476694507,-19.898263973491));
#79221=CARTESIAN_POINT('Ctrl Pts',(18.8749070161365,-16.8394159720983,-19.8956030992208));
#79222=CARTESIAN_POINT('Ctrl Pts',(18.840650991737,-16.8374097737959,-19.8936057886063));
#79223=CARTESIAN_POINT('Ctrl Pts',(18.7512799517122,-16.8343532529321,-19.8884611346919));
#79224=CARTESIAN_POINT('Ctrl Pts',(18.6961450163041,-16.834620962625,-19.8853531919853));
#79225=CARTESIAN_POINT('Ctrl Pts',(18.4578825206337,-16.8450889183847,-19.8720922416621));
#79226=CARTESIAN_POINT('Ctrl Pts',(18.2765290384972,-16.8769038756254,-19.8625001067257));
#79227=CARTESIAN_POINT('Ctrl Pts',(18.0574431867915,-16.9454864106654,-19.8495086414657));
#79228=CARTESIAN_POINT('Ctrl Pts',(18.0137951913747,-16.9607365193418,-19.8468424005504));
#79229=CARTESIAN_POINT('Ctrl Pts',(17.9635506949731,-16.9801593949427,-19.8436435510397));
#79230=CARTESIAN_POINT('Ctrl Pts',(17.9564315646845,-16.9829558593639,-19.8431872202555));
#79231=CARTESIAN_POINT('Ctrl Pts',(17.9450411793493,-16.9875015190664,-19.8424519074684));
#79232=CARTESIAN_POINT('Ctrl Pts',(17.9407601441824,-16.9892262401154,-19.8421743598098));
#79233=CARTESIAN_POINT('Ctrl Pts',(17.9331647342377,-16.9923151469594,-19.8416797724876));
#79234=CARTESIAN_POINT('Ctrl Pts',(17.9298481455986,-16.9936737654281,-19.841463070751));
#79235=CARTESIAN_POINT('Ctrl Pts',(17.9227996537634,-16.9965820584099,-19.8410009421983));
#79236=CARTESIAN_POINT('Ctrl Pts',(17.919068790636,-16.9981339730167,-19.840755385955));
#79237=CARTESIAN_POINT('Ctrl Pts',(17.9090820094276,-17.00232172058,-19.8400955893012));
#79238=CARTESIAN_POINT('Ctrl Pts',(17.9028343500244,-17.0049769534421,-19.8396801983692));
#79239=CARTESIAN_POINT('Ctrl Pts',(17.8719118144841,-17.0182948762989,-19.8376115761724));
#79240=CARTESIAN_POINT('Ctrl Pts',(17.8474300203297,-17.0293962812278,-19.8359337265203));
#79241=CARTESIAN_POINT('Ctrl Pts',(17.777230875773,-17.062854325332,-19.8310195190076));
#79242=CARTESIAN_POINT('Ctrl Pts',(17.7321014556109,-17.0863963038991,-19.8277316425662));
#79243=CARTESIAN_POINT('Ctrl Pts',(17.6012698609584,-17.1607620478373,-19.8178997079442));
#79244=CARTESIAN_POINT('Ctrl Pts',(17.5182551517247,-17.2160347110697,-19.8112703400073));
#79245=CARTESIAN_POINT('Ctrl Pts',(17.4275637978787,-17.2861252294552,-19.8037403397405));
#79246=CARTESIAN_POINT('Ctrl Pts',(17.4157851062505,-17.2954301089221,-19.802756214046));
#79247=CARTESIAN_POINT('Ctrl Pts',(17.3105976467623,-17.3803579882302,-19.7939148841377));
#79248=CARTESIAN_POINT('Ctrl Pts',(17.2236759054821,-17.4636914070113,-19.7862491314523));
#79249=CARTESIAN_POINT('Ctrl Pts',(17.133907704203,-17.5657674731961,-19.7779486627357));
#79250=CARTESIAN_POINT('Ctrl Pts',(17.1236610246714,-17.5776840323712,-19.7769945202234));
#79251=CARTESIAN_POINT('Ctrl Pts',(17.1083597659514,-17.5958850239516,-19.7755591886708));
#79252=CARTESIAN_POINT('Ctrl Pts',(17.103207002873,-17.6020858537861,-19.7750739796163));
#79253=CARTESIAN_POINT('Ctrl Pts',(17.0940373121159,-17.6132497819579,-19.7742071116631));
#79254=CARTESIAN_POINT('Ctrl Pts',(17.0900071984328,-17.6182018766924,-19.7738249196995));
#79255=CARTESIAN_POINT('Ctrl Pts',(17.0815036577164,-17.6287478924441,-19.7730158948805));
#79256=CARTESIAN_POINT('Ctrl Pts',(17.0770360844197,-17.6343464469702,-19.7725893005581));
#79257=CARTESIAN_POINT('Ctrl Pts',(17.0651573365794,-17.6493882919641,-19.7714507848237));
#79258=CARTESIAN_POINT('Ctrl Pts',(17.0577978546972,-17.6588722127342,-19.770740926658));
#79259=CARTESIAN_POINT('Ctrl Pts',(17.0223745414901,-17.7053316367734,-19.7673013352193));
#79260=CARTESIAN_POINT('Ctrl Pts',(16.9954500887626,-17.7431623789647,-19.7646164247055));
#79261=CARTESIAN_POINT('Ctrl Pts',(16.919785290694,-17.8572405882314,-19.7568180538405));
#79262=CARTESIAN_POINT('Ctrl Pts',(16.8746620068182,-17.9357631156808,-19.75182947175));
#79263=CARTESIAN_POINT('Ctrl Pts',(16.8015554844187,-18.0842571027667,-19.7428030122621));
#79264=CARTESIAN_POINT('Ctrl Pts',(16.772015276171,-18.1532914773746,-19.7387531925283));
#79265=CARTESIAN_POINT('Ctrl Pts',(16.710891428836,-18.3201317462362,-19.7290386440713));
#79266=CARTESIAN_POINT('Ctrl Pts',(16.6826415341211,-18.4189441223155,-19.7233418111299));
#79267=CARTESIAN_POINT('Ctrl Pts',(16.6596911929394,-18.5288855123653,-19.7166879680927));
#79268=CARTESIAN_POINT('Ctrl Pts',(16.6577762683325,-18.5383843514854,-19.7161105270604));
#79269=CARTESIAN_POINT('Ctrl Pts',(16.6550450479744,-18.5524294323368,-19.7152525031138));
#79270=CARTESIAN_POINT('Ctrl Pts',(16.6541782809238,-18.5569658913124,-19.7149747201565));
#79271=CARTESIAN_POINT('Ctrl Pts',(16.6526668272638,-18.5650193685107,-19.7144803720146));
#79272=CARTESIAN_POINT('Ctrl Pts',(16.6520161987248,-18.5685352218286,-19.7142641484818));
#79273=CARTESIAN_POINT('Ctrl Pts',(16.650641182941,-18.5760721707847,-19.7137997354823));
#79274=CARTESIAN_POINT('Ctrl Pts',(16.6499195393132,-18.580093659469,-19.7135513995312));
#79275=CARTESIAN_POINT('Ctrl Pts',(16.6484624965497,-18.5883507147415,-19.7130404375919));
#79276=CARTESIAN_POINT('Ctrl Pts',(16.647728348886,-18.5925864805177,-19.7127777434399));
#79277=CARTESIAN_POINT('Ctrl Pts',(16.6459030758296,-18.603311687976,-19.7121111777086));
#79278=CARTESIAN_POINT('Ctrl Pts',(16.6448293063746,-18.6098039830409,-19.7117063815082));
#79279=CARTESIAN_POINT('Ctrl Pts',(16.6260483532597,-18.7267427401032,-19.7043930655705));
#79280=CARTESIAN_POINT('Ctrl Pts',(16.6170944882044,-18.8384008820488,-19.6970632328612));
#79281=CARTESIAN_POINT('Ctrl Pts',(16.6170007438877,-18.9502252831514,-19.6896814464532));
#79282=CARTESIAN_POINT('Ctrl Pts',(16.6170007453285,-18.9502235652229,-19.6896815598576));
#79283=CARTESIAN_POINT('Ctrl Pts',(16.6169157215329,-19.0515474721257,-19.6829929357409));
#79284=CARTESIAN_POINT('Ctrl Pts',(16.624105218519,-19.1527558515676,-19.676279183763));
#79285=CARTESIAN_POINT('Ctrl Pts',(16.6510570136956,-19.34034580853,-19.6640088596727));
#79286=CARTESIAN_POINT('Ctrl Pts',(16.6690385649789,-19.4267648125115,-19.6584257671682));
#79287=CARTESIAN_POINT('Ctrl Pts',(16.6977854267898,-19.5316033194997,-19.6517542931015));
#79288=CARTESIAN_POINT('Ctrl Pts',(16.7034973725127,-19.5513070351543,-19.6505046733498));
#79289=CARTESIAN_POINT('Ctrl Pts',(16.7120850741006,-19.5793974178702,-19.6487287240108));
#79290=CARTESIAN_POINT('Ctrl Pts',(16.7147283676524,-19.587853415537,-19.6481948376127));
#79291=CARTESIAN_POINT('Ctrl Pts',(16.7194027738261,-19.6024838660219,-19.647272300583));
#79292=CARTESIAN_POINT('Ctrl Pts',(16.7214093686994,-19.6086659698244,-19.6468828508525));
#79293=CARTESIAN_POINT('Ctrl Pts',(16.7253223050648,-19.6205348830199,-19.6461358268466));
#79294=CARTESIAN_POINT('Ctrl Pts',(16.7272244027105,-19.6262230159287,-19.6457781171379));
#79295=CARTESIAN_POINT('Ctrl Pts',(16.7322706374349,-19.641102991212,-19.6448431009333));
#79296=CARTESIAN_POINT('Ctrl Pts',(16.7354539394052,-19.6502814775665,-19.6442670940895));
#79297=CARTESIAN_POINT('Ctrl Pts',(16.7409108787423,-19.6656725528941,-19.6433023316371));
#79298=CARTESIAN_POINT('Ctrl Pts',(16.743150603721,-19.671896824708,-19.6429124843661));
#79299=CARTESIAN_POINT('Ctrl Pts',(16.7454194498907,-19.678110456974,-19.6425235871583));
#79300=CARTESIAN_POINT('Origin',(18.734,-18.952,0.));
#79301=CARTESIAN_POINT('',(16.7454194032426,-19.6781103292199,-18.8452753983371));
#79302=CARTESIAN_POINT('',(16.7454194499637,-19.6781104571739,-19.0663245191576));
#79303=CARTESIAN_POINT('',(16.7454194499637,-19.6781104571739,0.));
#79304=CARTESIAN_POINT('',(16.6180378855072,-18.9538841874204,-19.1109437209775));
#79305=CARTESIAN_POINT('Ctrl Pts',(16.7454194499637,-19.6781104571739,-19.0663245191576));
#79306=CARTESIAN_POINT('Ctrl Pts',(16.7290739263666,-19.6333453804777,-19.0692018282141));
#79307=CARTESIAN_POINT('Ctrl Pts',(16.7142587319683,-19.5880774621226,-19.0720791372705));
#79308=CARTESIAN_POINT('Ctrl Pts',(16.7009992479656,-19.5424209872857,-19.074956446327));
#79309=CARTESIAN_POINT('Ctrl Pts',(16.6758066766558,-19.4556752287146,-19.0804232362541));
#79310=CARTESIAN_POINT('Ctrl Pts',(16.6561521069708,-19.367253508475,-19.0858900261813));
#79311=CARTESIAN_POINT('Ctrl Pts',(16.6422180861824,-19.2777873923673,-19.0913568161084));
#79312=CARTESIAN_POINT('Ctrl Pts',(16.6285119268914,-19.1897843057392,-19.0967342082258));
#79313=CARTESIAN_POINT('Ctrl Pts',(16.6203407792448,-19.1007706087263,-19.1021116003432));
#79314=CARTESIAN_POINT('Ctrl Pts',(16.6178326248366,-19.0113686810859,-19.1074889924606));
#79315=CARTESIAN_POINT('Ctrl Pts',(16.6172955000017,-18.9922231310909,-19.1086405686329));
#79316=CARTESIAN_POINT('Ctrl Pts',(16.6170179137274,-18.9730598582114,-19.1097921448052));
#79317=CARTESIAN_POINT('Ctrl Pts',(16.6170008393112,-18.9538851108724,-19.1109437209775));
#79318=CARTESIAN_POINT('Ctrl Pts',(16.6180378855072,-18.9538841874204,-19.1109437209775));
#79319=CARTESIAN_POINT('Ctrl Pts',(16.622366738429,-18.4480050085671,-19.1413398983212));
#79320=CARTESIAN_POINT('Ctrl Pts',(17.0578064022828,-17.2299118723797,-19.2141280112252));
#79321=CARTESIAN_POINT('Ctrl Pts',(19.0938031787897,-16.4747288712945,-19.3293080596899));
#79322=CARTESIAN_POINT('Ctrl Pts',(21.0117476238401,-17.913637640173,-19.4564838663712));
#79323=CARTESIAN_POINT('Ctrl Pts',(20.8399999988754,-20.3051794704029,-19.5836596730529));
#79324=CARTESIAN_POINT('Ctrl Pts',(18.7361280843893,-21.4552630390637,-19.7108354797341));
#79325=CARTESIAN_POINT('Ctrl Pts',(17.1750895211376,-20.6053639705819,-19.8051103626019));
#79326=CARTESIAN_POINT('Ctrl Pts',(16.7978195176575,-19.8268833696163,-19.856993309909));
#79327=CARTESIAN_POINT('Ctrl Pts',(16.7452305273115,-19.6781794125984,-19.8664843216556));
#79328=CARTESIAN_POINT('Ctrl Pts',(16.7454194498907,-19.678110456974,-19.6425235871583));
#79329=CARTESIAN_POINT('Ctrl Pts',(16.7513832064613,-19.6944432479537,-19.6415013546644));
#79330=CARTESIAN_POINT('Ctrl Pts',(16.7575481680138,-19.7107025283047,-19.6404856934997));
#79331=CARTESIAN_POINT('Ctrl Pts',(16.8191736666767,-19.8673808173857,-19.6307122755094));
#79332=CARTESIAN_POINT('Ctrl Pts',(16.8893050312533,-20.0015661897086,-19.6224919227194));
#79333=CARTESIAN_POINT('Ctrl Pts',(17.0102352499799,-20.1827695245077,-19.6106616261116));
#79334=CARTESIAN_POINT('Ctrl Pts',(17.0499589213118,-20.2365869578084,-19.6070351305032));
#79335=CARTESIAN_POINT('Ctrl Pts',(17.1263126030287,-20.3303892442845,-19.6003481701723));
#79336=CARTESIAN_POINT('Ctrl Pts',(17.1620578397331,-20.3710182217699,-19.5973138498835));
#79337=CARTESIAN_POINT('Ctrl Pts',(17.2185936143475,-20.4305180581435,-19.5925772640953));
#79338=CARTESIAN_POINT('Ctrl Pts',(17.2382695806024,-20.4504200023401,-19.5909393363386));
#79339=CARTESIAN_POINT('Ctrl Pts',(17.2632160887945,-20.474672014578,-19.5888664616147));
#79340=CARTESIAN_POINT('Ctrl Pts',(17.2681218468328,-20.4793953694554,-19.5884590057323));
#79341=CARTESIAN_POINT('Ctrl Pts',(17.2760082684952,-20.4869155732619,-19.587804099952));
#79342=CARTESIAN_POINT('Ctrl Pts',(17.2789744377563,-20.4897276477795,-19.5875578083018));
#79343=CARTESIAN_POINT('Ctrl Pts',(17.2845504956219,-20.4949834469785,-19.5870948134674));
#79344=CARTESIAN_POINT('Ctrl Pts',(17.2871584375725,-20.4974291559132,-19.586878267291));
#79345=CARTESIAN_POINT('Ctrl Pts',(17.2931476521016,-20.5030173499238,-19.5863809687617));
#79346=CARTESIAN_POINT('Ctrl Pts',(17.2965330058392,-20.5061553808984,-19.5860998827092));
#79347=CARTESIAN_POINT('Ctrl Pts',(17.3054342628809,-20.5143523781155,-19.5853608968982));
#79348=CARTESIAN_POINT('Ctrl Pts',(17.3109667232938,-20.5193931568867,-19.5849016758516));
#79349=CARTESIAN_POINT('Ctrl Pts',(17.3483958362069,-20.5531343530628,-19.5817961650597));
#79350=CARTESIAN_POINT('Ctrl Pts',(17.3811296666267,-20.5808865522599,-19.5790866178343));
#79351=CARTESIAN_POINT('Ctrl Pts',(17.4212483212683,-20.6128559665986,-19.5757959124704));
#79352=CARTESIAN_POINT('Ctrl Pts',(17.4278463901912,-20.6180498960387,-19.5752556461949));
#79353=CARTESIAN_POINT('Ctrl Pts',(17.4457534187519,-20.6319743625904,-19.5737922505113));
#79354=CARTESIAN_POINT('Ctrl Pts',(17.4571200312392,-20.6406298127629,-19.572866419495));
#79355=CARTESIAN_POINT('Ctrl Pts',(17.5768592650271,-20.7299086070912,-19.5631519091738));
#79356=CARTESIAN_POINT('Ctrl Pts',(17.6926242410796,-20.8000996500337,-19.5541120302114));
#79357=CARTESIAN_POINT('Ctrl Pts',(17.9141593465285,-20.9069537602988,-19.5380905046534));
#79358=CARTESIAN_POINT('Ctrl Pts',(18.0176687647134,-20.9472090654657,-19.5310500916392));
#79359=CARTESIAN_POINT('Ctrl Pts',(18.1382376049595,-20.9834972954317,-19.5233698644076));
#79360=CARTESIAN_POINT('Ctrl Pts',(18.1526499363599,-20.9876684932426,-19.5224597225658));
#79361=CARTESIAN_POINT('Ctrl Pts',(18.1746298980515,-20.9937774305612,-19.5210834355425));
#79362=CARTESIAN_POINT('Ctrl Pts',(18.182165697115,-20.9958270209614,-19.5206136642382));
#79363=CARTESIAN_POINT('Ctrl Pts',(18.1958625178662,-20.9994710124786,-19.5197635505702));
#79364=CARTESIAN_POINT('Ctrl Pts',(18.2020196882585,-21.0010794142507,-19.5193827581294));
#79365=CARTESIAN_POINT('Ctrl Pts',(18.2152898241597,-21.0044820498446,-19.5185649500938));
#79366=CARTESIAN_POINT('Ctrl Pts',(18.2224050678729,-21.0062671294049,-19.5181282347316));
#79367=CARTESIAN_POINT('Ctrl Pts',(18.2416306582839,-21.0109843819199,-19.5169529332033));
#79368=CARTESIAN_POINT('Ctrl Pts',(18.2537579676296,-21.0138467096242,-19.5162166014125));
#79369=CARTESIAN_POINT('Ctrl Pts',(18.3117601982119,-21.0269970716835,-19.5127180538857));
#79370=CARTESIAN_POINT('Ctrl Pts',(18.357946135052,-21.0358625850952,-19.5100015925458));
#79371=CARTESIAN_POINT('Ctrl Pts',(18.4449512248838,-21.0495761606526,-19.5049896018816));
#79372=CARTESIAN_POINT('Ctrl Pts',(18.4856895137337,-21.0547879351184,-19.5026853727095));
#79373=CARTESIAN_POINT('Ctrl Pts',(18.6850377352986,-21.0744165262435,-19.4915595754524));
#79374=CARTESIAN_POINT('Ctrl Pts',(18.8447634385835,-21.0720887461264,-19.4831458930242));
#79375=CARTESIAN_POINT('Ctrl Pts',(19.0484598722091,-21.0460227443856,-19.4717142623738));
#79376=CARTESIAN_POINT('Ctrl Pts',(19.0940027330479,-21.038675287285,-19.4691089522826));
#79377=CARTESIAN_POINT('Ctrl Pts',(19.1557108640872,-21.0266396459103,-19.4654681083536));
#79378=CARTESIAN_POINT('Ctrl Pts',(19.1721163181589,-21.0232372556315,-19.4644893620884));
#79379=CARTESIAN_POINT('Ctrl Pts',(19.2001422140399,-21.0170770048535,-19.4627961245304));
#79380=CARTESIAN_POINT('Ctrl Pts',(19.2117830979068,-21.0144148215717,-19.4620865079337));
#79381=CARTESIAN_POINT('Ctrl Pts',(19.2282926041553,-21.0104919492343,-19.4610703168165));
#79382=CARTESIAN_POINT('Ctrl Pts',(19.2331804614697,-21.0093121176148,-19.4607682361835));
#79383=CARTESIAN_POINT('Ctrl Pts',(19.2415939745128,-21.0072495144299,-19.4602460790663));
#79384=CARTESIAN_POINT('Ctrl Pts',(19.2451216828042,-21.0063750472448,-19.4600264801571));
#79385=CARTESIAN_POINT('Ctrl Pts',(19.2519551409747,-21.0046624423578,-19.459599785814));
#79386=CARTESIAN_POINT('Ctrl Pts',(19.2552611250853,-21.0038253993509,-19.4593927596644));
#79387=CARTESIAN_POINT('Ctrl Pts',(19.264170918735,-21.0015466031443,-19.4588332379587));
#79388=CARTESIAN_POINT('Ctrl Pts',(19.269770815251,-21.0000898694273,-19.4584798895516));
#79389=CARTESIAN_POINT('Ctrl Pts',(19.2905078471284,-20.9946045577946,-19.4571653371271));
#79390=CARTESIAN_POINT('Ctrl Pts',(19.3056056722854,-20.9904310843758,-19.4561962625258));
#79391=CARTESIAN_POINT('Ctrl Pts',(19.449767543781,-20.9488531318853,-19.4468369344059));
#79392=CARTESIAN_POINT('Ctrl Pts',(19.5750295841489,-20.8994107506389,-19.4379069223211));
#79393=CARTESIAN_POINT('Ctrl Pts',(19.837816238959,-20.7655754525965,-19.4184305523235));
#79394=CARTESIAN_POINT('Ctrl Pts',(19.9721561617023,-20.6766606795245,-19.4079968559008));
#79395=CARTESIAN_POINT('Ctrl Pts',(20.1094539179999,-20.5613984819543,-19.3970168073795));
#79396=CARTESIAN_POINT('Ctrl Pts',(20.1235816983893,-20.5492162322996,-19.3958819751655));
#79397=CARTESIAN_POINT('Ctrl Pts',(20.1439297388161,-20.5311959419061,-19.3942396949984));
#79398=CARTESIAN_POINT('Ctrl Pts',(20.1502783601182,-20.5255047827425,-19.3937261681634));
#79399=CARTESIAN_POINT('Ctrl Pts',(20.1613653292252,-20.5154445154962,-19.3928272999184));
#79400=CARTESIAN_POINT('Ctrl Pts',(20.1661183969493,-20.5110918621599,-19.392441272119));
#79401=CARTESIAN_POINT('Ctrl Pts',(20.1753211256205,-20.502586809175,-19.3916925018503));
#79402=CARTESIAN_POINT('Ctrl Pts',(20.1797728982246,-20.4984367972524,-19.3913296634031));
#79403=CARTESIAN_POINT('Ctrl Pts',(20.1903914417592,-20.4884520946125,-19.3904626634993));
#79404=CARTESIAN_POINT('Ctrl Pts',(20.1965411645572,-20.4825993649006,-19.3899592823528));
#79405=CARTESIAN_POINT('Ctrl Pts',(20.2187191964895,-20.4612366821034,-19.3881391361993));
#79406=CARTESIAN_POINT('Ctrl Pts',(20.234537707751,-20.4455103275074,-19.3868317870986));
#79407=CARTESIAN_POINT('Ctrl Pts',(20.3782388263936,-20.2980581212227,-19.3748593846415));
#79408=CARTESIAN_POINT('Ctrl Pts',(20.4887239178553,-20.1504756742736,-19.365029261082));
#79409=CARTESIAN_POINT('Ctrl Pts',(20.6187517210273,-19.9194896954436,-19.3505852645999));
#79410=CARTESIAN_POINT('Ctrl Pts',(20.6545793194179,-19.8462585526793,-19.3461092757742));
#79411=CARTESIAN_POINT('Ctrl Pts',(20.7001745682777,-19.7376019264967,-19.3393714814267));
#79412=CARTESIAN_POINT('Ctrl Pts',(20.7133849161566,-19.703696624504,-19.337255711274));
#79413=CARTESIAN_POINT('Ctrl Pts',(20.7282518299472,-19.662425719248,-19.33464526405));
#79414=CARTESIAN_POINT('Ctrl Pts',(20.7307520027793,-19.6553679687156,-19.3341976301444));
#79415=CARTESIAN_POINT('Ctrl Pts',(20.7345842017419,-19.6443649257486,-19.3334976554587));
#79416=CARTESIAN_POINT('Ctrl Pts',(20.7359421452722,-19.6404286346189,-19.3332468233807));
#79417=CARTESIAN_POINT('Ctrl Pts',(20.7384412667097,-19.6331144696072,-19.3327799214073));
#79418=CARTESIAN_POINT('Ctrl Pts',(20.7395855275842,-19.6297377098414,-19.332564036783));
#79419=CARTESIAN_POINT('Ctrl Pts',(20.7421560610158,-19.6220884441896,-19.3320742636121));
#79420=CARTESIAN_POINT('Ctrl Pts',(20.7435772240377,-19.6178142895679,-19.3318000796951));
#79421=CARTESIAN_POINT('Ctrl Pts',(20.7478318299884,-19.6048808260464,-19.3309689225962));
#79422=CARTESIAN_POINT('Ctrl Pts',(20.7506229784018,-19.5962078613575,-19.3304095549054));
#79423=CARTESIAN_POINT('Ctrl Pts',(20.7716805003414,-19.5292975297536,-19.326080178729));
#79424=CARTESIAN_POINT('Ctrl Pts',(20.7874749007464,-19.4703180656595,-19.3221834057775));
#79425=CARTESIAN_POINT('Ctrl Pts',(20.8135917801933,-19.3526586091225,-19.3143577372729));
#79426=CARTESIAN_POINT('Ctrl Pts',(20.8240302306499,-19.2940562020501,-19.3104354811217));
#79427=CARTESIAN_POINT('Ctrl Pts',(20.8465428347647,-19.1272172980772,-19.2993134985049));
#79428=CARTESIAN_POINT('Ctrl Pts',(20.8527583288167,-19.0183698235923,-19.2921188905391));
#79429=CARTESIAN_POINT('Ctrl Pts',(20.8490716928712,-18.8346776074682,-19.2803153188366));
#79430=CARTESIAN_POINT('Ctrl Pts',(20.8436008343418,-18.759960260913,-19.2756059561699));
#79431=CARTESIAN_POINT('Ctrl Pts',(20.8318188580848,-18.667047596358,-19.2698686535368));
#79432=CARTESIAN_POINT('Ctrl Pts',(20.8292078886343,-18.6484447780359,-19.2687257837066));
#79433=CARTESIAN_POINT('Ctrl Pts',(20.8250486469854,-18.6214282864996,-19.2670740965107));
#79434=CARTESIAN_POINT('Ctrl Pts',(20.8236964948525,-18.6129857457606,-19.2665591017215));
#79435=CARTESIAN_POINT('Ctrl Pts',(20.8212348645011,-18.5981904410859,-19.2656585419943));
#79436=CARTESIAN_POINT('Ctrl Pts',(20.8201474438943,-18.5918341669058,-19.2652722826251));
#79437=CARTESIAN_POINT('Ctrl Pts',(20.8179785525398,-18.5794958455789,-19.2645237014159));
#79438=CARTESIAN_POINT('Ctrl Pts',(20.8169003266819,-18.5735132990433,-19.2641612806003));
#79439=CARTESIAN_POINT('Ctrl Pts',(20.8142595205016,-18.5592138782787,-19.2632962962392));
#79440=CARTESIAN_POINT('Ctrl Pts',(20.8126728040676,-18.5509015247552,-19.2627945047372));
#79441=CARTESIAN_POINT('Ctrl Pts',(20.8067569527533,-18.5208883293069,-19.2609862420577));
#79442=CARTESIAN_POINT('Ctrl Pts',(20.8021373881776,-18.49924570034,-19.2596890244646));
#79443=CARTESIAN_POINT('Ctrl Pts',(20.7556426527245,-18.2970051443598,-19.2476201150878));
#79444=CARTESIAN_POINT('Ctrl Pts',(20.6905574186346,-18.1225746712111,-19.237702832742));
#79445=CARTESIAN_POINT('Ctrl Pts',(20.5659197569792,-17.8879498976698,-19.2232203696414));
#79446=CARTESIAN_POINT('Ctrl Pts',(20.5242625130942,-17.8192640480971,-19.2188063243279));
#79447=CARTESIAN_POINT('Ctrl Pts',(20.4583862459383,-17.7233903089113,-19.2121526814936));
#79448=CARTESIAN_POINT('Ctrl Pts',(20.4372071578838,-17.6941944800549,-19.2100549595936));
#79449=CARTESIAN_POINT('Ctrl Pts',(20.4107559227381,-17.659624531298,-19.2074645333228));
#79450=CARTESIAN_POINT('Ctrl Pts',(20.4061863166082,-17.6537174054475,-19.2070180337968));
#79451=CARTESIAN_POINT('Ctrl Pts',(20.3990230156021,-17.6445579701804,-19.2063194511735));
#79452=CARTESIAN_POINT('Ctrl Pts',(20.3964507768393,-17.6412888503847,-19.2060688670949));
#79453=CARTESIAN_POINT('Ctrl Pts',(20.3916556988359,-17.6352314935894,-19.2056021863816));
#79454=CARTESIAN_POINT('Ctrl Pts',(20.3894354440697,-17.6324412838867,-19.2053862734997));
#79455=CARTESIAN_POINT('Ctrl Pts',(20.3843911162866,-17.6261348097701,-19.2048961250944));
#79456=CARTESIAN_POINT('Ctrl Pts',(20.3815628643992,-17.6226219701065,-19.2046215922564));
#79457=CARTESIAN_POINT('Ctrl Pts',(20.3742318633557,-17.6135758044634,-19.2039107753472));
#79458=CARTESIAN_POINT('Ctrl Pts',(20.3697123727214,-17.6080562053479,-19.2034733252998));
#79459=CARTESIAN_POINT('Ctrl Pts',(20.3417962865494,-17.574312033867,-19.2007764829244));
#79460=CARTESIAN_POINT('Ctrl Pts',(20.3176991783711,-17.5466781257956,-19.198470915906));
#79461=CARTESIAN_POINT('Ctrl Pts',(20.177474574603,-17.3940608236518,-19.185244408539));
#79462=CARTESIAN_POINT('Ctrl Pts',(20.0472904141954,-17.282849099074,-19.1737328150046));
#79463=CARTESIAN_POINT('Ctrl Pts',(19.8257629372119,-17.1357322821224,-19.1564516324388));
#79464=CARTESIAN_POINT('Ctrl Pts',(19.7428800537353,-17.0884174248192,-19.1503957283928));
#79465=CARTESIAN_POINT('Ctrl Pts',(19.6378354680984,-17.0375215562985,-19.1432258790296));
#79466=CARTESIAN_POINT('Ctrl Pts',(19.6184508683527,-17.02848941284,-19.1419224643709));
#79467=CARTESIAN_POINT('Ctrl Pts',(19.5907098734763,-17.0160717096726,-19.1400843555826));
#79468=CARTESIAN_POINT('Ctrl Pts',(19.582464069937,-17.0124436387284,-19.1395413598245));
#79469=CARTESIAN_POINT('Ctrl Pts',(19.5682051399277,-17.0062781867502,-19.1386081095363));
#79470=CARTESIAN_POINT('Ctrl Pts',(19.5622030256673,-17.0037157959389,-19.1382170045572));
#79471=CARTESIAN_POINT('Ctrl Pts',(19.5506923729632,-16.9988645339206,-19.1374702340522));
#79472=CARTESIAN_POINT('Ctrl Pts',(19.5451858307565,-16.9965711135368,-19.1371144167087));
#79473=CARTESIAN_POINT('Ctrl Pts',(19.530851145094,-16.9906718303984,-19.1361918113652));
#79474=CARTESIAN_POINT('Ctrl Pts',(19.52200813731,-16.9871022631275,-19.1356262555011));
#79475=CARTESIAN_POINT('Ctrl Pts',(19.4918208589233,-16.9751534402262,-19.1337075830069));
#79476=CARTESIAN_POINT('Ctrl Pts',(19.4703642364132,-16.9670610722524,-19.1323640975923));
#79477=CARTESIAN_POINT('Ctrl Pts',(19.2828331497991,-16.8997932065347,-19.1207863983065));
#79478=CARTESIAN_POINT('Ctrl Pts',(19.1101036752726,-16.8612290332538,-19.1113112693238));
#79479=CARTESIAN_POINT('Ctrl Pts',(18.8485362089927,-16.8363344380779,-19.0970129366175));
#79480=CARTESIAN_POINT('Ctrl Pts',(18.7620798226963,-16.8334230071062,-19.0922794870084));
#79481=CARTESIAN_POINT('Ctrl Pts',(18.6380318912868,-16.8368407315622,-19.085193286206));
#79482=CARTESIAN_POINT('Ctrl Pts',(18.6004054886259,-16.83888364723,-19.0830044536186));
#79483=CARTESIAN_POINT('Ctrl Pts',(18.5553177162121,-16.8425406270373,-19.0803129940251));
#79484=CARTESIAN_POINT('Ctrl Pts',(18.5477825515759,-16.8431924547958,-19.079860883827));
#79485=CARTESIAN_POINT('Ctrl Pts',(18.5360882550953,-16.8442672329068,-19.0791554174678));
#79486=CARTESIAN_POINT('Ctrl Pts',(18.531926522962,-16.844662156788,-19.0789036084861));
#79487=CARTESIAN_POINT('Ctrl Pts',(18.5242190415939,-16.8454165928799,-19.0784358269419));
#79488=CARTESIAN_POINT('Ctrl Pts',(18.5206730202344,-16.8457727328742,-19.078220045606));
#79489=CARTESIAN_POINT('Ctrl Pts',(18.5126690300257,-16.8465970233165,-19.0777317141393));
#79490=CARTESIAN_POINT('Ctrl Pts',(18.5082116643118,-16.8470703766849,-19.0774588761457));
#79491=CARTESIAN_POINT('Ctrl Pts',(18.4950909112337,-16.8485059002243,-19.0766531940646));
#79492=CARTESIAN_POINT('Ctrl Pts',(18.4864320471011,-16.8495074118605,-19.0761182152734));
#79493=CARTESIAN_POINT('Ctrl Pts',(18.4248767052849,-16.857012617993,-19.072292922822));
#79494=CARTESIAN_POINT('Ctrl Pts',(18.3722406731706,-16.8654577650984,-19.0689057252391));
#79495=CARTESIAN_POINT('Ctrl Pts',(18.3023589698188,-16.8793934208461,-19.0643005646603));
#79496=CARTESIAN_POINT('Ctrl Pts',(18.2847793266029,-16.8831324905262,-19.0631327684647));
#79497=CARTESIAN_POINT('Ctrl Pts',(18.2202253666096,-16.8977242381343,-19.0588147274084));
#79498=CARTESIAN_POINT('Ctrl Pts',(18.1735789140705,-16.9099565985596,-19.0556364797295));
#79499=CARTESIAN_POINT('Ctrl Pts',(18.0225990610318,-16.9551120277866,-19.0452266588094));
#79500=CARTESIAN_POINT('Ctrl Pts',(17.9203845395124,-16.9945306597934,-19.0379941005091));
#79501=CARTESIAN_POINT('Ctrl Pts',(17.7533799965462,-17.0742885084566,-19.0260981496392));
#79502=CARTESIAN_POINT('Ctrl Pts',(17.6868830803873,-17.1105428615085,-19.0213353689672));
#79503=CARTESIAN_POINT('Ctrl Pts',(17.6063835861017,-17.1602055849986,-19.0155404373673));
#79504=CARTESIAN_POINT('Ctrl Pts',(17.5904361796315,-17.1703412707252,-19.0143907435225));
#79505=CARTESIAN_POINT('Ctrl Pts',(17.5674553626784,-17.1853828770944,-19.0127310753828));
#79506=CARTESIAN_POINT('Ctrl Pts',(17.5603130230162,-17.1901199435717,-19.0122148394162));
#79507=CARTESIAN_POINT('Ctrl Pts',(17.547844701473,-17.1984988645741,-19.011312847506));
#79508=CARTESIAN_POINT('Ctrl Pts',(17.5425062721063,-17.2021219122513,-19.0109263903223));
#79509=CARTESIAN_POINT('Ctrl Pts',(17.5321751546603,-17.2092025587906,-19.0101779606139));
#79510=CARTESIAN_POINT('Ctrl Pts',(17.527180623417,-17.2126573444407,-19.0098158865991));
#79511=CARTESIAN_POINT('Ctrl Pts',(17.5152807732225,-17.2209645659733,-19.008952579822));
#79512=CARTESIAN_POINT('Ctrl Pts',(17.5083894353648,-17.2258369212145,-19.0084521122372));
#79513=CARTESIAN_POINT('Ctrl Pts',(17.4836527617036,-17.2435492124087,-19.0066536141676));
#79514=CARTESIAN_POINT('Ctrl Pts',(17.4659781640409,-17.2566260038337,-19.005364705296));
#79515=CARTESIAN_POINT('Ctrl Pts',(17.3000937233961,-17.383403510882,-18.9932203621058));
#79516=CARTESIAN_POINT('Ctrl Pts',(17.167345780027,-17.5159698428672,-18.983234834381));
#79517=CARTESIAN_POINT('Ctrl Pts',(17.00544248396,-17.7272249387109,-18.9687214708651));
#79518=CARTESIAN_POINT('Ctrl Pts',(16.9607585718426,-17.7928632905634,-18.9643555302891));
#79519=CARTESIAN_POINT('Ctrl Pts',(16.9014073609634,-17.89153974784,-18.9577673284734));
#79520=CARTESIAN_POINT('Ctrl Pts',(16.8837304163383,-17.9226925376627,-18.9556837510472));
#79521=CARTESIAN_POINT('Ctrl Pts',(16.8633406756185,-17.9608500406276,-18.9531090179757));
#79522=CARTESIAN_POINT('Ctrl Pts',(16.8598628566578,-17.9674419701935,-18.9526634156439));
#79523=CARTESIAN_POINT('Ctrl Pts',(16.8544998953419,-17.9777384166141,-18.9519659341345));
#79524=CARTESIAN_POINT('Ctrl Pts',(16.8525906926019,-17.9814304282409,-18.9517155463365));
#79525=CARTESIAN_POINT('Ctrl Pts',(16.849063646917,-17.9883005330516,-18.9512490401501));
#79526=CARTESIAN_POINT('Ctrl Pts',(16.8474429570878,-17.9914771002208,-18.9510331043112));
#79527=CARTESIAN_POINT('Ctrl Pts',(16.8437888034243,-17.9986842011171,-18.9505426562364));
#79528=CARTESIAN_POINT('Ctrl Pts',(16.8417602112045,-18.0027171333653,-18.9502678451362));
#79529=CARTESIAN_POINT('Ctrl Pts',(16.8357860256382,-18.0146893217936,-18.9494510214997));
#79530=CARTESIAN_POINT('Ctrl Pts',(16.8318774456107,-18.0226467938838,-18.9489067869505));
#79531=CARTESIAN_POINT('Ctrl Pts',(16.80314318914,-18.0820874656696,-18.9448329603227));
#79532=CARTESIAN_POINT('Ctrl Pts',(16.7803638034158,-18.1345281594861,-18.9411920259084));
#79533=CARTESIAN_POINT('Ctrl Pts',(16.6996314218625,-18.3431009769142,-18.926702986597));
#79534=CARTESIAN_POINT('Ctrl Pts',(16.6580537910332,-18.5049334714458,-18.915500136708));
#79535=CARTESIAN_POINT('Ctrl Pts',(16.6280919357943,-18.7278383788809,-18.9010061658868));
#79536=CARTESIAN_POINT('Ctrl Pts',(16.6227108984473,-18.7859984880139,-18.8973011289853));
#79537=CARTESIAN_POINT('Ctrl Pts',(16.6179213248027,-18.8800322479673,-18.8914414370162));
#79538=CARTESIAN_POINT('Ctrl Pts',(16.6170073710083,-18.9157954316116,-18.8892429293612));
#79539=CARTESIAN_POINT('Ctrl Pts',(16.616997796834,-18.9625398028534,-18.8864068425017));
#79540=CARTESIAN_POINT('Ctrl Pts',(16.6170808697117,-18.9735132186089,-18.8857437458361));
#79541=CARTESIAN_POINT('Ctrl Pts',(16.6173556708795,-18.9914191387053,-18.8846659965562));
#79542=CARTESIAN_POINT('Ctrl Pts',(16.6174961452131,-18.9983521191167,-18.8842497461034));
#79543=CARTESIAN_POINT('Ctrl Pts',(16.6178328488767,-19.0117251986035,-18.8834488062694));
#79544=CARTESIAN_POINT('Ctrl Pts',(16.6180244184857,-19.0181653284832,-18.8830639754413));
#79545=CARTESIAN_POINT('Ctrl Pts',(16.6185373485208,-19.0331125219242,-18.882172803864));
#79546=CARTESIAN_POINT('Ctrl Pts',(16.6188806293231,-19.0416187593832,-18.8816671552148));
#79547=CARTESIAN_POINT('Ctrl Pts',(16.620136566466,-19.0686864914159,-18.8800627579892));
#79548=CARTESIAN_POINT('Ctrl Pts',(16.6212423368452,-19.0872384645813,-18.8789700600468));
#79549=CARTESIAN_POINT('Ctrl Pts',(16.6243860729691,-19.1304038377679,-18.8764423790067));
#79550=CARTESIAN_POINT('Ctrl Pts',(16.6266107498987,-19.155001158676,-18.8750131988553));
#79551=CARTESIAN_POINT('Ctrl Pts',(16.6359173603785,-19.2410813321558,-18.8700446047059));
#79552=CARTESIAN_POINT('Ctrl Pts',(16.6452642973998,-19.3022896030012,-18.8665717716127));
#79553=CARTESIAN_POINT('Ctrl Pts',(16.6784970300946,-19.4702077849289,-18.8571027638153));
#79554=CARTESIAN_POINT('Ctrl Pts',(16.7079721266401,-19.5755543888119,-18.8512347660574));
#79555=CARTESIAN_POINT('Ctrl Pts',(16.7454194032426,-19.6781103292199,-18.8452753983371));
#79556=CARTESIAN_POINT('Origin',(18.734,-18.952,0.));
#79557=CARTESIAN_POINT('',(16.7454193872878,-19.6781102855251,-18.0457833417799));
#79558=CARTESIAN_POINT('',(16.745419450845,-19.6781104595875,-18.2676549380821));
#79559=CARTESIAN_POINT('',(16.7454194499637,-19.6781104571739,0.));
#79560=CARTESIAN_POINT('',(16.6170000023184,-18.9519009238278,-18.3109437209775));
#79561=CARTESIAN_POINT('Ctrl Pts',(16.745419450845,-19.6781104595875,-18.2676549380821));
#79562=CARTESIAN_POINT('Ctrl Pts',(16.7423111909751,-19.6695979460473,-18.2681610694787));
#79563=CARTESIAN_POINT('Ctrl Pts',(16.7392574281066,-19.6610650299046,-18.2686659571902));
#79564=CARTESIAN_POINT('Ctrl Pts',(16.7027368374843,-19.5569145222169,-18.2748002898151));
#79565=CARTESIAN_POINT('Ctrl Pts',(16.6761195712795,-19.4590312384636,-18.2802690475673));
#79566=CARTESIAN_POINT('Ctrl Pts',(16.6333078555506,-19.240845234103,-18.2923592474485));
#79567=CARTESIAN_POINT('Ctrl Pts',(16.6202348295939,-19.1203084927762,-18.2989763297896));
#79568=CARTESIAN_POINT('Ctrl Pts',(16.6172719191199,-18.987828630187,-18.3067856556148));
#79569=CARTESIAN_POINT('Ctrl Pts',(16.6171084239076,-18.9763207955218,-18.3074684926059));
#79570=CARTESIAN_POINT('Ctrl Pts',(16.6170172119703,-18.9612501741062,-18.3083692643783));
#79571=CARTESIAN_POINT('Ctrl Pts',(16.6170046437052,-18.9576878419957,-18.3085826629695));
#79572=CARTESIAN_POINT('Ctrl Pts',(16.6170002821642,-18.953343794759,-18.3088434905605));
#79573=CARTESIAN_POINT('Ctrl Pts',(16.6169999302839,-18.9525620664735,-18.3088904512387));
#79574=CARTESIAN_POINT('Ctrl Pts',(16.617000011396,-18.9517803397697,-18.3089374357138));
#79575=CARTESIAN_POINT('Ctrl Pts',(16.6170000023184,-18.9519009238278,-18.3109437209775));
#79576=CARTESIAN_POINT('Ctrl Pts',(16.6170002492315,-18.9466250329454,-18.3112630160645));
#79577=CARTESIAN_POINT('Ctrl Pts',(16.6170202186042,-18.9413491960951,-18.3115823111514));
#79578=CARTESIAN_POINT('Ctrl Pts',(16.6170599094811,-18.936073507803,-18.3119016062384));
#79579=CARTESIAN_POINT('Ctrl Pts',(16.6176053981758,-18.8635674674004,-18.3162898151688));
#79580=CARTESIAN_POINT('Ctrl Pts',(16.6218813020779,-18.7909479534649,-18.3206780240991));
#79581=CARTESIAN_POINT('Ctrl Pts',(16.6299021760198,-18.7186304494543,-18.3250662330295));
#79582=CARTESIAN_POINT('Ctrl Pts',(16.6379111456549,-18.6464202766101,-18.3294479291303));
#79583=CARTESIAN_POINT('Ctrl Pts',(16.6496539988946,-18.5745116993623,-18.333829625231));
#79584=CARTESIAN_POINT('Ctrl Pts',(16.6650932824123,-18.5033197197107,-18.3382113213318));
#79585=CARTESIAN_POINT('Ctrl Pts',(16.6805144235431,-18.4322113963008,-18.3425878685909));
#79586=CARTESIAN_POINT('Ctrl Pts',(16.6996232646345,-18.3618184668105,-18.34696441585));
#79587=CARTESIAN_POINT('Ctrl Pts',(16.7223308201355,-18.2925486289473,-18.3513409631092));
#79588=CARTESIAN_POINT('Ctrl Pts',(16.7450239748349,-18.2233227210085,-18.3557147348256));
#79589=CARTESIAN_POINT('Ctrl Pts',(16.7713111657669,-18.155218948753,-18.3600885065421));
#79590=CARTESIAN_POINT('Ctrl Pts',(16.8010531665404,-18.0886312844337,-18.3644622782586));
#79591=CARTESIAN_POINT('Ctrl Pts',(16.8307861167232,-18.0220638829642,-18.3688347190216));
#79592=CARTESIAN_POINT('Ctrl Pts',(16.8639715929645,-17.9570121136705,-18.3732071597847));
#79593=CARTESIAN_POINT('Ctrl Pts',(16.9004223233176,-17.8938497726825,-18.3775796005477));
#79594=CARTESIAN_POINT('Ctrl Pts',(16.93687398572,-17.8306858166264,-18.3819521531146));
#79595=CARTESIAN_POINT('Ctrl Pts',(16.9765908251607,-17.7694118015945,-18.3863247056814));
#79596=CARTESIAN_POINT('Ctrl Pts',(17.0193405651388,-17.7103752489413,-18.3906972582483));
#79597=CARTESIAN_POINT('Ctrl Pts',(17.0621346724097,-17.6512774259268,-18.3950743488151));
#79598=CARTESIAN_POINT('Ctrl Pts',(17.1079676812098,-17.5944220931023,-18.3994514393819));
#79599=CARTESIAN_POINT('Ctrl Pts',(17.1565655683569,-17.5401254964174,-18.4038285299488));
#79600=CARTESIAN_POINT('Ctrl Pts',(17.2051899966138,-17.4857992463457,-18.4082080110073));
#79601=CARTESIAN_POINT('Ctrl Pts',(17.2565819695237,-17.4340348572235,-18.4125874920657));
#79602=CARTESIAN_POINT('Ctrl Pts',(17.3104308762818,-17.3851113791988,-18.4169669731242));
#79603=CARTESIAN_POINT('Ctrl Pts',(17.3643752298659,-17.3361011846376,-18.4213542167834));
#79604=CARTESIAN_POINT('Ctrl Pts',(17.4207848402037,-17.2899422626056,-18.4257414604427));
#79605=CARTESIAN_POINT('Ctrl Pts',(17.4793168103112,-17.2468727046017,-18.4301287041019));
#79606=CARTESIAN_POINT('Ctrl Pts',(17.5191129099215,-17.2175895552844,-18.4331116070413));
#79607=CARTESIAN_POINT('Ctrl Pts',(17.5598894741973,-17.1897336331319,-18.4360945099806));
#79608=CARTESIAN_POINT('Ctrl Pts',(17.6015321394767,-17.1633676887404,-18.4390774129199));
#79609=CARTESIAN_POINT('Ctrl Pts',(17.6627935078073,-17.1245802139255,-18.4434656218502));
#79610=CARTESIAN_POINT('Ctrl Pts',(17.7261694924203,-17.0888680068776,-18.4478538307805));
#79611=CARTESIAN_POINT('Ctrl Pts',(17.7913186157342,-17.0564681992225,-18.4522420397107));
#79612=CARTESIAN_POINT('Ctrl Pts',(17.8563710469469,-17.0241164782541,-18.4566237358114));
#79613=CARTESIAN_POINT('Ctrl Pts',(17.9231909643683,-16.995067610473,-18.461005431912));
#79614=CARTESIAN_POINT('Ctrl Pts',(17.9914091442163,-16.96951473627,-18.4653871280127));
#79615=CARTESIAN_POINT('Ctrl Pts',(18.0595471622739,-16.9439918887279,-18.4697636752717));
#79616=CARTESIAN_POINT('Ctrl Pts',(18.1290797293045,-16.9219570424211,-18.4741402225307));
#79617=CARTESIAN_POINT('Ctrl Pts',(18.1996158698649,-16.9035560536203,-18.4785167697897));
#79618=CARTESIAN_POINT('Ctrl Pts',(18.27010727743,-16.8851667344591,-18.482890541506));
#79619=CARTESIAN_POINT('Ctrl Pts',(18.3416005301139,-16.8704068217632,-18.4872643132223));
#79620=CARTESIAN_POINT('Ctrl Pts',(18.4136889989943,-16.8593724978786,-18.4916380849387));
#79621=CARTESIAN_POINT('Ctrl Pts',(18.4857555311115,-16.8483415317759,-18.4960105257016));
#79622=CARTESIAN_POINT('Ctrl Pts',(18.5584164432962,-16.8410339766644,-18.5003829664645));
#79623=CARTESIAN_POINT('Ctrl Pts',(18.6312560654047,-16.8374946952292,-18.5047554072274));
#79624=CARTESIAN_POINT('Ctrl Pts',(18.7040975500304,-16.8339553232942,-18.5091279597941));
#79625=CARTESIAN_POINT('Ctrl Pts',(18.7771172717463,-16.8341844377533,-18.5135005123608));
#79626=CARTESIAN_POINT('Ctrl Pts',(18.8498972932256,-16.8381748375462,-18.5178730649275));
#79627=CARTESIAN_POINT('Ctrl Pts',(18.9227528485563,-16.8421693787264,-18.5222501554942));
#79628=CARTESIAN_POINT('Ctrl Pts',(18.9953677242796,-16.8499329725836,-18.5266272460608));
#79629=CARTESIAN_POINT('Ctrl Pts',(19.0673276840478,-16.8614063869209,-18.5310043366275));
#79630=CARTESIAN_POINT('Ctrl Pts',(19.1393269438208,-16.8728860673155,-18.5353838176858));
#79631=CARTESIAN_POINT('Ctrl Pts',(19.2106701033887,-16.8880795015321,-18.5397632987441));
#79632=CARTESIAN_POINT('Ctrl Pts',(19.2809543980004,-16.9068765595916,-18.5441427798024));
#79633=CARTESIAN_POINT('Ctrl Pts',(19.3513632710527,-16.9257069353104,-18.5485300234615));
#79634=CARTESIAN_POINT('Ctrl Pts',(19.4207090718553,-16.9481535415649,-18.5529172671205));
#79635=CARTESIAN_POINT('Ctrl Pts',(19.4886059995026,-16.974056930669,-18.5573045107796));
#79636=CARTESIAN_POINT('Ctrl Pts',(19.5347693678658,-16.9916687392515,-18.5602874137202));
#79637=CARTESIAN_POINT('Ctrl Pts',(19.580263370974,-17.010877494452,-18.5632703166607));
#79638=CARTESIAN_POINT('Ctrl Pts',(19.6249733426251,-17.0316210002368,-18.5662532196012));
#79639=CARTESIAN_POINT('Ctrl Pts',(19.6907470875151,-17.0621371917536,-18.5706414285353));
#79640=CARTESIAN_POINT('Ctrl Pts',(19.7550796205675,-17.0960960250392,-18.5750296374695));
#79641=CARTESIAN_POINT('Ctrl Pts',(19.817586716273,-17.1333387263383,-18.5794178464036));
#79642=CARTESIAN_POINT('Ctrl Pts',(19.8800010410849,-17.1705261532939,-18.5837995425081));
#79643=CARTESIAN_POINT('Ctrl Pts',(19.9405948958111,-17.2109875282316,-18.5881812386125));
#79644=CARTESIAN_POINT('Ctrl Pts',(19.9990060261177,-17.2545169356115,-18.592562934717));
#79645=CARTESIAN_POINT('Ctrl Pts',(20.0573485186977,-17.2979951924735,-18.5969394819799));
#79646=CARTESIAN_POINT('Ctrl Pts',(20.1135129971313,-17.3445340332472,-18.6013160292427));
#79647=CARTESIAN_POINT('Ctrl Pts',(20.1671651917851,-17.3938836586905,-18.6056925765056));
#79648=CARTESIAN_POINT('Ctrl Pts',(20.2207833609968,-17.4432019873186,-18.6100663482258));
#79649=CARTESIAN_POINT('Ctrl Pts',(20.2718920534934,-17.495327238032,-18.614440119946));
#79650=CARTESIAN_POINT('Ctrl Pts',(20.3201902946194,-17.549969561937,-18.6188138916661));
#79651=CARTESIAN_POINT('Ctrl Pts',(20.3684738384283,-17.6045952579991,-18.6231863324329));
#79652=CARTESIAN_POINT('Ctrl Pts',(20.413948309488,-17.6617361453877,-18.6275587731997));
#79653=CARTESIAN_POINT('Ctrl Pts',(20.4563509910147,-17.7210669946131,-18.6319312139664));
#79654=CARTESIAN_POINT('Ctrl Pts',(20.4987547567825,-17.7803993609347,-18.6363037665369));
#79655=CARTESIAN_POINT('Ctrl Pts',(20.5380862982194,-17.8419214066551,-18.6406763191075));
#79656=CARTESIAN_POINT('Ctrl Pts',(20.5741254487293,-17.9052778148243,-18.645048871678));
#79657=CARTESIAN_POINT('Ctrl Pts',(20.6102020020285,-17.968699976663,-18.6494259622485));
#79658=CARTESIAN_POINT('Ctrl Pts',(20.6429791031795,-18.0339598817704,-18.653803052819));
#79659=CARTESIAN_POINT('Ctrl Pts',(20.6722823388073,-18.1006771616669,-18.6581801433894));
#79660=CARTESIAN_POINT('Ctrl Pts',(20.7016015780196,-18.1674308783458,-18.6625596244515));
#79661=CARTESIAN_POINT('Ctrl Pts',(20.7274430033788,-18.2356431030904,-18.6669391055136));
#79662=CARTESIAN_POINT('Ctrl Pts',(20.7496812078476,-18.3049155632146,-18.6713185865757));
#79663=CARTESIAN_POINT('Ctrl Pts',(20.7719588293843,-18.3743108083083,-18.6757058302384));
#79664=CARTESIAN_POINT('Ctrl Pts',(20.7906203524691,-18.4447695748772,-18.6800930739012));
#79665=CARTESIAN_POINT('Ctrl Pts',(20.8055910206598,-18.5158811594051,-18.684480317564));
#79666=CARTESIAN_POINT('Ctrl Pts',(20.8157696323546,-18.564230184091,-18.6874632204702));
#79667=CARTESIAN_POINT('Ctrl Pts',(20.8242431499881,-18.6128807754351,-18.6904461233765));
#79668=CARTESIAN_POINT('Ctrl Pts',(20.8310018039417,-18.6617028517791,-18.6934290262827));
#79669=CARTESIAN_POINT('Ctrl Pts',(20.8409445967655,-18.7335259978741,-18.6978172352092));
#79670=CARTESIAN_POINT('Ctrl Pts',(20.8472125720512,-18.8060007495856,-18.7022054441356));
#79671=CARTESIAN_POINT('Ctrl Pts',(20.8497312594192,-18.8787180928442,-18.7065936530621));
#79672=CARTESIAN_POINT('Ctrl Pts',(20.8522462086376,-18.9513275115089,-18.7109753491589));
#79673=CARTESIAN_POINT('Ctrl Pts',(20.8510228997993,-19.0241783288765,-18.7153570452558));
#79674=CARTESIAN_POINT('Ctrl Pts',(20.8460383938856,-19.096854488205,-18.7197387413526));
#79675=CARTESIAN_POINT('Ctrl Pts',(20.841059745163,-19.1694452472631,-18.7241152886079));
#79676=CARTESIAN_POINT('Ctrl Pts',(20.8323287119819,-19.2418612771284,-18.7284918358631));
#79677=CARTESIAN_POINT('Ctrl Pts',(20.8198744021603,-19.3136862983475,-18.7328683831184));
#79678=CARTESIAN_POINT('Ctrl Pts',(20.8074279906809,-19.3854657691824,-18.737242154831));
#79679=CARTESIAN_POINT('Ctrl Pts',(20.7912630697939,-19.4566545009247,-18.7416159265437));
#79680=CARTESIAN_POINT('Ctrl Pts',(20.7714604446763,-19.5268425318116,-18.7459896982563));
#79681=CARTESIAN_POINT('Ctrl Pts',(20.7516638455638,-19.5970092042456,-18.7503621390155));
#79682=CARTESIAN_POINT('Ctrl Pts',(20.728231870793,-19.6661753164087,-18.7547345797747));
#79683=CARTESIAN_POINT('Ctrl Pts',(20.7012957832833,-19.7339439245084,-18.759107020534));
#79684=CARTESIAN_POINT('Ctrl Pts',(20.6743590070147,-19.8017142654596,-18.763479573097));
#79685=CARTESIAN_POINT('Ctrl Pts',(20.6439181201448,-19.8680865838727,-18.7678521256601));
#79686=CARTESIAN_POINT('Ctrl Pts',(20.6101527159953,-19.9326834281578,-18.7722246782232));
#79687=CARTESIAN_POINT('Ctrl Pts',(20.5763522688351,-19.9973473134859,-18.7766017687863));
#79688=CARTESIAN_POINT('Ctrl Pts',(20.5392206395556,-20.0602316172898,-18.7809788593495));
#79689=CARTESIAN_POINT('Ctrl Pts',(20.4989832512011,-20.1209837992802,-18.7853559499126));
#79690=CARTESIAN_POINT('Ctrl Pts',(20.458723887715,-20.1817691602927,-18.7897354309674));
#79691=CARTESIAN_POINT('Ctrl Pts',(20.4153556750915,-20.2404196929921,-18.7941149120222));
#79692=CARTESIAN_POINT('Ctrl Pts',(20.3691456171804,-20.2966143724562,-18.798494393077));
#79693=CARTESIAN_POINT('Ctrl Pts',(20.3228536522506,-20.352908656614,-18.8028816367327));
#79694=CARTESIAN_POINT('Ctrl Pts',(20.2737101085666,-20.4067380382461,-18.8072688803884));
#79695=CARTESIAN_POINT('Ctrl Pts',(20.2220198585457,-20.4578173529926,-18.8116561240441));
#79696=CARTESIAN_POINT('Ctrl Pts',(20.1868754689055,-20.4925463655101,-18.8146390270174));
#79697=CARTESIAN_POINT('Ctrl Pts',(20.1505545743005,-20.5260048960148,-18.8176219299908));
#79698=CARTESIAN_POINT('Ctrl Pts',(20.1131612647177,-20.5581143190639,-18.8206048329642));
#79699=CARTESIAN_POINT('Ctrl Pts',(20.0581512102737,-20.6053511411,-18.8249930418924));
#79700=CARTESIAN_POINT('Ctrl Pts',(20.0006041495887,-20.6498507249,-18.8293812508206));
#79701=CARTESIAN_POINT('Ctrl Pts',(19.9408236893631,-20.6913290611014,-18.8337694597489));
#79702=CARTESIAN_POINT('Ctrl Pts',(19.8811319532531,-20.7327458365742,-18.8381511558474));
#79703=CARTESIAN_POINT('Ctrl Pts',(19.8192137908502,-20.7711499931519,-18.8425328519459));
#79704=CARTESIAN_POINT('Ctrl Pts',(19.7554066235765,-20.8062970391267,-18.8469145480445));
#79705=CARTESIAN_POINT('Ctrl Pts',(19.6916744348034,-20.8414027845247,-18.8512910953013));
#79706=CARTESIAN_POINT('Ctrl Pts',(19.626058071091,-20.8732587908218,-18.8556676425582));
#79707=CARTESIAN_POINT('Ctrl Pts',(19.5589233130916,-20.9016642089134,-18.860044189815));
#79708=CARTESIAN_POINT('Ctrl Pts',(19.4918311309808,-20.9300516127014,-18.8644179615291));
#79709=CARTESIAN_POINT('Ctrl Pts',(19.4232229083438,-20.9549925826767,-18.8687917332433));
#79710=CARTESIAN_POINT('Ctrl Pts',(19.3534870964552,-20.9763331586786,-18.8731655049574));
#79711=CARTESIAN_POINT('Ctrl Pts',(19.2837725054089,-20.9976672406713,-18.8775379457181));
#79712=CARTESIAN_POINT('Ctrl Pts',(19.2129314673137,-21.0154029627471,-18.8819103864787));
#79713=CARTESIAN_POINT('Ctrl Pts',(19.1413687992101,-21.0294358381019,-18.8862828272394));
#79714=CARTESIAN_POINT('Ctrl Pts',(19.0698043012416,-21.0434690722788,-18.8906553798038));
#79715=CARTESIAN_POINT('Ctrl Pts',(18.9975186103771,-21.0537991808917,-18.8950279323683));
#79716=CARTESIAN_POINT('Ctrl Pts',(18.9249263141295,-21.0603728661157,-18.8994004849327));
#79717=CARTESIAN_POINT('Ctrl Pts',(18.8522586788592,-21.0669533737582,-18.9037775754971));
#79718=CARTESIAN_POINT('Ctrl Pts',(18.7792842843246,-21.0697696306809,-18.9081546660614));
#79719=CARTESIAN_POINT('Ctrl Pts',(18.706421578337,-21.0688203586177,-18.9125317566258));
#79720=CARTESIAN_POINT('Ctrl Pts',(18.6335190793216,-21.0678705681219,-18.9169112376818));
#79721=CARTESIAN_POINT('Ctrl Pts',(18.5607288719989,-21.0631511854097,-18.9212907187378));
#79722=CARTESIAN_POINT('Ctrl Pts',(18.4884654116451,-21.0547129537627,-18.9256701997938));
#79723=CARTESIAN_POINT('Ctrl Pts',(18.4160738647929,-21.0462597654067,-18.9300574434505));
#79724=CARTESIAN_POINT('Ctrl Pts',(18.3442114053898,-21.0340746456018,-18.9344446871072));
#79725=CARTESIAN_POINT('Ctrl Pts',(18.2732828331918,-21.0182595897438,-18.938831930764));
#79726=CARTESIAN_POINT('Ctrl Pts',(18.22505823831,-21.0075068755956,-18.9418148337245));
#79727=CARTESIAN_POINT('Ctrl Pts',(18.1772650979154,-20.9950772191552,-18.944797736685));
#79728=CARTESIAN_POINT('Ctrl Pts',(18.1300258654971,-20.9810155851672,-18.9477806396456));
#79729=CARTESIAN_POINT('Ctrl Pts',(18.0605280442509,-20.9603282692373,-18.9521690525416));
#79730=CARTESIAN_POINT('Ctrl Pts',(17.9919586602188,-20.9360257809644,-18.9565574654377));
#79731=CARTESIAN_POINT('Ctrl Pts',(17.9247209128513,-20.9082096920074,-18.9609458783338));
#79732=CARTESIAN_POINT('Ctrl Pts',(17.8574469480808,-20.8803786200008,-18.9653366550348));
#79733=CARTESIAN_POINT('Ctrl Pts',(17.7915065313157,-20.8490302580147,-18.9697274317358));
#79734=CARTESIAN_POINT('Ctrl Pts',(17.7272902809765,-20.8143169820478,-18.9741182084367));
#79735=CARTESIAN_POINT('Ctrl Pts',(17.6632831695812,-20.779716759986,-18.9784946852931));
#79736=CARTESIAN_POINT('Ctrl Pts',(17.6009894538961,-20.7417737029155,-18.9828711621495));
#79737=CARTESIAN_POINT('Ctrl Pts',(17.5407759393722,-20.7006867475734,-18.9872476390058));
#79738=CARTESIAN_POINT('Ctrl Pts',(17.4806016974324,-20.659626590051,-18.9916212614273));
#79739=CARTESIAN_POINT('Ctrl Pts',(17.4225053614458,-20.6154268749417,-18.9959948838488));
#79740=CARTESIAN_POINT('Ctrl Pts',(17.3668265523033,-20.5683309574197,-19.0003685062703));
#79741=CARTESIAN_POINT('Ctrl Pts',(17.3111656906036,-20.521250220741,-19.0047407189034));
#79742=CARTESIAN_POINT('Ctrl Pts',(17.2579211759187,-20.4712754472109,-19.0091129315366));
#79743=CARTESIAN_POINT('Ctrl Pts',(17.207399864766,-20.4186905014704,-19.0134851441697));
#79744=CARTESIAN_POINT('Ctrl Pts',(17.1565195529559,-20.3657318910396,-19.0178884254187));
#79745=CARTESIAN_POINT('Ctrl Pts',(17.1084016691149,-20.3101261971702,-19.0222917066677));
#79746=CARTESIAN_POINT('Ctrl Pts',(17.0633209237031,-20.2522001476787,-19.0266949879167));
#79747=CARTESIAN_POINT('Ctrl Pts',(17.0185206470214,-20.1946344836554,-19.0310708742615));
#79748=CARTESIAN_POINT('Ctrl Pts',(16.9767200691604,-20.134777679211,-19.0354467606063));
#79749=CARTESIAN_POINT('Ctrl Pts',(16.9381461790676,-20.0729808445475,-19.0398226469511));
#79750=CARTESIAN_POINT('Ctrl Pts',(16.8992100556101,-20.0106036982979,-19.0442396256522));
#79751=CARTESIAN_POINT('Ctrl Pts',(16.8635617987445,-19.9462503235747,-19.0486566043533));
#79752=CARTESIAN_POINT('Ctrl Pts',(16.8313871436981,-19.8803066944898,-19.0530735830544));
#79753=CARTESIAN_POINT('Ctrl Pts',(16.7992124886517,-19.814363065405,-19.0574905617554));
#79754=CARTESIAN_POINT('Ctrl Pts',(16.7705115857647,-19.7468296619722,-19.0619075404565));
#79755=CARTESIAN_POINT('Ctrl Pts',(16.7454194499637,-19.6781104571739,-19.0663245191576));
#79756=CARTESIAN_POINT('',(16.617000908626,-18.9539458502908,-18.0890147563015));
#79757=CARTESIAN_POINT('Ctrl Pts',(16.7454194032426,-19.6781103292199,-18.8452753983371));
#79758=CARTESIAN_POINT('Ctrl Pts',(16.7566881939313,-19.7089718906256,-18.8434820805428));
#79759=CARTESIAN_POINT('Ctrl Pts',(16.7686789069382,-19.7395806962145,-18.8416796834934));
#79760=CARTESIAN_POINT('Ctrl Pts',(16.8104694161502,-19.8393480406311,-18.8356907683221));
#79761=CARTESIAN_POINT('Ctrl Pts',(16.8432351201276,-19.9071764613245,-18.8314361897634));
#79762=CARTESIAN_POINT('Ctrl Pts',(16.8841144424798,-19.981418490006,-18.8264131304831));
#79763=CARTESIAN_POINT('Ctrl Pts',(16.8887460996236,-19.9896979517452,-18.8258476330491));
#79764=CARTESIAN_POINT('Ctrl Pts',(16.8956954529312,-20.001926834905,-18.8250040381805));
#79765=CARTESIAN_POINT('Ctrl Pts',(16.8979706403711,-20.0059004488585,-18.8247286065803));
#79766=CARTESIAN_POINT('Ctrl Pts',(16.9020434470251,-20.0129603879956,-18.8242368412663));
#79767=CARTESIAN_POINT('Ctrl Pts',(16.9038360027987,-20.0160495759128,-18.8240208358815));
#79768=CARTESIAN_POINT('Ctrl Pts',(16.9077088762315,-20.0226851241615,-18.8235550636621));
#79769=CARTESIAN_POINT('Ctrl Pts',(16.9097916793271,-20.0262299129979,-18.8233051407437));
#79770=CARTESIAN_POINT('Ctrl Pts',(16.9155744862816,-20.03600653928,-18.8226128459874));
#79771=CARTESIAN_POINT('Ctrl Pts',(16.9192961456524,-20.042225409565,-18.8221690997641));
#79772=CARTESIAN_POINT('Ctrl Pts',(16.9399459765362,-20.0763324587598,-18.8197172739954));
#79773=CARTESIAN_POINT('Ctrl Pts',(16.9574841480153,-20.1038439448968,-18.8176726554272));
#79774=CARTESIAN_POINT('Ctrl Pts',(17.0662168518925,-20.2660155521638,-18.805264759139));
#79775=CARTESIAN_POINT('Ctrl Pts',(17.172044238368,-20.3902043111935,-18.7943129840949));
#79776=CARTESIAN_POINT('Ctrl Pts',(17.3764984374317,-20.5806550935415,-18.7760619146059));
#79777=CARTESIAN_POINT('Ctrl Pts',(17.468403734541,-20.6530590231472,-18.7686227995385));
#79778=CARTESIAN_POINT('Ctrl Pts',(17.5777443467583,-20.7254052103008,-18.7606173482261));
#79779=CARTESIAN_POINT('Ctrl Pts',(17.5897407312338,-20.733169255611,-18.759749393334));
#79780=CARTESIAN_POINT('Ctrl Pts',(17.608958805573,-20.7453328714826,-18.7583751118294));
#79781=CARTESIAN_POINT('Ctrl Pts',(17.6161296709972,-20.7498115607239,-18.7578658573277));
#79782=CARTESIAN_POINT('Ctrl Pts',(17.6288239836027,-20.7576346977653,-18.7569704863235));
#79783=CARTESIAN_POINT('Ctrl Pts',(17.6343362262835,-20.7609970357085,-18.7565837137265));
#79784=CARTESIAN_POINT('Ctrl Pts',(17.6457691779259,-20.7678992983185,-18.7557856437207));
#79785=CARTESIAN_POINT('Ctrl Pts',(17.6516919854971,-20.7714356122765,-18.7553744817097));
#79786=CARTESIAN_POINT('Ctrl Pts',(17.6669394830321,-20.7804385918038,-18.754321758977));
#79787=CARTESIAN_POINT('Ctrl Pts',(17.6762890194396,-20.7858629499039,-18.7536817396316));
#79788=CARTESIAN_POINT('Ctrl Pts',(17.7154849428461,-20.8082039297598,-18.7510209714955));
#79789=CARTESIAN_POINT('Ctrl Pts',(17.7456997525526,-20.8244659591105,-18.749023753765));
#79790=CARTESIAN_POINT('Ctrl Pts',(17.8254447527903,-20.8649174860893,-18.7438793930431));
#79791=CARTESIAN_POINT('Ctrl Pts',(17.8755486531456,-20.8879204209889,-18.7407716447346));
#79792=CARTESIAN_POINT('Ctrl Pts',(18.0275779349079,-20.950653079891,-18.7316269039943));
#79793=CARTESIAN_POINT('Ctrl Pts',(18.1317423616883,-20.9844696524625,-18.7257386398546));
#79794=CARTESIAN_POINT('Ctrl Pts',(18.2827853275708,-21.0208672103745,-18.7172798203817));
#79795=CARTESIAN_POINT('Ctrl Pts',(18.3278563773501,-21.0301851048364,-18.7147638438892));
#79796=CARTESIAN_POINT('Ctrl Pts',(18.3949976153116,-21.0417980794796,-18.7109848781702));
#79797=CARTESIAN_POINT('Ctrl Pts',(18.4168587241051,-21.0452271719869,-18.7097495995151));
#79798=CARTESIAN_POINT('Ctrl Pts',(18.4897489455725,-21.0554925537055,-18.7056033962618));
#79799=CARTESIAN_POINT('Ctrl Pts',(18.5409694612286,-21.0608095662436,-18.7026452989099));
#79800=CARTESIAN_POINT('Ctrl Pts',(18.6009481606497,-21.0648324230259,-18.699077409215));
#79801=CARTESIAN_POINT('Ctrl Pts',(18.6095715145293,-21.0653577988538,-18.6985619360271));
#79802=CARTESIAN_POINT('Ctrl Pts',(18.6226567844534,-21.0660746513971,-18.6977756223819));
#79803=CARTESIAN_POINT('Ctrl Pts',(18.627116608313,-21.0663048226472,-18.6975068987528));
#79804=CARTESIAN_POINT('Ctrl Pts',(18.635135790304,-21.0666932548656,-18.6970223501101));
#79805=CARTESIAN_POINT('Ctrl Pts',(18.638694845575,-21.0668566432179,-18.6968068152881));
#79806=CARTESIAN_POINT('Ctrl Pts',(18.6464438424468,-21.0671927818179,-18.6963364759373));
#79807=CARTESIAN_POINT('Ctrl Pts',(18.650633836454,-21.0673620652389,-18.6960814852294));
#79808=CARTESIAN_POINT('Ctrl Pts',(18.662442174101,-21.067804005904,-18.6953610256101));
#79809=CARTESIAN_POINT('Ctrl Pts',(18.6700614367456,-21.0680479602122,-18.6948939967365));
#79810=CARTESIAN_POINT('Ctrl Pts',(18.7164072015587,-21.0692813272485,-18.6920407641863));
#79811=CARTESIAN_POINT('Ctrl Pts',(18.7551509430224,-21.0692486686368,-18.6896028519034));
#79812=CARTESIAN_POINT('Ctrl Pts',(18.8845131907873,-21.0655888262614,-18.681333952897));
#79813=CARTESIAN_POINT('Ctrl Pts',(18.974893523719,-21.0572031384328,-18.6753490967955));
#79814=CARTESIAN_POINT('Ctrl Pts',(19.1307471124744,-21.0325733814219,-18.6649220879059));
#79815=CARTESIAN_POINT('Ctrl Pts',(19.1965089919515,-21.0189494052263,-18.660487687018));
#79816=CARTESIAN_POINT('Ctrl Pts',(19.3726487719311,-20.9736293677325,-18.6486167199407));
#79817=CARTESIAN_POINT('Ctrl Pts',(19.4812879707059,-20.9360427574739,-18.6413128955223));
#79818=CARTESIAN_POINT('Ctrl Pts',(19.5994120513845,-20.8840854817969,-18.6334336638356));
#79819=CARTESIAN_POINT('Ctrl Pts',(19.6124064128512,-20.8782124797467,-18.6325675373782));
#79820=CARTESIAN_POINT('Ctrl Pts',(19.6330013965653,-20.8686525038525,-18.6311955947777));
#79821=CARTESIAN_POINT('Ctrl Pts',(19.6406408312576,-20.8650506365165,-18.6306868662307));
#79822=CARTESIAN_POINT('Ctrl Pts',(19.6540808683156,-20.8586152906548,-18.6297921068231));
#79823=CARTESIAN_POINT('Ctrl Pts',(19.6598904104937,-20.8558008351681,-18.629405422689));
#79824=CARTESIAN_POINT('Ctrl Pts',(19.6718843373592,-20.849922443605,-18.6286072350012));
#79825=CARTESIAN_POINT('Ctrl Pts',(19.6780668011357,-20.8468547461299,-18.6281958683257));
#79826=CARTESIAN_POINT('Ctrl Pts',(19.6939073019939,-20.8388980227925,-18.6271419992971));
#79827=CARTESIAN_POINT('Ctrl Pts',(19.7035431180672,-20.8339650171127,-18.6265010449154));
#79828=CARTESIAN_POINT('Ctrl Pts',(19.7436812226261,-20.8130264287069,-18.6238311729969));
#79829=CARTESIAN_POINT('Ctrl Pts',(19.7738294151995,-20.7963509768782,-18.6218259925375));
#79830=CARTESIAN_POINT('Ctrl Pts',(19.8513829875248,-20.750948394958,-18.61665646518));
#79831=CARTESIAN_POINT('Ctrl Pts',(19.8980917830871,-20.7210819776976,-18.6135320203849));
#79832=CARTESIAN_POINT('Ctrl Pts',(20.0335300057599,-20.6267907518905,-18.6043581632974));
#79833=CARTESIAN_POINT('Ctrl Pts',(20.1184857249567,-20.5572733191734,-18.5984573789497));
#79834=CARTESIAN_POINT('Ctrl Pts',(20.2426992191399,-20.4384047657141,-18.5890955320172));
#79835=CARTESIAN_POINT('Ctrl Pts',(20.2857958590893,-20.3933539943715,-18.5856824603306));
#79836=CARTESIAN_POINT('Ctrl Pts',(20.3639012475826,-20.3041377457612,-18.5790298356332));
#79837=CARTESIAN_POINT('Ctrl Pts',(20.399256256701,-20.2603481887809,-18.5758080523372));
#79838=CARTESIAN_POINT('Ctrl Pts',(20.438092472647,-20.2081193643591,-18.5719465619758));
#79839=CARTESIAN_POINT('Ctrl Pts',(20.4433182777822,-20.2009988118277,-18.5714197176639));
#79840=CARTESIAN_POINT('Ctrl Pts',(20.4511432992934,-20.1901955442262,-18.5706194554781));
#79841=CARTESIAN_POINT('Ctrl Pts',(20.4537756370564,-20.1865367849415,-18.5703482686789));
#79842=CARTESIAN_POINT('Ctrl Pts',(20.4584693906847,-20.1799686618464,-18.5698610983468));
#79843=CARTESIAN_POINT('Ctrl Pts',(20.4605351578184,-20.1770624728657,-18.5696454190418));
#79844=CARTESIAN_POINT('Ctrl Pts',(20.4649961607319,-20.1707528917966,-18.5691768850585));
#79845=CARTESIAN_POINT('Ctrl Pts',(20.4673886733092,-20.1673476976924,-18.5689238557573));
#79846=CARTESIAN_POINT('Ctrl Pts',(20.4740516026647,-20.1578048464379,-18.5682143389553));
#79847=CARTESIAN_POINT('Ctrl Pts',(20.4782995167663,-20.151651657609,-18.5677563648471));
#79848=CARTESIAN_POINT('Ctrl Pts',(20.5029286578228,-20.1155684793673,-18.5650685572634));
#79849=CARTESIAN_POINT('Ctrl Pts',(20.5225705690355,-20.0851439269181,-18.5627935961272));
#79850=CARTESIAN_POINT('Ctrl Pts',(20.5834967394197,-19.9852383128982,-18.5553330064697));
#79851=CARTESIAN_POINT('Ctrl Pts',(20.6215844027536,-19.9138955167407,-18.5500224958001));
#79852=CARTESIAN_POINT('Ctrl Pts',(20.7329517894314,-19.6730640035333,-18.5325028904051));
#79853=CARTESIAN_POINT('Ctrl Pts',(20.7881900015719,-19.4961251383215,-18.5203482820602));
#79854=CARTESIAN_POINT('Ctrl Pts',(20.823578394119,-19.292359193749,-18.5076281932193));
#79855=CARTESIAN_POINT('Ctrl Pts',(20.8270341481658,-19.2704185288717,-18.5062730881744));
#79856=CARTESIAN_POINT('Ctrl Pts',(20.8313307743985,-19.2400354945448,-18.5044159785995));
#79857=CARTESIAN_POINT('Ctrl Pts',(20.8324670567682,-19.2316369758864,-18.503904672391));
#79858=CARTESIAN_POINT('Ctrl Pts',(20.8343321428887,-19.2171997031284,-18.5030291612216));
#79859=CARTESIAN_POINT('Ctrl Pts',(20.8350854048173,-19.2111642642324,-18.5026641873878));
#79860=CARTESIAN_POINT('Ctrl Pts',(20.8365834849316,-19.1987250499832,-18.5019140550896));
#79861=CARTESIAN_POINT('Ctrl Pts',(20.8373250833411,-19.1923209449959,-18.5015290019172));
#79862=CARTESIAN_POINT('Ctrl Pts',(20.8389808961183,-19.1774270115935,-18.5006360895484));
#79863=CARTESIAN_POINT('Ctrl Pts',(20.8398730268565,-19.168934802639,-18.5001289310879));
#79864=CARTESIAN_POINT('Ctrl Pts',(20.8425572207124,-19.1418051705631,-18.4985148331182));
#79865=CARTESIAN_POINT('Ctrl Pts',(20.8441534603499,-19.1231489494608,-18.4974140497023));
#79866=CARTESIAN_POINT('Ctrl Pts',(20.8472975481736,-19.0796086255421,-18.4948649144028));
#79867=CARTESIAN_POINT('Ctrl Pts',(20.8486537667875,-19.054713233871,-18.4934225047331));
#79868=CARTESIAN_POINT('Ctrl Pts',(20.8518757022942,-18.967099821794,-18.4883928473224));
#79869=CARTESIAN_POINT('Ctrl Pts',(20.8513931145288,-18.9043262670549,-18.4848740890824));
#79870=CARTESIAN_POINT('Ctrl Pts',(20.8428720657502,-18.7410579587601,-18.4758356516143));
#79871=CARTESIAN_POINT('Ctrl Pts',(20.8304470317565,-18.6409562042584,-18.4704107149107));
#79872=CARTESIAN_POINT('Ctrl Pts',(20.7965003148142,-18.4689423211722,-18.4608584099424));
#79873=CARTESIAN_POINT('Ctrl Pts',(20.778202868702,-18.3965853635209,-18.4567643522567));
#79874=CARTESIAN_POINT('Ctrl Pts',(20.7434988088597,-18.2845993373892,-18.4501073430232));
#79875=CARTESIAN_POINT('Ctrl Pts',(20.7296422710282,-18.2442426404533,-18.4476401718042));
#79876=CARTESIAN_POINT('Ctrl Pts',(20.7119384163549,-18.1973448132485,-18.4446622154976));
#79877=CARTESIAN_POINT('Ctrl Pts',(20.7092625937099,-18.1903685195962,-18.4442162996176));
#79878=CARTESIAN_POINT('Ctrl Pts',(20.7048754146731,-18.1791090807788,-18.4434916390452));
#79879=CARTESIAN_POINT('Ctrl Pts',(20.7031868665043,-18.1748170376021,-18.443214228184));
#79880=CARTESIAN_POINT('Ctrl Pts',(20.7001646590617,-18.1672081079149,-18.4427202904085));
#79881=CARTESIAN_POINT('Ctrl Pts',(20.6988366100738,-18.1638890459291,-18.4425041030383));
#79882=CARTESIAN_POINT('Ctrl Pts',(20.6959712249961,-18.156780132217,-18.4420394824604));
#79883=CARTESIAN_POINT('Ctrl Pts',(20.6944313352032,-18.1529914236201,-18.4417909012787));
#79884=CARTESIAN_POINT('Ctrl Pts',(20.690169542193,-18.1425922974893,-18.4411060081735));
#79885=CARTESIAN_POINT('Ctrl Pts',(20.6874251472724,-18.135991239428,-18.4406683688955));
#79886=CARTESIAN_POINT('Ctrl Pts',(20.6725197096794,-18.1006454991603,-18.4383099641676));
#79887=CARTESIAN_POINT('Ctrl Pts',(20.6597582143494,-18.0721601217494,-18.4363558007127));
#79888=CARTESIAN_POINT('Ctrl Pts',(20.5760966198343,-17.8959633301123,-18.4239771898663));
#79889=CARTESIAN_POINT('Ctrl Pts',(20.4888791166918,-17.7566203763466,-18.4129410329578));
#79890=CARTESIAN_POINT('Ctrl Pts',(20.3132340903315,-17.537279171229,-18.3945838729834));
#79891=CARTESIAN_POINT('Ctrl Pts',(20.2325273192082,-17.4520536403855,-18.3871198485398));
#79892=CARTESIAN_POINT('Ctrl Pts',(20.1345136163129,-17.364405931851,-18.3790912181555));
#79893=CARTESIAN_POINT('Ctrl Pts',(20.1237621753973,-17.3549857776881,-18.3782229636172));
#79894=CARTESIAN_POINT('Ctrl Pts',(20.106499878153,-17.3401673208972,-18.3768482988525));
#79895=CARTESIAN_POINT('Ctrl Pts',(20.1000508048977,-17.3346980174894,-18.3763389581962));
#79896=CARTESIAN_POINT('Ctrl Pts',(20.0886196633919,-17.3251206991501,-18.3754434869755));
#79897=CARTESIAN_POINT('Ctrl Pts',(20.0836512779953,-17.3209965906778,-18.3750566998546));
#79898=CARTESIAN_POINT('Ctrl Pts',(20.0733366261643,-17.3125141117848,-18.3742586489582));
#79899=CARTESIAN_POINT('Ctrl Pts',(20.0679877660476,-17.3081590047671,-18.3738475203385));
#79900=CARTESIAN_POINT('Ctrl Pts',(20.0542045866659,-17.2970481506091,-18.3727949846699));
#79901=CARTESIAN_POINT('Ctrl Pts',(20.0457395867717,-17.290330647359,-18.3721551179221));
#79902=CARTESIAN_POINT('Ctrl Pts',(20.0102055714285,-17.2625729574387,-18.3694958325998));
#79903=CARTESIAN_POINT('Ctrl Pts',(19.9826780098854,-17.2421263740964,-18.3674999116233));
#79904=CARTESIAN_POINT('Ctrl Pts',(19.9096807218189,-17.1906098513979,-18.362359645393));
#79905=CARTESIAN_POINT('Ctrl Pts',(19.8634732909611,-17.1606286972659,-18.3592546126373));
#79906=CARTESIAN_POINT('Ctrl Pts',(19.727837858173,-17.079960403585,-18.3504794197238));
#79907=CARTESIAN_POINT('Ctrl Pts',(19.6358199211269,-17.0339364658272,-18.3449341285276));
#79908=CARTESIAN_POINT('Ctrl Pts',(19.4803896648853,-16.9698636977147,-18.3357918249254));
#79909=CARTESIAN_POINT('Ctrl Pts',(19.4188372419515,-16.9477647244043,-18.3322228016808));
#79910=CARTESIAN_POINT('Ctrl Pts',(19.2986437188813,-16.9107961091291,-18.3251901395197));
#79911=CARTESIAN_POINT('Ctrl Pts',(19.2401953705464,-16.8955222643694,-18.3217421064812));
#79912=CARTESIAN_POINT('Ctrl Pts',(19.1724048409849,-16.8808720943795,-18.3176284568805));
#79913=CARTESIAN_POINT('Ctrl Pts',(19.1636175382026,-16.8790315076044,-18.317093039572));
#79914=CARTESIAN_POINT('Ctrl Pts',(19.1503711548645,-16.8763447640996,-18.3162822750475));
#79915=CARTESIAN_POINT('Ctrl Pts',(19.1459204975999,-16.8754569352647,-18.316009246889));
#79916=CARTESIAN_POINT('Ctrl Pts',(19.1379657000894,-16.8738966713928,-18.3155200946242));
#79917=CARTESIAN_POINT('Ctrl Pts',(19.1344626835415,-16.8732187777328,-18.3153042852115));
#79918=CARTESIAN_POINT('Ctrl Pts',(19.1268921048169,-16.8717735875005,-18.3148370007428));
#79919=CARTESIAN_POINT('Ctrl Pts',(19.1228240583786,-16.8710093743036,-18.3145853593082));
#79920=CARTESIAN_POINT('Ctrl Pts',(19.1115023629221,-16.8689168652911,-18.3138835525874));
#79921=CARTESIAN_POINT('Ctrl Pts',(19.1042440573122,-16.8676145475311,-18.3134319514192));
#79922=CARTESIAN_POINT('Ctrl Pts',(19.0640934201704,-16.8606268706243,-18.3109251497323));
#79923=CARTESIAN_POINT('Ctrl Pts',(19.0310789275326,-16.8556825015567,-18.3088317579333));
#79924=CARTESIAN_POINT('Ctrl Pts',(18.8373260946397,-16.8313339153715,-18.2964120106022));
#79925=CARTESIAN_POINT('Ctrl Pts',(18.6749075199446,-16.8296406854287,-18.2855109424445));
#79926=CARTESIAN_POINT('Ctrl Pts',(18.3979805757313,-16.858591214453,-18.2673255206477));
#79927=CARTESIAN_POINT('Ctrl Pts',(18.283261350022,-16.880258746877,-18.2599031165561));
#79928=CARTESIAN_POINT('Ctrl Pts',(18.1571215227772,-16.9150649736418,-18.2519132263159));
#79929=CARTESIAN_POINT('Ctrl Pts',(18.1433890974706,-16.9190042162842,-18.251045479298));
#79930=CARTESIAN_POINT('Ctrl Pts',(18.1215956177038,-16.9254952916182,-18.2496714636791));
#79931=CARTESIAN_POINT('Ctrl Pts',(18.1135083425481,-16.927956876245,-18.2491622689517));
#79932=CARTESIAN_POINT('Ctrl Pts',(18.0992705550748,-16.9323838932443,-18.2482669674717));
#79933=CARTESIAN_POINT('Ctrl Pts',(18.0931139241121,-16.93432913336,-18.2478802049454));
#79934=CARTESIAN_POINT('Ctrl Pts',(18.0803978464947,-16.9384109619467,-18.2470821216522));
#79935=CARTESIAN_POINT('Ctrl Pts',(18.0738397439389,-16.9405515101588,-18.2466709364509));
#79936=CARTESIAN_POINT('Ctrl Pts',(18.057031618539,-16.9461286979084,-18.2456180838121));
#79937=CARTESIAN_POINT('Ctrl Pts',(18.0467971646687,-16.9496118908345,-18.2449779584978));
#79938=CARTESIAN_POINT('Ctrl Pts',(18.0047965984569,-16.964266302249,-18.2423544795766));
#79939=CARTESIAN_POINT('Ctrl Pts',(17.9732714908691,-16.9761166088163,-18.2403936915787));
#79940=CARTESIAN_POINT('Ctrl Pts',(17.8919727295616,-17.0089112646876,-18.2353480281249));
#79941=CARTESIAN_POINT('Ctrl Pts',(17.8426929771977,-17.0310168764147,-18.2323009029342));
#79942=CARTESIAN_POINT('Ctrl Pts',(17.6803077428662,-17.1114547002125,-18.2222154692447));
#79943=CARTESIAN_POINT('Ctrl Pts',(17.5716302494621,-17.1780858783338,-18.2154056647421));
#79944=CARTESIAN_POINT('Ctrl Pts',(17.3877165003719,-17.3150422530441,-18.2028664152522));
#79945=CARTESIAN_POINT('Ctrl Pts',(17.3103691808172,-17.3818472560374,-18.1971988908188));
#79946=CARTESIAN_POINT('Ctrl Pts',(17.2312944835982,-17.4608061670488,-18.1905785117495));
#79947=CARTESIAN_POINT('Ctrl Pts',(17.224484104867,-17.4677006128363,-18.1900010107411));
#79948=CARTESIAN_POINT('Ctrl Pts',(17.2144982268397,-17.4779495618229,-18.1891429143673));
#79949=CARTESIAN_POINT('Ctrl Pts',(17.2112858742483,-17.4812682014599,-18.1888651196395));
#79950=CARTESIAN_POINT('Ctrl Pts',(17.2056059778469,-17.4871745843698,-18.1883707584947));
#79951=CARTESIAN_POINT('Ctrl Pts',(17.2031341027769,-17.4897580946576,-18.188154533796));
#79952=CARTESIAN_POINT('Ctrl Pts',(17.1978517445306,-17.4953070915276,-18.1876901273039));
#79953=CARTESIAN_POINT('Ctrl Pts',(17.1950433396807,-17.4982744105637,-18.1874417990732));
#79954=CARTESIAN_POINT('Ctrl Pts',(17.1892976820677,-17.504380495982,-18.1869308558748));
#79955=CARTESIAN_POINT('Ctrl Pts',(17.1863613664049,-17.5075201148841,-18.1866681727624));
#79956=CARTESIAN_POINT('Ctrl Pts',(17.1729077089025,-17.5219933826711,-18.185457478628));
#79957=CARTESIAN_POINT('Ctrl Pts',(17.1625054854867,-17.5334327559568,-18.1845012563713));
#79958=CARTESIAN_POINT('Ctrl Pts',(17.0941974976145,-17.6102247657089,-18.1780928140918));
#79959=CARTESIAN_POINT('Ctrl Pts',(17.0402626620495,-17.6789863629095,-18.1724082029247));
#79960=CARTESIAN_POINT('Ctrl Pts',(16.9494514377864,-17.8107861005604,-18.1618725522541));
#79961=CARTESIAN_POINT('Ctrl Pts',(16.9112865552785,-17.8727879806763,-18.157046709732));
#79962=CARTESIAN_POINT('Ctrl Pts',(16.87410699438,-17.9408078058736,-18.1519487847017));
#79963=CARTESIAN_POINT('Ctrl Pts',(16.8718386494663,-17.9449911864191,-18.151636005868));
#79964=CARTESIAN_POINT('Ctrl Pts',(16.8058494279297,-18.0676768142243,-18.1424856031553));
#79965=CARTESIAN_POINT('Ctrl Pts',(16.7535466437575,-18.1919945354638,-18.1338552605409));
#79966=CARTESIAN_POINT('Ctrl Pts',(16.7086937510272,-18.3355002086818,-18.1246738660042));
#79967=CARTESIAN_POINT('Ctrl Pts',(16.7041601067162,-18.3505954576644,-18.1237169459198));
#79968=CARTESIAN_POINT('Ctrl Pts',(16.6975600327991,-18.373496400646,-18.1222782755559));
#79969=CARTESIAN_POINT('Ctrl Pts',(16.6953690585521,-18.381265348987,-18.1217924773275));
#79970=CARTESIAN_POINT('Ctrl Pts',(16.691524469894,-18.3952024733846,-18.1209249582957));
#79971=CARTESIAN_POINT('Ctrl Pts',(16.6898542383013,-18.4013659263714,-18.1205427012609));
#79972=CARTESIAN_POINT('Ctrl Pts',(16.6863713131255,-18.4144528128727,-18.119733955102));
#79973=CARTESIAN_POINT('Ctrl Pts',(16.6845657850165,-18.4213780836742,-18.1193077023673));
#79974=CARTESIAN_POINT('Ctrl Pts',(16.6809624106011,-18.4354919538744,-18.1184424202491));
#79975=CARTESIAN_POINT('Ctrl Pts',(16.6791671181644,-18.4426811067311,-18.1180034781013));
#79976=CARTESIAN_POINT('Ctrl Pts',(16.6747876919857,-18.4606184102313,-18.1169126994108));
#79977=CARTESIAN_POINT('Ctrl Pts',(16.6722499088619,-18.4713777316691,-18.1162623476298));
#79978=CARTESIAN_POINT('Ctrl Pts',(16.6345655716992,-18.6369395762027,-18.1063131404208));
#79979=CARTESIAN_POINT('Ctrl Pts',(16.6168549652036,-18.7951908614192,-18.0976369962091));
#79980=CARTESIAN_POINT('Ctrl Pts',(16.6170008943745,-18.9539459653064,-18.0890147266704));
#79981=CARTESIAN_POINT('Ctrl Pts',(16.6170008942677,-18.9539458490376,-18.0890147329851));
#79982=CARTESIAN_POINT('Ctrl Pts',(16.617132245813,-19.0968506163556,-18.0812533231527));
#79983=CARTESIAN_POINT('Ctrl Pts',(16.6317330753476,-19.2393602546854,-18.0735574166762));
#79984=CARTESIAN_POINT('Ctrl Pts',(16.6625404198842,-19.3888517284755,-18.0645862748028));
#79985=CARTESIAN_POINT('Ctrl Pts',(16.6645760527504,-19.3983952772006,-18.0640094873609));
#79986=CARTESIAN_POINT('Ctrl Pts',(16.6678828636037,-19.4133895330032,-18.0630963762149));
#79987=CARTESIAN_POINT('Ctrl Pts',(16.669109829536,-19.4188499810754,-18.0627624050525));
#79988=CARTESIAN_POINT('Ctrl Pts',(16.6714750735612,-19.4291844290826,-18.0621274827003));
#79989=CARTESIAN_POINT('Ctrl Pts',(16.6726090155973,-19.4340593944653,-18.061826773435));
#79990=CARTESIAN_POINT('Ctrl Pts',(16.6745952714028,-19.4424633975876,-18.0613062272276));
#79991=CARTESIAN_POINT('Ctrl Pts',(16.6754394037885,-19.4459943847055,-18.0610868599088));
#79992=CARTESIAN_POINT('Ctrl Pts',(16.6770955964153,-19.4528442359433,-18.0606600010243));
#79993=CARTESIAN_POINT('Ctrl Pts',(16.6779066098708,-19.456163311683,-18.0604525759641));
#79994=CARTESIAN_POINT('Ctrl Pts',(16.6801205638094,-19.4651297326649,-18.0598906479025));
#79995=CARTESIAN_POINT('Ctrl Pts',(16.681538747412,-19.4707732315171,-18.0595352792088));
#79996=CARTESIAN_POINT('Ctrl Pts',(16.6869136685068,-19.4917950548166,-18.0582054256839));
#79997=CARTESIAN_POINT('Ctrl Pts',(16.691020011754,-19.5071341126097,-18.0572228373783));
#79998=CARTESIAN_POINT('Ctrl Pts',(16.7100014012788,-19.574973688845,-18.0528271902886));
#79999=CARTESIAN_POINT('Ctrl Pts',(16.7267229156432,-19.626906712487,-18.0493291599082));
#80000=CARTESIAN_POINT('Ctrl Pts',(16.7454193872878,-19.6781102855251,-18.0457833417799));
#80001=CARTESIAN_POINT('Origin',(18.734,-18.952,0.));
#80002=CARTESIAN_POINT('',(16.7454194498739,-19.6781104569281,-17.2426989690604));
#80003=CARTESIAN_POINT('',(16.745419450228,-19.6781104578977,-17.467776498566));
#80004=CARTESIAN_POINT('',(16.7454194499637,-19.6781104571739,0.));
#80005=CARTESIAN_POINT('Ctrl Pts',(16.745419450228,-19.6781104578977,-17.467776498566));
#80006=CARTESIAN_POINT('Ctrl Pts',(16.7278145373555,-19.6298963233431,-17.4710694417504));
#80007=CARTESIAN_POINT('Ctrl Pts',(16.7119674247689,-19.5810538475648,-17.4743159728977));
#80008=CARTESIAN_POINT('Ctrl Pts',(16.6884846842029,-19.4985720493969,-17.479647127548));
#80009=CARTESIAN_POINT('Ctrl Pts',(16.6798675447131,-19.4652387232586,-17.4817614672596));
#80010=CARTESIAN_POINT('Ctrl Pts',(16.669614458812,-19.421167833389,-17.484506134469));
#80011=CARTESIAN_POINT('Ctrl Pts',(16.6672430096864,-19.4106084041471,-17.4851599772679));
#80012=CARTESIAN_POINT('Ctrl Pts',(16.6634921056292,-19.3932863961265,-17.4862264942702));
#80013=CARTESIAN_POINT('Ctrl Pts',(16.6620645843557,-19.3865345316673,-17.4866407035569));
#80014=CARTESIAN_POINT('Ctrl Pts',(16.6593656416203,-19.3734533816376,-17.4874403333963));
#80015=CARTESIAN_POINT('Ctrl Pts',(16.6580901071281,-19.3671250317248,-17.4878258815601));
#80016=CARTESIAN_POINT('Ctrl Pts',(16.65521237201,-19.3525026263704,-17.4887137982358));
#80017=CARTESIAN_POINT('Ctrl Pts',(16.6536308201122,-19.3442045825099,-17.4892155031073));
#80018=CARTESIAN_POINT('Ctrl Pts',(16.649512270004,-19.3218694008198,-17.4905601871931));
#80019=CARTESIAN_POINT('Ctrl Pts',(16.6470673784447,-19.3078155675167,-17.4914002383051));
#80020=CARTESIAN_POINT('Ctrl Pts',(16.626190687621,-19.1801846309213,-17.4989769015963));
#80021=CARTESIAN_POINT('Ctrl Pts',(16.6169037092795,-19.065299216771,-17.5054071035181));
#80022=CARTESIAN_POINT('Ctrl Pts',(16.6171578062868,-18.7639639400357,-17.5219135265107));
#80023=CARTESIAN_POINT('Ctrl Pts',(16.6418924521979,-18.578581011756,-17.5316811112538));
#80024=CARTESIAN_POINT('Ctrl Pts',(16.694256245899,-18.3851344243615,-17.5434580684037));
#80025=CARTESIAN_POINT('Ctrl Pts',(16.6981093688863,-18.3714481272867,-17.5443004579815));
#80026=CARTESIAN_POINT('Ctrl Pts',(16.7036607297581,-18.3524648719532,-17.5454829971989));
#80027=CARTESIAN_POINT('Ctrl Pts',(16.7052425223522,-18.347133884778,-17.5458166422803));
#80028=CARTESIAN_POINT('Ctrl Pts',(16.7078156428536,-18.3385855522126,-17.5463542432883));
#80029=CARTESIAN_POINT('Ctrl Pts',(16.7087936868813,-18.3353641894629,-17.5465574266642));
#80030=CARTESIAN_POINT('Ctrl Pts',(16.7108530776938,-18.3286389672065,-17.5469828783114));
#80031=CARTESIAN_POINT('Ctrl Pts',(16.7119358447885,-18.3251355825079,-17.5472052320709));
#80032=CARTESIAN_POINT('Ctrl Pts',(16.7145777280571,-18.3166656110929,-17.5477445271499));
#80033=CARTESIAN_POINT('Ctrl Pts',(16.716146066486,-18.3117019445417,-17.5480620046195));
#80034=CARTESIAN_POINT('Ctrl Pts',(16.7216994320505,-18.294349029513,-17.5491768005403));
#80035=CARTESIAN_POINT('Ctrl Pts',(16.7257802907857,-18.2819910784939,-17.5499794650986));
#80036=CARTESIAN_POINT('Ctrl Pts',(16.7505712486492,-18.209179030544,-17.5547573500665));
#80037=CARTESIAN_POINT('Ctrl Pts',(16.7738944055408,-18.1496552434907,-17.5588615632688));
#80038=CARTESIAN_POINT('Ctrl Pts',(16.8760922808093,-17.9200048733331,-17.5752528705611));
#80039=CARTESIAN_POINT('Ctrl Pts',(16.9747462057869,-17.7595736626754,-17.5878515521336));
#80040=CARTESIAN_POINT('Ctrl Pts',(17.128654570568,-17.5708067306473,-17.6032548870418));
#80041=CARTESIAN_POINT('Ctrl Pts',(17.1657757998303,-17.528798475539,-17.6067354248861));
#80042=CARTESIAN_POINT('Ctrl Pts',(17.2128425128144,-17.4796163269227,-17.6108793336885));
#80043=CARTESIAN_POINT('Ctrl Pts',(17.2212358738615,-17.4709940953485,-17.611608568766));
#80044=CARTESIAN_POINT('Ctrl Pts',(17.2352366791693,-17.4568547317422,-17.6128091676919));
#80045=CARTESIAN_POINT('Ctrl Pts',(17.2408020912742,-17.451296540604,-17.6132823608392));
#80046=CARTESIAN_POINT('Ctrl Pts',(17.2509287698957,-17.4412951081666,-17.6141361329356));
#80047=CARTESIAN_POINT('Ctrl Pts',(17.2554793306571,-17.4368412045365,-17.61451718038));
#80048=CARTESIAN_POINT('Ctrl Pts',(17.2652853707379,-17.4273296962544,-17.6153327738553));
#80049=CARTESIAN_POINT('Ctrl Pts',(17.2705470436209,-17.4222785731252,-17.6157670343438));
#80050=CARTESIAN_POINT('Ctrl Pts',(17.2849677572284,-17.4085774181892,-17.6169481634482));
#80051=CARTESIAN_POINT('Ctrl Pts',(17.2941781651148,-17.3999817008966,-17.6176926871672));
#80052=CARTESIAN_POINT('Ctrl Pts',(17.343313531804,-17.354939438352,-17.6216137829902));
#80053=CARTESIAN_POINT('Ctrl Pts',(17.3845488252999,-17.3199480580817,-17.6247285100711));
#80054=CARTESIAN_POINT('Ctrl Pts',(17.5775455933136,-17.1684969047962,-17.6386249859452));
#80055=CARTESIAN_POINT('Ctrl Pts',(17.7433014241674,-17.0713669327261,-17.6486491865709));
#80056=CARTESIAN_POINT('Ctrl Pts',(17.9351116018922,-16.9914541473783,-17.6602002585299));
#80057=CARTESIAN_POINT('Ctrl Pts',(17.9504572506331,-16.9852708745889,-17.6611247414616));
#80058=CARTESIAN_POINT('Ctrl Pts',(18.0154371536849,-16.959969520619,-17.6650468852495));
#80059=CARTESIAN_POINT('Ctrl Pts',(18.0657061740732,-16.9425472520998,-17.668099243892));
#80060=CARTESIAN_POINT('Ctrl Pts',(18.1249048980915,-16.9244970945919,-17.6717720142836));
#80061=CARTESIAN_POINT('Ctrl Pts',(18.1332522419629,-16.9220081281144,-17.6722916800794));
#80062=CARTESIAN_POINT('Ctrl Pts',(18.145916687653,-16.9183168637882,-17.6730831390944));
#80063=CARTESIAN_POINT('Ctrl Pts',(18.1502227551509,-16.9170766087342,-17.6733527736882));
#80064=CARTESIAN_POINT('Ctrl Pts',(18.1579604175239,-16.9148745496692,-17.6738382878472));
#80065=CARTESIAN_POINT('Ctrl Pts',(18.1613905293181,-16.913907731541,-17.6740538720244));
#80066=CARTESIAN_POINT('Ctrl Pts',(18.1688506107295,-16.9118253377499,-17.6745235251855));
#80067=CARTESIAN_POINT('Ctrl Pts',(18.1728813964128,-16.9107130538088,-17.6747777760013));
#80068=CARTESIAN_POINT('Ctrl Pts',(18.184216700423,-16.9076212194275,-17.6754941009582));
#80069=CARTESIAN_POINT('Ctrl Pts',(18.191528491049,-16.9056689092541,-17.6759577071562));
#80070=CARTESIAN_POINT('Ctrl Pts',(18.235382845567,-16.8942109794016,-17.6787468819658));
#80071=CARTESIAN_POINT('Ctrl Pts',(18.2721615201621,-16.8856458361256,-17.6811215559806));
#80072=CARTESIAN_POINT('Ctrl Pts',(18.3941300914431,-16.8606600724104,-17.6890699536874));
#80073=CARTESIAN_POINT('Ctrl Pts',(18.4800978884145,-16.848491964533,-17.6947857651894));
#80074=CARTESIAN_POINT('Ctrl Pts',(18.7418263909396,-16.8277264202923,-17.7121324653516));
#80075=CARTESIAN_POINT('Ctrl Pts',(18.9181758879456,-16.8357055199715,-17.7236768034007));
#80076=CARTESIAN_POINT('Ctrl Pts',(19.1141647727758,-16.8692875610003,-17.7359157672763));
#80077=CARTESIAN_POINT('Ctrl Pts',(19.1367352434748,-16.8735340400004,-17.7373176331889));
#80078=CARTESIAN_POINT('Ctrl Pts',(19.1685801250482,-16.8800636690634,-17.7392854451132));
#80079=CARTESIAN_POINT('Ctrl Pts',(19.1779144317484,-16.8820434723188,-17.7398610149612));
#80080=CARTESIAN_POINT('Ctrl Pts',(19.1930628252236,-16.8853636227724,-17.7407931707343));
#80081=CARTESIAN_POINT('Ctrl Pts',(19.1988851156082,-16.8866655419519,-17.7411509825978));
#80082=CARTESIAN_POINT('Ctrl Pts',(19.2110637386624,-16.8894429056283,-17.741898486785));
#80083=CARTESIAN_POINT('Ctrl Pts',(19.2174189182583,-16.890923162706,-17.7422880201902));
#80084=CARTESIAN_POINT('Ctrl Pts',(19.232526468667,-16.8945157537857,-17.7432127893382));
#80085=CARTESIAN_POINT('Ctrl Pts',(19.241272453318,-16.8966545970809,-17.7437471659618));
#80086=CARTESIAN_POINT('Ctrl Pts',(19.2707150346374,-16.9040542037183,-17.7455429722428));
#80087=CARTESIAN_POINT('Ctrl Pts',(19.2913460269346,-16.9095724080665,-17.7467960910483));
#80088=CARTESIAN_POINT('Ctrl Pts',(19.403356258191,-16.9413556345067,-17.7535761794883));
#80089=CARTESIAN_POINT('Ctrl Pts',(19.4929752629715,-16.9734429080522,-17.7589088427267));
#80090=CARTESIAN_POINT('Ctrl Pts',(19.7363115714171,-17.079545364619,-17.7735134467975));
#80091=CARTESIAN_POINT('Ctrl Pts',(19.8836711959582,-17.1662343191764,-17.7824759839761));
#80092=CARTESIAN_POINT('Ctrl Pts',(20.048552498187,-17.2921746194202,-17.794322069814));
#80093=CARTESIAN_POINT('Ctrl Pts',(20.0774690342639,-17.3154917838281,-17.7964789767863));
#80094=CARTESIAN_POINT('Ctrl Pts',(20.1112115357397,-17.3441975548522,-17.7991126283722));
#80095=CARTESIAN_POINT('Ctrl Pts',(20.1166440942714,-17.3488669356307,-17.7995403718011));
#80096=CARTESIAN_POINT('Ctrl Pts',(20.1254647929601,-17.3565266686795,-17.8002411863204));
#80097=CARTESIAN_POINT('Ctrl Pts',(20.1288672920435,-17.359500499931,-17.8005130626462));
#80098=CARTESIAN_POINT('Ctrl Pts',(20.1349380775842,-17.3648408325228,-17.8010009730552));
#80099=CARTESIAN_POINT('Ctrl Pts',(20.1376099281236,-17.3672032024468,-17.8012166989892));
#80100=CARTESIAN_POINT('Ctrl Pts',(20.1433802634822,-17.372331198733,-17.8016847555476));
#80101=CARTESIAN_POINT('Ctrl Pts',(20.1464765407044,-17.3750991565526,-17.8019372576699));
#80102=CARTESIAN_POINT('Ctrl Pts',(20.1550952620772,-17.382849726684,-17.8026438425883));
#80103=CARTESIAN_POINT('Ctrl Pts',(20.1605995582269,-17.3878523021026,-17.8030993926092));
#80104=CARTESIAN_POINT('Ctrl Pts',(20.1922720582496,-17.4169440815917,-17.8057450338897));
#80105=CARTESIAN_POINT('Ctrl Pts',(20.2178545770922,-17.4416592049688,-17.8079786492476));
#80106=CARTESIAN_POINT('Ctrl Pts',(20.2978229168524,-17.5229095085538,-17.8152428688612));
#80107=CARTESIAN_POINT('Ctrl Pts',(20.3496920383832,-17.5818250753066,-17.8203916877443));
#80108=CARTESIAN_POINT('Ctrl Pts',(20.5144698303587,-17.7913882872951,-17.8379874255252));
#80109=CARTESIAN_POINT('Ctrl Pts',(20.6105594130797,-17.9541794143467,-17.8503964698286));
#80110=CARTESIAN_POINT('Ctrl Pts',(20.6923693512098,-18.1476646945847,-17.8633118362426));
#80111=CARTESIAN_POINT('Ctrl Pts',(20.7005616519169,-18.1679074515319,-17.864643826459));
#80112=CARTESIAN_POINT('Ctrl Pts',(20.711475681688,-18.196123186614,-17.8664745615214));
#80113=CARTESIAN_POINT('Ctrl Pts',(20.7144650189755,-18.2039905478562,-17.8669822677787));
#80114=CARTESIAN_POINT('Ctrl Pts',(20.7195283612208,-18.2175594434026,-17.867853241419));
#80115=CARTESIAN_POINT('Ctrl Pts',(20.7216249019649,-18.2232524067499,-17.8682172598299));
#80116=CARTESIAN_POINT('Ctrl Pts',(20.7259016343792,-18.2350212369487,-17.8689669111436));
#80117=CARTESIAN_POINT('Ctrl Pts',(20.7280785686044,-18.2410982266401,-17.8693524322109));
#80118=CARTESIAN_POINT('Ctrl Pts',(20.7330881853936,-18.2552868259416,-17.8702489391956));
#80119=CARTESIAN_POINT('Ctrl Pts',(20.7358993622759,-18.263405949397,-17.870759206552));
#80120=CARTESIAN_POINT('Ctrl Pts',(20.7447721193394,-18.2895455084089,-17.8723933985687));
#80121=CARTESIAN_POINT('Ctrl Pts',(20.7506405097874,-18.3076308833396,-17.8735109456384));
#80122=CARTESIAN_POINT('Ctrl Pts',(20.7789096093923,-18.3989227851026,-17.8790898709617));
#80123=CARTESIAN_POINT('Ctrl Pts',(20.7975726116513,-18.4732311752088,-17.8834281140622));
#80124=CARTESIAN_POINT('Ctrl Pts',(20.8331227192317,-18.656278848617,-17.8937908286963));
#80125=CARTESIAN_POINT('Ctrl Pts',(20.8456426825138,-18.7656315762455,-17.8997059276357));
#80126=CARTESIAN_POINT('Ctrl Pts',(20.8521618575798,-18.945835922279,-17.909526728321));
#80127=CARTESIAN_POINT('Ctrl Pts',(20.8511947689397,-19.0162867885636,-17.9133874850769));
#80128=CARTESIAN_POINT('Ctrl Pts',(20.843675002066,-19.1343596947872,-17.9200725876549));
#80129=CARTESIAN_POINT('Ctrl Pts',(20.8390088837037,-19.1820445862877,-17.922832093884));
#80130=CARTESIAN_POINT('Ctrl Pts',(20.831716743104,-19.2371898066608,-17.9261346949096));
#80131=CARTESIAN_POINT('Ctrl Pts',(20.8306613725614,-19.2448478185067,-17.9265958377179));
#80132=CARTESIAN_POINT('Ctrl Pts',(20.8289055491562,-19.257092223195,-17.9273374258822));
#80133=CARTESIAN_POINT('Ctrl Pts',(20.8282319091574,-19.2616824732989,-17.927616397696));
#80134=CARTESIAN_POINT('Ctrl Pts',(20.8270106633001,-19.2698179221795,-17.9281125924166));
#80135=CARTESIAN_POINT('Ctrl Pts',(20.8264691291266,-19.2733639865203,-17.9283294695038));
#80136=CARTESIAN_POINT('Ctrl Pts',(20.8253005432132,-19.2808879047706,-17.9287909196289));
#80137=CARTESIAN_POINT('Ctrl Pts',(20.8246711637287,-19.2848652887816,-17.9290356167509));
#80138=CARTESIAN_POINT('Ctrl Pts',(20.8229381171665,-19.295618498979,-17.9296991881539));
#80139=CARTESIAN_POINT('Ctrl Pts',(20.8218128431955,-19.302390723329,-17.9301192582767));
#80140=CARTESIAN_POINT('Ctrl Pts',(20.8160132847415,-19.3362740501696,-17.9322314104331));
#80141=CARTESIAN_POINT('Ctrl Pts',(20.8108440047118,-19.363296336031,-17.9339493125006));
#80142=CARTESIAN_POINT('Ctrl Pts',(20.7942858840615,-19.4415566561962,-17.9390072848292));
#80143=CARTESIAN_POINT('Ctrl Pts',(20.7815167274972,-19.4924795555058,-17.9424020358221));
#80144=CARTESIAN_POINT('Ctrl Pts',(20.7277878889936,-19.6773314205922,-17.9549904834507));
#80145=CARTESIAN_POINT('Ctrl Pts',(20.6754578583809,-19.8075943668165,-17.9643539487579));
#80146=CARTESIAN_POINT('Ctrl Pts',(20.5673798944559,-20.0146138090563,-17.9794560317214));
#80147=CARTESIAN_POINT('Ctrl Pts',(20.5186649396223,-20.0945432683055,-17.9853563567417));
#80148=CARTESIAN_POINT('Ctrl Pts',(20.4568674936831,-20.1822874562478,-17.991905285481));
#80149=CARTESIAN_POINT('Ctrl Pts',(20.4488069964224,-20.1934977265337,-17.9927435596222));
#80150=CARTESIAN_POINT('Ctrl Pts',(20.435717997427,-20.2113307651203,-17.994079817909));
#80151=CARTESIAN_POINT('Ctrl Pts',(20.4307592501047,-20.2180040161901,-17.9945804831779));
#80152=CARTESIAN_POINT('Ctrl Pts',(20.421893141664,-20.229789945465,-17.9954659117261));
#80153=CARTESIAN_POINT('Ctrl Pts',(20.4180015635411,-20.2349143142924,-17.9958512852074));
#80154=CARTESIAN_POINT('Ctrl Pts',(20.4098529272256,-20.245543346032,-17.9966515072384));
#80155=CARTESIAN_POINT('Ctrl Pts',(20.4055919646096,-20.251044928932,-17.9970661954092));
#80156=CARTESIAN_POINT('Ctrl Pts',(20.394474131314,-20.2652545458578,-17.9981386135188));
#80157=CARTESIAN_POINT('Ctrl Pts',(20.3875758074244,-20.2739299902588,-17.9987946873923));
#80158=CARTESIAN_POINT('Ctrl Pts',(20.3574947852159,-20.31115644722,-18.0016161870161));
#80159=CARTESIAN_POINT('Ctrl Pts',(20.3336375784294,-20.3391558758331,-18.0037542983399));
#80160=CARTESIAN_POINT('Ctrl Pts',(20.2685087528343,-20.4116764973964,-18.0093503088328));
#80161=CARTESIAN_POINT('Ctrl Pts',(20.2260306807968,-20.4550694791138,-18.0127591017667));
#80162=CARTESIAN_POINT('Ctrl Pts',(20.0631393871247,-20.6077484814625,-18.0251198802547));
#80163=CARTESIAN_POINT('Ctrl Pts',(19.9321358206603,-20.7048772656731,-18.0336927930378));
#80164=CARTESIAN_POINT('Ctrl Pts',(19.7414663596128,-20.8147968027434,-18.0460280754051));
#80165=CARTESIAN_POINT('Ctrl Pts',(19.6904661444035,-20.8414897878346,-18.0493202579872));
#80166=CARTESIAN_POINT('Ctrl Pts',(19.6304186964888,-20.8698637522312,-18.0532601877973));
#80167=CARTESIAN_POINT('Ctrl Pts',(19.6223664241616,-20.8736068645068,-18.0537898204125));
#80168=CARTESIAN_POINT('Ctrl Pts',(19.6101826138716,-20.8791775825208,-18.0545934997434));
#80169=CARTESIAN_POINT('Ctrl Pts',(19.6060682677586,-20.8810428566834,-18.0548652869437));
#80170=CARTESIAN_POINT('Ctrl Pts',(19.5986951356964,-20.8843571206202,-18.0553531015523));
#80171=CARTESIAN_POINT('Ctrl Pts',(19.5954386311095,-20.8858110569209,-18.0555688213183));
#80172=CARTESIAN_POINT('Ctrl Pts',(19.5883808065901,-20.8889408083918,-18.0560369389422));
#80173=CARTESIAN_POINT('Ctrl Pts',(19.5845782755089,-20.8906136423822,-18.0562895086996));
#80174=CARTESIAN_POINT('Ctrl Pts',(19.5739491837222,-20.8952523684646,-18.0569964695375));
#80175=CARTESIAN_POINT('Ctrl Pts',(19.5671119469399,-20.8981934330538,-18.0574523303214));
#80176=CARTESIAN_POINT('Ctrl Pts',(19.5274374274844,-20.915012208453,-18.0601033296458));
#80177=CARTESIAN_POINT('Ctrl Pts',(19.4942713519237,-20.9280938757247,-18.0623421943833));
#80178=CARTESIAN_POINT('Ctrl Pts',(19.3868409024943,-20.9673628503226,-18.0696311619156));
#80179=CARTESIAN_POINT('Ctrl Pts',(19.3114428514005,-20.9902459971906,-18.0748003112139));
#80180=CARTESIAN_POINT('Ctrl Pts',(19.0525855787614,-21.0532906141568,-18.0923861963261));
#80181=CARTESIAN_POINT('Ctrl Pts',(18.8650793089506,-21.073265143475,-18.1047628427769));
#80182=CARTESIAN_POINT('Ctrl Pts',(18.6554961582511,-21.0676571365953,-18.1176535355759));
#80183=CARTESIAN_POINT('Ctrl Pts',(18.6336283222385,-21.0667325021242,-18.1189886028542));
#80184=CARTESIAN_POINT('Ctrl Pts',(18.6033682105101,-21.0649825598461,-18.1208228563401));
#80185=CARTESIAN_POINT('Ctrl Pts',(18.5949612134311,-21.0644460186423,-18.1213310488727));
#80186=CARTESIAN_POINT('Ctrl Pts',(18.5805035304397,-21.063436634994,-18.1222026350934));
#80187=CARTESIAN_POINT('Ctrl Pts',(18.5744513113502,-21.0629879314921,-18.122566782213));
#80188=CARTESIAN_POINT('Ctrl Pts',(18.5619669217578,-21.062008358501,-18.1233164963825));
#80189=CARTESIAN_POINT('Ctrl Pts',(18.5555350756361,-21.0614740873377,-18.1237019524874));
#80190=CARTESIAN_POINT('Ctrl Pts',(18.5405539541994,-21.0601606490404,-18.1245979655291));
#80191=CARTESIAN_POINT('Ctrl Pts',(18.5320067359999,-21.0593588729516,-18.125107806354));
#80192=CARTESIAN_POINT('Ctrl Pts',(18.5045860860872,-21.0566183055288,-18.1267392318985));
#80193=CARTESIAN_POINT('Ctrl Pts',(18.4857334213134,-21.05447775171,-18.1278544697676));
#80194=CARTESIAN_POINT('Ctrl Pts',(18.3912626732096,-21.0424629752717,-18.1334139694499));
#80195=CARTESIAN_POINT('Ctrl Pts',(18.3161842460222,-21.0287609633748,-18.1377360970775));
#80196=CARTESIAN_POINT('Ctrl Pts',(18.0773748424344,-20.9716985198246,-18.1513837359916));
#80197=CARTESIAN_POINT('Ctrl Pts',(17.9180734980709,-20.9127641214443,-18.1602911163621));
#80198=CARTESIAN_POINT('Ctrl Pts',(17.7613194130465,-20.832327021385,-18.1701569555515));
#80199=CARTESIAN_POINT('Ctrl Pts',(17.7551562201155,-20.8291260172312,-18.1705468248623));
#80200=CARTESIAN_POINT('Ctrl Pts',(17.7028138526511,-20.8016128586891,-18.1738755930327));
#80201=CARTESIAN_POINT('Ctrl Pts',(17.6575364368848,-20.7756331414273,-18.1768726740398));
#80202=CARTESIAN_POINT('Ctrl Pts',(17.6059737175145,-20.7434574106965,-18.18047977821));
#80203=CARTESIAN_POINT('Ctrl Pts',(17.5987062147721,-20.7388606447802,-18.1809928107255));
#80204=CARTESIAN_POINT('Ctrl Pts',(17.5877557857993,-20.7318406208264,-18.1817731799165));
#80205=CARTESIAN_POINT('Ctrl Pts',(17.5840519913075,-20.7294498616357,-18.182038408293));
#80206=CARTESIAN_POINT('Ctrl Pts',(17.5775081618246,-20.7251968762569,-18.1825093356745));
#80207=CARTESIAN_POINT('Ctrl Pts',(17.5746651128291,-20.7233393669585,-18.1827147185618));
#80208=CARTESIAN_POINT('Ctrl Pts',(17.5718041261608,-20.7214602995117,-18.1829221940531));
#80209=CARTESIAN_POINT('Ctrl Pts',(17.5717817453369,-20.7214455994025,-18.182923817134));
#80210=CARTESIAN_POINT('Ctrl Pts',(17.5717374603198,-20.7214165110405,-18.1829270288269));
#80211=CARTESIAN_POINT('Ctrl Pts',(17.5717155564107,-20.7214021230001,-18.1829286174163));
#80212=CARTESIAN_POINT('Ctrl Pts',(17.5716721963381,-20.7213736398775,-18.1829317622151));
#80213=CARTESIAN_POINT('Ctrl Pts',(17.5716507400462,-20.7213595447347,-18.1829333184319));
#80214=CARTESIAN_POINT('Ctrl Pts',(17.5716082477229,-20.7213316294216,-18.1829364004733));
#80215=CARTESIAN_POINT('Ctrl Pts',(17.5715872117662,-20.721317809322,-18.1829379262908));
#80216=CARTESIAN_POINT('Ctrl Pts',(17.5715455349472,-20.721290427626,-18.1829409493539));
#80217=CARTESIAN_POINT('Ctrl Pts',(17.5715248941418,-20.7212768660868,-18.1829424465938));
#80218=CARTESIAN_POINT('Ctrl Pts',(17.5714839844136,-20.72124998632,-18.1829454141805));
#80219=CARTESIAN_POINT('Ctrl Pts',(17.5714637154324,-20.7212366680724,-18.1829468845301));
#80220=CARTESIAN_POINT('Ctrl Pts',(17.5714235280464,-20.7212102609435,-18.1829497998776));
#80221=CARTESIAN_POINT('Ctrl Pts',(17.5714036093988,-20.7211971719198,-18.1829512448917));
#80222=CARTESIAN_POINT('Ctrl Pts',(17.5713641022553,-20.7211712098677,-18.1829541110458));
#80223=CARTESIAN_POINT('Ctrl Pts',(17.571344513777,-20.7211583368667,-18.1829555321832));
#80224=CARTESIAN_POINT('Ctrl Pts',(17.5713056478953,-20.7211327943702,-18.1829583519641));
#80225=CARTESIAN_POINT('Ctrl Pts',(17.5712863706823,-20.7211201250144,-18.1829597505926));
#80226=CARTESIAN_POINT('Ctrl Pts',(17.5712481100679,-20.7210949785061,-18.1829625266047));
#80227=CARTESIAN_POINT('Ctrl Pts',(17.5712291266373,-20.7210825013479,-18.1829639039894));
#80228=CARTESIAN_POINT('Ctrl Pts',(17.5711914372614,-20.7210577285445,-18.1829666386951));
#80229=CARTESIAN_POINT('Ctrl Pts',(17.5711727312304,-20.7210454328555,-18.1829679960213));
#80230=CARTESIAN_POINT('Ctrl Pts',(17.5711355812659,-20.7210210129135,-18.1829706917238));
#80231=CARTESIAN_POINT('Ctrl Pts',(17.5711171372815,-20.7210088886387,-18.1829720301027));
#80232=CARTESIAN_POINT('Ctrl Pts',(17.571080496686,-20.720984801881,-18.1829746889762));
#80233=CARTESIAN_POINT('Ctrl Pts',(17.5710623001659,-20.7209728394689,-18.1829760094633));
#80234=CARTESIAN_POINT('Ctrl Pts',(17.5710261413792,-20.7209490678442,-18.1829786335024));
#80235=CARTESIAN_POINT('Ctrl Pts',(17.5710081789585,-20.7209372585405,-18.1829799370648));
#80236=CARTESIAN_POINT('Ctrl Pts',(17.5709724748682,-20.7209137842859,-18.1829825282321));
#80237=CARTESIAN_POINT('Ctrl Pts',(17.5709547334959,-20.72090211954,-18.1829838158146));
#80238=CARTESIAN_POINT('Ctrl Pts',(17.5709194597347,-20.7208789266924,-18.1829863758739));
#80239=CARTESIAN_POINT('Ctrl Pts',(17.5709019273821,-20.7208673986234,-18.1829876483473));
#80240=CARTESIAN_POINT('Ctrl Pts',(17.5708670602951,-20.7208444716831,-18.182990179011));
#80241=CARTESIAN_POINT('Ctrl Pts',(17.5708497255287,-20.720833072799,-18.182991437203));
#80242=CARTESIAN_POINT('Ctrl Pts',(17.5708152429612,-20.7208103972483,-18.1829939400751));
#80243=CARTESIAN_POINT('Ctrl Pts',(17.5707980950534,-20.7207991205193,-18.1829951847623));
#80244=CARTESIAN_POINT('Ctrl Pts',(17.5707639756402,-20.7207766823554,-18.1829976613898));
#80245=CARTESIAN_POINT('Ctrl Pts',(17.570747004238,-20.7207655209957,-18.1829988933219));
#80246=CARTESIAN_POINT('Ctrl Pts',(17.5707132280953,-20.7207433071862,-18.1830013451445));
#80247=CARTESIAN_POINT('Ctrl Pts',(17.5706964233892,-20.7207322547658,-18.1830025650319));
#80248=CARTESIAN_POINT('Ctrl Pts',(17.5706629717341,-20.7207102529986,-18.1830049934098));
#80249=CARTESIAN_POINT('Ctrl Pts',(17.5706463245488,-20.7206993035027,-18.1830062019169));
#80250=CARTESIAN_POINT('Ctrl Pts',(17.5706131793865,-20.7206775019807,-18.1830086081533));
#80251=CARTESIAN_POINT('Ctrl Pts',(17.5705966811634,-20.7206666497986,-18.1830098059));
#80252=CARTESIAN_POINT('Ctrl Pts',(17.570563824197,-20.7206450365227,-18.1830121913202));
#80253=CARTESIAN_POINT('Ctrl Pts',(17.5705474659792,-20.72063427578,-18.1830133789553));
#80254=CARTESIAN_POINT('Ctrl Pts',(17.5705148823415,-20.7206128410041,-18.1830157446361));
#80255=CARTESIAN_POINT('Ctrl Pts',(17.570498656574,-20.7206021667472,-18.1830169227067));
#80256=CARTESIAN_POINT('Ctrl Pts',(17.5669733594806,-20.7182829510758,-18.1832728822284));
#80257=CARTESIAN_POINT('Ctrl Pts',(17.5634712015733,-20.7159639946129,-18.1835283658869));
#80258=CARTESIAN_POINT('Ctrl Pts',(17.5533745623766,-20.7092351892539,-18.1842683500758));
#80259=CARTESIAN_POINT('Ctrl Pts',(17.5467980218839,-20.7047987314328,-18.1847545907038));
#80260=CARTESIAN_POINT('Ctrl Pts',(17.5031777922752,-20.6750149220107,-18.1880072092336));
#80261=CARTESIAN_POINT('Ctrl Pts',(17.4669261534767,-20.6485338013872,-18.190843091036));
#80262=CARTESIAN_POINT('Ctrl Pts',(17.3376286846866,-20.5476280480046,-18.2013741625363));
#80263=CARTESIAN_POINT('Ctrl Pts',(17.2500690229898,-20.4665391393246,-18.2093154794288));
#80264=CARTESIAN_POINT('Ctrl Pts',(17.070835538936,-20.2700066449078,-18.2268361359592));
#80265=CARTESIAN_POINT('Ctrl Pts',(16.983418077119,-20.1514729917286,-18.2363012277721));
#80266=CARTESIAN_POINT('Ctrl Pts',(16.9017510066727,-20.0125448676335,-18.2461406433001));
#80267=CARTESIAN_POINT('Ctrl Pts',(16.8946583767629,-20.000195687072,-18.2470056080363));
#80268=CARTESIAN_POINT('Ctrl Pts',(16.8835611924874,-19.9804145364375,-18.2483760643911));
#80269=CARTESIAN_POINT('Ctrl Pts',(16.8794756432188,-19.9730287226287,-18.2488844585938));
#80270=CARTESIAN_POINT('Ctrl Pts',(16.8723439638226,-19.959952113074,-18.2497788294476));
#80271=CARTESIAN_POINT('Ctrl Pts',(16.8692795042379,-19.9542714868748,-18.2501654575796));
#80272=CARTESIAN_POINT('Ctrl Pts',(16.862991058598,-19.9424858426101,-18.2509637211513));
#80273=CARTESIAN_POINT('Ctrl Pts',(16.8597708575872,-19.9363788837048,-18.2513752187681));
#80274=CARTESIAN_POINT('Ctrl Pts',(16.8515737311609,-19.920647376848,-18.2524298207301));
#80275=CARTESIAN_POINT('Ctrl Pts',(16.846640677324,-19.9110001001063,-18.2530713728825));
#80276=CARTESIAN_POINT('Ctrl Pts',(16.8262952097781,-19.8704465919449,-18.2557470804528));
#80277=CARTESIAN_POINT('Ctrl Pts',(16.8115656643136,-19.8392024201524,-18.2577573662174));
#80278=CARTESIAN_POINT('Ctrl Pts',(16.778791499888,-19.7650288552953,-18.2624217793942));
#80279=CARTESIAN_POINT('Ctrl Pts',(16.7613864427332,-19.7218388607945,-18.2650549637422));
#80280=CARTESIAN_POINT('Ctrl Pts',(16.745419450845,-19.6781104595875,-18.2676549380821));
#80281=CARTESIAN_POINT('Ctrl Pts',(16.7454193872878,-19.6781102855251,-18.0457833417799));
#80282=CARTESIAN_POINT('Ctrl Pts',(16.7693936118093,-19.74376791225,-18.0412365887061));
#80283=CARTESIAN_POINT('Ctrl Pts',(16.7966152266407,-19.8082261759475,-18.0366121350535));
#80284=CARTESIAN_POINT('Ctrl Pts',(16.8578701043261,-19.9353018072534,-18.0272902389871));
#80285=CARTESIAN_POINT('Ctrl Pts',(16.8919573327061,-19.9977654881651,-18.0226009975555));
#80286=CARTESIAN_POINT('Ctrl Pts',(16.9780524348281,-20.1382131432663,-18.0118976631239));
#80287=CARTESIAN_POINT('Ctrl Pts',(17.0322252502904,-20.2147035228647,-18.0059486028066));
#80288=CARTESIAN_POINT('Ctrl Pts',(17.1052039057518,-20.3044787334957,-17.9988355474707));
#80289=CARTESIAN_POINT('Ctrl Pts',(17.1193830444339,-20.3213748886869,-17.9974902752154));
#80290=CARTESIAN_POINT('Ctrl Pts',(17.1384824928375,-20.3434249922963,-17.9957252654999));
#80291=CARTESIAN_POINT('Ctrl Pts',(17.1431680433609,-20.3487796220301,-17.9952959019302));
#80292=CARTESIAN_POINT('Ctrl Pts',(17.1524850363611,-20.3593193498321,-17.9944492379624));
#80293=CARTESIAN_POINT('Ctrl Pts',(17.1571151993546,-20.3645054548259,-17.9940318919085));
#80294=CARTESIAN_POINT('Ctrl Pts',(17.1660812176998,-20.3744489875953,-17.9932302181764));
#80295=CARTESIAN_POINT('Ctrl Pts',(17.1704133815653,-20.379209626602,-17.9928457417555));
#80296=CARTESIAN_POINT('Ctrl Pts',(17.1804002879802,-20.3900842427672,-17.9919659233094));
#80297=CARTESIAN_POINT('Ctrl Pts',(17.1860695534442,-20.3961847839294,-17.9914712059013));
#80298=CARTESIAN_POINT('Ctrl Pts',(17.201266138522,-20.4123451209219,-17.9901574964782));
#80299=CARTESIAN_POINT('Ctrl Pts',(17.2108565646309,-20.422345214983,-17.9893412226815));
#80300=CARTESIAN_POINT('Ctrl Pts',(17.2872013390473,-20.5004025426934,-17.9829410960019));
#80301=CARTESIAN_POINT('Ctrl Pts',(17.3583895325229,-20.5639788844936,-17.9775621476939));
#80302=CARTESIAN_POINT('Ctrl Pts',(17.5143262243304,-20.6853616863687,-17.9666495829469));
#80303=CARTESIAN_POINT('Ctrl Pts',(17.5994685176907,-20.7422473287287,-17.9611478091277));
#80304=CARTESIAN_POINT('Ctrl Pts',(17.7570931387863,-20.8317832892747,-17.9512617703116));
#80305=CARTESIAN_POINT('Ctrl Pts',(17.8279227704957,-20.8669293300417,-17.9469131895881));
#80306=CARTESIAN_POINT('Ctrl Pts',(17.9333381983799,-20.9120771349535,-17.9403514629299));
#80307=CARTESIAN_POINT('Ctrl Pts',(17.9664795984596,-20.9252900926776,-17.9382759520062));
#80308=CARTESIAN_POINT('Ctrl Pts',(18.0068870952703,-20.940228038729,-17.9357122556132));
#80309=CARTESIAN_POINT('Ctrl Pts',(18.0138508293981,-20.9427609295474,-17.9352692603445));
#80310=CARTESIAN_POINT('Ctrl Pts',(18.0247634647876,-20.9466653882889,-17.9345730132578));
#80311=CARTESIAN_POINT('Ctrl Pts',(18.0287034523018,-20.9480619362208,-17.934321219382));
#80312=CARTESIAN_POINT('Ctrl Pts',(18.0360102047989,-20.9506275159754,-17.9338534515313));
#80313=CARTESIAN_POINT('Ctrl Pts',(18.039375795226,-20.9517997188161,-17.933637668691));
#80314=CARTESIAN_POINT('Ctrl Pts',(18.0469814189056,-20.9544271683891,-17.9331493153539));
#80315=CARTESIAN_POINT('Ctrl Pts',(18.0512230996814,-20.9558774411146,-17.9328764568797));
#80316=CARTESIAN_POINT('Ctrl Pts',(18.0637275845528,-20.9601085370153,-17.9320706595235));
#80317=CARTESIAN_POINT('Ctrl Pts',(18.0720028802374,-20.9628517634983,-17.9315355850433));
#80318=CARTESIAN_POINT('Ctrl Pts',(18.1310095042004,-20.9820085073495,-17.9277086034642));
#80319=CARTESIAN_POINT('Ctrl Pts',(18.1823238144446,-20.9965499332094,-17.9243197205658));
#80320=CARTESIAN_POINT('Ctrl Pts',(18.2514714852123,-21.0133524250873,-17.9197208026075));
#80321=CARTESIAN_POINT('Ctrl Pts',(18.2688680759763,-21.0173473935484,-17.9185610543798));
#80322=CARTESIAN_POINT('Ctrl Pts',(18.4475858537301,-21.056015813411,-17.9066314229938));
#80323=CARTESIAN_POINT('Ctrl Pts',(18.6124100646995,-21.0719390599156,-17.8955614339438));
#80324=CARTESIAN_POINT('Ctrl Pts',(18.8531727896178,-21.0670009749237,-17.8801417825589));
#80325=CARTESIAN_POINT('Ctrl Pts',(18.9288029784438,-21.0613803171453,-17.8753960106413));
#80326=CARTESIAN_POINT('Ctrl Pts',(19.0178487259798,-21.0499310078119,-17.8699246123796));
#80327=CARTESIAN_POINT('Ctrl Pts',(19.0317029290583,-21.0480099220996,-17.86907660208));
#80328=CARTESIAN_POINT('Ctrl Pts',(19.0531996865828,-21.0448116425523,-17.8677656478585));
#80329=CARTESIAN_POINT('Ctrl Pts',(19.0608557934811,-21.0436295809423,-17.8672997081182));
#80330=CARTESIAN_POINT('Ctrl Pts',(19.0747857084879,-21.0414005250706,-17.8664536475409));
#80331=CARTESIAN_POINT('Ctrl Pts',(19.0810615885703,-21.0403672350382,-17.866073097295));
#80332=CARTESIAN_POINT('Ctrl Pts',(19.0946146228468,-21.0380730185192,-17.865252600454));
#80333=CARTESIAN_POINT('Ctrl Pts',(19.1018900448154,-21.0368022596519,-17.8648129713455));
#80334=CARTESIAN_POINT('Ctrl Pts',(19.1216341082358,-21.0332470970613,-17.8636220556546));
#80335=CARTESIAN_POINT('Ctrl Pts',(19.1340892478913,-21.0308887139837,-17.8628731273959));
#80336=CARTESIAN_POINT('Ctrl Pts',(19.1950019111816,-21.0187871780044,-17.8592210163664));
#80337=CARTESIAN_POINT('Ctrl Pts',(19.2431314240933,-21.0074604723946,-17.8563687029365));
#80338=CARTESIAN_POINT('Ctrl Pts',(19.3300587152406,-20.9837620051366,-17.8512511582915));
#80339=CARTESIAN_POINT('Ctrl Pts',(19.3689790980515,-20.9719367871477,-17.8489724874093));
#80340=CARTESIAN_POINT('Ctrl Pts',(19.5830361901105,-20.9001005188713,-17.8364468755194));
#80341=CARTESIAN_POINT('Ctrl Pts',(19.7500303845104,-20.8184476352614,-17.8267723700119));
#80342=CARTESIAN_POINT('Ctrl Pts',(19.9385731007309,-20.6933752742972,-17.8138977969149));
#80343=CARTESIAN_POINT('Ctrl Pts',(19.9722093725219,-20.6696208095459,-17.8115121651604));
#80344=CARTESIAN_POINT('Ctrl Pts',(20.0113290505122,-20.6402474956649,-17.8086027096268));
#80345=CARTESIAN_POINT('Ctrl Pts',(20.0175032145462,-20.63555831617,-17.8081394013585));
#80346=CARTESIAN_POINT('Ctrl Pts',(20.0269991210544,-20.6282637304151,-17.8074202076817));
#80347=CARTESIAN_POINT('Ctrl Pts',(20.0303391355034,-20.6256820683754,-17.8071659675805));
#80348=CARTESIAN_POINT('Ctrl Pts',(20.0364823399228,-20.6209042618402,-17.8066959451347));
#80349=CARTESIAN_POINT('Ctrl Pts',(20.039287719743,-20.6187110274869,-17.8064803686794));
#80350=CARTESIAN_POINT('Ctrl Pts',(20.0455716383609,-20.6137726899483,-17.8059953887306));
#80351=CARTESIAN_POINT('Ctrl Pts',(20.049047075152,-20.6110237565865,-17.8057257150846));
#80352=CARTESIAN_POINT('Ctrl Pts',(20.0578942383287,-20.6039807325387,-17.8050355826186));
#80353=CARTESIAN_POINT('Ctrl Pts',(20.0632536703179,-20.5996713786234,-17.8046140662291));
#80354=CARTESIAN_POINT('Ctrl Pts',(20.0940126448746,-20.5746912907569,-17.8021754183637));
#80355=CARTESIAN_POINT('Ctrl Pts',(20.1189493404682,-20.5534607304561,-17.8001214848639));
#80356=CARTESIAN_POINT('Ctrl Pts',(20.2722964420945,-20.4166436975308,-17.787052808929));
#80357=CARTESIAN_POINT('Ctrl Pts',(20.3866452805175,-20.2862799923726,-17.7753881239929));
#80358=CARTESIAN_POINT('Ctrl Pts',(20.538613230693,-20.0630879329642,-17.7578248716403));
#80359=CARTESIAN_POINT('Ctrl Pts',(20.5877451883144,-19.9790241345162,-17.7516410983881));
#80360=CARTESIAN_POINT('Ctrl Pts',(20.6405228267156,-19.8725035509622,-17.7443372880991));
#80361=CARTESIAN_POINT('Ctrl Pts',(20.6498208818888,-19.8529919416943,-17.7430197631765));
#80362=CARTESIAN_POINT('Ctrl Pts',(20.6625851614088,-19.8251151821034,-17.7411653993401));
#80363=CARTESIAN_POINT('Ctrl Pts',(20.666298799818,-19.8168654220279,-17.7406200579321));
#80364=CARTESIAN_POINT('Ctrl Pts',(20.6726029557417,-19.8026175766791,-17.7396840388364));
#80365=CARTESIAN_POINT('Ctrl Pts',(20.6752187780872,-19.7966308891183,-17.7392924973758));
#80366=CARTESIAN_POINT('Ctrl Pts',(20.6801667413029,-19.7851623506839,-17.7385457473988));
#80367=CARTESIAN_POINT('Ctrl Pts',(20.6825035346509,-19.779682586576,-17.7381903829529));
#80368=CARTESIAN_POINT('Ctrl Pts',(20.6885039127454,-19.7654454903334,-17.7372707866537));
#80369=CARTESIAN_POINT('Ctrl Pts',(20.6921318073627,-19.7566731884048,-17.7367077707049));
#80370=CARTESIAN_POINT('Ctrl Pts',(20.7042219197092,-19.726873117927,-17.7348070905714));
#80371=CARTESIAN_POINT('Ctrl Pts',(20.7124055777902,-19.7057335006389,-17.7334788098968));
#80372=CARTESIAN_POINT('Ctrl Pts',(20.782377154087,-19.515989610415,-17.7217234681205));
#80373=CARTESIAN_POINT('Ctrl Pts',(20.8228190666641,-19.3402970886071,-17.712088878132));
#80374=CARTESIAN_POINT('Ctrl Pts',(20.8489329988472,-19.0778304230901,-17.6977272841027));
#80375=CARTESIAN_POINT('Ctrl Pts',(20.8522629491512,-18.9936501035693,-17.6931104868366));
#80376=CARTESIAN_POINT('Ctrl Pts',(20.8498286810781,-18.8724118636735,-17.6861818769906));
#80377=CARTESIAN_POINT('Ctrl Pts',(20.8481091707749,-18.8353496038035,-17.6840257623756));
#80378=CARTESIAN_POINT('Ctrl Pts',(20.8448705662682,-18.7908443280256,-17.6813705740444));
#80379=CARTESIAN_POINT('Ctrl Pts',(20.8442840196782,-18.7833374654045,-17.6809204457278));
#80380=CARTESIAN_POINT('Ctrl Pts',(20.8433101782056,-18.7716753277115,-17.6802174105148));
#80381=CARTESIAN_POINT('Ctrl Pts',(20.8429506158881,-18.7675177125768,-17.6799660337094));
#80382=CARTESIAN_POINT('Ctrl Pts',(20.8422611386093,-18.7598108284493,-17.6794986428312));
#80383=CARTESIAN_POINT('Ctrl Pts',(20.8419345517853,-18.7562613195348,-17.6792828173551));
#80384=CARTESIAN_POINT('Ctrl Pts',(20.8411761378834,-18.7482405776633,-17.6787938551327));
#80385=CARTESIAN_POINT('Ctrl Pts',(20.8407390456659,-18.743769908845,-17.6785204272316));
#80386=CARTESIAN_POINT('Ctrl Pts',(20.8394074873847,-18.730583946111,-17.6777114216681));
#80387=CARTESIAN_POINT('Ctrl Pts',(20.8384731569533,-18.7218728994083,-17.677173683437));
#80388=CARTESIAN_POINT('Ctrl Pts',(20.831346153911,-18.6591026363319,-17.673276359708));
#80389=CARTESIAN_POINT('Ctrl Pts',(20.8231258686592,-18.6052987339085,-17.669815802896));
#80390=CARTESIAN_POINT('Ctrl Pts',(20.8079047420478,-18.5262173015384,-17.6646074650703));
#80391=CARTESIAN_POINT('Ctrl Pts',(20.8024914932381,-18.5006524003797,-17.6629045327568));
#80392=CARTESIAN_POINT('Ctrl Pts',(20.7656089183897,-18.341102404484,-17.6521791688563));
#80393=CARTESIAN_POINT('Ctrl Pts',(20.7216054697338,-18.210339866693,-17.6429844498354));
#80394=CARTESIAN_POINT('Ctrl Pts',(20.6398097258069,-18.0281895750498,-17.6300818320424));
#80395=CARTESIAN_POINT('Ctrl Pts',(20.6119240084307,-17.9727457059202,-17.6261358421616));
#80396=CARTESIAN_POINT('Ctrl Pts',(20.5634080540366,-17.8860026460309,-17.6199423725365));
#80397=CARTESIAN_POINT('Ctrl Pts',(20.544314439973,-17.8538897623401,-17.6176445784271));
#80398=CARTESIAN_POINT('Ctrl Pts',(20.5184327855038,-17.8128718941052,-17.6147011787904));
#80399=CARTESIAN_POINT('Ctrl Pts',(20.5124110952523,-17.8034934952971,-17.6140275929162));
#80400=CARTESIAN_POINT('Ctrl Pts',(20.5025023090888,-17.7883259934935,-17.6129371069797));
#80401=CARTESIAN_POINT('Ctrl Pts',(20.4986602376119,-17.7825078630994,-17.6125185368357));
#80402=CARTESIAN_POINT('Ctrl Pts',(20.4912197051231,-17.7713606590949,-17.6117160194871));
#80403=CARTESIAN_POINT('Ctrl Pts',(20.4876255756273,-17.7660287999786,-17.6113319154873));
#80404=CARTESIAN_POINT('Ctrl Pts',(20.4793454019425,-17.7538651755275,-17.6104550387788));
#80405=CARTESIAN_POINT('Ctrl Pts',(20.4746434182545,-17.7470443480522,-17.6099628764798));
#80406=CARTESIAN_POINT('Ctrl Pts',(20.4620560413474,-17.729012189554,-17.6086604336094));
#80407=CARTESIAN_POINT('Ctrl Pts',(20.454101518667,-17.717849423612,-17.6078527968192));
#80408=CARTESIAN_POINT('Ctrl Pts',(20.3933122321799,-17.6342719562811,-17.6017937214933));
#80409=CARTESIAN_POINT('Ctrl Pts',(20.3360310618835,-17.5651966353714,-17.5967220776201));
#80410=CARTESIAN_POINT('Ctrl Pts',(20.1788562727152,-17.3984432328899,-17.5840326092265));
#80411=CARTESIAN_POINT('Ctrl Pts',(20.0733814625243,-17.3066417416989,-17.5766122070599));
#80412=CARTESIAN_POINT('Ctrl Pts',(19.9141818591566,-17.1936004370378,-17.5658309436337));
#80413=CARTESIAN_POINT('Ctrl Pts',(19.867462249585,-17.1631286505904,-17.562707799087));
#80414=CARTESIAN_POINT('Ctrl Pts',(19.7950071468588,-17.1198500887044,-17.5578405708402));
#80415=CARTESIAN_POINT('Ctrl Pts',(19.7701220587053,-17.1056629885674,-17.5561647922503));
#80416=CARTESIAN_POINT('Ctrl Pts',(19.7388464650812,-17.0886640210807,-17.5540439634812));
#80417=CARTESIAN_POINT('Ctrl Pts',(19.7327184496974,-17.0853723338889,-17.553627725962));
#80418=CARTESIAN_POINT('Ctrl Pts',(19.7229997152573,-17.080213435689,-17.5529663267001));
#80419=CARTESIAN_POINT('Ctrl Pts',(19.7194196109493,-17.0783261839799,-17.552722415704));
#80420=CARTESIAN_POINT('Ctrl Pts',(19.7126599401845,-17.0747875564422,-17.5522613316506));
#80421=CARTESIAN_POINT('Ctrl Pts',(19.7094815854193,-17.0731339822743,-17.5520443003138));
#80422=CARTESIAN_POINT('Ctrl Pts',(19.7022086767756,-17.0693735999185,-17.5515471580382));
#80423=CARTESIAN_POINT('Ctrl Pts',(19.6981114417043,-17.0672720803474,-17.5512667192591));
#80424=CARTESIAN_POINT('Ctrl Pts',(19.6872225580158,-17.0617318426961,-17.5505205039179));
#80425=CARTESIAN_POINT('Ctrl Pts',(19.6804192335744,-17.0583163986691,-17.5500533296973));
#80426=CARTESIAN_POINT('Ctrl Pts',(19.6328430162482,-17.0347523286347,-17.5467805626035));
#80427=CARTESIAN_POINT('Ctrl Pts',(19.5914515921,-17.0158870143595,-17.5439039320113));
#80428=CARTESIAN_POINT('Ctrl Pts',(19.5442118732782,-16.9961681017593,-17.5406137141424));
#80429=CARTESIAN_POINT('Ctrl Pts',(19.5389264162691,-16.9939869364191,-17.5402454832081));
#80430=CARTESIAN_POINT('Ctrl Pts',(19.3878092937333,-16.9323402676795,-17.5297156380831));
#80431=CARTESIAN_POINT('Ctrl Pts',(19.2358034663099,-16.8893102486276,-17.5191256203768));
#80432=CARTESIAN_POINT('Ctrl Pts',(18.9788177328514,-16.8466825928729,-17.5022143684257));
#80433=CARTESIAN_POINT('Ctrl Pts',(18.876104813786,-16.8372638948765,-17.4956951972229));
#80434=CARTESIAN_POINT('Ctrl Pts',(18.7582952600754,-16.8350876255305,-17.4885096311951));
#80435=CARTESIAN_POINT('Ctrl Pts',(18.7434875798233,-16.8349694701884,-17.4876115069509));
#80436=CARTESIAN_POINT('Ctrl Pts',(18.7209109500846,-16.8350262097226,-17.4862496124459));
#80437=CARTESIAN_POINT('Ctrl Pts',(18.7131424099457,-16.8350884960878,-17.4857823308274));
#80438=CARTESIAN_POINT('Ctrl Pts',(18.69901349972,-16.8352795621371,-17.484934856235));
#80439=CARTESIAN_POINT('Ctrl Pts',(18.6926530595032,-16.8353942504218,-17.4845542266078));
#80440=CARTESIAN_POINT('Ctrl Pts',(18.678927403502,-16.8357036381158,-17.4837346976736));
#80441=CARTESIAN_POINT('Ctrl Pts',(18.6715624751479,-16.8359081211337,-17.483296109709));
#80442=CARTESIAN_POINT('Ctrl Pts',(18.6516067723349,-16.8365664545909,-17.4821107776325));
#80443=CARTESIAN_POINT('Ctrl Pts',(18.6390186128716,-16.8370942632281,-17.4813663544352));
#80444=CARTESIAN_POINT('Ctrl Pts',(18.577949934905,-16.8402011620293,-17.4777700543958));
#80445=CARTESIAN_POINT('Ctrl Pts',(18.5295609594839,-16.8443351392701,-17.4749671528917));
#80446=CARTESIAN_POINT('Ctrl Pts',(18.4408402304731,-16.8549994204974,-17.4698882870485));
#80447=CARTESIAN_POINT('Ctrl Pts',(18.4004743829692,-16.8610396968277,-17.467600608625));
#80448=CARTESIAN_POINT('Ctrl Pts',(18.2279671460885,-16.8919765050713,-17.4578738577562));
#80449=CARTESIAN_POINT('Ctrl Pts',(18.0981936187453,-16.9282619744091,-17.4507040359213));
#80450=CARTESIAN_POINT('Ctrl Pts',(17.9142079942015,-16.9991649604153,-17.4398677466165));
#80451=CARTESIAN_POINT('Ctrl Pts',(17.8567128028137,-17.0243097633019,-17.4363742109886));
#80452=CARTESIAN_POINT('Ctrl Pts',(17.7726606680223,-17.065608597365,-17.4309874974222));
#80453=CARTESIAN_POINT('Ctrl Pts',(17.7452021025995,-17.079855687701,-17.4291811158706));
#80454=CARTESIAN_POINT('Ctrl Pts',(17.7118128456444,-17.098119410001,-17.4269145457118));
#80455=CARTESIAN_POINT('Ctrl Pts',(17.7055759330753,-17.1015720074039,-17.4264881038169));
#80456=CARTESIAN_POINT('Ctrl Pts',(17.6957925209745,-17.1070525969064,-17.4258141574643));
#80457=CARTESIAN_POINT('Ctrl Pts',(17.6922341844883,-17.1090595032209,-17.4255679853148));
#80458=CARTESIAN_POINT('Ctrl Pts',(17.6855723009197,-17.1128422727838,-17.4251050888916));
#80459=CARTESIAN_POINT('Ctrl Pts',(17.6824674364376,-17.1146157035432,-17.424888520867));
#80460=CARTESIAN_POINT('Ctrl Pts',(17.6753618171657,-17.1186981875299,-17.4243910040629));
#80461=CARTESIAN_POINT('Ctrl Pts',(17.6713641284959,-17.1210124682511,-17.4241097204899));
#80462=CARTESIAN_POINT('Ctrl Pts',(17.6590006515957,-17.1282238707399,-17.4232356134878));
#80463=CARTESIAN_POINT('Ctrl Pts',(17.6506610396186,-17.1331653023303,-17.4226400250973));
#80464=CARTESIAN_POINT('Ctrl Pts',(17.5601832148601,-17.1876187224859,-17.4161155732146));
#80465=CARTESIAN_POINT('Ctrl Pts',(17.4814755037281,-17.2425950820262,-17.4098775435969));
#80466=CARTESIAN_POINT('Ctrl Pts',(17.3080589833185,-17.3821475748548,-17.3952245706541));
#80467=CARTESIAN_POINT('Ctrl Pts',(17.2166658688101,-17.4702962509117,-17.3867947967225));
#80468=CARTESIAN_POINT('Ctrl Pts',(17.0955502512068,-17.6101476027983,-17.3748732461246));
#80469=CARTESIAN_POINT('Ctrl Pts',(17.0592305945565,-17.6557616599507,-17.3711748626576));
#80470=CARTESIAN_POINT('Ctrl Pts',(17.0037578913632,-17.7316609561797,-17.3653244375874));
#80471=CARTESIAN_POINT('Ctrl Pts',(16.9834112147788,-17.7610322063367,-17.363128715548));
#80472=CARTESIAN_POINT('Ctrl Pts',(16.957800802189,-17.8000773821775,-17.3602956476176));
#80473=CARTESIAN_POINT('Ctrl Pts',(16.9518562852668,-17.809295709781,-17.3596328517881));
#80474=CARTESIAN_POINT('Ctrl Pts',(16.9422715547169,-17.8244157469037,-17.358555467737));
#80475=CARTESIAN_POINT('Ctrl Pts',(16.938588272585,-17.8302897877315,-17.3581392837314));
#80476=CARTESIAN_POINT('Ctrl Pts',(16.931537785762,-17.841657493327,-17.3573383877422));
#80477=CARTESIAN_POINT('Ctrl Pts',(16.9281666793966,-17.8471486364691,-17.3569535347569));
#80478=CARTESIAN_POINT('Ctrl Pts',(16.9204737498509,-17.8598088030428,-17.3560708139716));
#80479=CARTESIAN_POINT('Ctrl Pts',(16.9161692543657,-17.8669882701148,-17.3555735847864));
#80480=CARTESIAN_POINT('Ctrl Pts',(16.904778877573,-17.886244337519,-17.3542487688532));
#80481=CARTESIAN_POINT('Ctrl Pts',(16.8977699574249,-17.8983661491638,-17.3534239746956));
#80482=CARTESIAN_POINT('Ctrl Pts',(16.841012124919,-17.9988146452115,-17.3466623653921));
#80483=CARTESIAN_POINT('Ctrl Pts',(16.797542816139,-18.090546111532,-17.3409591144045));
#80484=CARTESIAN_POINT('Ctrl Pts',(16.7062965953606,-18.3253020389762,-17.327088482644));
#80485=CARTESIAN_POINT('Ctrl Pts',(16.66689522666,-18.4709554092311,-17.3191198229837));
#80486=CARTESIAN_POINT('Ctrl Pts',(16.6370543890108,-18.6586173482729,-17.3084710818138));
#80487=CARTESIAN_POINT('Ctrl Pts',(16.6319381894214,-18.6978542678952,-17.3062221120722));
#80488=CARTESIAN_POINT('Ctrl Pts',(16.6263939790653,-18.752216547317,-17.3030474639199));
#80489=CARTESIAN_POINT('Ctrl Pts',(16.6250239190544,-18.7672395315892,-17.302163979958));
#80490=CARTESIAN_POINT('Ctrl Pts',(16.6229323250401,-18.7932443177377,-17.3006220405579));
#80491=CARTESIAN_POINT('Ctrl Pts',(16.6221356451372,-18.8042196565844,-17.2999673810642));
#80492=CARTESIAN_POINT('Ctrl Pts',(16.6211102618329,-18.8200544997707,-17.2990166266043));
#80493=CARTESIAN_POINT('Ctrl Pts',(16.6208126721322,-18.8249095717865,-17.2987242743752));
#80494=CARTESIAN_POINT('Ctrl Pts',(16.6203235173838,-18.8333671970458,-17.2982134544967));
#80495=CARTESIAN_POINT('Ctrl Pts',(16.6201244222717,-18.8369693221453,-17.2979954085226));
#80496=CARTESIAN_POINT('Ctrl Pts',(16.6197264097709,-18.8445206026431,-17.2975372654557));
#80497=CARTESIAN_POINT('Ctrl Pts',(16.6195293495792,-18.8484697961352,-17.297297070256));
#80498=CARTESIAN_POINT('Ctrl Pts',(16.6190357980362,-18.8589506819446,-17.2966580745959));
#80499=CARTESIAN_POINT('Ctrl Pts',(16.6187585037423,-18.865483174457,-17.2962582227246));
#80500=CARTESIAN_POINT('Ctrl Pts',(16.6177066689221,-18.8933033043853,-17.2945489332139));
#80501=CARTESIAN_POINT('Ctrl Pts',(16.6172232249897,-18.9145998706016,-17.2932244419876));
#80502=CARTESIAN_POINT('Ctrl Pts',(16.6170218768584,-18.9410730857242,-17.29156108135));
#80503=CARTESIAN_POINT('Ctrl Pts',(16.6170014935722,-18.9462471117899,-17.2912351841013));
#80504=CARTESIAN_POINT('Ctrl Pts',(16.6169868170195,-18.9999278656385,-17.2878459960333));
#80505=CARTESIAN_POINT('Ctrl Pts',(16.6186407107698,-19.048417613827,-17.2847171524678));
#80506=CARTESIAN_POINT('Ctrl Pts',(16.6353861375546,-19.2926578549782,-17.2687464387349));
#80507=CARTESIAN_POINT('Ctrl Pts',(16.6759975329941,-19.4857400604894,-17.2555537953033));
#80508=CARTESIAN_POINT('Ctrl Pts',(16.7435636736328,-19.6730128904649,-17.2430395163305));
#80509=CARTESIAN_POINT('Ctrl Pts',(16.7444891185652,-19.6755625818381,-17.2428691667365));
#80510=CARTESIAN_POINT('Ctrl Pts',(16.7454194498739,-19.6781104569281,-17.2426989690604));
#80511=CARTESIAN_POINT('Origin',(18.734,-18.952,0.));
#80512=CARTESIAN_POINT('',(16.7454194329591,-19.6781104106039,-16.4437313840672));
#80513=CARTESIAN_POINT('',(16.7454194499739,-19.6781104572019,-16.6645989847956));
#80514=CARTESIAN_POINT('',(16.7454194499637,-19.6781104571739,0.));
#80515=CARTESIAN_POINT('',(16.6170007987637,-18.9530960249984,-16.7126929437736));
#80516=CARTESIAN_POINT('Ctrl Pts',(16.7454194499739,-19.6781104572019,-16.6645989847956));
#80517=CARTESIAN_POINT('Ctrl Pts',(16.7447285794631,-19.6762183874118,-16.6647267402562));
#80518=CARTESIAN_POINT('Ctrl Pts',(16.7440404071567,-19.6743253256948,-16.6648546065633));
#80519=CARTESIAN_POINT('Ctrl Pts',(16.6879393952875,-19.5193109532753,-16.675328438261));
#80520=CARTESIAN_POINT('Ctrl Pts',(16.6503766399063,-19.3603127697113,-16.6862947944489));
#80521=CARTESIAN_POINT('Ctrl Pts',(16.6218547097861,-19.1171078230942,-16.7022899066289));
#80522=CARTESIAN_POINT('Ctrl Pts',(16.6170428510306,-19.0351423589209,-16.7075611653873));
#80523=CARTESIAN_POINT('Ctrl Pts',(16.6170002849213,-18.9530983426379,-16.7126936923974));
#80524=CARTESIAN_POINT('Ctrl Pts',(16.6170002837491,-18.9530960809383,-16.7126938338853));
#80525=CARTESIAN_POINT('Ctrl Pts',(16.6169868619618,-18.9271728859926,-16.7143155418154));
#80526=CARTESIAN_POINT('Ctrl Pts',(16.6174495936263,-18.9012505641371,-16.715923233117));
#80527=CARTESIAN_POINT('Ctrl Pts',(16.6190263314276,-18.8577355919444,-16.718599006575));
#80528=CARTESIAN_POINT('Ctrl Pts',(16.6198840706988,-18.8401372970935,-16.7196748223783));
#80529=CARTESIAN_POINT('Ctrl Pts',(16.6214584275455,-18.8144384867155,-16.7212369178697));
#80530=CARTESIAN_POINT('Ctrl Pts',(16.6220021597015,-18.8063284834004,-16.721728583908));
#80531=CARTESIAN_POINT('Ctrl Pts',(16.6230473347477,-18.7919780147991,-16.7225963283517));
#80532=CARTESIAN_POINT('Ctrl Pts',(16.6235297739623,-18.7857363028034,-16.7229729989713));
#80533=CARTESIAN_POINT('Ctrl Pts',(16.6245388663628,-18.7733936660693,-16.7237163836535));
#80534=CARTESIAN_POINT('Ctrl Pts',(16.6250643172567,-18.7672927069112,-16.7240831317392));
#80535=CARTESIAN_POINT('Ctrl Pts',(16.626163866657,-18.7551428118738,-16.7248121241648));
#80536=CARTESIAN_POINT('Ctrl Pts',(16.6267375501404,-18.7490938982214,-16.725174377874));
#80537=CARTESIAN_POINT('Ctrl Pts',(16.6281714412872,-18.7346373835589,-16.7260385542006));
#80538=CARTESIAN_POINT('Ctrl Pts',(16.629055973347,-18.7262322575702,-16.7265397080837));
#80539=CARTESIAN_POINT('Ctrl Pts',(16.631901147117,-18.7006681922977,-16.7280602026543));
#80540=CARTESIAN_POINT('Ctrl Pts',(16.6340214765645,-18.6835274836393,-16.729074529535));
#80541=CARTESIAN_POINT('Ctrl Pts',(16.6419661876515,-18.6251729868462,-16.7325118371407));
#80542=CARTESIAN_POINT('Ctrl Pts',(16.6487962645608,-18.5841045300971,-16.734903572597));
#80543=CARTESIAN_POINT('Ctrl Pts',(16.6900265319096,-18.3745762578523,-16.7470133625295));
#80544=CARTESIAN_POINT('Ctrl Pts',(16.7436413674956,-18.2105702553108,-16.7561209259851));
#80545=CARTESIAN_POINT('Ctrl Pts',(16.8430671589661,-17.9980646740256,-16.7690150810144));
#80546=CARTESIAN_POINT('Ctrl Pts',(16.8721436967597,-17.9424904293108,-16.7725069238828));
#80547=CARTESIAN_POINT('Ctrl Pts',(16.9191779886948,-17.8615568448669,-16.777891277069));
#80548=CARTESIAN_POINT('Ctrl Pts',(16.935298360219,-17.8351663546488,-16.7796970804036));
#80549=CARTESIAN_POINT('Ctrl Pts',(16.955838015889,-17.8031397960092,-16.7819630062873));
#80550=CARTESIAN_POINT('Ctrl Pts',(16.9597163394809,-17.7971591889894,-16.782389404854));
#80551=CARTESIAN_POINT('Ctrl Pts',(16.9658647092424,-17.7877821157767,-16.7830632979736));
#80552=CARTESIAN_POINT('Ctrl Pts',(16.9681145509226,-17.7843723759453,-16.7833094605694));
#80553=CARTESIAN_POINT('Ctrl Pts',(16.9723521715762,-17.7779903260258,-16.7837723491849));
#80554=CARTESIAN_POINT('Ctrl Pts',(16.9743376166485,-17.7750165328631,-16.7839889190161));
#80555=CARTESIAN_POINT('Ctrl Pts',(16.978905371182,-17.7682123568627,-16.7844864535024));
#80556=CARTESIAN_POINT('Ctrl Pts',(16.9814926831268,-17.7643853977311,-16.784767753039));
#80557=CARTESIAN_POINT('Ctrl Pts',(16.9895487940191,-17.7525530505832,-16.7856419578467));
#80558=CARTESIAN_POINT('Ctrl Pts',(16.9950599851321,-17.7445768715979,-16.7862376289525));
#80559=CARTESIAN_POINT('Ctrl Pts',(17.05732849338,-17.6557681672781,-16.7929390074858));
#80560=CARTESIAN_POINT('Ctrl Pts',(17.1196150424624,-17.5789738219457,-16.7993722687496));
#80561=CARTESIAN_POINT('Ctrl Pts',(17.3015406410054,-17.3842341960491,-16.8169267170906));
#80562=CARTESIAN_POINT('Ctrl Pts',(17.4302425940965,-17.2756758752608,-16.8280724208305));
#80563=CARTESIAN_POINT('Ctrl Pts',(17.5967906324138,-17.1660996689677,-16.8405985752254));
#80564=CARTESIAN_POINT('Ctrl Pts',(17.6235430655295,-17.1493434326143,-16.8425611955875));
#80565=CARTESIAN_POINT('Ctrl Pts',(17.6638282754041,-17.1253483213788,-16.8454447197155));
#80566=CARTESIAN_POINT('Ctrl Pts',(17.6770802494969,-17.117648742606,-16.8463820279014));
#80567=CARTESIAN_POINT('Ctrl Pts',(17.7013526733181,-17.1038965027822,-16.8480787278338));
#80568=CARTESIAN_POINT('Ctrl Pts',(17.7123455632341,-17.0977968665062,-16.8488397815537));
#80569=CARTESIAN_POINT('Ctrl Pts',(17.7297375505029,-17.088348187627,-16.8500324660596));
#80570=CARTESIAN_POINT('Ctrl Pts',(17.7361004338387,-17.0849334229608,-16.8504664370605));
#80571=CARTESIAN_POINT('Ctrl Pts',(17.7425268570161,-17.0815267953092,-16.8509023811204));
#80572=CARTESIAN_POINT('Ctrl Pts',(17.7425729891198,-17.0815023430055,-16.8509055104243));
#80573=CARTESIAN_POINT('Ctrl Pts',(17.7426668794635,-17.0814525809145,-16.8509118790902));
#80574=CARTESIAN_POINT('Ctrl Pts',(17.7427146386244,-17.0814272707957,-16.8509151185059));
#80575=CARTESIAN_POINT('Ctrl Pts',(17.7428118423549,-17.0813757621387,-16.8509217113889));
#80576=CARTESIAN_POINT('Ctrl Pts',(17.7428612879522,-17.081349563224,-16.8509250649166));
#80577=CARTESIAN_POINT('Ctrl Pts',(17.7429619260082,-17.0812962449244,-16.8509318901631));
#80578=CARTESIAN_POINT('Ctrl Pts',(17.7430131194289,-17.0812691252103,-16.8509353619371));
#80579=CARTESIAN_POINT('Ctrl Pts',(17.7431173170041,-17.0812139320234,-16.8509424279772));
#80580=CARTESIAN_POINT('Ctrl Pts',(17.7431703219175,-17.081185858342,-16.850946022284));
#80581=CARTESIAN_POINT('Ctrl Pts',(17.7432782085371,-17.0811287228202,-16.8509533378366));
#80582=CARTESIAN_POINT('Ctrl Pts',(17.7433330911034,-17.081099660732,-16.8509570591291));
#80583=CARTESIAN_POINT('Ctrl Pts',(17.7434448015627,-17.0810405127361,-16.8509646332646));
#80584=CARTESIAN_POINT('Ctrl Pts',(17.7435016301821,-17.0810104266667,-16.8509684861445));
#80585=CARTESIAN_POINT('Ctrl Pts',(17.7436173038241,-17.0809491937557,-16.850976328236));
#80586=CARTESIAN_POINT('Ctrl Pts',(17.7436761494837,-17.080918046816,-16.8509803174775));
#80587=CARTESIAN_POINT('Ctrl Pts',(17.7437959307841,-17.0808546539457,-16.8509884372397));
#80588=CARTESIAN_POINT('Ctrl Pts',(17.7438568670515,-17.08082240794,-16.8509925677885));
#80589=CARTESIAN_POINT('Ctrl Pts',(17.7439809057941,-17.0807567773794,-16.851000975289));
#80590=CARTESIAN_POINT('Ctrl Pts',(17.7440440088359,-17.0807233927999,-16.8510052522637));
#80591=CARTESIAN_POINT('Ctrl Pts',(17.744172460018,-17.0806554441905,-16.8510139579162));
#80592=CARTESIAN_POINT('Ctrl Pts',(17.7442378087646,-17.0806208801353,-16.8510183866186));
#80593=CARTESIAN_POINT('Ctrl Pts',(17.7443708352629,-17.0805505290919,-16.851027401363));
#80594=CARTESIAN_POINT('Ctrl Pts',(17.7444385102685,-17.0805147438732,-16.8510319872011));
#80595=CARTESIAN_POINT('Ctrl Pts',(17.7445651192025,-17.0804478043335,-16.8510405660683));
#80596=CARTESIAN_POINT('Ctrl Pts',(17.7446240540237,-17.0804166484052,-16.8510445592212));
#80597=CARTESIAN_POINT('Ctrl Pts',(17.7447516746761,-17.0803491893842,-16.8510532057803));
#80598=CARTESIAN_POINT('Ctrl Pts',(17.7448203621204,-17.0803128867143,-16.8510578592246));
#80599=CARTESIAN_POINT('Ctrl Pts',(17.7449690843897,-17.0802342945335,-16.8510679342921));
#80600=CARTESIAN_POINT('Ctrl Pts',(17.7450491209302,-17.0801920058454,-16.8510733559352));
#80601=CARTESIAN_POINT('Ctrl Pts',(17.7452223913948,-17.0801004696195,-16.8510850924134));
#80602=CARTESIAN_POINT('Ctrl Pts',(17.7453156269186,-17.0800512235794,-16.8510914072264));
#80603=CARTESIAN_POINT('Ctrl Pts',(17.7455174354136,-17.079944649701,-16.8511050745769));
#80604=CARTESIAN_POINT('Ctrl Pts',(17.7456260101929,-17.0798873240781,-16.8511124270602));
#80605=CARTESIAN_POINT('Ctrl Pts',(17.7458609678064,-17.0797632966216,-16.8511283364974));
#80606=CARTESIAN_POINT('Ctrl Pts',(17.7459873521322,-17.0796965982846,-16.8511368933133));
#80607=CARTESIAN_POINT('Ctrl Pts',(17.7462732758041,-17.0795457413211,-16.8511562496328));
#80608=CARTESIAN_POINT('Ctrl Pts',(17.7464328191866,-17.0794615902696,-16.8511670488684));
#80609=CARTESIAN_POINT('Ctrl Pts',(17.7523042775245,-17.076365652558,-16.8515644249942));
#80610=CARTESIAN_POINT('Ctrl Pts',(17.7580299798871,-17.0733799697391,-16.851950074291));
#80611=CARTESIAN_POINT('Ctrl Pts',(17.7712868268408,-17.0665441172548,-16.8528387314697));
#80612=CARTESIAN_POINT('Ctrl Pts',(17.7788275960508,-17.062712774231,-16.8533410721469));
#80613=CARTESIAN_POINT('Ctrl Pts',(17.7991801830064,-17.052524954163,-16.8546885868926));
#80614=CARTESIAN_POINT('Ctrl Pts',(17.8120339262939,-17.0462528725238,-16.8555308132934));
#80615=CARTESIAN_POINT('Ctrl Pts',(17.9304939887427,-16.989928428021,-16.8632149915667));
#80616=CARTESIAN_POINT('Ctrl Pts',(18.0400179132035,-16.9485677221105,-16.8697401034514));
#80617=CARTESIAN_POINT('Ctrl Pts',(18.3090801895793,-16.8716919252939,-16.8850589580981));
#80618=CARTESIAN_POINT('Ctrl Pts',(18.4703755118528,-16.8451709323919,-16.8936690031478));
#80619=CARTESIAN_POINT('Ctrl Pts',(18.6653344442067,-16.8358677130347,-16.9048788398518));
#80620=CARTESIAN_POINT('Ctrl Pts',(18.6976039157534,-16.8350668684478,-16.9067617345747));
#80621=CARTESIAN_POINT('Ctrl Pts',(18.7371007728534,-16.8349899462351,-16.9091135022835));
#80622=CARTESIAN_POINT('Ctrl Pts',(18.7443244133671,-16.8350128518101,-16.9095455516763));
#80623=CARTESIAN_POINT('Ctrl Pts',(18.7556537446253,-16.8351067631316,-16.9102263895025));
#80624=CARTESIAN_POINT('Ctrl Pts',(18.7597596651064,-16.8351527452482,-16.9104737998769));
#80625=CARTESIAN_POINT('Ctrl Pts',(18.7674374807421,-16.8352610701164,-16.9109377275042));
#80626=CARTESIAN_POINT('Ctrl Pts',(18.7710093606906,-16.8353205086823,-16.9111540806862));
#80627=CARTESIAN_POINT('Ctrl Pts',(18.7791670149684,-16.8354769126114,-16.911649388466));
#80628=CARTESIAN_POINT('Ctrl Pts',(18.7837526198016,-16.8355797405529,-16.9119286667462));
#80629=CARTESIAN_POINT('Ctrl Pts',(18.7978618606407,-16.8359420068896,-16.9127905191966));
#80630=CARTESIAN_POINT('Ctrl Pts',(18.807383954816,-16.8362508289425,-16.9133757499156));
#80631=CARTESIAN_POINT('Ctrl Pts',(18.9364216048654,-16.8413079269359,-16.9213520338047));
#80632=CARTESIAN_POINT('Ctrl Pts',(19.0553143784831,-16.8561121280792,-16.9292199952126));
#80633=CARTESIAN_POINT('Ctrl Pts',(19.2789140605583,-16.9034317053216,-16.9443187785163));
#80634=CARTESIAN_POINT('Ctrl Pts',(19.3836298788765,-16.9341923064276,-16.951521706623));
#80635=CARTESIAN_POINT('Ctrl Pts',(19.5556677213986,-16.9995190604651,-16.9633455044071));
#80636=CARTESIAN_POINT('Ctrl Pts',(19.6243581520663,-17.0298698870102,-16.9680665544473));
#80637=CARTESIAN_POINT('Ctrl Pts',(19.7080738059936,-17.072313066918,-16.9738164718044));
#80638=CARTESIAN_POINT('Ctrl Pts',(19.7247354535037,-17.0810414106852,-16.9749608382613));
#80639=CARTESIAN_POINT('Ctrl Pts',(19.7488030543216,-17.0940611045734,-16.9766142763129));
#80640=CARTESIAN_POINT('Ctrl Pts',(19.7563024514415,-17.0981769557664,-16.9771295437616));
#80641=CARTESIAN_POINT('Ctrl Pts',(19.7694115851867,-17.1054753070374,-16.9780304179974));
#80642=CARTESIAN_POINT('Ctrl Pts',(19.7750320715254,-17.1086381744371,-16.9784167207105));
#80643=CARTESIAN_POINT('Ctrl Pts',(19.7859208829156,-17.1148314196666,-16.9791652681094));
#80644=CARTESIAN_POINT('Ctrl Pts',(19.7911907786622,-17.117858894421,-16.9795276123247));
#80645=CARTESIAN_POINT('Ctrl Pts',(19.8037626957109,-17.1251534546107,-16.9803922263226));
#80646=CARTESIAN_POINT('Ctrl Pts',(19.81105236395,-17.1294417062823,-16.9808937255789));
#80647=CARTESIAN_POINT('Ctrl Pts',(19.8372940336706,-17.1450911698053,-16.9826998226498));
#80648=CARTESIAN_POINT('Ctrl Pts',(19.8560939917438,-17.1567054912149,-16.9839951962583));
#80649=CARTESIAN_POINT('Ctrl Pts',(20.0311368845103,-17.2686682715246,-16.9960802779257));
#80650=CARTESIAN_POINT('Ctrl Pts',(20.1737172751414,-17.3888653358452,-17.0060122550063));
#80651=CARTESIAN_POINT('Ctrl Pts',(20.3527290484362,-17.5853189324434,-17.0205013874553));
#80652=CARTESIAN_POINT('Ctrl Pts',(20.4032560404005,-17.647514223404,-17.0249051360636));
#80653=CARTESIAN_POINT('Ctrl Pts',(20.4712215009817,-17.7416086132237,-17.0315447780943));
#80654=CARTESIAN_POINT('Ctrl Pts',(20.4915580853202,-17.771332781315,-17.0336394819498));
#80655=CARTESIAN_POINT('Ctrl Pts',(20.5151821465616,-17.8078256736547,-17.0362265599653));
#80656=CARTESIAN_POINT('Ctrl Pts',(20.5192056819206,-17.8141136270391,-17.0366728687045));
#80657=CARTESIAN_POINT('Ctrl Pts',(20.5254189178358,-17.8239376972936,-17.0373712172081));
#80658=CARTESIAN_POINT('Ctrl Pts',(20.5276316423008,-17.8274592808524,-17.0376217595799));
#80659=CARTESIAN_POINT('Ctrl Pts',(20.5317222171217,-17.8340122782707,-17.0380884032046));
#80660=CARTESIAN_POINT('Ctrl Pts',(20.5336027909015,-17.8370419244456,-17.0383043209604));
#80661=CARTESIAN_POINT('Ctrl Pts',(20.5378449737054,-17.8439148684098,-17.0387945329832));
#80662=CARTESIAN_POINT('Ctrl Pts',(20.5402019468074,-17.8477609522881,-17.0390691248937));
#80663=CARTESIAN_POINT('Ctrl Pts',(20.5462563197446,-17.8577116609078,-17.0397801942039));
#80664=CARTESIAN_POINT('Ctrl Pts',(20.5499351383302,-17.8638274458553,-17.0402178389317));
#80665=CARTESIAN_POINT('Ctrl Pts',(20.5723468941321,-17.9015156168502,-17.0429180080681));
#80666=CARTESIAN_POINT('Ctrl Pts',(20.5902856621675,-17.9335502427578,-17.0452268350105));
#80667=CARTESIAN_POINT('Ctrl Pts',(20.6867170429272,-18.1167741044773,-17.0584408359818));
#80668=CARTESIAN_POINT('Ctrl Pts',(20.7475690815485,-18.2765381088593,-17.0699344866839));
#80669=CARTESIAN_POINT('Ctrl Pts',(20.8116284131515,-18.5345466485141,-17.0872115149507));
#80670=CARTESIAN_POINT('Ctrl Pts',(20.8283439679135,-18.6286816855436,-17.0932786896403));
#80671=CARTESIAN_POINT('Ctrl Pts',(20.8409558102816,-18.7449146453183,-17.1004603605687));
#80672=CARTESIAN_POINT('Ctrl Pts',(20.8429419120807,-18.7662281106361,-17.1017650263321));
#80673=CARTESIAN_POINT('Ctrl Pts',(20.8453044658029,-18.796553331079,-17.1036045772717));
#80674=CARTESIAN_POINT('Ctrl Pts',(20.845947066957,-18.8055424822839,-17.1041477817932));
#80675=CARTESIAN_POINT('Ctrl Pts',(20.8469560595829,-18.8210485263731,-17.1050812784005));
#80676=CARTESIAN_POINT('Ctrl Pts',(20.8473497456271,-18.8275634607029,-17.105472422119));
#80677=CARTESIAN_POINT('Ctrl Pts',(20.8480455177565,-18.8400351780281,-17.1062191902275));
#80678=CARTESIAN_POINT('Ctrl Pts',(20.8483525711413,-18.8459916110184,-17.1065749668025));
#80679=CARTESIAN_POINT('Ctrl Pts',(20.8490849458517,-18.8614708124556,-17.1074973016845));
#80680=CARTESIAN_POINT('Ctrl Pts',(20.8494711332539,-18.8709953652404,-17.1080626293174));
#80681=CARTESIAN_POINT('Ctrl Pts',(20.8505663739781,-18.9034153135123,-17.1099796816219));
#80682=CARTESIAN_POINT('Ctrl Pts',(20.8509681820027,-18.9263199714303,-17.1113217975202));
#80683=CARTESIAN_POINT('Ctrl Pts',(20.8512294930595,-19.1258362738193,-17.1229163774947));
#80684=CARTESIAN_POINT('Ctrl Pts',(20.8293620217039,-19.3017776712722,-17.1324066359812));
#80685=CARTESIAN_POINT('Ctrl Pts',(20.7646786984319,-19.5565379749944,-17.1467108196941));
#80686=CARTESIAN_POINT('Ctrl Pts',(20.7383784614357,-19.638721758431,-17.151433132377));
#80687=CARTESIAN_POINT('Ctrl Pts',(20.6935122054658,-19.7541324046316,-17.1585043066941));
#80688=CARTESIAN_POINT('Ctrl Pts',(20.6789486538994,-19.7888266357435,-17.1606900429626));
#80689=CARTESIAN_POINT('Ctrl Pts',(20.6603586880015,-19.8300024841953,-17.1633780704574));
#80690=CARTESIAN_POINT('Ctrl Pts',(20.6572109370662,-19.8368761748025,-17.1638299946993));
#80691=CARTESIAN_POINT('Ctrl Pts',(20.6522658643476,-19.8475236145485,-17.1645352329974));
#80692=CARTESIAN_POINT('Ctrl Pts',(20.6504940333148,-19.8513092294148,-17.1647870014815));
#80693=CARTESIAN_POINT('Ctrl Pts',(20.6471906570234,-19.8583129768261,-17.1652547463598));
#80694=CARTESIAN_POINT('Ctrl Pts',(20.6456621918922,-19.8615324983697,-17.1654705317739));
#80695=CARTESIAN_POINT('Ctrl Pts',(20.6421925962735,-19.8687933878563,-17.1659589220415));
#80696=CARTESIAN_POINT('Ctrl Pts',(20.6402467642362,-19.872832435068,-17.1662318150648));
#80697=CARTESIAN_POINT('Ctrl Pts',(20.6344782275707,-19.8847097936444,-17.1670378067765));
#80698=CARTESIAN_POINT('Ctrl Pts',(20.6306199561418,-19.8925305888619,-17.1675730425713));
#80699=CARTESIAN_POINT('Ctrl Pts',(20.6028094446167,-19.9480360450982,-17.1714027852549));
#80700=CARTESIAN_POINT('Ctrl Pts',(20.5771120906545,-19.9948198922747,-17.1747944177196));
#80701=CARTESIAN_POINT('Ctrl Pts',(20.5406295266286,-20.0556704152153,-17.1793798390697));
#80702=CARTESIAN_POINT('Ctrl Pts',(20.5313936963559,-20.0706485185349,-17.18052311187));
#80703=CARTESIAN_POINT('Ctrl Pts',(20.4960022688965,-20.1264741635916,-17.1848351015557));
#80704=CARTESIAN_POINT('Ctrl Pts',(20.4686326062794,-20.1665332600283,-17.1880325757327));
#80705=CARTESIAN_POINT('Ctrl Pts',(20.3751393206793,-20.2937582976294,-17.1984619202417));
#80706=CARTESIAN_POINT('Ctrl Pts',(20.3036275260464,-20.3767548892263,-17.2056947196037));
#80707=CARTESIAN_POINT('Ctrl Pts',(20.1869267148664,-20.4926911218813,-17.2162683684722));
#80708=CARTESIAN_POINT('Ctrl Pts',(20.1463326182621,-20.5299868720245,-17.2197575951288));
#80709=CARTESIAN_POINT('Ctrl Pts',(20.0781788416052,-20.587863377476,-17.2253152909978));
#80710=CARTESIAN_POINT('Ctrl Pts',(20.0514942467233,-20.6094302018997,-17.2274222011303));
#80711=CARTESIAN_POINT('Ctrl Pts',(20.0157271166172,-20.6369277202113,-17.2301587782194));
#80712=CARTESIAN_POINT('Ctrl Pts',(20.0071077758976,-20.6434497987061,-17.2308117875296));
#80713=CARTESIAN_POINT('Ctrl Pts',(19.9929062851411,-20.6540257189612,-17.2318772931054));
#80714=CARTESIAN_POINT('Ctrl Pts',(19.9873536799611,-20.6581187348637,-17.2322913188467));
#80715=CARTESIAN_POINT('Ctrl Pts',(19.9765651495648,-20.6659902387322,-17.2330908347344));
#80716=CARTESIAN_POINT('Ctrl Pts',(19.9713317550894,-20.6697720508424,-17.2334764512315));
#80717=CARTESIAN_POINT('Ctrl Pts',(19.9592058797045,-20.6784504141309,-17.2343648686458));
#80718=CARTESIAN_POINT('Ctrl Pts',(19.9523011746944,-20.6833297580232,-17.2348670035122));
#80719=CARTESIAN_POINT('Ctrl Pts',(19.9336483210147,-20.6963443178347,-17.2362136017454));
#80720=CARTESIAN_POINT('Ctrl Pts',(19.9218466006839,-20.704402254458,-17.2370551237865));
#80721=CARTESIAN_POINT('Ctrl Pts',(19.8128220352967,-20.777234176032,-17.244736211265));
#80722=CARTESIAN_POINT('Ctrl Pts',(19.7104695089811,-20.8339801649476,-17.2512591668123));
#80723=CARTESIAN_POINT('Ctrl Pts',(19.4555753743655,-20.9488735719642,-17.266565339726));
#80724=CARTESIAN_POINT('Ctrl Pts',(19.3000076244706,-20.998411150779,-17.2751654658189));
#80725=CARTESIAN_POINT('Ctrl Pts',(19.1084209255003,-21.0358797194721,-17.2863744842733));
#80726=CARTESIAN_POINT('Ctrl Pts',(19.0763806304814,-21.0413829130412,-17.2882704544787));
#80727=CARTESIAN_POINT('Ctrl Pts',(19.037067009099,-21.0472068630164,-17.2906367699506));
#80728=CARTESIAN_POINT('Ctrl Pts',(19.0299003533086,-21.0482309959315,-17.2910697519764));
#80729=CARTESIAN_POINT('Ctrl Pts',(19.0186574245896,-21.0497788348875,-17.2917517357108));
#80730=CARTESIAN_POINT('Ctrl Pts',(19.0145845617733,-21.0503274750406,-17.2919993516869));
#80731=CARTESIAN_POINT('Ctrl Pts',(19.0069688193734,-21.0513307939579,-17.2924634529984));
#80732=CARTESIAN_POINT('Ctrl Pts',(19.0034263778175,-21.0517883667384,-17.2926797729726));
#80733=CARTESIAN_POINT('Ctrl Pts',(18.9953375389615,-21.0528123860249,-17.2931747252015));
#80734=CARTESIAN_POINT('Ctrl Pts',(18.9907904661317,-21.0533730383105,-17.2934536793413));
#80735=CARTESIAN_POINT('Ctrl Pts',(18.9768089142779,-21.0550509002867,-17.294313560248));
#80736=CARTESIAN_POINT('Ctrl Pts',(18.9673688572317,-21.0561193470884,-17.2948971263252));
#80737=CARTESIAN_POINT('Ctrl Pts',(18.8825100990503,-21.0651457761149,-17.3001678465681));
#80738=CARTESIAN_POINT('Ctrl Pts',(18.806729387204,-21.0691084564982,-17.3050497269885));
#80739=CARTESIAN_POINT('Ctrl Pts',(18.5459858057495,-21.0687277182614,-17.3221026647377));
#80740=CARTESIAN_POINT('Ctrl Pts',(18.3618555908207,-21.0442270342742,-17.3344994882983));
#80741=CARTESIAN_POINT('Ctrl Pts',(18.1318214783832,-20.9822479470869,-17.3495264397384));
#80742=CARTESIAN_POINT('Ctrl Pts',(18.0809327593344,-20.9664551810059,-17.3528279669364));
#80743=CARTESIAN_POINT('Ctrl Pts',(18.018861844955,-20.9445922023598,-17.3568295848838));
#80744=CARTESIAN_POINT('Ctrl Pts',(18.0070706217971,-20.9403208884438,-17.3575886336221));
#80745=CARTESIAN_POINT('Ctrl Pts',(17.9884944316745,-20.9334044163272,-17.3587828592442));
#80746=CARTESIAN_POINT('Ctrl Pts',(17.9816841035877,-20.9308286453137,-17.3592203398635));
#80747=CARTESIAN_POINT('Ctrl Pts',(17.9689419835707,-20.9259340899503,-17.3600382710444));
#80748=CARTESIAN_POINT('Ctrl Pts',(17.9630071203189,-20.9236235799011,-17.3604189934957));
#80749=CARTESIAN_POINT('Ctrl Pts',(17.9497498742878,-20.9183933685983,-17.361268944669));
#80750=CARTESIAN_POINT('Ctrl Pts',(17.9424331662305,-20.9154594699138,-17.3617376895754));
#80751=CARTESIAN_POINT('Ctrl Pts',(17.9239378049553,-20.9079228976669,-17.3629218176192));
#80752=CARTESIAN_POINT('Ctrl Pts',(17.9127817811841,-20.9032651761447,-17.3636353351782));
#80753=CARTESIAN_POINT('Ctrl Pts',(17.8493602283988,-20.876145945981,-17.3676884274963));
#80754=CARTESIAN_POINT('Ctrl Pts',(17.7979742561163,-20.8516793899288,-17.3709588925312));
#80755=CARTESIAN_POINT('Ctrl Pts',(17.7238752779461,-20.8126606260659,-17.3756896508523));
#80756=CARTESIAN_POINT('Ctrl Pts',(17.7003574321009,-20.7996993886095,-17.3771935568014));
#80757=CARTESIAN_POINT('Ctrl Pts',(17.5767171564955,-20.7284586784432,-17.3851309162804));
#80758=CARTESIAN_POINT('Ctrl Pts',(17.481259293531,-20.6624825405355,-17.3913558095641));
#80759=CARTESIAN_POINT('Ctrl Pts',(17.3297857736773,-20.538277826611,-17.4020347080446));
#80760=CARTESIAN_POINT('Ctrl Pts',(17.2708273778643,-20.4840635801267,-17.4064365281268));
#80761=CARTESIAN_POINT('Ctrl Pts',(17.190006383073,-20.4008163593799,-17.4130735474593));
#80762=CARTESIAN_POINT('Ctrl Pts',(17.1655931027784,-20.374351781112,-17.4151676854633));
#80763=CARTESIAN_POINT('Ctrl Pts',(17.1369483247276,-20.3416656668973,-17.4177541356966));
#80764=CARTESIAN_POINT('Ctrl Pts',(17.1320583846019,-20.3360259305138,-17.4182004086209));
#80765=CARTESIAN_POINT('Ctrl Pts',(17.1244905989249,-20.3272039065964,-17.4188987131706));
#80766=CARTESIAN_POINT('Ctrl Pts',(17.1217920767779,-20.3240393246855,-17.4191492477084));
#80767=CARTESIAN_POINT('Ctrl Pts',(17.1167971590114,-20.3181466564993,-17.4196158843617));
#80768=CARTESIAN_POINT('Ctrl Pts',(17.1144983247872,-20.3154207125252,-17.4198318030281));
#80769=CARTESIAN_POINT('Ctrl Pts',(17.1093069350145,-20.3092331392292,-17.4203220269863));
#80770=CARTESIAN_POINT('Ctrl Pts',(17.1064185647059,-20.3057680821503,-17.420596629983));
#80771=CARTESIAN_POINT('Ctrl Pts',(17.0978965642405,-20.2954779001013,-17.4214122749751));
#80772=CARTESIAN_POINT('Ctrl Pts',(17.0922947139665,-20.2886267497324,-17.4219555296657));
#80773=CARTESIAN_POINT('Ctrl Pts',(17.05110318643,-20.2375992746436,-17.4260018982156));
#80774=CARTESIAN_POINT('Ctrl Pts',(17.0172621886901,-20.1920472768033,-17.4296147071732));
#80775=CARTESIAN_POINT('Ctrl Pts',(16.9504045590503,-20.0940631314751,-17.4372973967215));
#80776=CARTESIAN_POINT('Ctrl Pts',(16.9177756663548,-20.0414262112772,-17.4413750699095));
#80777=CARTESIAN_POINT('Ctrl Pts',(16.833894641212,-19.8918409600347,-17.4527032348205));
#80778=CARTESIAN_POINT('Ctrl Pts',(16.7877887117364,-19.7922181179369,-17.4599518152647));
#80779=CARTESIAN_POINT('Ctrl Pts',(16.7481977200789,-19.6856856149317,-17.4672585804267));
#80780=CARTESIAN_POINT('Ctrl Pts',(16.7468031555774,-19.6818999771293,-17.4675176808637));
#80781=CARTESIAN_POINT('Ctrl Pts',(16.745419450228,-19.6781104578977,-17.467776498566));
#80782=CARTESIAN_POINT('',(16.6170006442199,-18.9503484472246,-16.4878149124144));
#80783=CARTESIAN_POINT('Ctrl Pts',(16.7454194498739,-19.6781104569281,-17.2426989690604));
#80784=CARTESIAN_POINT('Ctrl Pts',(16.7608133381091,-19.720269313674,-17.2398827637156));
#80785=CARTESIAN_POINT('Ctrl Pts',(16.7775450772594,-19.761930911878,-17.2371085316352));
#80786=CARTESIAN_POINT('Ctrl Pts',(16.8006203767587,-19.8144898912909,-17.2336175673096));
#80787=CARTESIAN_POINT('Ctrl Pts',(16.8057522414893,-19.8259028392701,-17.2328600420512));
#80788=CARTESIAN_POINT('Ctrl Pts',(16.8140577700572,-19.8439444070767,-17.2316632137377));
#80789=CARTESIAN_POINT('Ctrl Pts',(16.817165214111,-19.8506030254568,-17.2312216439893));
#80790=CARTESIAN_POINT('Ctrl Pts',(16.8230280590925,-19.8629971052561,-17.2303999472867));
#80791=CARTESIAN_POINT('Ctrl Pts',(16.8257747635559,-19.8687365668966,-17.2300195250802));
#80792=CARTESIAN_POINT('Ctrl Pts',(16.8319433148699,-19.8814784057187,-17.2291751312795));
#80793=CARTESIAN_POINT('Ctrl Pts',(16.8353780490435,-19.8884744684066,-17.2287116140876));
#80794=CARTESIAN_POINT('Ctrl Pts',(16.8455036916702,-19.9088142507746,-17.2273642260543));
#80795=CARTESIAN_POINT('Ctrl Pts',(16.8522972775726,-19.9221065397874,-17.2264839527934));
#80796=CARTESIAN_POINT('Ctrl Pts',(16.9092402998089,-20.030671754689,-17.2192939161027));
#80797=CARTESIAN_POINT('Ctrl Pts',(16.9664531715157,-20.122069809812,-17.2132499545465));
#80798=CARTESIAN_POINT('Ctrl Pts',(17.109751978709,-20.3163257349589,-17.1999842959857));
#80799=CARTESIAN_POINT('Ctrl Pts',(17.1991351650164,-20.4161561880625,-17.1928656132533));
#80800=CARTESIAN_POINT('Ctrl Pts',(17.3093860429016,-20.5180247310711,-17.1845197435298));
#80801=CARTESIAN_POINT('Ctrl Pts',(17.3215698782723,-20.5290223577061,-17.1836024659585));
#80802=CARTESIAN_POINT('Ctrl Pts',(17.3736850652844,-20.5749752300406,-17.1796940207168));
#80803=CARTESIAN_POINT('Ctrl Pts',(17.4147922239866,-20.6085612447708,-17.1766482415168));
#80804=CARTESIAN_POINT('Ctrl Pts',(17.4640562984496,-20.6458145583144,-17.1729828814155));
#80805=CARTESIAN_POINT('Ctrl Pts',(17.4710311312166,-20.6510215989395,-17.1724635928918));
#80806=CARTESIAN_POINT('Ctrl Pts',(17.4816439613699,-20.6588431154939,-17.1716725967923));
#80807=CARTESIAN_POINT('Ctrl Pts',(17.4852585715187,-20.6614893718151,-17.1714030440656));
#80808=CARTESIAN_POINT('Ctrl Pts',(17.4917636998961,-20.666220136105,-17.1709176169094));
#80809=CARTESIAN_POINT('Ctrl Pts',(17.4946511041306,-20.6683088341939,-17.1707020374017));
#80810=CARTESIAN_POINT('Ctrl Pts',(17.5009388064773,-20.6728331082946,-17.1702323235958));
#80811=CARTESIAN_POINT('Ctrl Pts',(17.5043410081815,-20.6752658694224,-17.169978007079));
#80812=CARTESIAN_POINT('Ctrl Pts',(17.5139234868172,-20.6820750420492,-17.1692613151904));
#80813=CARTESIAN_POINT('Ctrl Pts',(17.5201199972535,-20.6864283450447,-17.1687974052941));
#80814=CARTESIAN_POINT('Ctrl Pts',(17.5574222943183,-20.7123369299239,-17.1660026228435));
#80815=CARTESIAN_POINT('Ctrl Pts',(17.5890761154363,-20.7330867728352,-17.1636224197635));
#80816=CARTESIAN_POINT('Ctrl Pts',(17.6953529688962,-20.7987499626778,-17.1556463562796));
#80817=CARTESIAN_POINT('Ctrl Pts',(17.7721887097019,-20.8399063014434,-17.149907405615));
#80818=CARTESIAN_POINT('Ctrl Pts',(18.0106979530405,-20.9493141414109,-17.1325699008923));
#80819=CARTESIAN_POINT('Ctrl Pts',(18.1785589325585,-21.0023507636008,-17.1210593388659));
#80820=CARTESIAN_POINT('Ctrl Pts',(18.3736831637739,-21.0382381905442,-17.1088475285528));
#80821=CARTESIAN_POINT('Ctrl Pts',(18.3963709338924,-21.0420298297795,-17.1074434360905));
#80822=CARTESIAN_POINT('Ctrl Pts',(18.4285581431009,-21.0468712202328,-17.1054730705881));
#80823=CARTESIAN_POINT('Ctrl Pts',(18.4380091888165,-21.0482274689719,-17.1048971398273));
#80824=CARTESIAN_POINT('Ctrl Pts',(18.4533813732738,-21.0503273796725,-17.1039645592587));
#80825=CARTESIAN_POINT('Ctrl Pts',(18.459296972004,-21.0511100146233,-17.1036066812973));
#80826=CARTESIAN_POINT('Ctrl Pts',(18.4716873170801,-21.0526959852523,-17.1028591653505));
#80827=CARTESIAN_POINT('Ctrl Pts',(18.4781626357032,-21.0534944231606,-17.1024696857292));
#80828=CARTESIAN_POINT('Ctrl Pts',(18.4935773304073,-21.0553228260666,-17.1015452736181));
#80829=CARTESIAN_POINT('Ctrl Pts',(18.502519832215,-21.0563257605315,-17.1010111984618));
#80830=CARTESIAN_POINT('Ctrl Pts',(18.5326744604026,-21.0595131652074,-17.0992174794108));
#80831=CARTESIAN_POINT('Ctrl Pts',(18.5539135556114,-21.0614341980435,-17.0979661196598));
#80832=CARTESIAN_POINT('Ctrl Pts',(18.6697334727688,-21.0701477840668,-17.0912024154926));
#80833=CARTESIAN_POINT('Ctrl Pts',(18.7646651557298,-21.0709013431714,-17.0858832799327));
#80834=CARTESIAN_POINT('Ctrl Pts',(19.028529215096,-21.0552518385551,-17.0713393476969));
#80835=CARTESIAN_POINT('Ctrl Pts',(19.1958840140949,-21.024936900985,-17.0624206444878));
#80836=CARTESIAN_POINT('Ctrl Pts',(19.3943175094104,-20.963747711953,-17.0505774117002));
#80837=CARTESIAN_POINT('Ctrl Pts',(19.4305054318287,-20.9515069006588,-17.0483610129389));
#80838=CARTESIAN_POINT('Ctrl Pts',(19.4731203919463,-20.9357949167947,-17.0456612832462));
#80839=CARTESIAN_POINT('Ctrl Pts',(19.4798879872012,-20.9332602890218,-17.0452298166369));
#80840=CARTESIAN_POINT('Ctrl Pts',(19.4908840459019,-20.9290776757838,-17.0445241115834));
#80841=CARTESIAN_POINT('Ctrl Pts',(19.4951204853496,-20.9274506323682,-17.0442510958433));
#80842=CARTESIAN_POINT('Ctrl Pts',(19.5026783434633,-20.9245200468903,-17.0437619570049));
#80843=CARTESIAN_POINT('Ctrl Pts',(19.5060017278716,-20.9232217183765,-17.0435461485296));
#80844=CARTESIAN_POINT('Ctrl Pts',(19.513173647039,-20.9203989845235,-17.0430788559055));
#80845=CARTESIAN_POINT('Ctrl Pts',(19.5170209436177,-20.9188717130743,-17.0428272053239));
#80846=CARTESIAN_POINT('Ctrl Pts',(19.5277103026619,-20.9145919967092,-17.042125347873));
#80847=CARTESIAN_POINT('Ctrl Pts',(19.5345424211642,-20.9118150979959,-17.0416737047906));
#80848=CARTESIAN_POINT('Ctrl Pts',(19.5733080544851,-20.8958223686678,-17.0390942672009));
#80849=CARTESIAN_POINT('Ctrl Pts',(19.604926719919,-20.881862622319,-17.0369254057522));
#80850=CARTESIAN_POINT('Ctrl Pts',(19.7038743504449,-20.8352501164384,-17.0299622041732));
#80851=CARTESIAN_POINT('Ctrl Pts',(19.7698188607241,-20.7998000452166,-17.0250595697919));
#80852=CARTESIAN_POINT('Ctrl Pts',(19.9994199025862,-20.6602140366031,-17.0073366904222));
#80853=CARTESIAN_POINT('Ctrl Pts',(20.1505147734033,-20.5371814167816,-16.9945245030053));
#80854=CARTESIAN_POINT('Ctrl Pts',(20.2971798395324,-20.3797973900105,-16.9813073144602));
#80855=CARTESIAN_POINT('Ctrl Pts',(20.3113709528804,-20.3641039358507,-16.9800173556114));
#80856=CARTESIAN_POINT('Ctrl Pts',(20.3308017985663,-20.3419575462654,-16.9782348656409));
#80857=CARTESIAN_POINT('Ctrl Pts',(20.3362420327966,-20.3356829245671,-16.9777339751764));
#80858=CARTESIAN_POINT('Ctrl Pts',(20.3455734683754,-20.3247914656884,-16.9768715754523));
#80859=CARTESIAN_POINT('Ctrl Pts',(20.3494820702649,-20.3201897288262,-16.9765093486441));
#80860=CARTESIAN_POINT('Ctrl Pts',(20.357539689041,-20.3106205380405,-16.9757605045732));
#80861=CARTESIAN_POINT('Ctrl Pts',(20.3616857239668,-20.3056506468461,-16.9753740118534));
#80862=CARTESIAN_POINT('Ctrl Pts',(20.3713500024069,-20.2939573845309,-16.9744702903082));
#80863=CARTESIAN_POINT('Ctrl Pts',(20.3768497578128,-20.2872188318682,-16.973953815822));
#80864=CARTESIAN_POINT('Ctrl Pts',(20.3946060463662,-20.2651872102885,-16.9722790123744));
#80865=CARTESIAN_POINT('Ctrl Pts',(20.406692005351,-20.249757521216,-16.9711275213006));
#80866=CARTESIAN_POINT('Ctrl Pts',(20.4676142374132,-20.1697151343637,-16.965259176585));
#80867=CARTESIAN_POINT('Ctrl Pts',(20.5129305547886,-20.1025027703689,-16.9606809236321));
#80868=CARTESIAN_POINT('Ctrl Pts',(20.6403754894141,-19.8878699686321,-16.946845481282));
#80869=CARTESIAN_POINT('Ctrl Pts',(20.7088263484278,-19.7331358983087,-16.9379734116954));
#80870=CARTESIAN_POINT('Ctrl Pts',(20.7740118195889,-19.5202936294107,-16.9254615545825));
#80871=CARTESIAN_POINT('Ctrl Pts',(20.7878439982756,-19.4680713616,-16.9223639644062));
#80872=CARTESIAN_POINT('Ctrl Pts',(20.8015776565788,-19.4068495453228,-16.9186407751822));
#80873=CARTESIAN_POINT('Ctrl Pts',(20.8034388880319,-19.3983050051234,-16.9181190839369));
#80874=CARTESIAN_POINT('Ctrl Pts',(20.8061752264278,-19.3853577945994,-16.9173251402454));
#80875=CARTESIAN_POINT('Ctrl Pts',(20.8070893834219,-19.3809633488445,-16.917055066754));
#80876=CARTESIAN_POINT('Ctrl Pts',(20.8087043779408,-19.3730741604594,-16.9165690857206));
#80877=CARTESIAN_POINT('Ctrl Pts',(20.809410370695,-19.3695805280093,-16.9163534760681));
#80878=CARTESIAN_POINT('Ctrl Pts',(20.8109243312331,-19.3619899506241,-16.9158841457757));
#80879=CARTESIAN_POINT('Ctrl Pts',(20.8117289904723,-19.3578924472523,-16.9156302453674));
#80880=CARTESIAN_POINT('Ctrl Pts',(20.8139529194793,-19.3463877955289,-16.9149158755395));
#80881=CARTESIAN_POINT('Ctrl Pts',(20.8153447206003,-19.3389754909675,-16.9144538871779));
#80882=CARTESIAN_POINT('Ctrl Pts',(20.8233854198353,-19.2948546302163,-16.9116943315946));
#80883=CARTESIAN_POINT('Ctrl Pts',(20.8291022163494,-19.2579853568534,-16.909348839196));
#80884=CARTESIAN_POINT('Ctrl Pts',(20.8446390631089,-19.1366973034976,-16.9015453574746));
#80885=CARTESIAN_POINT('Ctrl Pts',(20.850350781311,-19.0518391556437,-16.8959504851851));
#80886=CARTESIAN_POINT('Ctrl Pts',(20.8522009215649,-18.7885117643345,-16.8785545586206));
#80887=CARTESIAN_POINT('Ctrl Pts',(20.8309074044943,-18.6106680750795,-16.8668318577111));
#80888=CARTESIAN_POINT('Ctrl Pts',(20.7820171741914,-18.4154994476065,-16.8544504481824));
#80889=CARTESIAN_POINT('Ctrl Pts',(20.7761297522396,-18.3935079884013,-16.8530610021513));
#80890=CARTESIAN_POINT('Ctrl Pts',(20.767281718803,-18.3624706382347,-16.8511074365896));
#80891=CARTESIAN_POINT('Ctrl Pts',(20.764613238919,-18.3533437589543,-16.8505338812383));
#80892=CARTESIAN_POINT('Ctrl Pts',(20.7601722662553,-18.3385259014823,-16.8496040959525));
#80893=CARTESIAN_POINT('Ctrl Pts',(20.7584370954151,-18.332823958853,-16.8492466524165));
#80894=CARTESIAN_POINT('Ctrl Pts',(20.7547502605002,-18.3208898415695,-16.8484992092437));
#80895=CARTESIAN_POINT('Ctrl Pts',(20.752793789441,-18.3146592084495,-16.8481093716364));
#80896=CARTESIAN_POINT('Ctrl Pts',(20.7480626355886,-18.2998326237891,-16.8471825892301));
#80897=CARTESIAN_POINT('Ctrl Pts',(20.7452616936003,-18.2912451359431,-16.8466465136296));
#80898=CARTESIAN_POINT('Ctrl Pts',(20.735599876556,-18.2622534336926,-16.8448389090109));
#80899=CARTESIAN_POINT('Ctrl Pts',(20.7284826382223,-18.2419356031438,-16.843575842695));
#80900=CARTESIAN_POINT('Ctrl Pts',(20.6587625341826,-18.052228159565,-16.8318084486334));
#80901=CARTESIAN_POINT('Ctrl Pts',(20.5750396925942,-17.8913964400097,-16.8221122767492));
#80902=CARTESIAN_POINT('Ctrl Pts',(20.4037872425938,-17.6451980469061,-16.8057870189803));
#80903=CARTESIAN_POINT('Ctrl Pts',(20.3275183156282,-17.5532105615416,-16.7992370027396));
#80904=CARTESIAN_POINT('Ctrl Pts',(20.2372586948839,-17.4613649868366,-16.7916053244576));
#80905=CARTESIAN_POINT('Ctrl Pts',(20.2305472092367,-17.4546270040145,-16.7910384557641));
#80906=CARTESIAN_POINT('Ctrl Pts',(20.22053426422,-17.4447090892447,-16.7901932030767));
#80907=CARTESIAN_POINT('Ctrl Pts',(20.2172674023483,-17.4414941838675,-16.7899175001571));
#80908=CARTESIAN_POINT('Ctrl Pts',(20.2114360080532,-17.435792691584,-16.7894254381044));
#80909=CARTESIAN_POINT('Ctrl Pts',(20.2088755971124,-17.4333019612841,-16.7892094088383));
#80910=CARTESIAN_POINT('Ctrl Pts',(20.2033567500202,-17.4279604270036,-16.7887437993385));
#80911=CARTESIAN_POINT('Ctrl Pts',(20.2003963590415,-17.4251117930851,-16.7884940641518));
#80912=CARTESIAN_POINT('Ctrl Pts',(20.1922007241211,-17.4172713678801,-16.7878028062736));
#80913=CARTESIAN_POINT('Ctrl Pts',(20.1869482155621,-17.4122978192224,-16.7873599158284));
#80914=CARTESIAN_POINT('Ctrl Pts',(20.1580142745287,-17.3851804480279,-16.7849214477747));
#80915=CARTESIAN_POINT('Ctrl Pts',(20.133853401822,-17.3635572564836,-16.7828897892502));
#80916=CARTESIAN_POINT('Ctrl Pts',(19.98543406416,-17.2367432253775,-16.7704862553441));
#80917=CARTESIAN_POINT('Ctrl Pts',(19.8498790234841,-17.1456204884811,-16.7595226115642));
#80918=CARTESIAN_POINT('Ctrl Pts',(19.6013627714859,-17.0173079933107,-16.7412534803143));
#80919=CARTESIAN_POINT('Ctrl Pts',(19.4932278867572,-16.9723706974251,-16.7338079034804));
#80920=CARTESIAN_POINT('Ctrl Pts',(19.3683385792524,-16.9322210383114,-16.7257980479885));
#80921=CARTESIAN_POINT('Ctrl Pts',(19.3547141709729,-16.9279924849947,-16.724931577184));
#80922=CARTESIAN_POINT('Ctrl Pts',(19.3329551158053,-16.9214795917772,-16.7235591940653));
#80923=CARTESIAN_POINT('Ctrl Pts',(19.3248479202649,-16.9191057338591,-16.7230503664338));
#80924=CARTESIAN_POINT('Ctrl Pts',(19.3105204631249,-16.9150034782016,-16.7221554918337));
#80925=CARTESIAN_POINT('Ctrl Pts',(19.3043061381691,-16.9132548995965,-16.7217687910603));
#80926=CARTESIAN_POINT('Ctrl Pts',(19.2914323989594,-16.9096959717912,-16.7209706256762));
#80927=CARTESIAN_POINT('Ctrl Pts',(19.284771928854,-16.9078897027881,-16.7205592976642));
#80928=CARTESIAN_POINT('Ctrl Pts',(19.2676444147524,-16.9033346417586,-16.719505645151));
#80929=CARTESIAN_POINT('Ctrl Pts',(19.2571648286956,-16.900633460336,-16.7188648673748));
#80930=CARTESIAN_POINT('Ctrl Pts',(19.2132695484185,-16.8896774203105,-16.7161967173036));
#80931=CARTESIAN_POINT('Ctrl Pts',(19.1796746584067,-16.882157489057,-16.7141930430451));
#80932=CARTESIAN_POINT('Ctrl Pts',(19.0916091003971,-16.8646884938097,-16.7090282793365));
#80933=CARTESIAN_POINT('Ctrl Pts',(19.0369042807986,-16.8560507539028,-16.7059069956425));
#80934=CARTESIAN_POINT('Ctrl Pts',(18.8731176615586,-16.8367369042163,-16.6967386492996));
#80935=CARTESIAN_POINT('Ctrl Pts',(18.763479979485,-16.8323718538326,-16.6908402341054));
#80936=CARTESIAN_POINT('Ctrl Pts',(18.5938601737218,-16.8387864509178,-16.6815976616243));
#80937=CARTESIAN_POINT('Ctrl Pts',(18.5338497145011,-16.8436238732439,-16.6783024020314));
#80938=CARTESIAN_POINT('Ctrl Pts',(18.4161592016012,-16.8581809452183,-16.6716603173663));
#80939=CARTESIAN_POINT('Ctrl Pts',(18.3585155632465,-16.8677468619627,-16.6683205330776));
#80940=CARTESIAN_POINT('Ctrl Pts',(18.292624137677,-16.8815035010199,-16.6643275489039));
#80941=CARTESIAN_POINT('Ctrl Pts',(18.2839130739329,-16.8833796489422,-16.6637960873633));
#80942=CARTESIAN_POINT('Ctrl Pts',(18.2707977188182,-16.8862911352157,-16.6629901673629));
#80943=CARTESIAN_POINT('Ctrl Pts',(18.2663843508655,-16.8872857168237,-16.6627179871656));
#80944=CARTESIAN_POINT('Ctrl Pts',(18.2584971197321,-16.8890897416922,-16.6622297498418));
#80945=CARTESIAN_POINT('Ctrl Pts',(18.2550220843796,-16.8898938244951,-16.6620140025918));
#80946=CARTESIAN_POINT('Ctrl Pts',(18.2475087902232,-16.8916523301257,-16.6615461528995));
#80947=CARTESIAN_POINT('Ctrl Pts',(18.2434713563658,-16.8926098312757,-16.6612938803223));
#80948=CARTESIAN_POINT('Ctrl Pts',(18.2322211407829,-16.895312846393,-16.6605885706356));
#80949=CARTESIAN_POINT('Ctrl Pts',(18.2250147656582,-16.8970844059083,-16.6601340746958));
#80950=CARTESIAN_POINT('Ctrl Pts',(18.1835905623223,-16.9074990785256,-16.6575065042065));
#80951=CARTESIAN_POINT('Ctrl Pts',(18.1495859426044,-16.9169583693435,-16.655290583589));
#80952=CARTESIAN_POINT('Ctrl Pts',(18.0417718274778,-16.9498746348247,-16.6481093977352));
#80953=CARTESIAN_POINT('Ctrl Pts',(17.9690089488369,-16.9765322364171,-16.6430286910299));
#80954=CARTESIAN_POINT('Ctrl Pts',(17.727659407066,-17.0802906230617,-16.6256920557288));
#80955=CARTESIAN_POINT('Ctrl Pts',(17.567747693774,-17.1755147528589,-16.6134598082781));
#80956=CARTESIAN_POINT('Ctrl Pts',(17.4027686880646,-17.3057530074339,-16.6004987701282));
#80957=CARTESIAN_POINT('Ctrl Pts',(17.3835444186322,-17.3214860406576,-16.5989806449776));
#80958=CARTESIAN_POINT('Ctrl Pts',(17.357083333934,-17.3439307643588,-16.5968791102854));
#80959=CARTESIAN_POINT('Ctrl Pts',(17.3496103738568,-17.3503597344983,-16.5962842401266));
#80960=CARTESIAN_POINT('Ctrl Pts',(17.3376431755914,-17.3608014230724,-16.595329306469));
#80961=CARTESIAN_POINT('Ctrl Pts',(17.3331207510334,-17.3647814821929,-16.5949678968203));
#80962=CARTESIAN_POINT('Ctrl Pts',(17.3240615457209,-17.3728231155704,-16.5942428137148));
#80963=CARTESIAN_POINT('Ctrl Pts',(17.3195251758366,-17.3768850676299,-16.5938791611097));
#80964=CARTESIAN_POINT('Ctrl Pts',(17.3088168713055,-17.3865570553455,-16.5930193487606));
#80965=CARTESIAN_POINT('Ctrl Pts',(17.3026604104845,-17.3921841308002,-16.5925239142729));
#80966=CARTESIAN_POINT('Ctrl Pts',(17.2835121501476,-17.4098946901846,-16.5909793473806));
#80967=CARTESIAN_POINT('Ctrl Pts',(17.2706386846395,-17.4221054028918,-16.5899356515955));
#80968=CARTESIAN_POINT('Ctrl Pts',(17.2410243399071,-17.4509109877491,-16.5875210324327));
#80969=CARTESIAN_POINT('Ctrl Pts',(17.2244039201489,-17.4676266364197,-16.5861553944354));
#80970=CARTESIAN_POINT('Ctrl Pts',(17.1679676918297,-17.5263147711664,-16.5814760427944));
#80971=CARTESIAN_POINT('Ctrl Pts',(17.1295938981425,-17.5696406574505,-16.5782202756028));
#80972=CARTESIAN_POINT('Ctrl Pts',(16.9903283854136,-17.7405017733826,-16.5659901996405));
#80973=CARTESIAN_POINT('Ctrl Pts',(16.9024811696542,-17.877918134153,-16.5574141688273));
#80974=CARTESIAN_POINT('Ctrl Pts',(16.8041932721513,-18.0794530417435,-16.5448862244106));
#80975=CARTESIAN_POINT('Ctrl Pts',(16.7795980725527,-18.1360319846932,-16.5413681963752));
#80976=CARTESIAN_POINT('Ctrl Pts',(16.7542382247236,-18.202122879313,-16.5371698402641));
#80977=CARTESIAN_POINT('Ctrl Pts',(16.7510222061416,-18.2106691391418,-16.5366252730384));
#80978=CARTESIAN_POINT('Ctrl Pts',(16.7463011558343,-18.2234654228872,-16.5358070208537));
#80979=CARTESIAN_POINT('Ctrl Pts',(16.7447542002184,-18.2277000121953,-16.5355357742192));
#80980=CARTESIAN_POINT('Ctrl Pts',(16.7420079791541,-18.2352925957539,-16.5350485397713));
#80981=CARTESIAN_POINT('Ctrl Pts',(16.740803661073,-18.2386487060184,-16.5348328565262));
#80982=CARTESIAN_POINT('Ctrl Pts',(16.7382123271679,-18.2459278517811,-16.5343643644504));
#80983=CARTESIAN_POINT('Ctrl Pts',(16.7368284154959,-18.2498518853688,-16.53411138127));
#80984=CARTESIAN_POINT('Ctrl Pts',(16.7329911455468,-18.2608354603816,-16.5334021211097));
#80985=CARTESIAN_POINT('Ctrl Pts',(16.7305636178113,-18.2679038699715,-16.5329443592239));
#80986=CARTESIAN_POINT('Ctrl Pts',(16.7166116786433,-18.3092399734625,-16.5302602773391));
#80987=CARTESIAN_POINT('Ctrl Pts',(16.7059299249571,-18.3437833444819,-16.527988972574));
#80988=CARTESIAN_POINT('Ctrl Pts',(16.6743068167818,-18.4561679762689,-16.5205458836166));
#80989=CARTESIAN_POINT('Ctrl Pts',(16.6569252794185,-18.5349337236618,-16.5152498176493));
#80990=CARTESIAN_POINT('Ctrl Pts',(16.6261433829434,-18.725542196976,-16.5025015877908));
#80991=CARTESIAN_POINT('Ctrl Pts',(16.6170884083753,-18.8378502798878,-16.4950530971665));
#80992=CARTESIAN_POINT('Ctrl Pts',(16.6170006442199,-18.9503484472246,-16.4878149124144));
#80993=CARTESIAN_POINT('Ctrl Pts',(16.6170006421844,-18.950351058477,-16.4878147444052));
#80994=CARTESIAN_POINT('Ctrl Pts',(16.6169350225851,-19.0345970111522,-16.4823943227854));
#80995=CARTESIAN_POINT('Ctrl Pts',(16.6218981987577,-19.1187818305546,-16.4770994274566));
#80996=CARTESIAN_POINT('Ctrl Pts',(16.6330988071922,-19.2127900135317,-16.4713270383168));
#80997=CARTESIAN_POINT('Ctrl Pts',(16.6344059067415,-19.2231123433587,-16.470695060677));
#80998=CARTESIAN_POINT('Ctrl Pts',(16.6367383502125,-19.2405022784468,-16.4696333962698));
#80999=CARTESIAN_POINT('Ctrl Pts',(16.6377234421186,-19.2475750110736,-16.4692024471379));
#81000=CARTESIAN_POINT('Ctrl Pts',(16.6396009381099,-19.2605732900813,-16.4684119641199));
#81001=CARTESIAN_POINT('Ctrl Pts',(16.640482747474,-19.2665002707839,-16.4680520988851));
#81002=CARTESIAN_POINT('Ctrl Pts',(16.6423536700532,-19.27871882569,-16.4673114013629));
#81003=CARTESIAN_POINT('Ctrl Pts',(16.6433460343191,-19.2850098463914,-16.4669306761883));
#81004=CARTESIAN_POINT('Ctrl Pts',(16.6456303028236,-19.2990780301301,-16.4660806799525));
#81005=CARTESIAN_POINT('Ctrl Pts',(16.6469372952717,-19.306852673919,-16.4656118929438));
#81006=CARTESIAN_POINT('Ctrl Pts',(16.6503588008292,-19.3265324429957,-16.4644275862324));
#81007=CARTESIAN_POINT('Ctrl Pts',(16.6525319517493,-19.3384271871218,-16.4637139331016));
#81008=CARTESIAN_POINT('Ctrl Pts',(16.6655166180058,-19.4062088468947,-16.4596586362792));
#81009=CARTESIAN_POINT('Ctrl Pts',(16.6784773407092,-19.461663229567,-16.4563861926103));
#81010=CARTESIAN_POINT('Ctrl Pts',(16.7044778887797,-19.5556349278304,-16.4508783781244));
#81011=CARTESIAN_POINT('Ctrl Pts',(16.71641941116,-19.5944203584224,-16.4486161291037));
#81012=CARTESIAN_POINT('Ctrl Pts',(16.7346157472973,-19.6479940728282,-16.4454900620391));
#81013=CARTESIAN_POINT('Ctrl Pts',(16.7399331058666,-19.663085142709,-16.4446093145535));
#81014=CARTESIAN_POINT('Ctrl Pts',(16.7454194329591,-19.6781104106039,-16.4437313840672));
#81015=CARTESIAN_POINT('Origin',(18.734,-18.952,0.));
#81016=CARTESIAN_POINT('',(16.7454194499637,-19.6781104571738,-15.6464962048466));
#81017=CARTESIAN_POINT('',(16.7454194501832,-19.6781104577752,-15.8662164286365));
#81018=CARTESIAN_POINT('',(16.7454194499637,-19.6781104571739,0.));
#81019=CARTESIAN_POINT('Ctrl Pts',(16.7454194501833,-19.6781104577752,-15.8662164286365));
#81020=CARTESIAN_POINT('Ctrl Pts',(16.7372703347662,-19.6557926792016,-15.8675066642955));
#81021=CARTESIAN_POINT('Ctrl Pts',(16.7294937152069,-19.6333289218962,-15.8687972040221));
#81022=CARTESIAN_POINT('Ctrl Pts',(16.6950140071841,-19.5280200481297,-15.8748264318793));
#81023=CARTESIAN_POINT('Ctrl Pts',(16.6730620557294,-19.4437269241824,-15.8795907813764));
#81024=CARTESIAN_POINT('Ctrl Pts',(16.6490998720476,-19.3212039000817,-15.8867186533905));
#81025=CARTESIAN_POINT('Ctrl Pts',(16.6428359557392,-19.283892458455,-15.8889160472875));
#81026=CARTESIAN_POINT('Ctrl Pts',(16.6365221775586,-19.2389374853729,-15.8916169963615));
#81027=CARTESIAN_POINT('Ctrl Pts',(16.6355092983807,-19.2314335474448,-15.8920696192867));
#81028=CARTESIAN_POINT('Ctrl Pts',(16.633999500955,-19.2197767652956,-15.8927757145532));
#81029=CARTESIAN_POINT('Ctrl Pts',(16.6334745846423,-19.2156275227724,-15.893027635281));
#81030=CARTESIAN_POINT('Ctrl Pts',(16.632525166272,-19.2079398830612,-15.8934955182764));
#81031=CARTESIAN_POINT('Ctrl Pts',(16.6320973022205,-19.2044019592219,-15.893711288639));
#81032=CARTESIAN_POINT('Ctrl Pts',(16.6311517265553,-19.1964140123727,-15.8941994589649));
#81033=CARTESIAN_POINT('Ctrl Pts',(16.630639209231,-19.1919634421649,-15.8944721459476));
#81034=CARTESIAN_POINT('Ctrl Pts',(16.6291723812961,-19.1788600409237,-15.8952769781407));
#81035=CARTESIAN_POINT('Ctrl Pts',(16.6282573251611,-19.170203033916,-15.8958112514642));
#81036=CARTESIAN_POINT('Ctrl Pts',(16.6221408153505,-19.1087111158599,-15.8996231482018));
#81037=CARTESIAN_POINT('Ctrl Pts',(16.6188755553666,-19.0557070404166,-15.9029969230022));
#81038=CARTESIAN_POINT('Ctrl Pts',(16.6172125016367,-18.9862051693057,-15.9074892857674));
#81039=CARTESIAN_POINT('Ctrl Pts',(16.6170107020019,-18.9697651382934,-15.9085569565694));
#81040=CARTESIAN_POINT('Ctrl Pts',(16.6169886661743,-18.9345501864226,-15.910852690008));
#81041=CARTESIAN_POINT('Ctrl Pts',(16.6172266707935,-18.9157766073064,-15.9120819059916));
#81042=CARTESIAN_POINT('Ctrl Pts',(16.6217705414464,-18.7409093396794,-15.9235687458873));
#81043=CARTESIAN_POINT('Ctrl Pts',(16.6430867211467,-18.5857152159715,-15.9339904918105));
#81044=CARTESIAN_POINT('Ctrl Pts',(16.6824568347016,-18.4296182623915,-15.9442508982956));
#81045=CARTESIAN_POINT('Ctrl Pts',(16.6836465121877,-18.4249681087383,-15.9445563983091));
#81046=CARTESIAN_POINT('Ctrl Pts',(16.7007571342291,-18.359021806834,-15.9488865474276));
#81047=CARTESIAN_POINT('Ctrl Pts',(16.7194060610022,-18.2984617249976,-15.9528331782942));
#81048=CARTESIAN_POINT('Ctrl Pts',(16.7449593097039,-18.2270429779827,-15.9574536825387));
#81049=CARTESIAN_POINT('Ctrl Pts',(16.7492788043921,-18.2152996961582,-15.9582123647703));
#81050=CARTESIAN_POINT('Ctrl Pts',(16.7565350599576,-18.1960994629787,-15.9594512257848));
#81051=CARTESIAN_POINT('Ctrl Pts',(16.7594104544035,-18.1886197931944,-15.9599334418581));
#81052=CARTESIAN_POINT('Ctrl Pts',(16.7646512969167,-18.1752147095066,-15.9607970148743));
#81053=CARTESIAN_POINT('Ctrl Pts',(16.7670011814372,-18.1692833520257,-15.9611788887989));
#81054=CARTESIAN_POINT('Ctrl Pts',(16.772057444012,-18.1566873908091,-15.9619893893467));
#81055=CARTESIAN_POINT('Ctrl Pts',(16.7747710537981,-18.1500257624715,-15.9624177663289));
#81056=CARTESIAN_POINT('Ctrl Pts',(16.7821563599653,-18.1321568264676,-15.9635661745951));
#81057=CARTESIAN_POINT('Ctrl Pts',(16.7868906525702,-18.1209755582761,-15.9642840786211));
#81058=CARTESIAN_POINT('Ctrl Pts',(16.8108464004613,-18.0657265600386,-15.9678287044714));
#81059=CARTESIAN_POINT('Ctrl Pts',(16.8314697893408,-18.0222797762008,-15.9706071483523));
#81060=CARTESIAN_POINT('Ctrl Pts',(16.9305680820079,-17.8306476235727,-15.9828818136258));
#81061=CARTESIAN_POINT('Ctrl Pts',(17.0249942527189,-17.6914054106297,-15.9918000628666));
#81062=CARTESIAN_POINT('Ctrl Pts',(17.1995488648122,-17.4901881659197,-16.0063839563767));
#81063=CARTESIAN_POINT('Ctrl Pts',(17.2693656376801,-17.4202444105187,-16.0118767114489));
#81064=CARTESIAN_POINT('Ctrl Pts',(17.3511068420273,-17.3490684642471,-16.0182979722239));
#81065=CARTESIAN_POINT('Ctrl Pts',(17.3584620171353,-17.3427522737928,-16.0188757105727));
#81066=CARTESIAN_POINT('Ctrl Pts',(17.3693853966609,-17.3335015216189,-16.0197340934665));
#81067=CARTESIAN_POINT('Ctrl Pts',(17.3729203594835,-17.3305276593748,-16.0200119346769));
#81068=CARTESIAN_POINT('Ctrl Pts',(17.3792087461223,-17.3252724738799,-16.0205063471644));
#81069=CARTESIAN_POINT('Ctrl Pts',(17.3819582459784,-17.3229865313653,-16.0207225764601));
#81070=CARTESIAN_POINT('Ctrl Pts',(17.3878614410547,-17.3181038379143,-16.0211869573383));
#81071=CARTESIAN_POINT('Ctrl Pts',(17.3910168173919,-17.3155092854105,-16.021435255173));
#81072=CARTESIAN_POINT('Ctrl Pts',(17.399698555727,-17.3084126230133,-16.0221185876823));
#81073=CARTESIAN_POINT('Ctrl Pts',(17.4052401183606,-17.3039293147464,-16.022554939886));
#81074=CARTESIAN_POINT('Ctrl Pts',(17.4349422076825,-17.2801465205998,-16.0248942040046));
#81075=CARTESIAN_POINT('Ctrl Pts',(17.4594994307903,-17.2613512280133,-16.0268298884726));
#81076=CARTESIAN_POINT('Ctrl Pts',(17.5350662537209,-17.2060969594658,-16.0327692589338));
#81077=CARTESIAN_POINT('Ctrl Pts',(17.5872900996043,-17.1713611088715,-16.0368503751244));
#81078=CARTESIAN_POINT('Ctrl Pts',(17.7561738710654,-17.0695442561145,-16.0498093953593));
#81079=CARTESIAN_POINT('Ctrl Pts',(17.8777424301249,-17.011223934353,-16.0587750487683));
#81080=CARTESIAN_POINT('Ctrl Pts',(18.0423576790512,-16.95075353411,-16.0700684998409));
#81081=CARTESIAN_POINT('Ctrl Pts',(18.081089600638,-16.9377843096704,-16.0726704465894));
#81082=CARTESIAN_POINT('Ctrl Pts',(18.1665838574833,-16.911882489028,-16.0782894208243));
#81083=CARTESIAN_POINT('Ctrl Pts',(18.2134654252641,-16.8994199410769,-16.0812910304164));
#81084=CARTESIAN_POINT('Ctrl Pts',(18.2730119884972,-16.8857624391251,-16.0850068970682));
#81085=CARTESIAN_POINT('Ctrl Pts',(18.2853121758558,-16.8830565856138,-16.0857693651917));
#81086=CARTESIAN_POINT('Ctrl Pts',(18.3048443099977,-16.8789421958838,-16.0869722355475));
#81087=CARTESIAN_POINT('Ctrl Pts',(18.3120605770515,-16.8774614028735,-16.0874149431685));
#81088=CARTESIAN_POINT('Ctrl Pts',(18.3255227051634,-16.8747720953552,-16.0882377081858));
#81089=CARTESIAN_POINT('Ctrl Pts',(18.3317665494526,-16.8735540130042,-16.0886180672727));
#81090=CARTESIAN_POINT('Ctrl Pts',(18.3456487778405,-16.8709106933413,-16.0894610129257));
#81091=CARTESIAN_POINT('Ctrl Pts',(18.353289733302,-16.8694993230886,-16.0899231528547));
#81092=CARTESIAN_POINT('Ctrl Pts',(18.3755207956689,-16.8655194411239,-16.0912625317377));
#81093=CARTESIAN_POINT('Ctrl Pts',(18.3901304948097,-16.8630619342365,-16.092136239277));
#81094=CARTESIAN_POINT('Ctrl Pts',(18.5067618096874,-16.8447000700295,-16.0990618643436));
#81095=CARTESIAN_POINT('Ctrl Pts',(18.609803334359,-16.8361244369894,-16.1048707542409));
#81096=CARTESIAN_POINT('Ctrl Pts',(18.8727086928598,-16.8335251595991,-16.119346090252));
#81097=CARTESIAN_POINT('Ctrl Pts',(19.031997284835,-16.8500091641537,-16.1277744505008));
#81098=CARTESIAN_POINT('Ctrl Pts',(19.2353144808817,-16.8946403690136,-16.139529537776));
#81099=CARTESIAN_POINT('Ctrl Pts',(19.2823470765735,-16.9066737288974,-16.1423243045287));
#81100=CARTESIAN_POINT('Ctrl Pts',(19.3363662797182,-16.9224916708742,-16.1456660154322));
#81101=CARTESIAN_POINT('Ctrl Pts',(19.3437998689047,-16.9247128203816,-16.1461288035218));
#81102=CARTESIAN_POINT('Ctrl Pts',(19.3556666774905,-16.9283297841018,-16.1468725362401));
#81103=CARTESIAN_POINT('Ctrl Pts',(19.3601078802106,-16.9296994481504,-16.1471519938138));
#81104=CARTESIAN_POINT('Ctrl Pts',(19.3679699583758,-16.9321524889215,-16.1476487385434));
#81105=CARTESIAN_POINT('Ctrl Pts',(19.3713926319858,-16.9332299515151,-16.1478656771871));
#81106=CARTESIAN_POINT('Ctrl Pts',(19.3786461699568,-16.9355336615265,-16.1483269039742));
#81107=CARTESIAN_POINT('Ctrl Pts',(19.382476223875,-16.9367621070747,-16.1485713144113));
#81108=CARTESIAN_POINT('Ctrl Pts',(19.3928139944947,-16.9401103497302,-16.1492333172739));
#81109=CARTESIAN_POINT('Ctrl Pts',(19.3993149046837,-16.9422507820992,-16.1496520960965));
#81110=CARTESIAN_POINT('Ctrl Pts',(19.4316547552038,-16.9530728211618,-16.1517473431767));
#81111=CARTESIAN_POINT('Ctrl Pts',(19.4573334247137,-16.9622209627075,-16.1534491484479));
#81112=CARTESIAN_POINT('Ctrl Pts',(19.53124858766,-16.9901733847922,-16.1584445562623));
#81113=CARTESIAN_POINT('Ctrl Pts',(19.5789792332993,-17.0102537877554,-16.1617913664516));
#81114=CARTESIAN_POINT('Ctrl Pts',(19.7513269543476,-17.0903192847404,-16.174213526663));
#81115=CARTESIAN_POINT('Ctrl Pts',(19.8707327340156,-17.1607289522861,-16.1834600987806));
#81116=CARTESIAN_POINT('Ctrl Pts',(20.0600479526787,-17.2989648119022,-16.1986383744613));
#81117=CARTESIAN_POINT('Ctrl Pts',(20.133735067057,-17.3608762734982,-16.2047110354426));
#81118=CARTESIAN_POINT('Ctrl Pts',(20.2129592962322,-17.4372191776249,-16.2114253125287));
#81119=CARTESIAN_POINT('Ctrl Pts',(20.2228563068343,-17.4469456980767,-16.2122678406753));
#81120=CARTESIAN_POINT('Ctrl Pts',(20.238543465594,-17.4626688023455,-16.21360955599));
#81121=CARTESIAN_POINT('Ctrl Pts',(20.2443949460963,-17.4686033685904,-16.2141114590476));
#81122=CARTESIAN_POINT('Ctrl Pts',(20.2547039919481,-17.4791830354241,-16.2149983141814));
#81123=CARTESIAN_POINT('Ctrl Pts',(20.2591756726663,-17.483814176885,-16.2153838830514));
#81124=CARTESIAN_POINT('Ctrl Pts',(20.2684305113066,-17.4934869556387,-16.2161837635302));
#81125=CARTESIAN_POINT('Ctrl Pts',(20.2732101141948,-17.4985318989633,-16.21659791847));
#81126=CARTESIAN_POINT('Ctrl Pts',(20.2855195228238,-17.5116534802965,-16.2176673646747));
#81127=CARTESIAN_POINT('Ctrl Pts',(20.2930111963687,-17.5197657233853,-16.2183210173688));
#81128=CARTESIAN_POINT('Ctrl Pts',(20.3249207388038,-17.554865528277,-16.2211176600265));
#81129=CARTESIAN_POINT('Ctrl Pts',(20.3487048042152,-17.5824226353241,-16.2232339409861));
#81130=CARTESIAN_POINT('Ctrl Pts',(20.4096658827529,-17.6568513174003,-16.2287590731736));
#81131=CARTESIAN_POINT('Ctrl Pts',(20.4455879951238,-17.7047095012102,-16.2321204281713));
#81132=CARTESIAN_POINT('Ctrl Pts',(20.5743802826088,-17.892358956618,-16.2447295055551));
#81133=CARTESIAN_POINT('Ctrl Pts',(20.6525336174655,-18.0414727667594,-16.2535601340439));
#81134=CARTESIAN_POINT('Ctrl Pts',(20.7314610822797,-18.2486186819283,-16.2660208019192));
#81135=CARTESIAN_POINT('Ctrl Pts',(20.7487249397084,-18.29971292963,-16.2691133738655));
#81136=CARTESIAN_POINT('Ctrl Pts',(20.7664984314635,-18.3597875911247,-16.2728309766068));
#81137=CARTESIAN_POINT('Ctrl Pts',(20.7689263695775,-18.3681848960799,-16.273352453169));
#81138=CARTESIAN_POINT('Ctrl Pts',(20.7725219681294,-18.3809156580833,-16.2741461335582));
#81139=CARTESIAN_POINT('Ctrl Pts',(20.7737280018862,-18.3852383061664,-16.2744161605898));
#81140=CARTESIAN_POINT('Ctrl Pts',(20.7758672110919,-18.3930008977206,-16.2749020921806));
#81141=CARTESIAN_POINT('Ctrl Pts',(20.7768054513431,-18.3964393896689,-16.275117699115));
#81142=CARTESIAN_POINT('Ctrl Pts',(20.7788242308213,-18.403912135396,-16.2755870634525));
#81143=CARTESIAN_POINT('Ctrl Pts',(20.7799015026422,-18.4079471688606,-16.2758410008417));
#81144=CARTESIAN_POINT('Ctrl Pts',(20.7828913476432,-18.4192804043579,-16.2765555768137));
#81145=CARTESIAN_POINT('Ctrl Pts',(20.7847768338458,-18.4265855960734,-16.2770177357182));
#81146=CARTESIAN_POINT('Ctrl Pts',(20.795764778106,-18.4701179926372,-16.2797803932719));
#81147=CARTESIAN_POINT('Ctrl Pts',(20.8039455709976,-18.5065685165476,-16.2821289400003));
#81148=CARTESIAN_POINT('Ctrl Pts',(20.8276019738143,-18.6267732820587,-16.2899475036255));
#81149=CARTESIAN_POINT('Ctrl Pts',(20.8389884247766,-18.7112438844614,-16.2955549415315));
#81150=CARTESIAN_POINT('Ctrl Pts',(20.8583667167199,-18.9737803897779,-16.3129456621551));
#81151=CARTESIAN_POINT('Ctrl Pts',(20.849013248908,-19.1523790932572,-16.324649687209));
#81152=CARTESIAN_POINT('Ctrl Pts',(20.8133486346228,-19.3501424844108,-16.337016254709));
#81153=CARTESIAN_POINT('Ctrl Pts',(20.8089428419907,-19.3725002358559,-16.3384070518362));
#81154=CARTESIAN_POINT('Ctrl Pts',(20.8021872471084,-19.4040851641647,-16.3403621676895));
#81155=CARTESIAN_POINT('Ctrl Pts',(20.8001349855574,-19.4133737214395,-16.3409359426052));
#81156=CARTESIAN_POINT('Ctrl Pts',(20.7966949890208,-19.428459769655,-16.3418659862223));
#81157=CARTESIAN_POINT('Ctrl Pts',(20.7953452681792,-19.4342657113208,-16.3422234698676));
#81158=CARTESIAN_POINT('Ctrl Pts',(20.7924655870635,-19.4464199294729,-16.3429709193507));
#81159=CARTESIAN_POINT('Ctrl Pts',(20.7909307379732,-19.452766992162,-16.3433607234993));
#81160=CARTESIAN_POINT('Ctrl Pts',(20.7872036394685,-19.4678733798395,-16.3442872848735));
#81161=CARTESIAN_POINT('Ctrl Pts',(20.7849846575012,-19.4766260265132,-16.3448231740085));
#81162=CARTESIAN_POINT('Ctrl Pts',(20.7772910205284,-19.5061781139872,-16.3466294806816));
#81163=CARTESIAN_POINT('Ctrl Pts',(20.7715553129258,-19.5269086653753,-16.3478914522964));
#81164=CARTESIAN_POINT('Ctrl Pts',(20.7148921410049,-19.72019507986,-16.3596187548537));
#81165=CARTESIAN_POINT('Ctrl Pts',(20.6424810743416,-19.885683184866,-16.3692827107052));
#81166=CARTESIAN_POINT('Ctrl Pts',(20.4883353213915,-20.1429637841121,-16.3856069446835));
#81167=CARTESIAN_POINT('Ctrl Pts',(20.4180341199188,-20.2404517273013,-16.3921921004463));
#81168=CARTESIAN_POINT('Ctrl Pts',(20.3336708919768,-20.3386623697774,-16.399865070986));
#81169=CARTESIAN_POINT('Ctrl Pts',(20.3274239761863,-20.3458362582712,-16.4004320763371));
#81170=CARTESIAN_POINT('Ctrl Pts',(20.3180955402748,-20.3564042622438,-16.4012774942516));
#81171=CARTESIAN_POINT('Ctrl Pts',(20.3150509023666,-20.3598309755598,-16.4015532242197));
#81172=CARTESIAN_POINT('Ctrl Pts',(20.3096138989233,-20.3659103938445,-16.4020453159078));
#81173=CARTESIAN_POINT('Ctrl Pts',(20.307225925006,-20.36856695887,-16.4022613476075));
#81174=CARTESIAN_POINT('Ctrl Pts',(20.3020771778445,-20.3742657419567,-16.4027269410849));
#81175=CARTESIAN_POINT('Ctrl Pts',(20.2993143103751,-20.377305926983,-16.4029766577034));
#81176=CARTESIAN_POINT('Ctrl Pts',(20.2916630066476,-20.3856761363734,-16.4036678129278));
#81177=CARTESIAN_POINT('Ctrl Pts',(20.2867561323809,-20.3909891230169,-16.4041106186315));
#81178=CARTESIAN_POINT('Ctrl Pts',(20.2597168805611,-20.419966916857,-16.4065477680321));
#81179=CARTESIAN_POINT('Ctrl Pts',(20.2370719402452,-20.4431449778755,-16.4085781475792));
#81180=CARTESIAN_POINT('Ctrl Pts',(20.0974804802588,-20.579611596734,-16.4209812558022));
#81181=CARTESIAN_POINT('Ctrl Pts',(19.9683173785099,-20.679616581074,-16.4319460768));
#81182=CARTESIAN_POINT('Ctrl Pts',(19.7289709719092,-20.8242644031252,-16.4502135242569));
#81183=CARTESIAN_POINT('Ctrl Pts',(19.6241275051833,-20.8763237946651,-16.4576564611517));
#81184=CARTESIAN_POINT('Ctrl Pts',(19.5022239938354,-20.9247455896178,-16.4656656227366));
#81185=CARTESIAN_POINT('Ctrl Pts',(19.488887991633,-20.9298871054424,-16.4665337725271));
#81186=CARTESIAN_POINT('Ctrl Pts',(19.4675809751566,-20.9378548399909,-16.4679083033623));
#81187=CARTESIAN_POINT('Ctrl Pts',(19.459643508529,-20.94076896456,-16.4684176139481));
#81188=CARTESIAN_POINT('Ctrl Pts',(19.4456142137588,-20.9458244410496,-16.4693130502426));
#81189=CARTESIAN_POINT('Ctrl Pts',(19.4395296886263,-20.9479856088786,-16.4696998323463));
#81190=CARTESIAN_POINT('Ctrl Pts',(19.4269249371902,-20.9523978629374,-16.4704978900684));
#81191=CARTESIAN_POINT('Ctrl Pts',(19.4204033985751,-20.9546449897025,-16.4709090304463));
#81192=CARTESIAN_POINT('Ctrl Pts',(19.4036362611302,-20.9603309169603,-16.4719616317673));
#81193=CARTESIAN_POINT('Ctrl Pts',(19.3933750221711,-20.9637232366635,-16.4726015520328));
#81194=CARTESIAN_POINT('Ctrl Pts',(19.3504477926322,-20.9775510502206,-16.4752613566935));
#81195=CARTESIAN_POINT('Ctrl Pts',(19.3175555766062,-20.9872709950973,-16.4772577317778));
#81196=CARTESIAN_POINT('Ctrl Pts',(19.2312587072101,-21.0105082290224,-16.4823994315742));
#81197=CARTESIAN_POINT('Ctrl Pts',(19.1775361357973,-21.0227483409673,-16.4855054150318));
#81198=CARTESIAN_POINT('Ctrl Pts',(19.0159372518612,-21.0529882753304,-16.4946470768221));
#81199=CARTESIAN_POINT('Ctrl Pts',(18.9070811406451,-21.0647432764596,-16.500534016658));
#81200=CARTESIAN_POINT('Ctrl Pts',(18.754557487999,-21.0693422957247,-16.5088416995531));
#81201=CARTESIAN_POINT('Ctrl Pts',(18.7112817142969,-21.0693201676826,-16.5112068805828));
#81202=CARTESIAN_POINT('Ctrl Pts',(18.5928022414449,-21.0656267771603,-16.5177700317084));
#81203=CARTESIAN_POINT('Ctrl Pts',(18.5177529915108,-21.0592706621016,-16.5220240790493));
#81204=CARTESIAN_POINT('Ctrl Pts',(18.433813817885,-21.047630514903,-16.527046539221));
#81205=CARTESIAN_POINT('Ctrl Pts',(18.4244260268215,-21.0462642971886,-16.5276120225052));
#81206=CARTESIAN_POINT('Ctrl Pts',(18.4105213361184,-21.0441451957291,-16.528455600293));
#81207=CARTESIAN_POINT('Ctrl Pts',(18.4059970370115,-21.0434406569076,-16.5287310291195));
#81208=CARTESIAN_POINT('Ctrl Pts',(18.3979477694756,-21.0421604376735,-16.529222791435));
#81209=CARTESIAN_POINT('Ctrl Pts',(18.3944219373657,-21.0415905091673,-16.5294387966109));
#81210=CARTESIAN_POINT('Ctrl Pts',(18.3868404097546,-21.0403453074201,-16.5299045706142));
#81211=CARTESIAN_POINT('Ctrl Pts',(18.382785293564,-21.0396671510185,-16.5301544955373));
#81212=CARTESIAN_POINT('Ctrl Pts',(18.3715873651308,-21.0377609187876,-16.5308468012469));
#81213=CARTESIAN_POINT('Ctrl Pts',(18.3644489230377,-21.03650798182,-16.5312905564889));
#81214=CARTESIAN_POINT('Ctrl Pts',(18.3252118006344,-21.0294132144889,-16.5337425227298));
#81215=CARTESIAN_POINT('Ctrl Pts',(18.2932469065661,-21.0228669428704,-16.5357872775799));
#81216=CARTESIAN_POINT('Ctrl Pts',(18.102923303442,-20.9792836830192,-16.5481952218939));
#81217=CARTESIAN_POINT('Ctrl Pts',(17.9491137172016,-20.9248381569016,-16.5591468745221));
#81218=CARTESIAN_POINT('Ctrl Pts',(17.698177629127,-20.8019721539079,-16.5773969993904));
#81219=CARTESIAN_POINT('Ctrl Pts',(17.5977167085537,-20.742025987069,-16.5848353319221));
#81220=CARTESIAN_POINT('Ctrl Pts',(17.4910707202066,-20.6657736644029,-16.5928404902917));
#81221=CARTESIAN_POINT('Ctrl Pts',(17.4795260775724,-20.6573411861138,-16.5937088582423));
#81222=CARTESIAN_POINT('Ctrl Pts',(17.4612896724176,-20.6437354793409,-16.595083668108));
#81223=CARTESIAN_POINT('Ctrl Pts',(17.4545421187629,-20.6386380890332,-16.595593041415));
#81224=CARTESIAN_POINT('Ctrl Pts',(17.4426964996947,-20.6295774090116,-16.5964885506709));
#81225=CARTESIAN_POINT('Ctrl Pts',(17.437585718763,-20.6256309945637,-16.5968753433513));
#81226=CARTESIAN_POINT('Ctrl Pts',(17.427224592324,-20.6175544589851,-16.5976603990638));
#81227=CARTESIAN_POINT('Ctrl Pts',(17.4219755768825,-20.6134227447185,-16.5980585927475));
#81228=CARTESIAN_POINT('Ctrl Pts',(17.408667114926,-20.6028447081675,-16.5990694635341));
#81229=CARTESIAN_POINT('Ctrl Pts',(17.4006350297258,-20.5963641228461,-16.5996807631242));
#81230=CARTESIAN_POINT('Ctrl Pts',(17.3833150813318,-20.5821793938909,-16.6010017738933));
#81231=CARTESIAN_POINT('Ctrl Pts',(17.3740450171815,-20.574454023816,-16.601710610031));
#81232=CARTESIAN_POINT('Ctrl Pts',(17.3475939408034,-20.5520245645737,-16.603738896327));
#81233=CARTESIAN_POINT('Ctrl Pts',(17.330581512773,-20.5371236460894,-16.6050504224965));
#81234=CARTESIAN_POINT('Ctrl Pts',(17.2733864095188,-20.4853845817584,-16.6094885618791));
#81235=CARTESIAN_POINT('Ctrl Pts',(17.2343878027962,-20.4472672744546,-16.6125639234843));
#81236=CARTESIAN_POINT('Ctrl Pts',(17.1220538027896,-20.3286506781454,-16.6216521111689));
#81237=CARTESIAN_POINT('Ctrl Pts',(17.0534107792096,-20.2439591491638,-16.6275160339473));
#81238=CARTESIAN_POINT('Ctrl Pts',(16.9234840216056,-20.0556749204459,-16.639967260909));
#81239=CARTESIAN_POINT('Ctrl Pts',(16.8638998360526,-19.9513915378515,-16.6465480302672));
#81240=CARTESIAN_POINT('Ctrl Pts',(16.8094654177348,-19.8340125791549,-16.6542160209437));
#81241=CARTESIAN_POINT('Ctrl Pts',(16.8055204012333,-19.8253532948458,-16.6547832048003));
#81242=CARTESIAN_POINT('Ctrl Pts',(16.799761470724,-19.8124831955633,-16.6556288384967));
#81243=CARTESIAN_POINT('Ctrl Pts',(16.7979025800113,-19.8082924718744,-16.6559046037539));
#81244=CARTESIAN_POINT('Ctrl Pts',(16.794619514984,-19.8008257153549,-16.656396734067));
#81245=CARTESIAN_POINT('Ctrl Pts',(16.7931900054604,-19.7975520833015,-16.6566127689027));
#81246=CARTESIAN_POINT('Ctrl Pts',(16.790134469513,-19.7905062149881,-16.657078341352));
#81247=CARTESIAN_POINT('Ctrl Pts',(16.7885111584007,-19.7867329152124,-16.6573280336598));
#81248=CARTESIAN_POINT('Ctrl Pts',(16.7840607654319,-19.776304714235,-16.6580190546477));
#81249=CARTESIAN_POINT('Ctrl Pts',(16.7812568114658,-19.7696400898785,-16.6584617495682));
#81250=CARTESIAN_POINT('Ctrl Pts',(16.7668566461675,-19.7349162288726,-16.6607733010531));
#81251=CARTESIAN_POINT('Ctrl Pts',(16.7558316161175,-19.7066259962242,-16.6626735717684));
#81252=CARTESIAN_POINT('Ctrl Pts',(16.7454194499739,-19.6781104572019,-16.6645989847956));
#81253=CARTESIAN_POINT('Ctrl Pts',(16.7454194329591,-19.6781104106039,-16.4437313840672));
#81254=CARTESIAN_POINT('Ctrl Pts',(16.790870432835,-19.8025859363448,-16.4364582452718));
#81255=CARTESIAN_POINT('Ctrl Pts',(16.8479181674973,-19.9225464740244,-16.4293983430912));
#81256=CARTESIAN_POINT('Ctrl Pts',(16.9473167103501,-20.0892030165193,-16.4185943673103));
#81257=CARTESIAN_POINT('Ctrl Pts',(16.9810870901895,-20.1405969870292,-16.4151048852973));
#81258=CARTESIAN_POINT('Ctrl Pts',(17.0245020075486,-20.200786707114,-16.4107315787639));
#81259=CARTESIAN_POINT('Ctrl Pts',(17.0320553064698,-20.2110615029907,-16.4099744760412));
#81260=CARTESIAN_POINT('Ctrl Pts',(17.042796460597,-20.2253994847967,-16.4089020906605));
#81261=CARTESIAN_POINT('Ctrl Pts',(17.0459072301081,-20.2295204337018,-16.4085920048467));
#81262=CARTESIAN_POINT('Ctrl Pts',(17.051248104375,-20.236542115058,-16.4080603741517));
#81263=CARTESIAN_POINT('Ctrl Pts',(17.0534707368775,-20.2394485555461,-16.4078393537839));
#81264=CARTESIAN_POINT('Ctrl Pts',(17.0577587450601,-20.2450257746831,-16.4074133441053));
#81265=CARTESIAN_POINT('Ctrl Pts',(17.0598229851405,-20.2476973880126,-16.4072084395794));
#81266=CARTESIAN_POINT('Ctrl Pts',(17.0653347550376,-20.2547957560812,-16.4066618124772));
#81267=CARTESIAN_POINT('Ctrl Pts',(17.068793479839,-20.2592137259725,-16.4063193047755));
#81268=CARTESIAN_POINT('Ctrl Pts',(17.0812698832623,-20.2750204779662,-16.4050857823426));
#81269=CARTESIAN_POINT('Ctrl Pts',(17.0903869325908,-20.2863298250179,-16.4041880754989));
#81270=CARTESIAN_POINT('Ctrl Pts',(17.2005041091458,-20.4200849236513,-16.3933978926925));
#81271=CARTESIAN_POINT('Ctrl Pts',(17.3148424589957,-20.5308821178171,-16.3827536433332));
#81272=CARTESIAN_POINT('Ctrl Pts',(17.5176071082078,-20.6873877011818,-16.3658986061808));
#81273=CARTESIAN_POINT('Ctrl Pts',(17.5987614499756,-20.7415304798629,-16.3595729150787));
#81274=CARTESIAN_POINT('Ctrl Pts',(17.7122871256008,-20.8064275698765,-16.3513404788038));
#81275=CARTESIAN_POINT('Ctrl Pts',(17.741596230581,-20.8222763863991,-16.3492657415093));
#81276=CARTESIAN_POINT('Ctrl Pts',(17.7854580167468,-20.8446729626536,-16.3462342720938));
#81277=CARTESIAN_POINT('Ctrl Pts',(17.799729144325,-20.851758097113,-16.3452591350037));
#81278=CARTESIAN_POINT('Ctrl Pts',(17.8257480175641,-20.86431147907,-16.3435012080746));
#81279=CARTESIAN_POINT('Ctrl Pts',(17.8374684592054,-20.8698342119811,-16.3427165589774));
#81280=CARTESIAN_POINT('Ctrl Pts',(17.8559006557477,-20.8783136582262,-16.3414936641234));
#81281=CARTESIAN_POINT('Ctrl Pts',(17.8625781826974,-20.8813436155032,-16.3410528970905));
#81282=CARTESIAN_POINT('Ctrl Pts',(17.8693098683501,-20.8843560691563,-16.3406107948684));
#81283=CARTESIAN_POINT('Ctrl Pts',(17.8693483533328,-20.8843732899451,-16.3406082674477));
#81284=CARTESIAN_POINT('Ctrl Pts',(17.8694266528058,-20.8844083236273,-16.340603125443));
#81285=CARTESIAN_POINT('Ctrl Pts',(17.8694664677064,-20.8844261366072,-16.3406005108372));
#81286=CARTESIAN_POINT('Ctrl Pts',(17.8695474765426,-20.8844623765354,-16.3405951912257));
#81287=CARTESIAN_POINT('Ctrl Pts',(17.8695886703042,-20.8844808033018,-16.3405924862369));
#81288=CARTESIAN_POINT('Ctrl Pts',(17.8696724882164,-20.8845182934591,-16.3405869825039));
#81289=CARTESIAN_POINT('Ctrl Pts',(17.8697151123922,-20.8845373567497,-16.340584183764));
#81290=CARTESIAN_POINT('Ctrl Pts',(17.8698018534751,-20.8845761474981,-16.3405784884534));
#81291=CARTESIAN_POINT('Ctrl Pts',(17.8698459568872,-20.8845958688004,-16.3405755927754));
#81292=CARTESIAN_POINT('Ctrl Pts',(17.8699357066387,-20.8846359976562,-16.3405697003117));
#81293=CARTESIAN_POINT('Ctrl Pts',(17.869981354246,-20.884656405647,-16.3405667034499));
#81294=CARTESIAN_POINT('Ctrl Pts',(17.8700742454782,-20.8846979312222,-16.3405606051544));
#81295=CARTESIAN_POINT('Ctrl Pts',(17.8701214901366,-20.8847190491308,-16.3405575036602));
#81296=CARTESIAN_POINT('Ctrl Pts',(17.8702176357682,-20.884762021075,-16.3405511921638));
#81297=CARTESIAN_POINT('Ctrl Pts',(17.8702665377603,-20.8847838754179,-16.3405479821027));
#81298=CARTESIAN_POINT('Ctrl Pts',(17.8703660607466,-20.8848283477957,-16.3405414493814));
#81299=CARTESIAN_POINT('Ctrl Pts',(17.8704166827655,-20.8848509661294,-16.3405381266624));
#81300=CARTESIAN_POINT('Ctrl Pts',(17.8705197111997,-20.8848969952243,-16.3405313643588));
#81301=CARTESIAN_POINT('Ctrl Pts',(17.8705721184478,-20.8849204061864,-16.3405279247286));
#81302=CARTESIAN_POINT('Ctrl Pts',(17.8706787853405,-20.8849680503954,-16.3405209241672));
#81303=CARTESIAN_POINT('Ctrl Pts',(17.870733045853,-20.8849922838461,-16.3405173631887));
#81304=CARTESIAN_POINT('Ctrl Pts',(17.8708434900583,-20.8850416040868,-16.3405101153149));
#81305=CARTESIAN_POINT('Ctrl Pts',(17.8708996745735,-20.8850666910467,-16.3405064283761));
#81306=CARTESIAN_POINT('Ctrl Pts',(17.8710140406351,-20.885117750681,-16.3404989237674));
#81307=CARTESIAN_POINT('Ctrl Pts',(17.8710722227819,-20.8851437234113,-16.3404951060694));
#81308=CARTESIAN_POINT('Ctrl Pts',(17.871190660852,-20.8851965882011,-16.3404873349406));
#81309=CARTESIAN_POINT('Ctrl Pts',(17.8712509174634,-20.8852234803395,-16.3404833814768));
#81310=CARTESIAN_POINT('Ctrl Pts',(17.871373584344,-20.8852782189024,-16.3404753336124));
#81311=CARTESIAN_POINT('Ctrl Pts',(17.8714359952802,-20.8853060653792,-16.340471239181));
#81312=CARTESIAN_POINT('Ctrl Pts',(17.8715630540712,-20.8853627490224,-16.3404629039587));
#81313=CARTESIAN_POINT('Ctrl Pts',(17.8716277024957,-20.885391586179,-16.3404586631444));
#81314=CARTESIAN_POINT('Ctrl Pts',(17.871759322882,-20.885450289017,-16.3404500295168));
#81315=CARTESIAN_POINT('Ctrl Pts',(17.8718262954497,-20.8854801546846,-16.3404456366788));
#81316=CARTESIAN_POINT('Ctrl Pts',(17.8719626562509,-20.885540954765,-16.3404366930068));
#81317=CARTESIAN_POINT('Ctrl Pts',(17.8720320421291,-20.8855718878217,-16.3404321423436));
#81318=CARTESIAN_POINT('Ctrl Pts',(17.8721601038573,-20.8856289710135,-16.3404237438717));
#81319=CARTESIAN_POINT('Ctrl Pts',(17.8722187806341,-20.8856551228372,-16.3404198959346));
#81320=CARTESIAN_POINT('Ctrl Pts',(17.8723460084028,-20.8857118204108,-16.3404115528925));
#81321=CARTESIAN_POINT('Ctrl Pts',(17.8724145607914,-20.8857423656154,-16.340407057758));
#81322=CARTESIAN_POINT('Ctrl Pts',(17.8725632119349,-20.8858085913183,-16.3403973108709));
#81323=CARTESIAN_POINT('Ctrl Pts',(17.872643312163,-20.8858442708779,-16.3403920591065));
#81324=CARTESIAN_POINT('Ctrl Pts',(17.8728170160953,-20.8859216320037,-16.3403806709104));
#81325=CARTESIAN_POINT('Ctrl Pts',(17.8729106212553,-20.8859633120389,-16.340374534499));
#81326=CARTESIAN_POINT('Ctrl Pts',(17.8731136254053,-20.8860536870461,-16.3403612272282));
#81327=CARTESIAN_POINT('Ctrl Pts',(17.8732230259628,-20.8861023797377,-16.3403540564243));
#81328=CARTESIAN_POINT('Ctrl Pts',(17.8734603006058,-20.886207963316,-16.3403385052251));
#81329=CARTESIAN_POINT('Ctrl Pts',(17.8735881758082,-20.8862648506291,-16.3403301249728));
#81330=CARTESIAN_POINT('Ctrl Pts',(17.8738616666911,-20.8863864849013,-16.340312203577));
#81331=CARTESIAN_POINT('Ctrl Pts',(17.8740072841099,-20.8864512281296,-16.3403026625587));
#81332=CARTESIAN_POINT('Ctrl Pts',(17.8800535644706,-20.8891386583196,-16.3399065468012));
#81333=CARTESIAN_POINT('Ctrl Pts',(17.8859662385224,-20.8917343728278,-16.3395208998026));
#81334=CARTESIAN_POINT('Ctrl Pts',(17.8996506613505,-20.8976674218847,-16.338632259072));
#81335=CARTESIAN_POINT('Ctrl Pts',(17.9074307519843,-20.9009853300859,-16.338129932466));
#81336=CARTESIAN_POINT('Ctrl Pts',(17.9284186390258,-20.9097875745876,-16.3367824802344));
#81337=CARTESIAN_POINT('Ctrl Pts',(17.9416626125614,-20.9151849112528,-16.3359403018445));
#81338=CARTESIAN_POINT('Ctrl Pts',(18.0636053365809,-20.9634453736655,-16.3282574841005));
#81339=CARTESIAN_POINT('Ctrl Pts',(18.1756298754291,-20.9973776089088,-16.3217335538499));
#81340=CARTESIAN_POINT('Ctrl Pts',(18.4491388267183,-21.0560600675816,-16.3064198250329));
#81341=CARTESIAN_POINT('Ctrl Pts',(18.6117726556967,-21.0717318756183,-16.2978135107385));
#81342=CARTESIAN_POINT('Ctrl Pts',(18.8069306832055,-21.0679909046237,-16.2866039925212));
#81343=CARTESIAN_POINT('Ctrl Pts',(18.8392677397602,-21.066628770721,-16.2847161910742));
#81344=CARTESIAN_POINT('Ctrl Pts',(18.878773225667,-21.0640563395597,-16.2823589638163));
#81345=CARTESIAN_POINT('Ctrl Pts',(18.8859850599166,-21.0635496220732,-16.2819265636368));
#81346=CARTESIAN_POINT('Ctrl Pts',(18.8972899233484,-21.0626971058423,-16.2812452948227));
#81347=CARTESIAN_POINT('Ctrl Pts',(18.9013848606183,-21.0623763122852,-16.2809978071314));
#81348=CARTESIAN_POINT('Ctrl Pts',(18.9090393193728,-21.0617542505493,-16.2805338143156));
#81349=CARTESIAN_POINT('Ctrl Pts',(18.9125990207231,-21.0614558896018,-16.2803174737478));
#81350=CARTESIAN_POINT('Ctrl Pts',(18.9207257494407,-21.0607540195608,-16.2798223002071));
#81351=CARTESIAN_POINT('Ctrl Pts',(18.9252922161545,-21.060344684259,-16.2795431442299));
#81352=CARTESIAN_POINT('Ctrl Pts',(18.9393335414826,-21.059040035636,-16.2786820358269));
#81353=CARTESIAN_POINT('Ctrl Pts',(18.9488035686918,-21.0580956754469,-16.278097433364));
#81354=CARTESIAN_POINT('Ctrl Pts',(19.0774789355211,-21.0443871717375,-16.2701048129342));
#81355=CARTESIAN_POINT('Ctrl Pts',(19.1953834914841,-21.0215846132481,-16.2622176741382));
#81356=CARTESIAN_POINT('Ctrl Pts',(19.484144606796,-20.9398287306077,-16.2423911049925));
#81357=CARTESIAN_POINT('Ctrl Pts',(19.6506363054677,-20.8687638327228,-16.2305530386383));
#81358=CARTESIAN_POINT('Ctrl Pts',(19.824503642287,-20.7666473678887,-16.2181683321501));
#81359=CARTESIAN_POINT('Ctrl Pts',(19.8427182067667,-20.7555762400712,-16.2168692632026));
#81360=CARTESIAN_POINT('Ctrl Pts',(19.8683794335763,-20.7394432128729,-16.2150361647547));
#81361=CARTESIAN_POINT('Ctrl Pts',(19.875965344941,-20.7346062642732,-16.2144938950286));
#81362=CARTESIAN_POINT('Ctrl Pts',(19.8889986750243,-20.7261785768464,-16.2135615009464));
#81363=CARTESIAN_POINT('Ctrl Pts',(19.8944607080641,-20.7226107726902,-16.213170530257));
#81364=CARTESIAN_POINT('Ctrl Pts',(19.9048871161495,-20.7157312640052,-16.2124237498338));
#81365=CARTESIAN_POINT('Ctrl Pts',(19.9098541437289,-20.7124237115515,-16.212067789564));
#81366=CARTESIAN_POINT('Ctrl Pts',(19.922733333768,-20.7037686085051,-16.2111442379887));
#81367=CARTESIAN_POINT('Ctrl Pts',(19.9306234724815,-20.6983884064559,-16.2105778839342));
#81368=CARTESIAN_POINT('Ctrl Pts',(19.9574020030513,-20.6798617205987,-16.2086535479297));
#81369=CARTESIAN_POINT('Ctrl Pts',(19.9761127357752,-20.6664604397004,-16.2073052758252));
#81370=CARTESIAN_POINT('Ctrl Pts',(20.1353308296661,-20.5484478765306,-16.1957892854875));
#81371=CARTESIAN_POINT('Ctrl Pts',(20.2625690373503,-20.4270787534546,-16.1863693519422));
#81372=CARTESIAN_POINT('Ctrl Pts',(20.4285946627165,-20.2238668941518,-16.1720920257346));
#81373=CARTESIAN_POINT('Ctrl Pts',(20.4795474567863,-20.152982154557,-16.1673177413224));
#81374=CARTESIAN_POINT('Ctrl Pts',(20.5461470359653,-20.0471013030606,-16.1601764776963));
#81375=CARTESIAN_POINT('Ctrl Pts',(20.5654490634911,-20.0145053745493,-16.1579763405716));
#81376=CARTESIAN_POINT('Ctrl Pts',(20.5875483766073,-19.9747926445354,-16.1552723510711));
#81377=CARTESIAN_POINT('Ctrl Pts',(20.5911960988069,-19.9681540359541,-16.1548195644448));
#81378=CARTESIAN_POINT('Ctrl Pts',(20.5968027001453,-19.9578193661804,-16.1541132684264));
#81379=CARTESIAN_POINT('Ctrl Pts',(20.5987864265803,-19.9541367569344,-16.153861312065));
#81380=CARTESIAN_POINT('Ctrl Pts',(20.602439980852,-19.9473058515472,-16.153393396742));
#81381=CARTESIAN_POINT('Ctrl Pts',(20.6041127782342,-19.9441592091365,-16.153177629902));
#81382=CARTESIAN_POINT('Ctrl Pts',(20.6078702097987,-19.9370479685832,-16.1526895110134));
#81383=CARTESIAN_POINT('Ctrl Pts',(20.6099501990588,-19.9330809922625,-16.1524168722143));
#81384=CARTESIAN_POINT('Ctrl Pts',(20.6160338566233,-19.9213880967619,-16.1516123109474));
#81385=CARTESIAN_POINT('Ctrl Pts',(20.6200024410146,-19.9136441681554,-16.1510782624641));
#81386=CARTESIAN_POINT('Ctrl Pts',(20.647813158319,-19.8585425525057,-16.1472709083415));
#81387=CARTESIAN_POINT('Ctrl Pts',(20.669914486368,-19.8103322703828,-16.1439017005862));
#81388=CARTESIAN_POINT('Ctrl Pts',(20.6974113780925,-19.7438727332394,-16.1392543754242));
#81389=CARTESIAN_POINT('Ctrl Pts',(20.704406976404,-19.7263016096593,-16.138025381011));
#81390=CARTESIAN_POINT('Ctrl Pts',(20.7281751076773,-19.6641933764022,-16.1336853322327));
#81391=CARTESIAN_POINT('Ctrl Pts',(20.7436801987438,-19.6191874117372,-16.130547938903));
#81392=CARTESIAN_POINT('Ctrl Pts',(20.7897744966679,-19.4691484961866,-16.1201795930754));
#81393=CARTESIAN_POINT('Ctrl Pts',(20.8137458529611,-19.3622584568169,-16.1129475375456));
#81394=CARTESIAN_POINT('Ctrl Pts',(20.8372084631734,-19.1994630648936,-16.1023754510687));
#81395=CARTESIAN_POINT('Ctrl Pts',(20.8429360692748,-19.1446480841279,-16.0988870377518));
#81396=CARTESIAN_POINT('Ctrl Pts',(20.8487493920924,-19.0554426046535,-16.0933304857184));
#81397=CARTESIAN_POINT('Ctrl Pts',(20.8501478170604,-19.021166439767,-16.0912239257994));
#81398=CARTESIAN_POINT('Ctrl Pts',(20.8508908246223,-18.9760633851422,-16.0884877302167));
#81399=CARTESIAN_POINT('Ctrl Pts',(20.8509860899126,-18.9652556318372,-16.0878347603344));
#81400=CARTESIAN_POINT('Ctrl Pts',(20.8510065598869,-18.9475495836587,-16.0867693026503));
#81401=CARTESIAN_POINT('Ctrl Pts',(20.8509808212093,-18.9406516435527,-16.0863552856376));
#81402=CARTESIAN_POINT('Ctrl Pts',(20.8508657181623,-18.9272973407832,-16.0855557752481));
#81403=CARTESIAN_POINT('Ctrl Pts',(20.8507805294708,-18.920841027263,-16.0851701555803));
#81404=CARTESIAN_POINT('Ctrl Pts',(20.8505155760219,-18.9059315463767,-16.0842817146317));
#81405=CARTESIAN_POINT('Ctrl Pts',(20.8503147050802,-18.8974788280797,-16.0837795595154));
#81406=CARTESIAN_POINT('Ctrl Pts',(20.849638101385,-18.8747429523219,-16.082432870961));
#81407=CARTESIAN_POINT('Ctrl Pts',(20.8490683671309,-18.8604628778926,-16.0815912794742));
#81408=CARTESIAN_POINT('Ctrl Pts',(20.8425104977684,-18.7294206390747,-16.0739047929736));
#81409=CARTESIAN_POINT('Ctrl Pts',(20.8270039789032,-18.6133295019638,-16.0673770411299));
#81410=CARTESIAN_POINT('Ctrl Pts',(20.7671093396643,-18.339844901842,-16.0520508208194));
#81411=CARTESIAN_POINT('Ctrl Pts',(20.7139571800078,-18.1851720940548,-16.0434362593785));
#81412=CARTESIAN_POINT('Ctrl Pts',(20.6297096594212,-18.0091272720831,-16.0322260260118));
#81413=CARTESIAN_POINT('Ctrl Pts',(20.6151625807948,-17.9804284973649,-16.0303490608423));
#81414=CARTESIAN_POINT('Ctrl Pts',(20.5965595767998,-17.9457133105134,-16.0280038914757));
#81415=CARTESIAN_POINT('Ctrl Pts',(20.5931185269444,-17.9393700686196,-16.0275722674848));
#81416=CARTESIAN_POINT('Ctrl Pts',(20.5876695288222,-17.9294467613557,-16.0268919523945));
#81417=CARTESIAN_POINT('Ctrl Pts',(20.5856834486021,-17.9258546626033,-16.0266446358606));
#81418=CARTESIAN_POINT('Ctrl Pts',(20.5819491622501,-17.9191468362812,-16.0261807873233));
#81419=CARTESIAN_POINT('Ctrl Pts',(20.580203511372,-17.9160297504265,-16.0259644188014));
#81420=CARTESIAN_POINT('Ctrl Pts',(20.5761974743839,-17.9089187346331,-16.0254689478649));
#81421=CARTESIAN_POINT('Ctrl Pts',(20.5739319938753,-17.9049277399415,-16.0251895209438));
#81422=CARTESIAN_POINT('Ctrl Pts',(20.567981938688,-17.8945247336758,-16.0244576980905));
#81423=CARTESIAN_POINT('Ctrl Pts',(20.564276747183,-17.8881246711347,-16.024004021211));
#81424=CARTESIAN_POINT('Ctrl Pts',(20.5397061299632,-17.8461915439389,-16.0210094648727));
#81425=CARTESIAN_POINT('Ctrl Pts',(20.5178420378848,-17.811257243094,-16.0184102381458));
#81426=CARTESIAN_POINT('Ctrl Pts',(20.4893197886858,-17.7685114149095,-16.0151182561479));
#81427=CARTESIAN_POINT('Ctrl Pts',(20.4836041503097,-17.7600779795412,-16.0144631906337));
#81428=CARTESIAN_POINT('Ctrl Pts',(20.4774539859061,-17.7511429585327,-16.0137634472015));
#81429=CARTESIAN_POINT('Ctrl Pts',(20.4770797722772,-17.7505998408149,-16.0137208904825));
#81430=CARTESIAN_POINT('Ctrl Pts',(20.4637376061681,-17.7312549453425,-16.0122042912174));
#81431=CARTESIAN_POINT('Ctrl Pts',(20.4504667935286,-17.7126645454522,-16.0107197907439));
#81432=CARTESIAN_POINT('Ctrl Pts',(20.4097658136839,-17.6575566207473,-16.0062448339325));
#81433=CARTESIAN_POINT('Ctrl Pts',(20.3814524296277,-17.6217086687584,-16.0032337147627));
#81434=CARTESIAN_POINT('Ctrl Pts',(20.2814844878627,-17.5032285749942,-15.9929934745232));
#81435=CARTESIAN_POINT('Ctrl Pts',(20.2045911610316,-17.4252347967746,-15.9857628952117));
#81436=CARTESIAN_POINT('Ctrl Pts',(20.0804339718783,-17.317424623352,-15.9751939093095));
#81437=CARTESIAN_POINT('Ctrl Pts',(20.0374614036461,-17.2829552758222,-15.971707110043));
#81438=CARTESIAN_POINT('Ctrl Pts',(19.9656280004393,-17.2298045783962,-15.9661528278837));
#81439=CARTESIAN_POINT('Ctrl Pts',(19.9375729779295,-17.210082405946,-15.964046962912));
#81440=CARTESIAN_POINT('Ctrl Pts',(19.9000608369179,-17.1850512438452,-15.9613115242494));
#81441=CARTESIAN_POINT('Ctrl Pts',(19.891025843108,-17.1791218351412,-15.960658632483));
#81442=CARTESIAN_POINT('Ctrl Pts',(19.876150228919,-17.1695215480902,-15.9595932695886));
#81443=CARTESIAN_POINT('Ctrl Pts',(19.8703364509914,-17.1658096269315,-15.9591792697749));
#81444=CARTESIAN_POINT('Ctrl Pts',(19.8590454231097,-17.1586780859239,-15.9583797700264));
#81445=CARTESIAN_POINT('Ctrl Pts',(19.8535704726618,-17.1552549847753,-15.9579941439189));
#81446=CARTESIAN_POINT('Ctrl Pts',(19.8408898479375,-17.1474071478114,-15.9571056558735));
#81447=CARTESIAN_POINT('Ctrl Pts',(19.8336731231094,-17.1430004082056,-15.956603460327));
#81448=CARTESIAN_POINT('Ctrl Pts',(19.8141869539514,-17.131261292758,-15.955256591742));
#81449=CARTESIAN_POINT('Ctrl Pts',(19.8018692004384,-17.1240096605255,-15.9544148619002));
#81450=CARTESIAN_POINT('Ctrl Pts',(19.687971680864,-17.0585008012987,-15.9467174721327));
#81451=CARTESIAN_POINT('Ctrl Pts',(19.5817896987187,-17.0086371674994,-15.9401800340575));
#81452=CARTESIAN_POINT('Ctrl Pts',(19.3186486417966,-16.9107625227303,-15.9248116556554));
#81453=CARTESIAN_POINT('Ctrl Pts',(19.1592046897174,-16.8716987720604,-15.9161664053772));
#81454=CARTESIAN_POINT('Ctrl Pts',(18.9656472618229,-16.8474765239346,-15.90495304526));
#81455=CARTESIAN_POINT('Ctrl Pts',(18.9343369884688,-16.8442655841497,-15.9031159309338));
#81456=CARTESIAN_POINT('Ctrl Pts',(18.8958240926246,-16.8411818325507,-15.9008151250625));
#81457=CARTESIAN_POINT('Ctrl Pts',(18.8886767210276,-16.84064605487,-15.9003863995166));
#81458=CARTESIAN_POINT('Ctrl Pts',(18.8774430125444,-16.8398613062728,-15.8997096462996));
#81459=CARTESIAN_POINT('Ctrl Pts',(18.8733583627015,-16.839587870353,-15.899462969489));
#81460=CARTESIAN_POINT('Ctrl Pts',(18.8657059532007,-16.8390978920514,-15.8989996559279));
#81461=CARTESIAN_POINT('Ctrl Pts',(18.8621384295506,-16.8388785368364,-15.8987831786253));
#81462=CARTESIAN_POINT('Ctrl Pts',(18.8539725028342,-16.8383971961382,-15.8982865765393));
#81463=CARTESIAN_POINT('Ctrl Pts',(18.849373803297,-16.8381411829274,-15.8980061215519));
#81464=CARTESIAN_POINT('Ctrl Pts',(18.8351628063768,-16.8373965567705,-15.897137090127));
#81465=CARTESIAN_POINT('Ctrl Pts',(18.8255481414695,-16.8369584956144,-15.8965457938941));
#81466=CARTESIAN_POINT('Ctrl Pts',(18.7294004102483,-16.8332346462027,-15.8906016314718));
#81467=CARTESIAN_POINT('Ctrl Pts',(18.6427551493516,-16.835196115579,-15.8849957698359));
#81468=CARTESIAN_POINT('Ctrl Pts',(18.4300104430436,-16.8530983041842,-15.8709781186537));
#81469=CARTESIAN_POINT('Ctrl Pts',(18.3047396631587,-16.8750943410494,-15.8625167823198));
#81470=CARTESIAN_POINT('Ctrl Pts',(18.0889889624705,-16.9333445438758,-15.8480526013624));
#81471=CARTESIAN_POINT('Ctrl Pts',(17.9976063499515,-16.964856819913,-15.8419579293624));
#81472=CARTESIAN_POINT('Ctrl Pts',(17.8952172022191,-17.0082031399688,-15.8351790061739));
#81473=CARTESIAN_POINT('Ctrl Pts',(17.8818109212061,-17.0140431878553,-15.8342922471612));
#81474=CARTESIAN_POINT('Ctrl Pts',(17.8614116480839,-17.0231821446244,-15.8329439789958));
#81475=CARTESIAN_POINT('Ctrl Pts',(17.8543746313355,-17.0263811476855,-15.8324790654898));
#81476=CARTESIAN_POINT('Ctrl Pts',(17.8415803412243,-17.0322821571645,-15.8316340821913));
#81477=CARTESIAN_POINT('Ctrl Pts',(17.835817445277,-17.034971689508,-15.831253588536));
#81478=CARTESIAN_POINT('Ctrl Pts',(17.8233758132716,-17.0408465941867,-15.8304323316166));
#81479=CARTESIAN_POINT('Ctrl Pts',(17.8167014656041,-17.0440411034477,-15.8299918906153));
#81480=CARTESIAN_POINT('Ctrl Pts',(17.7985847175199,-17.0528292698749,-15.8287966171928));
#81481=CARTESIAN_POINT('Ctrl Pts',(17.7871757109439,-17.0584913548715,-15.8280441724757));
#81482=CARTESIAN_POINT('Ctrl Pts',(17.7311353448464,-17.0869363438208,-15.8243486684603));
#81483=CARTESIAN_POINT('Ctrl Pts',(17.6872694606958,-17.1111969910668,-15.8214579755489));
#81484=CARTESIAN_POINT('Ctrl Pts',(17.4954797331696,-17.2263440211844,-15.8087586060616));
#81485=CARTESIAN_POINT('Ctrl Pts',(17.3582177111238,-17.3336539369157,-15.7995651201117));
#81486=CARTESIAN_POINT('Ctrl Pts',(17.19129709884,-17.5009007949591,-15.7865788751071));
#81487=CARTESIAN_POINT('Ctrl Pts',(17.1489969915537,-17.5472276132431,-15.7830863866958));
#81488=CARTESIAN_POINT('Ctrl Pts',(17.0889996923105,-17.6191011162198,-15.7777011333854));
#81489=CARTESIAN_POINT('Ctrl Pts',(17.0697048262149,-17.6432728343305,-15.7758951095653));
#81490=CARTESIAN_POINT('Ctrl Pts',(17.0466234948629,-17.673524210655,-15.7736289380349));
#81491=CARTESIAN_POINT('Ctrl Pts',(17.0423282297889,-17.6792131236494,-15.7732025229752));
#81492=CARTESIAN_POINT('Ctrl Pts',(17.0356167548009,-17.6881962014242,-15.7725286096085));
#81493=CARTESIAN_POINT('Ctrl Pts',(17.0331811635645,-17.6914759130248,-15.7722824433926));
#81494=CARTESIAN_POINT('Ctrl Pts',(17.0286315565037,-17.6976395024459,-15.7718195518475));
#81495=CARTESIAN_POINT('Ctrl Pts',(17.0265153489583,-17.7005216934863,-15.77160298273));
#81496=CARTESIAN_POINT('Ctrl Pts',(17.0216819502259,-17.7071396722318,-15.7711054550512));
#81497=CARTESIAN_POINT('Ctrl Pts',(17.0189696857335,-17.7108789908125,-15.7708241616419));
#81498=CARTESIAN_POINT('Ctrl Pts',(17.0106032988427,-17.722493271639,-15.7699499942839));
#81499=CARTESIAN_POINT('Ctrl Pts',(17.004991109216,-17.7303980877424,-15.7693543548345));
#81500=CARTESIAN_POINT('Ctrl Pts',(16.9421416671983,-17.820222770141,-15.7625809764419));
#81501=CARTESIAN_POINT('Ctrl Pts',(16.8907261571511,-17.9060493411936,-15.7560680493768));
#81502=CARTESIAN_POINT('Ctrl Pts',(16.7684063382777,-18.1474645592063,-15.7382365648547));
#81503=CARTESIAN_POINT('Ctrl Pts',(16.7099350758424,-18.3085601099599,-15.7269007107454));
#81504=CARTESIAN_POINT('Ctrl Pts',(16.6614520670905,-18.5181762464437,-15.7134187920268));
#81505=CARTESIAN_POINT('Ctrl Pts',(16.6528139417587,-18.56171415668,-15.7106795622788));
#81506=CARTESIAN_POINT('Ctrl Pts',(16.6436144405759,-18.61716111556,-15.7072652715688));
#81507=CARTESIAN_POINT('Ctrl Pts',(16.6417764780847,-18.6288442963189,-15.7065499634193));
#81508=CARTESIAN_POINT('Ctrl Pts',(16.6389885125765,-18.6475880966758,-15.7054088041597));
#81509=CARTESIAN_POINT('Ctrl Pts',(16.6379760959988,-18.6546390491194,-15.7049809837439));
#81510=CARTESIAN_POINT('Ctrl Pts',(16.6361227657834,-18.6680264706376,-15.7041714091887));
#81511=CARTESIAN_POINT('Ctrl Pts',(16.635274926425,-18.6743618863432,-15.7037894401518));
#81512=CARTESIAN_POINT('Ctrl Pts',(16.6334140698792,-18.6887627946346,-15.7029237642299));
#81513=CARTESIAN_POINT('Ctrl Pts',(16.6324187836107,-18.696830507611,-15.7024406220194));
#81514=CARTESIAN_POINT('Ctrl Pts',(16.6299653959485,-18.7177062719833,-15.7011950717472));
#81515=CARTESIAN_POINT('Ctrl Pts',(16.6285777519007,-18.7305223843567,-15.7004348848485));
#81516=CARTESIAN_POINT('Ctrl Pts',(16.6203967177342,-18.8131247043734,-15.6955629085869));
#81517=CARTESIAN_POINT('Ctrl Pts',(16.6169563817282,-18.8832033388859,-15.6915582484701));
#81518=CARTESIAN_POINT('Ctrl Pts',(16.6171212268753,-19.1457165867496,-15.6768592614934));
#81519=CARTESIAN_POINT('Ctrl Pts',(16.6434647893585,-19.3371656425855,-15.6668249320135));
#81520=CARTESIAN_POINT('Ctrl Pts',(16.708705242865,-19.5703427336084,-15.6531662090734));
#81521=CARTESIAN_POINT('Ctrl Pts',(16.7238020963104,-19.6177853506364,-15.650302711385));
#81522=CARTESIAN_POINT('Ctrl Pts',(16.7421614448645,-19.669140807954,-15.6470652109916));
#81523=CARTESIAN_POINT('Ctrl Pts',(16.7437828787667,-19.673628420565,-15.6467811358882));
#81524=CARTESIAN_POINT('Ctrl Pts',(16.7454194499636,-19.6781104571738,-15.6464962048466));
#81525=CARTESIAN_POINT('Origin',(18.734,-18.952,0.));
#81526=CARTESIAN_POINT('',(16.7454194444943,-19.678110442195,-14.843838520965));
#81527=CARTESIAN_POINT('',(16.7486736625677,-19.6769293383554,-15.066381399119));
#81528=CARTESIAN_POINT('',(16.7454194499637,-19.6781104571739,0.));
#81529=CARTESIAN_POINT('',(16.6156459649053,-18.9502594248307,-15.110942953281));
#81530=CARTESIAN_POINT('Ctrl Pts',(16.7486736625677,-19.6769293383554,-15.066381399119));
#81531=CARTESIAN_POINT('Ctrl Pts',(16.6638907236804,-19.4439527091799,-15.0812352505063));
#81532=CARTESIAN_POINT('Ctrl Pts',(16.6178442275957,-19.196755842275,-15.0960891018936));
#81533=CARTESIAN_POINT('Ctrl Pts',(16.6156459649053,-18.9502594248307,-15.110942953281));
#81534=CARTESIAN_POINT('Ctrl Pts',(16.6170007608285,-18.9502051888479,-15.1101643145793));
#81535=CARTESIAN_POINT('Ctrl Pts',(16.6170691197414,-18.8695751089078,-15.1145731378411));
#81536=CARTESIAN_POINT('Ctrl Pts',(16.6217438741122,-18.7890199750102,-15.119036689108));
#81537=CARTESIAN_POINT('Ctrl Pts',(16.6337248049843,-18.6853612827869,-15.1250697269885));
#81538=CARTESIAN_POINT('Ctrl Pts',(16.6368453918934,-18.6618370352918,-15.1264584620397));
#81539=CARTESIAN_POINT('Ctrl Pts',(16.6412432750163,-18.632478810018,-15.1282217045135));
#81540=CARTESIAN_POINT('Ctrl Pts',(16.642150837834,-18.6265901327867,-15.1285768971463));
#81541=CARTESIAN_POINT('Ctrl Pts',(16.6437157802129,-18.6167132296185,-15.1291753239111));
#81542=CARTESIAN_POINT('Ctrl Pts',(16.6443597514526,-18.612722872974,-15.1294178270275));
#81543=CARTESIAN_POINT('Ctrl Pts',(16.6455594680531,-18.6054218501564,-15.1298629101726));
#81544=CARTESIAN_POINT('Ctrl Pts',(16.6461116697674,-18.6021106038405,-15.1300652910502));
#81545=CARTESIAN_POINT('Ctrl Pts',(16.6472681665263,-18.5952759684218,-15.1304841220257));
#81546=CARTESIAN_POINT('Ctrl Pts',(16.6478735058979,-18.5917528217064,-15.1307006328781));
#81547=CARTESIAN_POINT('Ctrl Pts',(16.6492800584961,-18.5836889554203,-15.1311975757814));
#81548=CARTESIAN_POINT('Ctrl Pts',(16.650087182348,-18.5791493227035,-15.131478339748));
#81549=CARTESIAN_POINT('Ctrl Pts',(16.6526294586288,-18.565116554505,-15.1323492617065));
#81550=CARTESIAN_POINT('Ctrl Pts',(16.654414669687,-18.5556327753986,-15.1329421562727));
#81551=CARTESIAN_POINT('Ctrl Pts',(16.6734315733765,-18.4582735619008,-15.1390706475135));
#81552=CARTESIAN_POINT('Ctrl Pts',(16.6961558783454,-18.3715728930258,-15.1448764856683));
#81553=CARTESIAN_POINT('Ctrl Pts',(16.7385997773342,-18.2433832521665,-15.1537504415924));
#81554=CARTESIAN_POINT('Ctrl Pts',(16.7542920791194,-18.2006570659467,-15.1567594586229));
#81555=CARTESIAN_POINT('Ctrl Pts',(16.78571002011,-18.1229505124147,-15.1622979063625));
#81556=CARTESIAN_POINT('Ctrl Pts',(16.8010330016433,-18.0878266598706,-15.1648270677989));
#81557=CARTESIAN_POINT('Ctrl Pts',(16.857652263453,-17.9670939618537,-15.1735859408722));
#81558=CARTESIAN_POINT('Ctrl Pts',(16.9037553332312,-17.8838573008273,-15.179735059823));
#81559=CARTESIAN_POINT('Ctrl Pts',(16.9803710678194,-17.7651504868338,-15.1886008576126));
#81560=CARTESIAN_POINT('Ctrl Pts',(17.0067075740656,-17.7271377223248,-15.1914572318686));
#81561=CARTESIAN_POINT('Ctrl Pts',(17.0414157516356,-17.6803902820937,-15.194994944838));
#81562=CARTESIAN_POINT('Ctrl Pts',(17.048643778364,-17.6708258791469,-15.1957201448677));
#81563=CARTESIAN_POINT('Ctrl Pts',(17.060317393222,-17.6556486655401,-15.1968733133754));
#81564=CARTESIAN_POINT('Ctrl Pts',(17.0647108064457,-17.6499962208848,-15.197303324918));
#81565=CARTESIAN_POINT('Ctrl Pts',(17.0730769213008,-17.6393445622146,-15.1981147191934));
#81566=CARTESIAN_POINT('Ctrl Pts',(17.0770437240328,-17.6343408359456,-15.1984963300181));
#81567=CARTESIAN_POINT('Ctrl Pts',(17.0860738322339,-17.6230555170312,-15.1993580737097));
#81568=CARTESIAN_POINT('Ctrl Pts',(17.091150549023,-17.6167847449192,-15.1998376618733));
#81569=CARTESIAN_POINT('Ctrl Pts',(17.1062386027625,-17.5983642777021,-15.2012488179835));
#81570=CARTESIAN_POINT('Ctrl Pts',(17.1163498928958,-17.5862968895233,-15.2021763319154));
#81571=CARTESIAN_POINT('Ctrl Pts',(17.2076539789396,-17.4797662679517,-15.2103951493466));
#81572=CARTESIAN_POINT('Ctrl Pts',(17.2969060023568,-17.3925221414867,-15.2173235739227));
#81573=CARTESIAN_POINT('Ctrl Pts',(17.5230012227813,-17.2075094013752,-15.2332790499738));
#81574=CARTESIAN_POINT('Ctrl Pts',(17.6647991631224,-17.1171813181652,-15.2421389788301));
#81575=CARTESIAN_POINT('Ctrl Pts',(17.8351421427705,-17.0351777594775,-15.2531371160311));
#81576=CARTESIAN_POINT('Ctrl Pts',(17.8546904645034,-17.0261319855951,-15.2544047265975));
#81577=CARTESIAN_POINT('Ctrl Pts',(17.8801226391083,-17.0148314362456,-15.256065187557));
#81578=CARTESIAN_POINT('Ctrl Pts',(17.8858840296342,-17.0123021136349,-15.2564420896998));
#81579=CARTESIAN_POINT('Ctrl Pts',(17.8947418675373,-17.0084604205186,-15.2570228209372));
#81580=CARTESIAN_POINT('Ctrl Pts',(17.8978303674907,-17.0071296559354,-15.2572255417991));
#81581=CARTESIAN_POINT('Ctrl Pts',(17.90420414822,-17.0044013270906,-15.257644409394));
#81582=CARTESIAN_POINT('Ctrl Pts',(17.907489768869,-17.0030047245972,-15.2578606137712));
#81583=CARTESIAN_POINT('Ctrl Pts',(17.9149824864291,-16.9998421860427,-15.2583542929644));
#81584=CARTESIAN_POINT('Ctrl Pts',(17.9191917530114,-16.9980815426766,-15.2586320832073));
#81585=CARTESIAN_POINT('Ctrl Pts',(17.9301572903825,-16.9935364954571,-15.259356860997));
#81586=CARTESIAN_POINT('Ctrl Pts',(17.9369222789644,-16.9907734696079,-15.259805090379));
#81587=CARTESIAN_POINT('Ctrl Pts',(17.9802234226111,-16.9733490141404,-15.2626804287361));
#81588=CARTESIAN_POINT('Ctrl Pts',(18.0171457755562,-16.9596751222136,-15.2651607773159));
#81589=CARTESIAN_POINT('Ctrl Pts',(18.235201716319,-16.8857657503663,-15.2798884079933));
#81590=CARTESIAN_POINT('Ctrl Pts',(18.4234383087793,-16.849219367164,-15.2928183246153));
#81591=CARTESIAN_POINT('Ctrl Pts',(18.6690529453782,-16.8352791692237,-15.3086312183993));
#81592=CARTESIAN_POINT('Ctrl Pts',(18.7241703607051,-16.8343056418313,-15.3121204590878));
#81593=CARTESIAN_POINT('Ctrl Pts',(18.8135629070257,-16.8362175210011,-15.3176781746887));
#81594=CARTESIAN_POINT('Ctrl Pts',(18.8478374835046,-16.8377845430761,-15.3197850908614));
#81595=CARTESIAN_POINT('Ctrl Pts',(18.8928425358842,-16.8409398699132,-15.3225216745292));
#81596=CARTESIAN_POINT('Ctrl Pts',(18.903618791606,-16.8417783774286,-15.3231746845181));
#81597=CARTESIAN_POINT('Ctrl Pts',(18.9212612533888,-16.8432871684874,-15.3242401909176));
#81598=CARTESIAN_POINT('Ctrl Pts',(18.9281313432878,-16.8439085394338,-15.3246542168083));
#81599=CARTESIAN_POINT('Ctrl Pts',(18.9414258997368,-16.8451765177197,-15.3254537327886));
#81600=CARTESIAN_POINT('Ctrl Pts',(18.9478506781229,-16.8458189588116,-15.3258393492298));
#81601=CARTESIAN_POINT('Ctrl Pts',(18.9626811672482,-16.8473704830161,-15.326727766235));
#81602=CARTESIAN_POINT('Ctrl Pts',(18.9710846082253,-16.8483005510008,-15.3272299007503));
#81603=CARTESIAN_POINT('Ctrl Pts',(18.9936755513015,-16.8509379350574,-15.3285764974201));
#81604=CARTESIAN_POINT('Ctrl Pts',(19.0078518662731,-16.8527386149092,-15.3294180182596));
#81605=CARTESIAN_POINT('Ctrl Pts',(19.1377451283051,-16.8705758994455,-15.3370990129157));
#81606=CARTESIAN_POINT('Ctrl Pts',(19.2519741142662,-16.8960222535672,-15.3436218860048));
#81607=CARTESIAN_POINT('Ctrl Pts',(19.5189116212569,-16.9791626350241,-15.3589277184868));
#81608=CARTESIAN_POINT('Ctrl Pts',(19.668172525631,-17.0453056453673,-15.3675276002886));
#81609=CARTESIAN_POINT('Ctrl Pts',(19.8363822074808,-17.1443773754407,-15.3787365995727));
#81610=CARTESIAN_POINT('Ctrl Pts',(19.8640114923998,-17.1615196594594,-15.3806328928087));
#81611=CARTESIAN_POINT('Ctrl Pts',(19.8972958414608,-17.1832478405104,-15.3829995676429));
#81612=CARTESIAN_POINT('Ctrl Pts',(19.9033378842848,-17.1872364675708,-15.3834325726173));
#81613=CARTESIAN_POINT('Ctrl Pts',(19.9127774099826,-17.1935376865304,-15.3841145845471));
#81614=CARTESIAN_POINT('Ctrl Pts',(19.9161888857246,-17.1958293568144,-15.384362205581));
#81615=CARTESIAN_POINT('Ctrl Pts',(19.9225528715413,-17.2001313318991,-15.3848263111737));
#81616=CARTESIAN_POINT('Ctrl Pts',(19.9255069742107,-17.2021391802564,-15.3850426303395));
#81617=CARTESIAN_POINT('Ctrl Pts',(19.9322384985863,-17.2067394206386,-15.3855375738613));
#81618=CARTESIAN_POINT('Ctrl Pts',(19.9360125820067,-17.2093365955661,-15.3858165200582));
#81619=CARTESIAN_POINT('Ctrl Pts',(19.9475864351039,-17.2173567484563,-15.3866763526846));
#81620=CARTESIAN_POINT('Ctrl Pts',(19.9553580313984,-17.2228199061397,-15.3872598780031));
#81621=CARTESIAN_POINT('Ctrl Pts',(20.0609994710828,-17.2981495661774,-15.3952735575706));
#81622=CARTESIAN_POINT('Ctrl Pts',(20.1527691273615,-17.376171226247,-15.4031857664361));
#81623=CARTESIAN_POINT('Ctrl Pts',(20.3139826238442,-17.5387862437774,-15.4183136523095));
#81624=CARTESIAN_POINT('Ctrl Pts',(20.3844953901134,-17.6218170573477,-15.4255015744608));
#81625=CARTESIAN_POINT('Ctrl Pts',(20.4921552110227,-17.7704071972237,-15.4372889045334));
#81626=CARTESIAN_POINT('Ctrl Pts',(20.5327621513991,-17.833193430292,-15.4419888857415));
#81627=CARTESIAN_POINT('Ctrl Pts',(20.5793099886945,-17.914275495576,-15.4477160602456));
#81628=CARTESIAN_POINT('Ctrl Pts',(20.5884357176153,-17.9306727721841,-15.4488577274203));
#81629=CARTESIAN_POINT('Ctrl Pts',(20.6013989038248,-17.9547119902182,-15.4505080075677));
#81630=CARTESIAN_POINT('Ctrl Pts',(20.605409799819,-17.9622589202485,-15.4510227831713));
#81631=CARTESIAN_POINT('Ctrl Pts',(20.6123664339373,-17.9755420560458,-15.4519230902177));
#81632=CARTESIAN_POINT('Ctrl Pts',(20.6153318504578,-17.9812677782554,-15.4523093148902));
#81633=CARTESIAN_POINT('Ctrl Pts',(20.6210425004237,-17.9924185458965,-15.4530579237651));
#81634=CARTESIAN_POINT('Ctrl Pts',(20.6237906108457,-17.9978420393821,-15.4534204064972));
#81635=CARTESIAN_POINT('Ctrl Pts',(20.6303094713962,-18.0108458856296,-15.4542856898601));
#81636=CARTESIAN_POINT('Ctrl Pts',(20.6340582067159,-18.0184372048122,-15.4547877172227));
#81637=CARTESIAN_POINT('Ctrl Pts',(20.6474512464169,-18.045973438777,-15.4565977314761));
#81638=CARTESIAN_POINT('Ctrl Pts',(20.6568280796822,-18.0660473868922,-15.4578964409773));
#81639=CARTESIAN_POINT('Ctrl Pts',(20.741595176437,-18.2552053197196,-15.469951458362));
#81640=CARTESIAN_POINT('Ctrl Pts',(20.7948152000208,-18.4333402024837,-15.4798561845685));
#81641=CARTESIAN_POINT('Ctrl Pts',(20.8369504128257,-18.6955635533118,-15.4943330380546));
#81642=CARTESIAN_POINT('Ctrl Pts',(20.845174292267,-18.7756447490726,-15.4987559730682));
#81643=CARTESIAN_POINT('Ctrl Pts',(20.8504595433111,-18.8920665410086,-15.5054217007623));
#81644=CARTESIAN_POINT('Ctrl Pts',(20.8511738231199,-18.9281741761837,-15.5075220242888));
#81645=CARTESIAN_POINT('Ctrl Pts',(20.8509210469528,-18.9717509256829,-15.5101153368248));
#81646=CARTESIAN_POINT('Ctrl Pts',(20.8508381614858,-18.9792215429347,-15.5105620006315));
#81647=CARTESIAN_POINT('Ctrl Pts',(20.8506475586361,-18.990851272713,-15.5112607848848));
#81648=CARTESIAN_POINT('Ctrl Pts',(20.8505671202302,-18.9950108561649,-15.5115114049122));
#81649=CARTESIAN_POINT('Ctrl Pts',(20.850394970169,-19.0027350487422,-15.5119781176861));
#81650=CARTESIAN_POINT('Ctrl Pts',(20.8503065136778,-19.0062996729991,-15.5121940264597));
#81651=CARTESIAN_POINT('Ctrl Pts',(20.850085804409,-19.0143714707114,-15.5126841203791));
#81652=CARTESIAN_POINT('Ctrl Pts',(20.8499481577756,-19.0188784323672,-15.5129586025568));
#81653=CARTESIAN_POINT('Ctrl Pts',(20.849498006687,-19.0322205860429,-15.5137735637074));
#81654=CARTESIAN_POINT('Ctrl Pts',(20.8491445593857,-19.0410541709702,-15.5143162499787));
#81655=CARTESIAN_POINT('Ctrl Pts',(20.8461241401415,-19.1063081108626,-15.5183468313878));
#81656=CARTESIAN_POINT('Ctrl Pts',(20.8412556260364,-19.1625989035414,-15.5219434801864));
#81657=CARTESIAN_POINT('Ctrl Pts',(20.8131046449385,-19.3843401555385,-15.5364180765149));
#81658=CARTESIAN_POINT('Ctrl Pts',(20.7725261295108,-19.5469898889839,-15.5476594745444));
#81659=CARTESIAN_POINT('Ctrl Pts',(20.6924878529298,-19.7578757422094,-15.5621968538009));
#81660=CARTESIAN_POINT('Ctrl Pts',(20.66947368846,-19.811681890864,-15.5659093240687));
#81661=CARTESIAN_POINT('Ctrl Pts',(20.6288206965622,-19.8967890768006,-15.5717793660662));
#81662=CARTESIAN_POINT('Ctrl Pts',(20.6125643597269,-19.9287128872708,-15.5739809831105));
#81663=CARTESIAN_POINT('Ctrl Pts',(20.5902763260031,-19.9698643021249,-15.5768204393296));
#81664=CARTESIAN_POINT('Ctrl Pts',(20.5849725914846,-19.979477497907,-15.5774838714361));
#81665=CARTESIAN_POINT('Ctrl Pts',(20.5761967548112,-19.9950954979423,-15.5785620280071));
#81666=CARTESIAN_POINT('Ctrl Pts',(20.5727695531084,-20.0011251753757,-15.5789783526019));
#81667=CARTESIAN_POINT('Ctrl Pts',(20.5661017523705,-20.0127231845394,-15.5797793415378));
#81668=CARTESIAN_POINT('Ctrl Pts',(20.5628652492898,-20.018293771254,-15.5801641478218));
#81669=CARTESIAN_POINT('Ctrl Pts',(20.5553678073458,-20.0310636185869,-15.5810465119199));
#81670=CARTESIAN_POINT('Ctrl Pts',(20.5510895060822,-20.038252600708,-15.5815434328393));
#81671=CARTESIAN_POINT('Ctrl Pts',(20.5395461984696,-20.0573901879183,-15.5828668838649));
#81672=CARTESIAN_POINT('Ctrl Pts',(20.5322051523821,-20.0692926144422,-15.5836906305744));
#81673=CARTESIAN_POINT('Ctrl Pts',(20.4711016089967,-20.1662006504558,-15.5904048556163));
#81674=CARTESIAN_POINT('Ctrl Pts',(20.4114583636735,-20.247354159216,-15.5960656517049));
#81675=CARTESIAN_POINT('Ctrl Pts',(20.2351968897145,-20.4544873169829,-15.6110491234602));
#81676=CARTESIAN_POINT('Ctrl Pts',(20.108705877371,-20.5710220549652,-15.6200588730909));
#81677=CARTESIAN_POINT('Ctrl Pts',(19.937182119321,-20.6943067283641,-15.6320939663138));
#81678=CARTESIAN_POINT('Ctrl Pts',(19.9041445611221,-20.716664611552,-15.6344072888017));
#81679=CARTESIAN_POINT('Ctrl Pts',(19.8640134933786,-20.7422004286718,-15.6372366759696));
#81680=CARTESIAN_POINT('Ctrl Pts',(19.8575068967892,-20.7462910351449,-15.6376960082582));
#81681=CARTESIAN_POINT('Ctrl Pts',(19.8474045632327,-20.7525657380572,-15.6384103297905));
#81682=CARTESIAN_POINT('Ctrl Pts',(19.8438242700708,-20.7547747467025,-15.6386637088752));
#81683=CARTESIAN_POINT('Ctrl Pts',(19.8372005148472,-20.7588343342487,-15.6391329295904));
#81684=CARTESIAN_POINT('Ctrl Pts',(19.8341589573712,-20.760687909878,-15.6393485705007));
#81685=CARTESIAN_POINT('Ctrl Pts',(19.8273078768079,-20.7648393969629,-15.6398347007006));
#81686=CARTESIAN_POINT('Ctrl Pts',(19.8234958046325,-20.7671329657969,-15.640105466264));
#81687=CARTESIAN_POINT('Ctrl Pts',(19.813723307694,-20.7729708036188,-15.6408002325388));
#81688=CARTESIAN_POINT('Ctrl Pts',(19.8077526993204,-20.7764978011684,-15.6412253146944));
#81689=CARTESIAN_POINT('Ctrl Pts',(19.7727732468777,-20.7969299286036,-15.6437187512228));
#81690=CARTESIAN_POINT('Ctrl Pts',(19.7433845866367,-20.8131713419148,-15.6458258031895));
#81691=CARTESIAN_POINT('Ctrl Pts',(19.6974370899012,-20.8371555347414,-15.649124335273));
#81692=CARTESIAN_POINT('Ctrl Pts',(19.6811417857406,-20.8453950506753,-15.650294980898));
#81693=CARTESIAN_POINT('Ctrl Pts',(19.6425587959565,-20.8642813444969,-15.6530654005765));
#81694=CARTESIAN_POINT('Ctrl Pts',(19.6201874491395,-20.8747508327259,-15.6546706931166));
#81695=CARTESIAN_POINT('Ctrl Pts',(19.5566267091408,-20.9031514793808,-15.659219545964));
#81696=CARTESIAN_POINT('Ctrl Pts',(19.5150427438893,-20.9201663677265,-15.6621813381257));
#81697=CARTESIAN_POINT('Ctrl Pts',(19.3704830766048,-20.97401249267,-15.6723715694895));
#81698=CARTESIAN_POINT('Ctrl Pts',(19.2652050146525,-21.0041866207842,-15.6796016017227));
#81699=CARTESIAN_POINT('Ctrl Pts',(19.1041215629254,-21.0371211305131,-15.6901694386007));
#81700=CARTESIAN_POINT('Ctrl Pts',(19.0497690453268,-21.0460417449079,-15.6936556397206));
#81701=CARTESIAN_POINT('Ctrl Pts',(18.9611055328422,-21.0570623259829,-15.6992090807324));
#81702=CARTESIAN_POINT('Ctrl Pts',(18.9269852576525,-21.0604641864612,-15.7013146882049));
#81703=CARTESIAN_POINT('Ctrl Pts',(18.8820200993857,-21.0638465432519,-15.7040498464714));
#81704=CARTESIAN_POINT('Ctrl Pts',(18.8712382291001,-21.0645746015991,-15.7047027093586));
#81705=CARTESIAN_POINT('Ctrl Pts',(18.8535659120658,-21.0656320796666,-15.7057680372571));
#81706=CARTESIAN_POINT('Ctrl Pts',(18.8466786915673,-21.0660104280117,-15.7061820307599));
#81707=CARTESIAN_POINT('Ctrl Pts',(18.8333408041358,-21.0666777761061,-15.7069815267012));
#81708=CARTESIAN_POINT('Ctrl Pts',(18.8268904305926,-21.0669709363141,-15.7073671552684));
#81709=CARTESIAN_POINT('Ctrl Pts',(18.8119899272544,-21.0675798432687,-15.7082556609591));
#81710=CARTESIAN_POINT('Ctrl Pts',(18.8035390090154,-21.0678744838453,-15.7087578716069));
#81711=CARTESIAN_POINT('Ctrl Pts',(18.7807983235475,-21.0685309442126,-15.7101048072834));
#81712=CARTESIAN_POINT('Ctrl Pts',(18.7665061264124,-21.0687986884836,-15.710946588652));
#81713=CARTESIAN_POINT('Ctrl Pts',(18.6350479192716,-21.069929634011,-15.7186480889499));
#81714=CARTESIAN_POINT('Ctrl Pts',(18.5179952260785,-21.0612094921747,-15.7251891787752));
#81715=CARTESIAN_POINT('Ctrl Pts',(18.2404051985606,-21.0171651317415,-15.7405741040444));
#81716=CARTESIAN_POINT('Ctrl Pts',(18.0821079303989,-20.972783815009,-15.7492315240695));
#81717=CARTESIAN_POINT('Ctrl Pts',(17.9016682142281,-20.8987629912337,-15.7604463261497));
#81718=CARTESIAN_POINT('Ctrl Pts',(17.873071016026,-20.8862862759913,-15.7622678426905));
#81719=CARTESIAN_POINT('Ctrl Pts',(17.8382748875729,-20.870180548458,-15.7645512755516));
#81720=CARTESIAN_POINT('Ctrl Pts',(17.8318034371261,-20.8671452822531,-15.7649788474803));
#81721=CARTESIAN_POINT('Ctrl Pts',(17.8216539277324,-20.862322058866,-15.7656541828522));
#81722=CARTESIAN_POINT('Ctrl Pts',(17.8179653976249,-20.8605560853097,-15.7659006048208));
#81723=CARTESIAN_POINT('Ctrl Pts',(17.811062020589,-20.8572263033511,-15.7663637072348));
#81724=CARTESIAN_POINT('Ctrl Pts',(17.8078460100684,-20.8556650354194,-15.766580229846));
#81725=CARTESIAN_POINT('Ctrl Pts',(17.8004896175149,-20.8520706939302,-15.7670772915019));
#81726=CARTESIAN_POINT('Ctrl Pts',(17.7963519275842,-20.8500322356339,-15.7673581630583));
#81727=CARTESIAN_POINT('Ctrl Pts',(17.7855281762086,-20.844655817947,-15.7680962215253));
#81728=CARTESIAN_POINT('Ctrl Pts',(17.7788531372778,-20.8412959833172,-15.7685547244682));
#81729=CARTESIAN_POINT('Ctrl Pts',(17.734172197797,-20.8185088372921,-15.7716455918281));
#81730=CARTESIAN_POINT('Ctrl Pts',(17.6967462941565,-20.7979726583724,-15.7743405541364));
#81731=CARTESIAN_POINT('Ctrl Pts',(17.6537625704002,-20.7726669046396,-15.7775396716289));
#81732=CARTESIAN_POINT('Ctrl Pts',(17.6475742249394,-20.7689809892071,-15.7780028293955));
#81733=CARTESIAN_POINT('Ctrl Pts',(17.5067332157273,-20.6841162183012,-15.7886010738821));
#81734=CARTESIAN_POINT('Ctrl Pts',(17.3815204063515,-20.5882189996179,-15.7991743274516));
#81735=CARTESIAN_POINT('Ctrl Pts',(17.1996368762811,-20.4136489959253,-15.8155534556939));
#81736=CARTESIAN_POINT('Ctrl Pts',(17.1356824252017,-20.3434284383633,-15.8215790815982));
#81737=CARTESIAN_POINT('Ctrl Pts',(17.0633767559959,-20.2524468135082,-15.8287171598595));
#81738=CARTESIAN_POINT('Ctrl Pts',(17.0503589583529,-20.2355485317303,-15.830017206774));
#81739=CARTESIAN_POINT('Ctrl Pts',(17.0322147374942,-20.2112445779466,-15.8318514329844));
#81740=CARTESIAN_POINT('Ctrl Pts',(17.0268770680754,-20.2039989161242,-15.8323938663043));
#81741=CARTESIAN_POINT('Ctrl Pts',(17.0177495690668,-20.1914418205486,-15.8333264533301));
#81742=CARTESIAN_POINT('Ctrl Pts',(17.0139378247976,-20.1861465403754,-15.8337174542962));
#81743=CARTESIAN_POINT('Ctrl Pts',(17.0066870490848,-20.1759749071547,-15.8344642324701));
#81744=CARTESIAN_POINT('Ctrl Pts',(17.00324404074,-20.1711014782833,-15.8348201605029));
#81745=CARTESIAN_POINT('Ctrl Pts',(16.9943461598524,-20.1583932419596,-15.8357434985385));
#81746=CARTESIAN_POINT('Ctrl Pts',(16.9889235584248,-20.1505359216073,-15.8363096724455));
#81747=CARTESIAN_POINT('Ctrl Pts',(16.9706219367321,-20.1236294342209,-15.8382327302425));
#81748=CARTESIAN_POINT('Ctrl Pts',(16.957999916433,-20.1044068245473,-15.8395799220599));
#81749=CARTESIAN_POINT('Ctrl Pts',(16.8645247607842,-19.9568649544033,-15.8497291340341));
#81750=CARTESIAN_POINT('Ctrl Pts',(16.7973961928405,-19.8204578628901,-15.857987038895));
#81751=CARTESIAN_POINT('Ctrl Pts',(16.7454194501833,-19.6781104577752,-15.8662164286365));
#81752=CARTESIAN_POINT('',(16.6170002518852,-18.9530327061848,-14.8907771671312));
#81753=CARTESIAN_POINT('Ctrl Pts',(16.7454194499636,-19.6781104571738,-15.6464962048466));
#81754=CARTESIAN_POINT('Ctrl Pts',(16.7464618210687,-19.6809651728509,-15.646314725492));
#81755=CARTESIAN_POINT('Ctrl Pts',(16.7475103329493,-19.6838176265005,-15.6461328989071));
#81756=CARTESIAN_POINT('Ctrl Pts',(16.7501831766152,-19.6910409693967,-15.6456711856327));
#81757=CARTESIAN_POINT('Ctrl Pts',(16.7518158016566,-19.6954087341947,-15.6453908199843));
#81758=CARTESIAN_POINT('Ctrl Pts',(16.7547310336525,-19.7031299819739,-15.6448930447428));
#81759=CARTESIAN_POINT('Ctrl Pts',(16.756007757495,-19.7064856389605,-15.6446759886965));
#81760=CARTESIAN_POINT('Ctrl Pts',(16.7587298590321,-19.7135858325257,-15.6442151686796));
#81761=CARTESIAN_POINT('Ctrl Pts',(16.7601773285189,-19.717329452609,-15.6439712857206));
#81762=CARTESIAN_POINT('Ctrl Pts',(16.764107895231,-19.7274098375799,-15.6433121671797));
#81763=CARTESIAN_POINT('Ctrl Pts',(16.7666108941802,-19.7337387185235,-15.6428957624867));
#81764=CARTESIAN_POINT('Ctrl Pts',(16.7791207397704,-19.7649294743618,-15.6408312027123));
#81765=CARTESIAN_POINT('Ctrl Pts',(16.7895680676519,-19.7896106239208,-15.6391585752494));
#81766=CARTESIAN_POINT('Ctrl Pts',(16.8210382187307,-19.860193131573,-15.6342757155358));
#81767=CARTESIAN_POINT('Ctrl Pts',(16.8432373327428,-19.9055477946504,-15.6310148770947));
#81768=CARTESIAN_POINT('Ctrl Pts',(16.9295816576105,-20.0670626117623,-15.619052347282));
#81769=CARTESIAN_POINT('Ctrl Pts',(17.0029892562356,-20.1779261337073,-15.6101841445996));
#81770=CARTESIAN_POINT('Ctrl Pts',(17.1511162416845,-20.3615483824414,-15.5948582182858));
#81771=CARTESIAN_POINT('Ctrl Pts',(17.2217357575043,-20.4370622810837,-15.5883172728628));
#81772=CARTESIAN_POINT('Ctrl Pts',(17.307910783786,-20.5166583496608,-15.581156619092));
#81773=CARTESIAN_POINT('Ctrl Pts',(17.318321337597,-20.5260839061179,-15.5803038107971));
#81774=CARTESIAN_POINT('Ctrl Pts',(17.3350950535345,-20.5409695475882,-15.5789489182868));
#81775=CARTESIAN_POINT('Ctrl Pts',(17.341398060896,-20.5464965082337,-15.578444033336));
#81776=CARTESIAN_POINT('Ctrl Pts',(17.3526049390228,-20.5562064162179,-15.5775537326945));
#81777=CARTESIAN_POINT('Ctrl Pts',(17.3574953646269,-20.5604046538568,-15.5771676843011));
#81778=CARTESIAN_POINT('Ctrl Pts',(17.367682196607,-20.5690691566743,-15.5763685822068));
#81779=CARTESIAN_POINT('Ctrl Pts',(17.3729815138332,-20.5735318928106,-15.5759556763934));
#81780=CARTESIAN_POINT('Ctrl Pts',(17.3867089328402,-20.5849775168373,-15.5748932001708));
#81781=CARTESIAN_POINT('Ctrl Pts',(17.395169517965,-20.5919212594894,-15.5742452275677));
#81782=CARTESIAN_POINT('Ctrl Pts',(17.431306814496,-20.6211136683047,-15.5715060245732));
#81783=CARTESIAN_POINT('Ctrl Pts',(17.459488095506,-20.6427304917977,-15.5694401327033));
#81784=CARTESIAN_POINT('Ctrl Pts',(17.534931611253,-20.6976415973162,-15.5640773286126));
#81785=CARTESIAN_POINT('Ctrl Pts',(17.5830375216308,-20.7297276755951,-15.5608243468964));
#81786=CARTESIAN_POINT('Ctrl Pts',(17.7707930760212,-20.8441379628006,-15.5486248535451));
#81787=CARTESIAN_POINT('Ctrl Pts',(17.9184014546629,-20.9122926399963,-15.5400738392206));
#81788=CARTESIAN_POINT('Ctrl Pts',(18.0929192853502,-20.9697151258336,-15.5298130920824));
#81789=CARTESIAN_POINT('Ctrl Pts',(18.1136108022514,-20.9761729184677,-15.5285935048515));
#81790=CARTESIAN_POINT('Ctrl Pts',(18.1746751932879,-20.9942067886059,-15.5249758342402));
#81791=CARTESIAN_POINT('Ctrl Pts',(18.21529521678,-21.0048998087632,-15.5225459165641));
#81792=CARTESIAN_POINT('Ctrl Pts',(18.2634485539831,-21.0160556315644,-15.5196092817676));
#81793=CARTESIAN_POINT('Ctrl Pts',(18.2707026383087,-21.0176959758177,-15.5191654058786));
#81794=CARTESIAN_POINT('Ctrl Pts',(18.2824589206213,-21.0202893489095,-15.5184434191252));
#81795=CARTESIAN_POINT('Ctrl Pts',(18.286955918693,-21.0212659968284,-15.5181666261419));
#81796=CARTESIAN_POINT('Ctrl Pts',(18.29495096904,-21.0229750653415,-15.5176733684641));
#81797=CARTESIAN_POINT('Ctrl Pts',(18.2984477280889,-21.0237132984725,-15.5174572398138));
#81798=CARTESIAN_POINT('Ctrl Pts',(18.3059565595425,-21.025278706175,-15.516992268415));
#81799=CARTESIAN_POINT('Ctrl Pts',(18.3099691085308,-21.0261030791211,-15.5167432751951));
#81800=CARTESIAN_POINT('Ctrl Pts',(18.3210204078847,-21.0283401447055,-15.5160561112889));
#81801=CARTESIAN_POINT('Ctrl Pts',(18.3280639146646,-21.0297286712271,-15.5156165988955));
#81802=CARTESIAN_POINT('Ctrl Pts',(18.3661847034743,-21.0370424015846,-15.5132300037682));
#81803=CARTESIAN_POINT('Ctrl Pts',(18.3973830193666,-21.0423058791424,-15.5112485906621));
#81804=CARTESIAN_POINT('Ctrl Pts',(18.5904483669883,-21.0704439978995,-15.4988614468198));
#81805=CARTESIAN_POINT('Ctrl Pts',(18.7543926853166,-21.0752041806364,-15.4878510943337));
#81806=CARTESIAN_POINT('Ctrl Pts',(19.0338618070423,-21.0509218147031,-15.4695259693753));
#81807=CARTESIAN_POINT('Ctrl Pts',(19.1494464943902,-21.0311349041748,-15.4620691876712));
#81808=CARTESIAN_POINT('Ctrl Pts',(19.2766584371441,-20.9983174473749,-15.4540472948938));
#81809=CARTESIAN_POINT('Ctrl Pts',(19.2904615647938,-20.994607112851,-15.453179126206));
#81810=CARTESIAN_POINT('Ctrl Pts',(19.3123692430935,-20.9884796863122,-15.4518045712465));
#81811=CARTESIAN_POINT('Ctrl Pts',(19.3204985289586,-20.9861533798828,-15.4512952552727));
#81812=CARTESIAN_POINT('Ctrl Pts',(19.3348106924406,-20.9819648280142,-15.4503998127639));
#81813=CARTESIAN_POINT('Ctrl Pts',(19.3409993553586,-20.9801228944896,-15.4500130298047));
#81814=CARTESIAN_POINT('Ctrl Pts',(19.3537815600591,-20.976254775446,-15.4492149734379));
#81815=CARTESIAN_POINT('Ctrl Pts',(19.3603738273923,-20.9742246186303,-15.4488038352554));
#81816=CARTESIAN_POINT('Ctrl Pts',(19.3772687434226,-20.9689311129403,-15.4477512460136));
#81817=CARTESIAN_POINT('Ctrl Pts',(19.3875566197258,-20.965621002567,-15.4471113355632));
#81818=CARTESIAN_POINT('Ctrl Pts',(19.430379956665,-20.9514798810135,-15.4444516256623));
#81819=CARTESIAN_POINT('Ctrl Pts',(19.462676266121,-20.9399376082191,-15.4424553333884));
#81820=CARTESIAN_POINT('Ctrl Pts',(19.5460739492627,-20.9078266536128,-15.4373138949028));
#81821=CARTESIAN_POINT('Ctrl Pts',(19.5966791399523,-20.8860391267957,-15.434208084708));
#81822=CARTESIAN_POINT('Ctrl Pts',(19.7450257999569,-20.8151872147673,-15.4250667253287));
#81823=CARTESIAN_POINT('Ctrl Pts',(19.8398767713543,-20.7605013737198,-15.4191799156477));
#81824=CARTESIAN_POINT('Ctrl Pts',(19.9655431323308,-20.6744511242105,-15.4108879478435));
#81825=CARTESIAN_POINT('Ctrl Pts',(20.0002580291228,-20.649093626091,-15.4085384512978));
#81826=CARTESIAN_POINT('Ctrl Pts',(20.0938029621756,-20.5762947740697,-15.4019765739369));
#81827=CARTESIAN_POINT('Ctrl Pts',(20.1508964488008,-20.5267379112893,-15.3977073727041));
#81828=CARTESIAN_POINT('Ctrl Pts',(20.2120392649715,-20.467644767645,-15.3926678153139));
#81829=CARTESIAN_POINT('Ctrl Pts',(20.2188211745769,-20.4610013924521,-15.3921019241724));
#81830=CARTESIAN_POINT('Ctrl Pts',(20.2288083491485,-20.4510857139536,-15.3912578532898));
#81831=CARTESIAN_POINT('Ctrl Pts',(20.2320481543938,-20.4478481556217,-15.3909823437547));
#81832=CARTESIAN_POINT('Ctrl Pts',(20.2377957075304,-20.4420671890166,-15.3904904932399));
#81833=CARTESIAN_POINT('Ctrl Pts',(20.2403075502035,-20.4395279230118,-15.390274481031));
#81834=CARTESIAN_POINT('Ctrl Pts',(20.2456963630598,-20.4340526315139,-15.3898087557144));
#81835=CARTESIAN_POINT('Ctrl Pts',(20.2485711696053,-20.4311146230777,-15.389558886848));
#81836=CARTESIAN_POINT('Ctrl Pts',(20.2564882208778,-20.4229762356269,-15.3888668906742));
#81837=CARTESIAN_POINT('Ctrl Pts',(20.2615123043431,-20.4177583788191,-15.3884233908925));
#81838=CARTESIAN_POINT('Ctrl Pts',(20.2889763028575,-20.3889405723166,-15.3859754209218));
#81839=CARTESIAN_POINT('Ctrl Pts',(20.3108948352396,-20.3648524054532,-15.3839345442539));
#81840=CARTESIAN_POINT('Ctrl Pts',(20.4389281076429,-20.2174539255712,-15.3715279130892));
#81841=CARTESIAN_POINT('Ctrl Pts',(20.5310941521381,-20.0827546295301,-15.3605727186579));
#81842=CARTESIAN_POINT('Ctrl Pts',(20.6613730510475,-19.8354957893216,-15.3423172744141));
#81843=CARTESIAN_POINT('Ctrl Pts',(20.7071813389951,-19.7278188547983,-15.334877080425));
#81844=CARTESIAN_POINT('Ctrl Pts',(20.7483642047674,-19.603329434519,-15.3268706247309));
#81845=CARTESIAN_POINT('Ctrl Pts',(20.7527146989843,-19.5897179325849,-15.3260026566042));
#81846=CARTESIAN_POINT('Ctrl Pts',(20.7594193959784,-19.5679843736217,-15.3246283581713));
#81847=CARTESIAN_POINT('Ctrl Pts',(20.7618632717442,-19.5598906418935,-15.3241190998638));
#81848=CARTESIAN_POINT('Ctrl Pts',(20.7660879209208,-19.5455902381051,-15.3232237244325));
#81849=CARTESIAN_POINT('Ctrl Pts',(20.7678888954473,-19.5393896930787,-15.3228369511937));
#81850=CARTESIAN_POINT('Ctrl Pts',(20.7715552206011,-19.5265479147972,-15.3220388820318));
#81851=CARTESIAN_POINT('Ctrl Pts',(20.7734165371927,-19.5199056021499,-15.3216277214958));
#81852=CARTESIAN_POINT('Ctrl Pts',(20.7781109544491,-19.5028323104883,-15.3205750070277));
#81853=CARTESIAN_POINT('Ctrl Pts',(20.7808967178448,-19.4923884356752,-15.3199349944245));
#81854=CARTESIAN_POINT('Ctrl Pts',(20.7921897536862,-19.4487099953196,-15.3172742918244));
#81855=CARTESIAN_POINT('Ctrl Pts',(20.7999688277064,-19.4152913566914,-15.3152771314083));
#81856=CARTESIAN_POINT('Ctrl Pts',(20.8181177584978,-19.3277377675104,-15.3101329516797));
#81857=CARTESIAN_POINT('Ctrl Pts',(20.827192324167,-19.2733599861546,-15.3070253234151));
#81858=CARTESIAN_POINT('Ctrl Pts',(20.8479099511833,-19.1102105665311,-15.2978807920945));
#81859=CARTESIAN_POINT('Ctrl Pts',(20.8532599347427,-19.0008270167028,-15.2919926180276));
#81860=CARTESIAN_POINT('Ctrl Pts',(20.8488264569386,-18.8457035655288,-15.2835435935355));
#81861=CARTESIAN_POINT('Ctrl Pts',(20.8460294166224,-18.799942842889,-15.2810373870488));
#81862=CARTESIAN_POINT('Ctrl Pts',(20.8396445421111,-18.7318678535178,-15.2772457724828));
#81863=CARTESIAN_POINT('Ctrl Pts',(20.8371813577142,-18.7094608772383,-15.2759874206289));
#81864=CARTESIAN_POINT('Ctrl Pts',(20.8335646191318,-18.6807843904216,-15.2743590646324));
#81865=CARTESIAN_POINT('Ctrl Pts',(20.832739865342,-18.6744743740556,-15.273999642275));
#81866=CARTESIAN_POINT('Ctrl Pts',(20.8258023941404,-18.6231974214837,-15.2710691176888));
#81867=CARTESIAN_POINT('Ctrl Pts',(20.8182741464527,-18.578437396997,-15.2684500502094));
#81868=CARTESIAN_POINT('Ctrl Pts',(20.8078120118602,-18.526499567822,-15.2653035776034));
#81869=CARTESIAN_POINT('Ctrl Pts',(20.8062695433121,-18.5190498709481,-15.2648496596602));
#81870=CARTESIAN_POINT('Ctrl Pts',(20.8037293599071,-18.5071061163287,-15.2641174950169));
#81871=CARTESIAN_POINT('Ctrl Pts',(20.8027570659559,-18.5026066398684,-15.2638406631855));
#81872=CARTESIAN_POINT('Ctrl Pts',(20.8010019881233,-18.4946110884284,-15.2633468806029));
#81873=CARTESIAN_POINT('Ctrl Pts',(20.8002249966559,-18.4911137902387,-15.2631302638108));
#81874=CARTESIAN_POINT('Ctrl Pts',(20.7985511656071,-18.4836690587019,-15.2626677798618));
#81875=CARTESIAN_POINT('Ctrl Pts',(20.7976518945992,-18.4797222816298,-15.2624217805373));
#81876=CARTESIAN_POINT('Ctrl Pts',(20.7951756506108,-18.4689965017218,-15.2617510760597));
#81877=CARTESIAN_POINT('Ctrl Pts',(20.7935765735611,-18.4622227276084,-15.2613251317179));
#81878=CARTESIAN_POINT('Ctrl Pts',(20.7852143222332,-18.4275650067871,-15.2591341058772));
#81879=CARTESIAN_POINT('Ctrl Pts',(20.7779185197208,-18.3998142035234,-15.2573408876463));
#81880=CARTESIAN_POINT('Ctrl Pts',(20.7547512141243,-18.3184553916971,-15.2519855954401));
#81881=CARTESIAN_POINT('Ctrl Pts',(20.737318225969,-18.2653199675577,-15.2483615798352));
#81882=CARTESIAN_POINT('Ctrl Pts',(20.6690492547427,-18.0820704260946,-15.2355500629643));
#81883=CARTESIAN_POINT('Ctrl Pts',(20.6074582691765,-17.956333248364,-15.2262198423816));
#81884=CARTESIAN_POINT('Ctrl Pts',(20.4869333088051,-17.7616704259775,-15.211445076017));
#81885=CARTESIAN_POINT('Ctrl Pts',(20.4351764773242,-17.6888048920255,-15.2058201901091));
#81886=CARTESIAN_POINT('Ctrl Pts',(20.3703433829837,-17.6087736734458,-15.1995360879001));
#81887=CARTESIAN_POINT('Ctrl Pts',(20.3616177711602,-17.5982138144338,-15.1987045115429));
#81888=CARTESIAN_POINT('Ctrl Pts',(20.3474530788473,-17.5814064241127,-15.1973768501526));
#81889=CARTESIAN_POINT('Ctrl Pts',(20.3420788674547,-17.5751049615185,-15.1968781383255));
#81890=CARTESIAN_POINT('Ctrl Pts',(20.3324668673792,-17.5639675744327,-15.1959949566643));
#81891=CARTESIAN_POINT('Ctrl Pts',(20.3282437901353,-17.5591191438014,-15.195609887017));
#81892=CARTESIAN_POINT('Ctrl Pts',(20.3193946534816,-17.549052595502,-15.1948091032061));
#81893=CARTESIAN_POINT('Ctrl Pts',(20.3147647625277,-17.5438379374466,-15.1943935553569));
#81894=CARTESIAN_POINT('Ctrl Pts',(20.302665057392,-17.5303448856863,-15.1933163496394));
#81895=CARTESIAN_POINT('Ctrl Pts',(20.29515539482,-17.5221023929127,-15.1926563761632));
#81896=CARTESIAN_POINT('Ctrl Pts',(20.2621732122885,-17.4864712255106,-15.1897943605675));
#81897=CARTESIAN_POINT('Ctrl Pts',(20.2360415735037,-17.4596999900685,-15.1876206357482));
#81898=CARTESIAN_POINT('Ctrl Pts',(20.1646403548181,-17.3903280428261,-15.181908265251));
#81899=CARTESIAN_POINT('Ctrl Pts',(20.1181803061272,-17.349003781144,-15.1784214398209));
#81900=CARTESIAN_POINT('Ctrl Pts',(19.9663676309826,-17.2255021967237,-15.167597607391));
#81901=CARTESIAN_POINT('Ctrl Pts',(19.855030535987,-17.1512185487875,-15.1604808644335));
#81902=CARTESIAN_POINT('Ctrl Pts',(19.6640639489695,-17.0484206722914,-15.1485261417979));
#81903=CARTESIAN_POINT('Ctrl Pts',(19.5884279754497,-17.0132935445388,-15.1438419294371));
#81904=CARTESIAN_POINT('Ctrl Pts',(19.5020093978761,-16.9791993224962,-15.1383369991295));
#81905=CARTESIAN_POINT('Ctrl Pts',(19.4930659005399,-16.9757409331756,-15.1377655029824));
#81906=CARTESIAN_POINT('Ctrl Pts',(19.4797988862489,-16.9707140108053,-15.1369146581061));
#81907=CARTESIAN_POINT('Ctrl Pts',(19.4754931123857,-16.9690985619355,-15.1366380421839));
#81908=CARTESIAN_POINT('Ctrl Pts',(19.4678322038706,-16.9662527685321,-15.1361449790827));
#81909=CARTESIAN_POINT('Ctrl Pts',(19.4644791830265,-16.9650168763513,-15.1359288669445));
#81910=CARTESIAN_POINT('Ctrl Pts',(19.4572740091007,-16.9623818195544,-15.1354637935784));
#81911=CARTESIAN_POINT('Ctrl Pts',(19.4534209749595,-16.9609853701365,-15.1352146811577));
#81912=CARTESIAN_POINT('Ctrl Pts',(19.4427991126033,-16.9571705627356,-15.1345268599629));
#81913=CARTESIAN_POINT('Ctrl Pts',(19.4360220584232,-16.9547755028851,-15.1340868053146));
#81914=CARTESIAN_POINT('Ctrl Pts',(19.3992330326576,-16.9419843751326,-15.1316919738592));
#81915=CARTESIAN_POINT('Ctrl Pts',(19.3690038942946,-16.9322308046017,-15.1297025917515));
#81916=CARTESIAN_POINT('Ctrl Pts',(19.1820076956383,-16.8765082501724,-15.1173129046644));
#81917=CARTESIAN_POINT('Ctrl Pts',(19.0205774493177,-16.8481344881915,-15.1063100349775));
#81918=CARTESIAN_POINT('Ctrl Pts',(18.7406727451833,-16.8317788387786,-15.0879942660418));
#81919=CARTESIAN_POINT('Ctrl Pts',(18.6234743744695,-16.8346492426108,-15.0805396456059));
#81920=CARTESIAN_POINT('Ctrl Pts',(18.4928870449473,-16.848726882749,-15.0725197636851));
#81921=CARTESIAN_POINT('Ctrl Pts',(18.4786929316005,-16.8504026124406,-15.0716516208191));
#81922=CARTESIAN_POINT('Ctrl Pts',(18.4561300844777,-16.8532983055921,-15.0702770988864));
#81923=CARTESIAN_POINT('Ctrl Pts',(18.4477500014746,-16.8544248681758,-15.0697677903367));
#81924=CARTESIAN_POINT('Ctrl Pts',(18.4329827849576,-16.8565002202061,-15.0688723564639));
#81925=CARTESIAN_POINT('Ctrl Pts',(18.4265928636803,-16.8574280759924,-15.0684855747564));
#81926=CARTESIAN_POINT('Ctrl Pts',(18.4133856892092,-16.859407578504,-15.0676875167435));
#81927=CARTESIAN_POINT('Ctrl Pts',(18.4065691230234,-16.8604633397141,-15.067276375684));
#81928=CARTESIAN_POINT('Ctrl Pts',(18.3890861295657,-16.8632587002088,-15.0662237703251));
#81929=CARTESIAN_POINT('Ctrl Pts',(18.3784275594396,-16.865046708347,-15.0655838467272));
#81930=CARTESIAN_POINT('Ctrl Pts',(18.3340075361081,-16.8728484899745,-15.0629240090824));
#81931=CARTESIAN_POINT('Ctrl Pts',(18.3003799080524,-16.8796007177522,-15.0609276050943));
#81932=CARTESIAN_POINT('Ctrl Pts',(18.2132099163893,-16.8993187867546,-15.0557858138884));
#81933=CARTESIAN_POINT('Ctrl Pts',(18.159982371913,-16.9135626373115,-15.0526797697658));
#81934=CARTESIAN_POINT('Ctrl Pts',(18.0045299079525,-16.9617352896282,-15.0436303373786));
#81935=CARTESIAN_POINT('Ctrl Pts',(17.9042699295139,-17.0014028728595,-15.0378294711641));
#81936=CARTESIAN_POINT('Ctrl Pts',(17.6993569682821,-17.1011465049066,-15.0254258979975));
#81937=CARTESIAN_POINT('Ctrl Pts',(17.5959457510176,-17.1628748053974,-15.0188285157138));
#81938=CARTESIAN_POINT('Ctrl Pts',(17.4906332544539,-17.2385769950746,-15.0111418617979));
#81939=CARTESIAN_POINT('Ctrl Pts',(17.4829566618978,-17.2441739502166,-15.0105755764535));
#81940=CARTESIAN_POINT('Ctrl Pts',(17.4716343678639,-17.2525462638494,-15.0097310289831));
#81941=CARTESIAN_POINT('Ctrl Pts',(17.4679594639195,-17.2552821829749,-15.0094554414432));
#81942=CARTESIAN_POINT('Ctrl Pts',(17.4615604238182,-17.2600785504742,-15.0089729369825));
#81943=CARTESIAN_POINT('Ctrl Pts',(17.4588323581629,-17.2621336882941,-15.0087663927705));
#81944=CARTESIAN_POINT('Ctrl Pts',(17.452943447302,-17.2665923708874,-15.0083187004817));
#81945=CARTESIAN_POINT('Ctrl Pts',(17.449784434805,-17.2689981732058,-15.0080773971103));
#81946=CARTESIAN_POINT('Ctrl Pts',(17.4413944857164,-17.275425063839,-15.0074335109115));
#81947=CARTESIAN_POINT('Ctrl Pts',(17.4361755967001,-17.2794617051716,-15.0070298542132));
#81948=CARTESIAN_POINT('Ctrl Pts',(17.4245780164326,-17.2885190220691,-15.0061259843416));
#81949=CARTESIAN_POINT('Ctrl Pts',(17.4182091937257,-17.2935520977632,-15.005624956281));
#81950=CARTESIAN_POINT('Ctrl Pts',(17.3989854179596,-17.3089244640379,-15.0040988344534));
#81951=CARTESIAN_POINT('Ctrl Pts',(17.386222530684,-17.3193772607058,-15.0030667305062));
#81952=CARTESIAN_POINT('Ctrl Pts',(17.3390421698338,-17.3589481986043,-14.9991842798635));
#81953=CARTESIAN_POINT('Ctrl Pts',(17.3054371382018,-17.389012789395,-14.9962835857847));
#81954=CARTESIAN_POINT('Ctrl Pts',(17.2178843621736,-17.4725250841375,-14.9884087002875));
#81955=CARTESIAN_POINT('Ctrl Pts',(17.1658090434186,-17.5278408855327,-14.9833808222618));
#81956=CARTESIAN_POINT('Ctrl Pts',(17.0169246971401,-17.704080583839,-14.9681409955478));
#81957=CARTESIAN_POINT('Ctrl Pts',(16.9302842240295,-17.8329484910158,-14.9580560622777));
#81958=CARTESIAN_POINT('Ctrl Pts',(16.8473597513694,-17.9913486797774,-14.9470407091089));
#81959=CARTESIAN_POINT('Ctrl Pts',(16.8366142124931,-18.0127504942487,-14.9455780235587));
#81960=CARTESIAN_POINT('Ctrl Pts',(16.8220268664709,-18.0430765031995,-14.9435403616427));
#81961=CARTESIAN_POINT('Ctrl Pts',(16.8178801298435,-18.0518512153695,-14.9429548176323));
#81962=CARTESIAN_POINT('Ctrl Pts',(16.8112693089261,-18.0660927587062,-14.9420109046922));
#81963=CARTESIAN_POINT('Ctrl Pts',(16.8087678885144,-18.0715420120025,-14.9416512481585));
#81964=CARTESIAN_POINT('Ctrl Pts',(16.8036027000191,-18.0829214504145,-14.9409033115526));
#81965=CARTESIAN_POINT('Ctrl Pts',(16.8009430254914,-18.0888534331407,-14.9405151754291));
#81966=CARTESIAN_POINT('Ctrl Pts',(16.7947203172894,-18.1029052254155,-14.9395998444167));
#81967=CARTESIAN_POINT('Ctrl Pts',(16.7911808725664,-18.1110353956771,-14.9390734615493));
#81968=CARTESIAN_POINT('Ctrl Pts',(16.7796053354061,-18.1380877733401,-14.9373324198111));
#81969=CARTESIAN_POINT('Ctrl Pts',(16.7717936293248,-18.1571051512969,-14.9361253861798));
#81970=CARTESIAN_POINT('Ctrl Pts',(16.7318168056899,-18.2586098969516,-14.929767399564));
#81971=CARTESIAN_POINT('Ctrl Pts',(16.7045710054868,-18.3429450653894,-14.9247836181472));
#81972=CARTESIAN_POINT('Ctrl Pts',(16.6389736200311,-18.6001072463063,-14.9101349325607));
#81973=CARTESIAN_POINT('Ctrl Pts',(16.6169140090866,-18.7762389717622,-14.9008598182712));
#81974=CARTESIAN_POINT('Ctrl Pts',(16.6170002518852,-18.9530327061848,-14.8907771671312));
#81975=CARTESIAN_POINT('Ctrl Pts',(16.6170002532685,-18.9530355380041,-14.8907770056308));
#81976=CARTESIAN_POINT('Ctrl Pts',(16.6170133611375,-18.9798325798375,-14.8892487531684));
#81977=CARTESIAN_POINT('Ctrl Pts',(16.6175352642842,-19.0066259871557,-14.8877018039767));
#81978=CARTESIAN_POINT('Ctrl Pts',(16.6191227654136,-19.0478815541535,-14.8852809856311));
#81979=CARTESIAN_POINT('Ctrl Pts',(16.6198286097373,-19.0623553210824,-14.8844242982576));
#81980=CARTESIAN_POINT('Ctrl Pts',(16.6209600190508,-19.0815110785819,-14.8832793646105));
#81981=CARTESIAN_POINT('Ctrl Pts',(16.6212526903976,-19.0862009142593,-14.8829981706578));
#81982=CARTESIAN_POINT('Ctrl Pts',(16.6217938179313,-19.0944311792435,-14.8825030866471));
#81983=CARTESIAN_POINT('Ctrl Pts',(16.6220355693814,-19.0979720513336,-14.8822895645769));
#81984=CARTESIAN_POINT('Ctrl Pts',(16.6225281743406,-19.1049296119789,-14.8818689494618));
#81985=CARTESIAN_POINT('Ctrl Pts',(16.6227784202662,-19.108346339654,-14.8816618899991));
#81986=CARTESIAN_POINT('Ctrl Pts',(16.6233330673721,-19.1156749674767,-14.8812166601339));
#81987=CARTESIAN_POINT('Ctrl Pts',(16.6236400494739,-19.1195866167188,-14.8809783487989));
#81988=CARTESIAN_POINT('Ctrl Pts',(16.6244765273345,-19.1298783411693,-14.8803496173194));
#81989=CARTESIAN_POINT('Ctrl Pts',(16.625024088128,-19.1362568497938,-14.8799582038806));
#81990=CARTESIAN_POINT('Ctrl Pts',(16.627416796096,-19.1627202247775,-14.8783273285818));
#81991=CARTESIAN_POINT('Ctrl Pts',(16.6295199328799,-19.1827799525984,-14.8770744345601));
#81992=CARTESIAN_POINT('Ctrl Pts',(16.6324142606028,-19.2070383307557,-14.8755415570272));
#81993=CARTESIAN_POINT('Ctrl Pts',(16.6329320449516,-19.2112693924791,-14.8752735421504));
#81994=CARTESIAN_POINT('Ctrl Pts',(16.6366907709949,-19.241232883062,-14.8733710028631));
#81995=CARTESIAN_POINT('Ctrl Pts',(16.6403914468671,-19.2669043921709,-14.8717174068611));
#81996=CARTESIAN_POINT('Ctrl Pts',(16.6659945805772,-19.4240148036282,-14.861477304345));
#81997=CARTESIAN_POINT('Ctrl Pts',(16.6997789103089,-19.5531158497064,-14.8525677425466));
#81998=CARTESIAN_POINT('Ctrl Pts',(16.7454194444943,-19.6781104421951,-14.843838520965));
#81999=CARTESIAN_POINT('Origin',(18.734,-18.952,0.));
#82000=CARTESIAN_POINT('',(16.7454194457665,-19.6781104456791,-14.0426552583743));
#82001=CARTESIAN_POINT('',(16.7454194499637,-19.6781104571739,-14.2664527091733));
#82002=CARTESIAN_POINT('',(16.7454194499637,-19.6781104571739,0.));
#82003=CARTESIAN_POINT('',(16.6195738444081,-18.9515327933745,-14.3109440134329));
#82004=CARTESIAN_POINT('Ctrl Pts',(16.7454194499637,-19.6781104571739,-14.2664527091733));
#82005=CARTESIAN_POINT('Ctrl Pts',(16.719650694312,-19.6075382105118,-14.2709758243854));
#82006=CARTESIAN_POINT('Ctrl Pts',(16.6976093484952,-19.5355011702686,-14.2754989395975));
#82007=CARTESIAN_POINT('Ctrl Pts',(16.6794520904527,-19.4624134474864,-14.2800220548096));
#82008=CARTESIAN_POINT('Ctrl Pts',(16.6613181208718,-19.3894194668659,-14.2845393686835));
#82009=CARTESIAN_POINT('Ctrl Pts',(16.6470584424874,-19.31537790376,-14.2890566825574));
#82010=CARTESIAN_POINT('Ctrl Pts',(16.6367803548254,-19.2407191713304,-14.2935739964313));
#82011=CARTESIAN_POINT('Ctrl Pts',(16.6265157658079,-19.1661584913522,-14.298085377527));
#82012=CARTESIAN_POINT('Ctrl Pts',(16.620222420087,-19.0909826864512,-14.3025967586227));
#82013=CARTESIAN_POINT('Ctrl Pts',(16.6179565327474,-19.0156321042995,-14.3071081397184));
#82014=CARTESIAN_POINT('Ctrl Pts',(16.6173143794296,-18.9942777211936,-14.3083866668048));
#82015=CARTESIAN_POINT('Ctrl Pts',(16.6169953775011,-18.9729093504981,-14.3096651938911));
#82016=CARTESIAN_POINT('Ctrl Pts',(16.617000050606,-18.9515371115436,-14.3109437209775));
#82017=CARTESIAN_POINT('Ctrl Pts',(16.6203928623232,-18.9515314192714,-14.3109441064964));
#82018=CARTESIAN_POINT('Ctrl Pts',(16.6197600125371,-18.626044201896,-14.3304466040356));
#82019=CARTESIAN_POINT('Ctrl Pts',(16.8436652651824,-17.5938832267072,-14.3923410371352));
#82020=CARTESIAN_POINT('Ctrl Pts',(18.4531255181642,-16.4645434415686,-14.4966274057954));
#82021=CARTESIAN_POINT('Ctrl Pts',(20.6735252872927,-17.3694159533938,-14.6238032124768));
#82022=CARTESIAN_POINT('Ctrl Pts',(21.1145309858464,-19.7262111017335,-14.7509790191583));
#82023=CARTESIAN_POINT('Ctrl Pts',(19.3715472573024,-21.3727156171948,-14.8781548258396));
#82024=CARTESIAN_POINT('Ctrl Pts',(17.4471161530942,-20.8979085117977,-14.9832889524932));
#82025=CARTESIAN_POINT('Ctrl Pts',(16.864829023637,-19.9961148353166,-15.0460311435864));
#82026=CARTESIAN_POINT('Ctrl Pts',(16.7486736625677,-19.6769293383554,-15.066381399119));
#82027=CARTESIAN_POINT('Ctrl Pts',(16.7454194444943,-19.6781104421951,-14.843838520965));
#82028=CARTESIAN_POINT('Ctrl Pts',(16.7603648243346,-19.7190409811572,-14.8409800633554));
#82029=CARTESIAN_POINT('Ctrl Pts',(16.7765815379704,-19.7595310236544,-14.8381385948187));
#82030=CARTESIAN_POINT('Ctrl Pts',(16.8176696080674,-19.8535803150628,-14.8315214728077));
#82031=CARTESIAN_POINT('Ctrl Pts',(16.8435379478377,-19.9066326300905,-14.8277759596819));
#82032=CARTESIAN_POINT('Ctrl Pts',(16.8887248800872,-19.9902424674523,-14.8218599513893));
#82033=CARTESIAN_POINT('Ctrl Pts',(16.9066665112555,-20.0215046801535,-14.8196445490687));
#82034=CARTESIAN_POINT('Ctrl Pts',(16.9311172384433,-20.0616953709696,-14.8167901621556));
#82035=CARTESIAN_POINT('Ctrl Pts',(16.9369093018647,-20.0710509810126,-14.8161252487326));
#82036=CARTESIAN_POINT('Ctrl Pts',(16.9464736002627,-20.0862339024914,-14.8150452937432));
#82037=CARTESIAN_POINT('Ctrl Pts',(16.9502019638814,-20.0920884805326,-14.8146286419104));
#82038=CARTESIAN_POINT('Ctrl Pts',(16.9574453386305,-20.1033400956848,-14.8138274356015));
#82039=CARTESIAN_POINT('Ctrl Pts',(16.9609563133272,-20.108739628149,-14.8134427369955));
#82040=CARTESIAN_POINT('Ctrl Pts',(16.9690774761028,-20.1211053261279,-14.8125611979127));
#82041=CARTESIAN_POINT('Ctrl Pts',(16.9737043828028,-20.1280604244974,-14.8120649903535));
#82042=CARTESIAN_POINT('Ctrl Pts',(16.9861632145533,-20.1465501035786,-14.8107446955642));
#82043=CARTESIAN_POINT('Ctrl Pts',(16.9940682038156,-20.1580351309188,-14.8099233705307));
#82044=CARTESIAN_POINT('Ctrl Pts',(17.0584921859535,-20.2496837138478,-14.8033574783419));
#82045=CARTESIAN_POINT('Ctrl Pts',(17.1204100857391,-20.3259143218483,-14.7978305945283));
#82046=CARTESIAN_POINT('Ctrl Pts',(17.2808130706187,-20.4975262899131,-14.7848753274666));
#82047=CARTESIAN_POINT('Ctrl Pts',(17.383690158982,-20.5881737878757,-14.7775972522211));
#82048=CARTESIAN_POINT('Ctrl Pts',(17.5362176301092,-20.6983227406158,-14.767172385556));
#82049=CARTESIAN_POINT('Ctrl Pts',(17.5789237557827,-20.7268588340156,-14.7642854493444));
#82050=CARTESIAN_POINT('Ctrl Pts',(17.6379503440067,-20.7632671002145,-14.7602785940892));
#82051=CARTESIAN_POINT('Ctrl Pts',(17.6533983727011,-20.7725255932984,-14.7592284419061));
#82052=CARTESIAN_POINT('Ctrl Pts',(17.6764325565737,-20.7859342467276,-14.7576575146448));
#82053=CARTESIAN_POINT('Ctrl Pts',(17.6839294305201,-20.7902370664145,-14.7571454454383));
#82054=CARTESIAN_POINT('Ctrl Pts',(17.6975505237689,-20.7979443594023,-14.7562132627727));
#82055=CARTESIAN_POINT('Ctrl Pts',(17.7036657369816,-20.8013645930733,-14.755794105828));
#82056=CARTESIAN_POINT('Ctrl Pts',(17.7133274982744,-20.8067056130249,-14.7551306521781));
#82057=CARTESIAN_POINT('Ctrl Pts',(17.7168628128953,-20.8086467646673,-14.7548876366302));
#82058=CARTESIAN_POINT('Ctrl Pts',(17.7204127123641,-20.8105827424277,-14.7546433437848));
#82059=CARTESIAN_POINT('Ctrl Pts',(17.720421805009,-20.8105877011177,-14.7546427180559));
#82060=CARTESIAN_POINT('Ctrl Pts',(17.7204400455879,-20.810597648476,-14.7546414627898));
#82061=CARTESIAN_POINT('Ctrl Pts',(17.7204491939729,-20.8106026373893,-14.7546408332214));
#82062=CARTESIAN_POINT('Ctrl Pts',(17.7204675464048,-20.8106126453942,-14.7546395702505));
#82063=CARTESIAN_POINT('Ctrl Pts',(17.7204767503375,-20.8106176644225,-14.7546389368558));
#82064=CARTESIAN_POINT('Ctrl Pts',(17.7204952147367,-20.8106277331299,-14.7546376661722));
#82065=CARTESIAN_POINT('Ctrl Pts',(17.72050447466,-20.8106327825117,-14.7546370289206));
#82066=CARTESIAN_POINT('Ctrl Pts',(17.7205230511052,-20.8106429119579,-14.7546357505187));
#82067=CARTESIAN_POINT('Ctrl Pts',(17.720532367803,-20.8106479921173,-14.7546351093562));
#82068=CARTESIAN_POINT('Ctrl Pts',(17.7205510577489,-20.8106581830891,-14.7546338231357));
#82069=CARTESIAN_POINT('Ctrl Pts',(17.7205604314918,-20.8106632941703,-14.7546331780436));
#82070=CARTESIAN_POINT('Ctrl Pts',(17.7205792364403,-20.8106735474799,-14.7546318839011));
#82071=CARTESIAN_POINT('Ctrl Pts',(17.7205886672233,-20.8106786894768,-14.7546312348797));
#82072=CARTESIAN_POINT('Ctrl Pts',(17.7206075862087,-20.8106890045909,-14.7546299328815));
#82073=CARTESIAN_POINT('Ctrl Pts',(17.7206170751273,-20.8106941780974,-14.7546292798553));
#82074=CARTESIAN_POINT('Ctrl Pts',(17.7206361112033,-20.8107045566741,-14.754627969791));
#82075=CARTESIAN_POINT('Ctrl Pts',(17.7206456578982,-20.8107097614909,-14.7546273127847));
#82076=CARTESIAN_POINT('Ctrl Pts',(17.7206648098499,-20.8107202028609,-14.7546259947378));
#82077=CARTESIAN_POINT('Ctrl Pts',(17.7206744153742,-20.8107254395587,-14.7546253336788));
#82078=CARTESIAN_POINT('Ctrl Pts',(17.7206936855275,-20.8107359449828,-14.7546240074892));
#82079=CARTESIAN_POINT('Ctrl Pts',(17.720703349874,-20.8107412135541,-14.754623342378));
#82080=CARTESIAN_POINT('Ctrl Pts',(17.7207227380599,-20.8107517829333,-14.754622008057));
#82081=CARTESIAN_POINT('Ctrl Pts',(17.720732461944,-20.8107570837644,-14.7546213388442));
#82082=CARTESIAN_POINT('Ctrl Pts',(17.7207519318875,-20.8107676973171,-14.7546199988883));
#82083=CARTESIAN_POINT('Ctrl Pts',(17.7207617345034,-20.8107730408685,-14.7546193242527));
#82084=CARTESIAN_POINT('Ctrl Pts',(17.7207813823703,-20.8107837510092,-14.7546179720433));
#82085=CARTESIAN_POINT('Ctrl Pts',(17.7207912257096,-20.8107891165563,-14.754617294601));
#82086=CARTESIAN_POINT('Ctrl Pts',(17.7208109749234,-20.8107998815346,-14.7546159354083));
#82087=CARTESIAN_POINT('Ctrl Pts',(17.7208208790707,-20.810805280023,-14.7546152537767));
#82088=CARTESIAN_POINT('Ctrl Pts',(17.7208407832878,-20.8108161290784,-14.7546138839076));
#82089=CARTESIAN_POINT('Ctrl Pts',(17.7208507320892,-20.8108215516989,-14.7546131991987));
#82090=CARTESIAN_POINT('Ctrl Pts',(17.7238600593233,-20.8124617623195,-14.7544060867814));
#82091=CARTESIAN_POINT('Ctrl Pts',(17.7268633259617,-20.814089253502,-14.7541991910801));
#82092=CARTESIAN_POINT('Ctrl Pts',(17.7339044377272,-20.8178828641191,-14.7537136688863));
#82093=CARTESIAN_POINT('Ctrl Pts',(17.7379453724887,-20.8200431403993,-14.7534346760457));
#82094=CARTESIAN_POINT('Ctrl Pts',(17.7503888885578,-20.8266435661868,-14.7525745597346));
#82095=CARTESIAN_POINT('Ctrl Pts',(17.7588142462784,-20.831040195631,-14.7519907948979));
#82096=CARTESIAN_POINT('Ctrl Pts',(17.8741011760019,-20.8902165104202,-14.7439870055941));
#82097=CARTESIAN_POINT('Ctrl Pts',(17.9853937251691,-20.9358576552603,-14.7360862314006));
#82098=CARTESIAN_POINT('Ctrl Pts',(18.2037608151379,-21.0044075249404,-14.7209657371144));
#82099=CARTESIAN_POINT('Ctrl Pts',(18.3099493811008,-21.0289484332123,-14.7137738165293));
#82100=CARTESIAN_POINT('Ctrl Pts',(18.4915205581074,-21.0563972714244,-14.7019767744359));
#82101=CARTESIAN_POINT('Ctrl Pts',(18.56602766924,-21.0636513867005,-14.6972711837737));
#82102=CARTESIAN_POINT('Ctrl Pts',(18.6595278891682,-21.0677730133359,-14.6915379531465));
#82103=CARTESIAN_POINT('Ctrl Pts',(18.6782963262363,-21.0683503196864,-14.6903955667553));
#82104=CARTESIAN_POINT('Ctrl Pts',(18.7056176640075,-21.0688269934401,-14.6887444451672));
#82105=CARTESIAN_POINT('Ctrl Pts',(18.7141658016438,-21.0689243456196,-14.6882295384946));
#82106=CARTESIAN_POINT('Ctrl Pts',(18.7291626118652,-21.0690042938966,-14.6873290803836));
#82107=CARTESIAN_POINT('Ctrl Pts',(18.7356110080278,-21.0690092080056,-14.6869428349968));
#82108=CARTESIAN_POINT('Ctrl Pts',(18.7481386224584,-21.0689615152518,-14.686194242766));
#82109=CARTESIAN_POINT('Ctrl Pts',(18.7542177832687,-21.068912185266,-14.6858317971254));
#82110=CARTESIAN_POINT('Ctrl Pts',(18.7687599338419,-21.0687315333882,-14.6849666927904));
#82111=CARTESIAN_POINT('Ctrl Pts',(18.7772225561527,-21.0685756426931,-14.6844648066311));
#82112=CARTESIAN_POINT('Ctrl Pts',(18.8078160897656,-21.0678285142056,-14.6826558412952));
#82113=CARTESIAN_POINT('Ctrl Pts',(18.8299388123231,-21.0669408775289,-14.6813580252488));
#82114=CARTESIAN_POINT('Ctrl Pts',(19.0370389701553,-21.0553749533222,-14.6692946754642));
#82115=CARTESIAN_POINT('Ctrl Pts',(19.2198718785134,-21.0208048170024,-14.6593824185648));
#82116=CARTESIAN_POINT('Ctrl Pts',(19.4721947441697,-20.9377522807815,-14.6449022032807));
#82117=CARTESIAN_POINT('Ctrl Pts',(19.5470101888736,-20.9083118402315,-14.6404846012247));
#82118=CARTESIAN_POINT('Ctrl Pts',(19.6527371167917,-20.859593545986,-14.6338261229747));
#82119=CARTESIAN_POINT('Ctrl Pts',(19.6851152236189,-20.8436581371412,-14.6317273597458));
#82120=CARTESIAN_POINT('Ctrl Pts',(19.7236833739933,-20.8234357088646,-14.6291357782312));
#82121=CARTESIAN_POINT('Ctrl Pts',(19.7302801466285,-20.8199321879646,-14.6286892129485));
#82122=CARTESIAN_POINT('Ctrl Pts',(19.740521771587,-20.8144232143,-14.6279905496319));
#82123=CARTESIAN_POINT('Ctrl Pts',(19.7441795619733,-20.8124417641328,-14.6277399511774));
#82124=CARTESIAN_POINT('Ctrl Pts',(19.7509617901697,-20.8087418863478,-14.627273257665));
#82125=CARTESIAN_POINT('Ctrl Pts',(19.7540877351511,-20.807026341369,-14.6270573464479));
#82126=CARTESIAN_POINT('Ctrl Pts',(19.7611571988505,-20.803123287429,-14.6265672199138));
#82127=CARTESIAN_POINT('Ctrl Pts',(19.7650980510639,-20.8009310816346,-14.6262927073956));
#82128=CARTESIAN_POINT('Ctrl Pts',(19.7752540268794,-20.7952389776896,-14.625581977329));
#82129=CARTESIAN_POINT('Ctrl Pts',(19.7814584620601,-20.7917202625182,-14.6251445942695));
#82130=CARTESIAN_POINT('Ctrl Pts',(19.8194275875443,-20.7699325368102,-14.6224488957712));
#82131=CARTESIAN_POINT('Ctrl Pts',(19.8507292590293,-20.7508738547591,-14.62014444956));
#82132=CARTESIAN_POINT('Ctrl Pts',(20.0248086127646,-20.63858735415,-14.6069247806826));
#82133=CARTESIAN_POINT('Ctrl Pts',(20.1564066682974,-20.5291893155738,-14.5954192527772));
#82134=CARTESIAN_POINT('Ctrl Pts',(20.3389522421585,-20.3358064534019,-14.5781370528099));
#82135=CARTESIAN_POINT('Ctrl Pts',(20.3996864295436,-20.2620705985389,-14.5720751384163));
#82136=CARTESIAN_POINT('Ctrl Pts',(20.4677006787844,-20.1670838172241,-14.5648989846308));
#82137=CARTESIAN_POINT('Ctrl Pts',(20.4798921257299,-20.1495005071177,-14.5635949026581));
#82138=CARTESIAN_POINT('Ctrl Pts',(20.4968364360452,-20.1242533366134,-14.561756024665));
#82139=CARTESIAN_POINT('Ctrl Pts',(20.5018098241219,-20.1167397198995,-14.561212917568));
#82140=CARTESIAN_POINT('Ctrl Pts',(20.5103026318101,-20.103729375589,-14.5602795359416));
#82141=CARTESIAN_POINT('Ctrl Pts',(20.5138448513444,-20.0982477485228,-14.5598884103319));
#82142=CARTESIAN_POINT('Ctrl Pts',(20.520575731305,-20.0877252012392,-14.5591416411905));
#82143=CARTESIAN_POINT('Ctrl Pts',(20.5237685422999,-20.0826870223598,-14.5587858456449));
#82144=CARTESIAN_POINT('Ctrl Pts',(20.5320093747557,-20.0695608193267,-14.5578633847655));
#82145=CARTESIAN_POINT('Ctrl Pts',(20.5370241641798,-20.0614520109078,-14.5572979507869));
#82146=CARTESIAN_POINT('Ctrl Pts',(20.5539060487257,-20.0337375688856,-14.5553801433624));
#82147=CARTESIAN_POINT('Ctrl Pts',(20.5655097617488,-20.0139728090187,-14.5540373891474));
#82148=CARTESIAN_POINT('Ctrl Pts',(20.6636497706736,-19.8404147437282,-14.5424506522843));
#82149=CARTESIAN_POINT('Ctrl Pts',(20.7309626796511,-19.6765520703348,-14.5329674239608));
#82150=CARTESIAN_POINT('Ctrl Pts',(20.7997627420294,-19.4229179205356,-14.5186659629901));
#82151=CARTESIAN_POINT('Ctrl Pts',(20.8172421375998,-19.3383149430912,-14.5139384772064));
#82152=CARTESIAN_POINT('Ctrl Pts',(20.8348591924054,-19.2156229324011,-14.5068603226297));
#82153=CARTESIAN_POINT('Ctrl Pts',(20.8392147258312,-19.1782232544804,-14.5046731474516));
#82154=CARTESIAN_POINT('Ctrl Pts',(20.8432447221691,-19.1331984581278,-14.5019835250189));
#82155=CARTESIAN_POINT('Ctrl Pts',(20.8438784760683,-19.1256634433039,-14.5015315143473));
#82156=CARTESIAN_POINT('Ctrl Pts',(20.8447998580103,-19.1139581199353,-14.5008261700625));
#82157=CARTESIAN_POINT('Ctrl Pts',(20.8451155321546,-19.1097899945857,-14.5005743827684));
#82158=CARTESIAN_POINT('Ctrl Pts',(20.8456774774977,-19.1020664283429,-14.500106620884));
#82159=CARTESIAN_POINT('Ctrl Pts',(20.8459271159594,-19.0985112902746,-14.4998908373885));
#82160=CARTESIAN_POINT('Ctrl Pts',(20.8464704976197,-19.0904828272899,-14.4994024745223));
#82161=CARTESIAN_POINT('Ctrl Pts',(20.8467590080591,-19.0860092152714,-14.4991296071245));
#82162=CARTESIAN_POINT('Ctrl Pts',(20.8475667945086,-19.0728322150687,-14.4983237595379));
#82163=CARTESIAN_POINT('Ctrl Pts',(20.8480465071021,-19.0641266197254,-14.4977886433611));
#82164=CARTESIAN_POINT('Ctrl Pts',(20.8510777413293,-19.0021506463171,-14.4939609374982));
#82165=CARTESIAN_POINT('Ctrl Pts',(20.851669007667,-18.9488080223078,-14.4905713326707));
#82166=CARTESIAN_POINT('Ctrl Pts',(20.8497712787356,-18.8777207368241,-14.4859754337134));
#82167=CARTESIAN_POINT('Ctrl Pts',(20.8490723514105,-18.8599432990661,-14.4848194812918));
#82168=CARTESIAN_POINT('Ctrl Pts',(20.845641339746,-18.7938944644273,-14.4805046307251));
#82169=CARTESIAN_POINT('Ctrl Pts',(20.8414800045263,-18.7457130557192,-14.4773173739823));
#82170=CARTESIAN_POINT('Ctrl Pts',(20.8225347878885,-18.5891286039126,-14.4668984051702));
#82171=CARTESIAN_POINT('Ctrl Pts',(20.8009993719172,-18.4817125638282,-14.4596657342549));
#82172=CARTESIAN_POINT('Ctrl Pts',(20.7562766412917,-18.3234125975831,-14.4490923551298));
#82173=CARTESIAN_POINT('Ctrl Pts',(20.7392311382289,-18.2709905730079,-14.4456032688615));
#82174=CARTESIAN_POINT('Ctrl Pts',(20.7082857825986,-18.1871069811851,-14.4400457704914));
#82175=CARTESIAN_POINT('Ctrl Pts',(20.6956323614549,-18.1552162298279,-14.4379389208695));
#82176=CARTESIAN_POINT('Ctrl Pts',(20.6779797093515,-18.1136989138682,-14.4352024097579));
#82177=CARTESIAN_POINT('Ctrl Pts',(20.6736743539742,-18.1037846802256,-14.4345494073186));
#82178=CARTESIAN_POINT('Ctrl Pts',(20.6664971874799,-18.087597777187,-14.4334839101279));
#82179=CARTESIAN_POINT('Ctrl Pts',(20.6636703499423,-18.0813054928809,-14.4330698859469));
#82180=CARTESIAN_POINT('Ctrl Pts',(20.6581380598985,-18.0691504001565,-14.4322703711206));
#82181=CARTESIAN_POINT('Ctrl Pts',(20.6554364441083,-18.0632859390265,-14.4318847541351));
#82182=CARTESIAN_POINT('Ctrl Pts',(20.6491353941242,-18.0497711469525,-14.4309963328076));
#82183=CARTESIAN_POINT('Ctrl Pts',(20.6455168604704,-18.0421298024447,-14.4304941945357));
#82184=CARTESIAN_POINT('Ctrl Pts',(20.6356595183159,-18.0216321826915,-14.4291475809847));
#82185=CARTESIAN_POINT('Ctrl Pts',(20.6293360886682,-18.0088169186273,-14.428306047138));
#82186=CARTESIAN_POINT('Ctrl Pts',(20.5701243777261,-17.8918171469568,-14.4206240394106));
#82187=CARTESIAN_POINT('Ctrl Pts',(20.5088228373494,-17.7921079481606,-14.4141002663022));
#82188=CARTESIAN_POINT('Ctrl Pts',(20.3431641823924,-17.5667992185879,-14.3987907175919));
#82189=CARTESIAN_POINT('Ctrl Pts',(20.2319364432361,-17.4472192493636,-14.3901881689856));
#82190=CARTESIAN_POINT('Ctrl Pts',(20.0834401150863,-17.3205118968985,-14.3789789594798));
#82191=CARTESIAN_POINT('Ctrl Pts',(20.0582748973489,-17.3000200391511,-14.37708619202));
#82192=CARTESIAN_POINT('Ctrl Pts',(20.0269359738743,-17.275677261837,-14.3747234396652));
#82193=CARTESIAN_POINT('Ctrl Pts',(20.0211990300786,-17.2712680140642,-14.3742906854574));
#82194=CARTESIAN_POINT('Ctrl Pts',(20.0121690986088,-17.264401221301,-14.3736089816574));
#82195=CARTESIAN_POINT('Ctrl Pts',(20.008891305515,-17.2619236582429,-14.3733614159221));
#82196=CARTESIAN_POINT('Ctrl Pts',(20.0027504788832,-17.2573100631652,-14.3728973571606));
#82197=CARTESIAN_POINT('Ctrl Pts',(19.9998892447891,-17.2551717296833,-14.3726810291808));
#82198=CARTESIAN_POINT('Ctrl Pts',(19.9933447615646,-17.2503064982866,-14.3721859905242));
#82199=CARTESIAN_POINT('Ctrl Pts',(19.9896580738096,-17.2475843221155,-14.3719069575251));
#82200=CARTESIAN_POINT('Ctrl Pts',(19.9782963268728,-17.2392519062185,-14.3710465970564));
#82201=CARTESIAN_POINT('Ctrl Pts',(19.9705924150494,-17.2336814692508,-14.3704626260879));
#82202=CARTESIAN_POINT('Ctrl Pts',(19.8655544284441,-17.158804264792,-14.3624954152205));
#82203=CARTESIAN_POINT('Ctrl Pts',(19.7625708943982,-17.0978150956803,-14.3546360500476));
#82204=CARTESIAN_POINT('Ctrl Pts',(19.556843475407,-16.9984126205601,-14.3395419538394));
#82205=CARTESIAN_POINT('Ctrl Pts',(19.4551535936839,-16.9586319949511,-14.3323351635132));
#82206=CARTESIAN_POINT('Ctrl Pts',(19.2789846315027,-16.9049719317662,-14.3205019713434));
#82207=CARTESIAN_POINT('Ctrl Pts',(19.2060032480531,-16.8869219753311,-14.3157754911845));
#82208=CARTESIAN_POINT('Ctrl Pts',(19.1137256608774,-16.869249032614,-14.3100197141104));
#82209=CARTESIAN_POINT('Ctrl Pts',(19.0951953656295,-16.8659556300437,-14.3088746530865));
#82210=CARTESIAN_POINT('Ctrl Pts',(19.0681794453542,-16.8615248597706,-14.3072204026436));
#82211=CARTESIAN_POINT('Ctrl Pts',(19.059727342264,-16.8601912335316,-14.3067050088074));
#82212=CARTESIAN_POINT('Ctrl Pts',(19.0448905868193,-16.8579423027054,-14.3058039888301));
#82213=CARTESIAN_POINT('Ctrl Pts',(19.0385094482317,-16.8570048701877,-14.3054176660695));
#82214=CARTESIAN_POINT('Ctrl Pts',(19.0261077014693,-16.8552408293307,-14.3046691344161));
#82215=CARTESIAN_POINT('Ctrl Pts',(19.0200876284462,-16.854410955626,-14.3043068257372));
#82216=CARTESIAN_POINT('Ctrl Pts',(19.0056833679515,-16.8524884772962,-14.3034423834016));
#82217=CARTESIAN_POINT('Ctrl Pts',(18.9972960028912,-16.8514201504345,-14.3029410195686));
#82218=CARTESIAN_POINT('Ctrl Pts',(18.9669815049474,-16.8477433113492,-14.3011359235911));
#82219=CARTESIAN_POINT('Ctrl Pts',(18.9450198075027,-16.8454275971789,-14.2998414020953));
#82220=CARTESIAN_POINT('Ctrl Pts',(18.7379169477376,-16.8268613869831,-14.2877476574487));
#82221=CARTESIAN_POINT('Ctrl Pts',(18.5514349710742,-16.8347127102277,-14.277807919148));
#82222=CARTESIAN_POINT('Ctrl Pts',(18.2607935942403,-16.8856768599577,-14.2617211681073));
#82223=CARTESIAN_POINT('Ctrl Pts',(18.1548602647907,-16.9128319320364,-14.2557001056844));
#82224=CARTESIAN_POINT('Ctrl Pts',(18.0403434106466,-16.9518328360542,-14.2485597694457));
#82225=CARTESIAN_POINT('Ctrl Pts',(18.0292094009874,-16.9557288899198,-14.2478586747539));
#82226=CARTESIAN_POINT('Ctrl Pts',(18.0134001814295,-16.9614096515108,-14.2468526015562));
#82227=CARTESIAN_POINT('Ctrl Pts',(18.0086976111573,-16.9631182846657,-14.2465519960793));
#82228=CARTESIAN_POINT('Ctrl Pts',(18.0005936490082,-16.9660953440076,-14.246031571634));
#82229=CARTESIAN_POINT('Ctrl Pts',(17.9971893464367,-16.9673558910936,-14.245812221688));
#82230=CARTESIAN_POINT('Ctrl Pts',(17.9905867573782,-16.9698200313216,-14.2453853497427));
#82231=CARTESIAN_POINT('Ctrl Pts',(17.9873881369865,-16.9710226141728,-14.2451778940369));
#82232=CARTESIAN_POINT('Ctrl Pts',(17.978748319879,-16.9742948172629,-14.2446157813056));
#82233=CARTESIAN_POINT('Ctrl Pts',(17.9733127727665,-16.9763791278095,-14.2442602575995));
#82234=CARTESIAN_POINT('Ctrl Pts',(17.9530676974896,-16.9842382231789,-14.2429292355584));
#82235=CARTESIAN_POINT('Ctrl Pts',(17.9383151876999,-16.9901571631857,-14.2419456158599));
#82236=CARTESIAN_POINT('Ctrl Pts',(17.8094123898518,-17.0435680510149,-14.2332389818716));
#82237=CARTESIAN_POINT('Ctrl Pts',(17.6995697006187,-17.1008049873945,-14.2250577701307));
#82238=CARTESIAN_POINT('Ctrl Pts',(17.4544602765674,-17.2571841821322,-14.2058446951504));
#82239=CARTESIAN_POINT('Ctrl Pts',(17.3246745757517,-17.3634644444438,-14.1949287562502));
#82240=CARTESIAN_POINT('Ctrl Pts',(17.1939622353427,-17.499269412077,-14.1833517496273));
#82241=CARTESIAN_POINT('Ctrl Pts',(17.1794267457231,-17.5148345513655,-14.182053821091));
#82242=CARTESIAN_POINT('Ctrl Pts',(17.1590898221214,-17.5372817192189,-14.1802220377878));
#82243=CARTESIAN_POINT('Ctrl Pts',(17.1530939476409,-17.5439851066563,-14.1796799588728));
#82244=CARTESIAN_POINT('Ctrl Pts',(17.1428229797148,-17.5556163691263,-14.17874778975));
#82245=CARTESIAN_POINT('Ctrl Pts',(17.1385276475629,-17.5605261308442,-14.1783568542898));
#82246=CARTESIAN_POINT('Ctrl Pts',(17.1303461923325,-17.5699655997979,-14.1776100709782));
#82247=CARTESIAN_POINT('Ctrl Pts',(17.1264564021841,-17.5744920325338,-14.1772540729282));
#82248=CARTESIAN_POINT('Ctrl Pts',(17.116390057836,-17.5863066448367,-14.1763302714904));
#82249=CARTESIAN_POINT('Ctrl Pts',(17.1102435591015,-17.5936203437504,-14.1757637067052));
#82250=CARTESIAN_POINT('Ctrl Pts',(17.0894464840566,-17.6187095861363,-14.1738378763305));
#82251=CARTESIAN_POINT('Ctrl Pts',(17.0750362860497,-17.6366829083594,-14.1724883413812));
#82252=CARTESIAN_POINT('Ctrl Pts',(16.9537663431868,-17.7931028226989,-14.1609878253909));
#82253=CARTESIAN_POINT('Ctrl Pts',(16.8641501657937,-17.9440600889061,-14.1515817989786));
#82254=CARTESIAN_POINT('Ctrl Pts',(16.7591127368294,-18.1844380736309,-14.1373097815625));
#82255=CARTESIAN_POINT('Ctrl Pts',(16.7291075131656,-18.2666280500326,-14.1325252744366));
#82256=CARTESIAN_POINT('Ctrl Pts',(16.6934927520533,-18.3867941073107,-14.1253702344575));
#82257=CARTESIAN_POINT('Ctrl Pts',(16.6836950221498,-18.4234390994714,-14.1231672792692));
#82258=CARTESIAN_POINT('Ctrl Pts',(16.6731275271715,-18.467695269505,-14.1204601664176));
#82259=CARTESIAN_POINT('Ctrl Pts',(16.6714072199851,-18.4750750151874,-14.1200072118277));
#82260=CARTESIAN_POINT('Ctrl Pts',(16.6687987127553,-18.4865430789206,-14.1193007098061));
#82261=CARTESIAN_POINT('Ctrl Pts',(16.6678829298504,-18.4906251481073,-14.1190487168597));
#82262=CARTESIAN_POINT('Ctrl Pts',(16.6662094767803,-18.498189409679,-14.1185807682855));
#82263=CARTESIAN_POINT('Ctrl Pts',(16.6654484970054,-18.5016708107583,-14.1183650050015));
#82264=CARTESIAN_POINT('Ctrl Pts',(16.6637510235548,-18.5095316599399,-14.1178769386893));
#82265=CARTESIAN_POINT('Ctrl Pts',(16.6628196397407,-18.5139121425429,-14.117604349186));
#82266=CARTESIAN_POINT('Ctrl Pts',(16.6601202353279,-18.5268090113293,-14.1168000651794));
#82267=CARTESIAN_POINT('Ctrl Pts',(16.6583908185769,-18.5353332564236,-14.1162662468071));
#82268=CARTESIAN_POINT('Ctrl Pts',(16.6465063460822,-18.5958221003902,-14.1124636611002));
#82269=CARTESIAN_POINT('Ctrl Pts',(16.6382522868145,-18.6481366127104,-14.1090992535617));
#82270=CARTESIAN_POINT('Ctrl Pts',(16.6301911556275,-18.7155650934305,-14.1047115443988));
#82271=CARTESIAN_POINT('Ctrl Pts',(16.6285718192705,-18.730448021496,-14.1037398707023));
#82272=CARTESIAN_POINT('Ctrl Pts',(16.6204362476909,-18.8133924644856,-14.0983107777663));
#82273=CARTESIAN_POINT('Ctrl Pts',(16.6170625895878,-18.8817198861515,-14.0937881860309));
#82274=CARTESIAN_POINT('Ctrl Pts',(16.616855711663,-19.1108585919565,-14.0786472531482));
#82275=CARTESIAN_POINT('Ctrl Pts',(16.6350247738316,-19.2711508353488,-14.0681492526916));
#82276=CARTESIAN_POINT('Ctrl Pts',(16.6765204048595,-19.4510311559526,-14.056777750078));
#82277=CARTESIAN_POINT('Ctrl Pts',(16.6822553156789,-19.4741093771815,-14.0553254705806));
#82278=CARTESIAN_POINT('Ctrl Pts',(16.6908695980634,-19.5064373734598,-14.0532997717922));
#82279=CARTESIAN_POINT('Ctrl Pts',(16.6934253017039,-19.5157708275043,-14.0527159490391));
#82280=CARTESIAN_POINT('Ctrl Pts',(16.6976666649319,-19.5308535538158,-14.0517740673681));
#82281=CARTESIAN_POINT('Ctrl Pts',(16.6993128687413,-19.536613690664,-14.0514147315572));
#82282=CARTESIAN_POINT('Ctrl Pts',(16.7027975173043,-19.5486135996585,-14.0506668844873));
#82283=CARTESIAN_POINT('Ctrl Pts',(16.7046403176142,-19.5548520498185,-14.0502785197106));
#82284=CARTESIAN_POINT('Ctrl Pts',(16.7090695303949,-19.5695958395848,-14.0493616204611));
#82285=CARTESIAN_POINT('Ctrl Pts',(16.7116808336213,-19.5780936198187,-14.0488339058202));
#82286=CARTESIAN_POINT('Ctrl Pts',(16.7205471772908,-19.6063124363643,-14.0470838241541));
#82287=CARTESIAN_POINT('Ctrl Pts',(16.7270378946957,-19.6259585938869,-14.0458691933702));
#82288=CARTESIAN_POINT('Ctrl Pts',(16.7375951449116,-19.6564073802206,-14.0439912496844));
#82289=CARTESIAN_POINT('Ctrl Pts',(16.741463193259,-19.667275555683,-14.0433218615717));
#82290=CARTESIAN_POINT('Ctrl Pts',(16.7454194457665,-19.6781104456791,-14.0426552583743));
#82291=CARTESIAN_POINT('Origin',(18.734,-18.952,0.));
#82292=CARTESIAN_POINT('',(16.7454194499637,-19.6781104571739,-13.2445592876386));
#82293=CARTESIAN_POINT('',(16.7454194853472,-19.6781105540779,-13.4647888353055));
#82294=CARTESIAN_POINT('',(16.7454194499637,-19.6781104571739,0.));
#82295=CARTESIAN_POINT('',(16.6170008950802,-18.9539467328105,-13.5109437209775));
#82296=CARTESIAN_POINT('Ctrl Pts',(16.7454194853472,-19.6781105540779,-13.4647888353055));
#82297=CARTESIAN_POINT('Ctrl Pts',(16.7297666895009,-19.6352426400322,-13.4673502476732));
#82298=CARTESIAN_POINT('Ctrl Pts',(16.7154972636532,-19.5918609431498,-13.4699562924166));
#82299=CARTESIAN_POINT('Ctrl Pts',(16.6982006735783,-19.5329117146061,-13.4735579116563));
#82300=CARTESIAN_POINT('Ctrl Pts',(16.6939331613312,-19.5177425018985,-13.4744900067255));
#82301=CARTESIAN_POINT('Ctrl Pts',(16.6883270791775,-19.4969265527102,-13.4757780818251));
#82302=CARTESIAN_POINT('Ctrl Pts',(16.6868416780363,-19.4913194321066,-13.476125935793));
#82303=CARTESIAN_POINT('Ctrl Pts',(16.6845188929854,-19.4824034704128,-13.4766805778664));
#82304=CARTESIAN_POINT('Ctrl Pts',(16.6836664223934,-19.4790985387891,-13.4768865000793));
#82305=CARTESIAN_POINT('Ctrl Pts',(16.6819231278139,-19.4722717633015,-13.4773125674383));
#82306=CARTESIAN_POINT('Ctrl Pts',(16.6810333782576,-19.4687496940318,-13.4775327754571));
#82307=CARTESIAN_POINT('Ctrl Pts',(16.678936164473,-19.4603569743768,-13.4780584152838));
#82308=CARTESIAN_POINT('Ctrl Pts',(16.6777369482887,-19.4554843021042,-13.478364318273));
#82309=CARTESIAN_POINT('Ctrl Pts',(16.6752325957493,-19.4451503867218,-13.4790145418689));
#82310=CARTESIAN_POINT('Ctrl Pts',(16.6739318427581,-19.4396881325614,-13.4793591005458));
#82311=CARTESIAN_POINT('Ctrl Pts',(16.6704195235729,-19.4246740382725,-13.4803084432271));
#82312=CARTESIAN_POINT('Ctrl Pts',(16.668252589932,-19.4151120370729,-13.4809155501542));
#82313=CARTESIAN_POINT('Ctrl Pts',(16.6336164616417,-19.2571922345215,-13.4909794322946));
#82314=CARTESIAN_POINT('Ctrl Pts',(16.6171414694287,-19.1057964096688,-13.5011355937932));
#82315=CARTESIAN_POINT('Ctrl Pts',(16.6170009071419,-18.953959805644,-13.5111420756604));
#82316=CARTESIAN_POINT('Ctrl Pts',(16.6170008950802,-18.9539467328105,-13.5109437209775));
#82317=CARTESIAN_POINT('Ctrl Pts',(16.6169347298129,-18.8819944798437,-13.5152699622426));
#82318=CARTESIAN_POINT('Ctrl Pts',(16.6205410702701,-18.8099473001284,-13.5195962035077));
#82319=CARTESIAN_POINT('Ctrl Pts',(16.6278222442379,-18.738214450598,-13.5239224447729));
#82320=CARTESIAN_POINT('Ctrl Pts',(16.6350987839402,-18.6665272570402,-13.5282459325052));
#82321=CARTESIAN_POINT('Ctrl Pts',(16.6460454699348,-18.5951544878199,-13.5325694202375));
#82322=CARTESIAN_POINT('Ctrl Pts',(16.6606126061973,-18.524502964665,-13.5368929079699));
#82323=CARTESIAN_POINT('Ctrl Pts',(16.675175543473,-18.4538718068595,-13.541215149454));
#82324=CARTESIAN_POINT('Ctrl Pts',(16.6933567603003,-18.3839619667448,-13.545537390938));
#82325=CARTESIAN_POINT('Ctrl Pts',(16.7150553040208,-18.3151708906014,-13.5498596324221));
#82326=CARTESIAN_POINT('Ctrl Pts',(16.7367551488127,-18.2463756896604,-13.5541821330731));
#82327=CARTESIAN_POINT('Ctrl Pts',(16.7619725873321,-18.1786998565911,-13.5585046337241));
#82328=CARTESIAN_POINT('Ctrl Pts',(16.7905571249902,-18.1125246926958,-13.5628271343751));
#82329=CARTESIAN_POINT('Ctrl Pts',(16.8191715095123,-18.0462804312642,-13.5671541484134));
#82330=CARTESIAN_POINT('Ctrl Pts',(16.8511598101655,-17.9815404195957,-13.5714811624517));
#82331=CARTESIAN_POINT('Ctrl Pts',(16.8863242283789,-17.9186640222249,-13.57580817649));
#82332=CARTESIAN_POINT('Ctrl Pts',(16.9215100988963,-17.8557492666598,-13.5801378302541));
#82333=CARTESIAN_POINT('Ctrl Pts',(16.9598756760654,-17.7947008039885,-13.5844674840182));
#82334=CARTESIAN_POINT('Ctrl Pts',(17.0011797410101,-17.7358491252997,-13.5887971377822));
#82335=CARTESIAN_POINT('Ctrl Pts',(17.04255259404,-17.6768994346044,-13.5931340021826));
#82336=CARTESIAN_POINT('Ctrl Pts',(17.0868733907411,-17.6201542127689,-13.597470866583));
#82337=CARTESIAN_POINT('Ctrl Pts',(17.1338612235983,-17.5659102134942,-13.6018077309834));
#82338=CARTESIAN_POINT('Ctrl Pts',(17.1504345250056,-17.5467775552112,-13.6033374069974));
#82339=CARTESIAN_POINT('Ctrl Pts',(17.1673393021153,-17.5279557221355,-13.6048670830114));
#82340=CARTESIAN_POINT('Ctrl Pts',(17.1845622179522,-17.5094565657968,-13.6063967590254));
#82341=CARTESIAN_POINT('Ctrl Pts',(17.2339699045479,-17.4563877052552,-13.6107849679563));
#82342=CARTESIAN_POINT('Ctrl Pts',(17.2862036327226,-17.405756540934,-13.6151731768872));
#82343=CARTESIAN_POINT('Ctrl Pts',(17.3409933109754,-17.3578791249304,-13.6195613858181));
#82344=CARTESIAN_POINT('Ctrl Pts',(17.3957016722616,-17.3100727669502,-13.6239430819193));
#82345=CARTESIAN_POINT('Ctrl Pts',(17.4529580928702,-17.2650123587825,-13.6283247780206));
#82346=CARTESIAN_POINT('Ctrl Pts',(17.5124544762696,-17.2229784462147,-13.6327064741219));
#82347=CARTESIAN_POINT('Ctrl Pts',(17.5718809466836,-17.1809939268393,-13.6370830213816));
#82348=CARTESIAN_POINT('Ctrl Pts',(17.6335417591182,-17.1420291152643,-13.6414595686412));
#82349=CARTESIAN_POINT('Ctrl Pts',(17.6970957742222,-17.106324344159,-13.6458361159008));
#82350=CARTESIAN_POINT('Ctrl Pts',(17.7606094842934,-17.0706422165006,-13.6502098876178));
#82351=CARTESIAN_POINT('Ctrl Pts',(17.826013595286,-17.0382162628695,-13.6545836593348));
#82352=CARTESIAN_POINT('Ctrl Pts',(17.8929392167485,-17.009242743193,-13.6589574310518));
#82353=CARTESIAN_POINT('Ctrl Pts',(17.9598444725197,-16.9802780402557,-13.6633298718153));
#82354=CARTESIAN_POINT('Ctrl Pts',(18.0282698771528,-16.9547638770617,-13.6677023125789));
#82355=CARTESIAN_POINT('Ctrl Pts',(18.0978247669418,-16.9328491703582,-13.6720747533424));
#82356=CARTESIAN_POINT('Ctrl Pts',(18.167381435257,-16.9109339032931,-13.6764473059098));
#82357=CARTESIAN_POINT('Ctrl Pts',(18.2380671853859,-16.8926184185034,-13.6808198584771));
#82358=CARTESIAN_POINT('Ctrl Pts',(18.3094759435911,-16.8780018501623,-13.6851924110445));
#82359=CARTESIAN_POINT('Ctrl Pts',(18.3809588124991,-16.8633701121953,-13.6895695016118));
#82360=CARTESIAN_POINT('Ctrl Pts',(18.4531657140474,-16.8524450521881,-13.6939465921791));
#82361=CARTESIAN_POINT('Ctrl Pts',(18.5256809453902,-16.8452745381786,-13.6983236827465));
#82362=CARTESIAN_POINT('Ctrl Pts',(18.5982357799922,-16.8381001080853,-13.7027031638054));
#82363=CARTESIAN_POINT('Ctrl Pts',(18.6710987974697,-16.8346843291133,-13.7070826448644));
#82364=CARTESIAN_POINT('Ctrl Pts',(18.7438524696376,-16.8350229267085,-13.7114621259233));
#82365=CARTESIAN_POINT('Ctrl Pts',(18.8167350972012,-16.8353621244656,-13.715849369583));
#82366=CARTESIAN_POINT('Ctrl Pts',(18.8895075103812,-16.8394689605671,-13.7202366132428));
#82367=CARTESIAN_POINT('Ctrl Pts',(18.9617560691,-16.8472871518927,-13.7246238569025));
#82368=CARTESIAN_POINT('Ctrl Pts',(19.0108781271733,-16.8526027686348,-13.7276067598372));
#82369=CARTESIAN_POINT('Ctrl Pts',(19.0597581560649,-16.8596329436867,-13.730589662772));
#82370=CARTESIAN_POINT('Ctrl Pts',(19.1082694567066,-16.8683466282089,-13.7335725657068));
#82371=CARTESIAN_POINT('Ctrl Pts',(19.1796354137562,-16.8811655060193,-13.7379607746377));
#82372=CARTESIAN_POINT('Ctrl Pts',(19.2504813367648,-16.8976801162964,-13.7423489835686));
#82373=CARTESIAN_POINT('Ctrl Pts',(19.3203952805283,-16.9178344278368,-13.7467371924995));
#82374=CARTESIAN_POINT('Ctrl Pts',(19.3902054604072,-16.9379588270371,-13.7511188886007));
#82375=CARTESIAN_POINT('Ctrl Pts',(19.4590859472333,-16.9617120714409,-13.755500584702));
#82376=CARTESIAN_POINT('Ctrl Pts',(19.5266340795877,-16.9889869547361,-13.7598822808032));
#82377=CARTESIAN_POINT('Ctrl Pts',(19.594102837511,-17.0162297878729,-13.7642588280629));
#82378=CARTESIAN_POINT('Ctrl Pts',(19.6602419060114,-17.0469858596158,-13.7686353753225));
#82379=CARTESIAN_POINT('Ctrl Pts',(19.7246645510869,-17.0810984132724,-13.7730119225822));
#82380=CARTESIAN_POINT('Ctrl Pts',(19.7890463402572,-17.1151893332433,-13.7773856942991));
#82381=CARTESIAN_POINT('Ctrl Pts',(19.8517134405357,-17.1526322864694,-13.7817594660161));
#82382=CARTESIAN_POINT('Ctrl Pts',(19.9123011549776,-17.1932233262354,-13.7861332377331));
#82383=CARTESIAN_POINT('Ctrl Pts',(19.9728704323746,-17.2338020140118,-13.7905056784966));
#82384=CARTESIAN_POINT('Ctrl Pts',(20.0313611796543,-17.2775266181305,-13.7948781192602));
#82385=CARTESIAN_POINT('Ctrl Pts',(20.0874367225444,-17.3241492580497,-13.7992505600237));
#82386=CARTESIAN_POINT('Ctrl Pts',(20.1435136992923,-17.3707730901148,-13.8036231125911));
#82387=CARTESIAN_POINT('Ctrl Pts',(20.1971749793956,-17.4202947951746,-13.8079956651584));
#82388=CARTESIAN_POINT('Ctrl Pts',(20.2481174066906,-17.4724265889262,-13.8123682177258));
#82389=CARTESIAN_POINT('Ctrl Pts',(20.2991127039582,-17.5246124870198,-13.8167453082931));
#82390=CARTESIAN_POINT('Ctrl Pts',(20.3473831767919,-17.5794135364602,-13.8211223988604));
#82391=CARTESIAN_POINT('Ctrl Pts',(20.3926635636812,-17.6365061070015,-13.8254994894278));
#82392=CARTESIAN_POINT('Ctrl Pts',(20.4379686798704,-17.6936298579146,-13.8298789704867));
#82393=CARTESIAN_POINT('Ctrl Pts',(20.4802801788313,-17.7530472284184,-13.8342584515457));
#82394=CARTESIAN_POINT('Ctrl Pts',(20.5193756547,-17.8144048296496,-13.8386379326046));
#82395=CARTESIAN_POINT('Ctrl Pts',(20.5585404270373,-17.8758711868171,-13.8430251762643));
#82396=CARTESIAN_POINT('Ctrl Pts',(20.5944775548132,-17.9392842223068,-13.8474124199241));
#82397=CARTESIAN_POINT('Ctrl Pts',(20.6270104676962,-18.0042656652878,-13.8517996635838));
#82398=CARTESIAN_POINT('Ctrl Pts',(20.6491297135926,-18.0484467849177,-13.8547825665186));
#82399=CARTESIAN_POINT('Ctrl Pts',(20.6696762814795,-18.0933524542016,-13.8577654694534));
#82400=CARTESIAN_POINT('Ctrl Pts',(20.6886076987149,-18.1388593331259,-13.8607483723882));
#82401=CARTESIAN_POINT('Ctrl Pts',(20.7164580900962,-18.2058054245265,-13.8651365813191));
#82402=CARTESIAN_POINT('Ctrl Pts',(20.7409194707722,-18.2743146794849,-13.86952479025));
#82403=CARTESIAN_POINT('Ctrl Pts',(20.7618159759921,-18.3440103886486,-13.8739129991809));
#82404=CARTESIAN_POINT('Ctrl Pts',(20.7826814673336,-18.4136026578242,-13.8782946952822));
#82405=CARTESIAN_POINT('Ctrl Pts',(20.7999924489197,-18.4843774273517,-13.8826763913835));
#82406=CARTESIAN_POINT('Ctrl Pts',(20.8136211113041,-18.555938093957,-13.8870580874847));
#82407=CARTESIAN_POINT('Ctrl Pts',(20.8272337589255,-18.6274146710837,-13.8914346347444));
#82408=CARTESIAN_POINT('Ctrl Pts',(20.8371725931962,-18.6996748392574,-13.895811182004));
#82409=CARTESIAN_POINT('Ctrl Pts',(20.8433600899069,-18.7723085669599,-13.9001877292637));
#82410=CARTESIAN_POINT('Ctrl Pts',(20.8495436625971,-18.8448962314078,-13.9045615009806));
#82411=CARTESIAN_POINT('Ctrl Pts',(20.8519805772149,-18.9178565058778,-13.9089352726976));
#82412=CARTESIAN_POINT('Ctrl Pts',(20.8506449171335,-18.9907723454651,-13.9133090444146));
#82413=CARTESIAN_POINT('Ctrl Pts',(20.8493096634979,-19.0636659965176,-13.9176814851781));
#82414=CARTESIAN_POINT('Ctrl Pts',(20.8442041231404,-19.1365147575252,-13.9220539259417));
#82415=CARTESIAN_POINT('Ctrl Pts',(20.8353544889708,-19.2089013656685,-13.9264263667052));
#82416=CARTESIAN_POINT('Ctrl Pts',(20.826504628515,-19.2812898247453,-13.9307989192726));
#82417=CARTESIAN_POINT('Ctrl Pts',(20.8139105446928,-19.3532156289256,-13.9351714718399));
#82418=CARTESIAN_POINT('Ctrl Pts',(20.7976501258782,-19.4242680996667,-13.9395440244072));
#82419=CARTESIAN_POINT('Ctrl Pts',(20.7813728313876,-19.4953943113422,-13.9439211149746));
#82420=CARTESIAN_POINT('Ctrl Pts',(20.7614217126853,-19.5656449087054,-13.9482982055419));
#82421=CARTESIAN_POINT('Ctrl Pts',(20.737925310568,-19.6346216738904,-13.9526752961092));
#82422=CARTESIAN_POINT('Ctrl Pts',(20.7144160761934,-19.703636109847,-13.9570547771682));
#82423=CARTESIAN_POINT('Ctrl Pts',(20.687357882489,-19.7713748802473,-13.9614342582271));
#82424=CARTESIAN_POINT('Ctrl Pts',(20.6569274894879,-19.8374596942672,-13.965813739286));
#82425=CARTESIAN_POINT('Ctrl Pts',(20.6264431588195,-19.9036616431763,-13.9702009829458));
#82426=CARTESIAN_POINT('Ctrl Pts',(20.5925749169667,-19.9682033538493,-13.9745882266055));
#82427=CARTESIAN_POINT('Ctrl Pts',(20.5555452556642,-20.0307316077539,-13.9789754702652));
#82428=CARTESIAN_POINT('Ctrl Pts',(20.530368654148,-20.0732447952009,-13.9819583732));
#82429=CARTESIAN_POINT('Ctrl Pts',(20.503731560257,-20.1148277943093,-13.9849412761349));
#82430=CARTESIAN_POINT('Ctrl Pts',(20.475714693788,-20.1553781306983,-13.9879241790697));
#82431=CARTESIAN_POINT('Ctrl Pts',(20.434498513999,-20.2150325519721,-13.9923123880006));
#82432=CARTESIAN_POINT('Ctrl Pts',(20.3901335538169,-20.2726834623513,-13.9967005969315));
#82433=CARTESIAN_POINT('Ctrl Pts',(20.3428413739374,-20.3279790817841,-14.0010888058624));
#82434=CARTESIAN_POINT('Ctrl Pts',(20.2956193834941,-20.3831926333494,-14.0054705019636));
#82435=CARTESIAN_POINT('Ctrl Pts',(20.2454791086756,-20.4360574697364,-14.0098521980649));
#82436=CARTESIAN_POINT('Ctrl Pts',(20.1926848492426,-20.4862514495969,-14.0142338941661));
#82437=CARTESIAN_POINT('Ctrl Pts',(20.1399526272657,-20.5363864475366,-14.0186104414258));
#82438=CARTESIAN_POINT('Ctrl Pts',(20.084572963737,-20.5838564928137,-14.0229869886854));
#82439=CARTESIAN_POINT('Ctrl Pts',(20.0268486678902,-20.6283744575526,-14.027363535945));
#82440=CARTESIAN_POINT('Ctrl Pts',(19.9691609799528,-20.6728641896452,-14.031737307662));
#82441=CARTESIAN_POINT('Ctrl Pts',(19.9091319910002,-20.7144052619584,-14.036111079379));
#82442=CARTESIAN_POINT('Ctrl Pts',(19.8470983416197,-20.7527501442131,-14.040484851096));
#82443=CARTESIAN_POINT('Ctrl Pts',(19.785083569287,-20.7910833579914,-14.0448572918595));
#82444=CARTESIAN_POINT('Ctrl Pts',(19.7210657576847,-20.8262220591674,-14.0492297326231));
#82445=CARTESIAN_POINT('Ctrl Pts',(19.6554099365357,-20.8579624153832,-14.0536021733866));
#82446=CARTESIAN_POINT('Ctrl Pts',(19.5897524365603,-20.8897035832033,-14.057974725954));
#82447=CARTESIAN_POINT('Ctrl Pts',(19.5224572790424,-20.9180460253879,-14.0623472785213));
#82448=CARTESIAN_POINT('Ctrl Pts',(19.4539119391452,-20.9428329412274,-14.0667198310886));
#82449=CARTESIAN_POINT('Ctrl Pts',(19.3852954603087,-20.9676455818632,-14.071096921656));
#82450=CARTESIAN_POINT('Ctrl Pts',(19.3154266631736,-20.9888951643123,-14.0754740122233));
#82451=CARTESIAN_POINT('Ctrl Pts',(19.2447099626412,-21.0064742232647,-14.0798511027906));
#82452=CARTESIAN_POINT('Ctrl Pts',(19.1739546410939,-21.0240628827937,-14.0842305838495));
#82453=CARTESIAN_POINT('Ctrl Pts',(19.102350968027,-21.0379769355906,-14.0886100649085));
#82454=CARTESIAN_POINT('Ctrl Pts',(19.0303127030113,-21.0481602472221,-14.0929895459674));
#82455=CARTESIAN_POINT('Ctrl Pts',(18.9581467506545,-21.0583616087051,-14.0973767896272));
#82456=CARTESIAN_POINT('Ctrl Pts',(18.8855451489727,-21.0648189809294,-14.1017640332869));
#82457=CARTESIAN_POINT('Ctrl Pts',(18.8129253294097,-21.0675282537413,-14.1061512769466));
#82458=CARTESIAN_POINT('Ctrl Pts',(18.7635508497359,-21.0693702981885,-14.1091341798814));
#82459=CARTESIAN_POINT('Ctrl Pts',(18.7141679744272,-21.069480806371,-14.1121170828162));
#82460=CARTESIAN_POINT('Ctrl Pts',(18.6649065603162,-21.0678721834252,-14.1150999857511));
#82461=CARTESIAN_POINT('Ctrl Pts',(18.5924370961486,-21.0655057056244,-14.119488194682));
#82462=CARTESIAN_POINT('Ctrl Pts',(18.5199478924753,-21.0594071393707,-14.1238764036129));
#82463=CARTESIAN_POINT('Ctrl Pts',(18.4478546672521,-21.0495723702763,-14.1282646125438));
#82464=CARTESIAN_POINT('Ctrl Pts',(18.3758684403282,-21.0397521976099,-14.132646308645));
#82465=CARTESIAN_POINT('Ctrl Pts',(18.3042774991944,-21.0262068946334,-14.1370280047463));
#82466=CARTESIAN_POINT('Ctrl Pts',(18.2334957741921,-21.0089843266171,-14.1414097008476));
#82467=CARTESIAN_POINT('Ctrl Pts',(18.1627972233499,-20.9917819964889,-14.1457862481072));
#82468=CARTESIAN_POINT('Ctrl Pts',(18.0929064660597,-20.9709110986508,-14.1501627953669));
#82469=CARTESIAN_POINT('Ctrl Pts',(18.0242288363209,-20.9464708308746,-14.1545393426265));
#82470=CARTESIAN_POINT('Ctrl Pts',(17.9555947609367,-20.922046062761,-14.1589131143435));
#82471=CARTESIAN_POINT('Ctrl Pts',(17.8881727399583,-20.8940565773996,-14.1632868860605));
#82472=CARTESIAN_POINT('Ctrl Pts',(17.8223531243428,-20.8626514528046,-14.1676606577774));
#82473=CARTESIAN_POINT('Ctrl Pts',(17.7565535378573,-20.8312558848945,-14.172033098541));
#82474=CARTESIAN_POINT('Ctrl Pts',(17.6923558237617,-20.7964469488636,-14.1764055393046));
#82475=CARTESIAN_POINT('Ctrl Pts',(17.6301289564777,-20.7584212463523,-14.1807779800681));
#82476=CARTESIAN_POINT('Ctrl Pts',(17.5679004980457,-20.7203945715195,-14.1851505326355));
#82477=CARTESIAN_POINT('Ctrl Pts',(17.5076433970461,-20.6791512201339,-14.1895230852029));
#82478=CARTESIAN_POINT('Ctrl Pts',(17.4496992310181,-20.6349321242381,-14.1938956377702));
#82479=CARTESIAN_POINT('Ctrl Pts',(17.3916949283492,-20.5906671360969,-14.1982727283375));
#82480=CARTESIAN_POINT('Ctrl Pts',(17.3360087376062,-20.5434205306325,-14.2026498189049));
#82481=CARTESIAN_POINT('Ctrl Pts',(17.2829499222238,-20.4934741878428,-14.2070269094722));
#82482=CARTESIAN_POINT('Ctrl Pts',(17.2298621294529,-20.4435005675016,-14.2114063905312));
#82483=CARTESIAN_POINT('Ctrl Pts',(17.1794049028374,-20.3908246228572,-14.2157858715901));
#82484=CARTESIAN_POINT('Ctrl Pts',(17.1318494027602,-20.3357638757259,-14.220165352649));
#82485=CARTESIAN_POINT('Ctrl Pts',(17.0842096108783,-20.2806055337899,-14.2245525963088));
#82486=CARTESIAN_POINT('Ctrl Pts',(17.039482112747,-20.2230543293393,-14.2289398399685));
#82487=CARTESIAN_POINT('Ctrl Pts',(16.9978963120783,-20.1634590314099,-14.2333270836282));
#82488=CARTESIAN_POINT('Ctrl Pts',(16.9696219748223,-20.122939971408,-14.236309986563));
#82489=CARTESIAN_POINT('Ctrl Pts',(16.9427990411454,-20.0814766042669,-14.2392928894977));
#82490=CARTESIAN_POINT('Ctrl Pts',(16.9174873693316,-20.0391848336976,-14.2422757924325));
#82491=CARTESIAN_POINT('Ctrl Pts',(16.8789822269095,-19.9748488759218,-14.2468135054362));
#82492=CARTESIAN_POINT('Ctrl Pts',(16.8438347836027,-19.908358318242,-14.2513512184398));
#82493=CARTESIAN_POINT('Ctrl Pts',(16.8122834229314,-19.8400846791943,-14.2558889314435));
#82494=CARTESIAN_POINT('Ctrl Pts',(16.7877996091002,-19.7871044262843,-14.2594101906868));
#82495=CARTESIAN_POINT('Ctrl Pts',(16.7654805062868,-19.7330511704266,-14.26293144993));
#82496=CARTESIAN_POINT('Ctrl Pts',(16.7454194499637,-19.6781104571739,-14.2664527091733));
#82497=CARTESIAN_POINT('',(16.6170000012625,-18.9520658364028,-13.2889027715975));
#82498=CARTESIAN_POINT('Ctrl Pts',(16.7454194457665,-19.6781104456791,-14.0426552583743));
#82499=CARTESIAN_POINT('Ctrl Pts',(16.7721869599386,-19.7514179686387,-14.0381451037516));
#82500=CARTESIAN_POINT('Ctrl Pts',(16.8029921858641,-19.8232019799891,-14.033765580411));
#82501=CARTESIAN_POINT('Ctrl Pts',(16.8976427025996,-20.0139142964462,-14.0220204986683));
#82502=CARTESIAN_POINT('Ctrl Pts',(16.9689849492002,-20.1286859665614,-14.0148420563074));
#82503=CARTESIAN_POINT('Ctrl Pts',(17.0971457026277,-20.2967112557855,-14.0031497920472));
#82504=CARTESIAN_POINT('Ctrl Pts',(17.1467942036028,-20.3549666617983,-13.9988302072747));
#82505=CARTESIAN_POINT('Ctrl Pts',(17.2060220521686,-20.4172858419015,-13.9937348299809));
#82506=CARTESIAN_POINT('Ctrl Pts',(17.2126111808868,-20.4241261022789,-13.9931687001201));
#82507=CARTESIAN_POINT('Ctrl Pts',(17.2224462448901,-20.4341994572846,-13.9923243406249));
#82508=CARTESIAN_POINT('Ctrl Pts',(17.2256571117406,-20.4374668344645,-13.9920487838485));
#82509=CARTESIAN_POINT('Ctrl Pts',(17.2313903512189,-20.4432632234787,-13.9915568816742));
#82510=CARTESIAN_POINT('Ctrl Pts',(17.2339085440464,-20.445796298648,-13.9913408653148));
#82511=CARTESIAN_POINT('Ctrl Pts',(17.2393381903345,-20.4512304582825,-13.9908751683641));
#82512=CARTESIAN_POINT('Ctrl Pts',(17.2422516423121,-20.4541293982164,-13.9906253322116));
#82513=CARTESIAN_POINT('Ctrl Pts',(17.2503213433811,-20.4621122731473,-13.9899335167327));
#82514=CARTESIAN_POINT('Ctrl Pts',(17.2554952066476,-20.4671782093737,-13.9894901660879));
#82515=CARTESIAN_POINT('Ctrl Pts',(17.2840548107071,-20.4948564945067,-13.987044525901));
#82516=CARTESIAN_POINT('Ctrl Pts',(17.3079320181715,-20.5169527330886,-13.9850059098458));
#82517=CARTESIAN_POINT('Ctrl Pts',(17.4542418792366,-20.6462202684404,-13.9726000407908));
#82518=CARTESIAN_POINT('Ctrl Pts',(17.5881860833947,-20.7395328146315,-13.9616427776728));
#82519=CARTESIAN_POINT('Ctrl Pts',(17.8343782953957,-20.8718996729219,-13.9433846899226));
#82520=CARTESIAN_POINT('Ctrl Pts',(17.9416765416058,-20.9186126484348,-13.93594384611));
#82521=CARTESIAN_POINT('Ctrl Pts',(18.0658261082647,-20.9608396739953,-13.9279367855054));
#82522=CARTESIAN_POINT('Ctrl Pts',(18.0794008270803,-20.9653040316714,-13.9270688094193));
#82523=CARTESIAN_POINT('Ctrl Pts',(18.1010776420677,-20.972190527553,-13.9256945008057));
#82524=CARTESIAN_POINT('Ctrl Pts',(18.1091506623918,-20.9747021004872,-13.9251852402096));
#82525=CARTESIAN_POINT('Ctrl Pts',(18.1234152321935,-20.9790463562849,-13.9242898621162));
#82526=CARTESIAN_POINT('Ctrl Pts',(18.1296004855871,-20.980899188628,-13.9239030884917));
#82527=CARTESIAN_POINT('Ctrl Pts',(18.1424111056422,-20.9846729110359,-13.923105019838));
#82528=CARTESIAN_POINT('Ctrl Pts',(18.1490375853779,-20.9865897764408,-13.9226938601894));
#82529=CARTESIAN_POINT('Ctrl Pts',(18.1660708891544,-20.9914269665598,-13.9216411506931));
#82530=CARTESIAN_POINT('Ctrl Pts',(18.1764910046677,-20.9943000645251,-13.9210011421454));
#82531=CARTESIAN_POINT('Ctrl Pts',(18.2200727018896,-21.0059582694059,-13.9183404789634));
#82532=CARTESIAN_POINT('Ctrl Pts',(18.2534244406701,-21.0140167721381,-13.91634335302));
#82533=CARTESIAN_POINT('Ctrl Pts',(18.3408210802685,-21.0328978569808,-13.9111992821519));
#82534=CARTESIAN_POINT('Ctrl Pts',(18.3951196364458,-21.0424273005058,-13.9080917260888));
#82535=CARTESIAN_POINT('Ctrl Pts',(18.5580873773159,-21.0645104430544,-13.8989473207305));
#82536=CARTESIAN_POINT('Ctrl Pts',(18.6674211618566,-21.0707764782452,-13.8930592008436));
#82537=CARTESIAN_POINT('Ctrl Pts',(18.8224676133939,-21.0676449378191,-13.8846161010564));
#82538=CARTESIAN_POINT('Ctrl Pts',(18.8681428050623,-21.0652405192403,-13.8821158043807));
#82539=CARTESIAN_POINT('Ctrl Pts',(18.9364163957964,-21.059424079672,-13.8783162829452));
#82540=CARTESIAN_POINT('Ctrl Pts',(18.9590966352536,-21.057122348416,-13.8770437146181));
#82541=CARTESIAN_POINT('Ctrl Pts',(18.9827755514586,-21.0543322343119,-13.8757003233075));
#82542=CARTESIAN_POINT('Ctrl Pts',(18.9838163182545,-21.0542088158787,-13.8756412468457));
#82543=CARTESIAN_POINT('Ctrl Pts',(19.0033483655743,-21.051877915128,-13.8745319908282));
#82544=CARTESIAN_POINT('Ctrl Pts',(19.0218093283111,-21.0494273655847,-13.8734739878806));
#82545=CARTESIAN_POINT('Ctrl Pts',(19.0731185568614,-21.0419263239952,-13.8705009022357));
#82546=CARTESIAN_POINT('Ctrl Pts',(19.1058822686279,-21.036345637701,-13.8685651454196));
#82547=CARTESIAN_POINT('Ctrl Pts',(19.1452826450028,-21.028676033506,-13.8661774429272));
#82548=CARTESIAN_POINT('Ctrl Pts',(19.1520597259084,-21.0273223423892,-13.8657645920997));
#82549=CARTESIAN_POINT('Ctrl Pts',(19.1631812398754,-21.0250441846517,-13.8650833640594));
#82550=CARTESIAN_POINT('Ctrl Pts',(19.1675296669947,-21.0241391737013,-13.8648160726923));
#82551=CARTESIAN_POINT('Ctrl Pts',(19.1753596936741,-21.0224838336454,-13.8643330317671));
#82552=CARTESIAN_POINT('Ctrl Pts',(19.1788422714992,-21.021738398384,-13.8641175642141));
#82553=CARTESIAN_POINT('Ctrl Pts',(19.1864403038299,-21.0200919998191,-13.8636460993557));
#82554=CARTESIAN_POINT('Ctrl Pts',(19.1905549045828,-21.0191875499416,-13.8633899088532));
#82555=CARTESIAN_POINT('Ctrl Pts',(19.2021949835671,-21.0165924413463,-13.862662726988));
#82556=CARTESIAN_POINT('Ctrl Pts',(19.2097138695378,-21.0148729484948,-13.8621901298025));
#82557=CARTESIAN_POINT('Ctrl Pts',(19.2565595345929,-21.0038900903622,-13.8592284236552));
#82558=CARTESIAN_POINT('Ctrl Pts',(19.2956210702144,-20.9935441928995,-13.856683039728));
#82559=CARTESIAN_POINT('Ctrl Pts',(19.5037501477926,-20.9319940089521,-13.8427961641896));
#82560=CARTESIAN_POINT('Ctrl Pts',(19.6662060911874,-20.8608973874339,-13.8308635704815));
#82561=CARTESIAN_POINT('Ctrl Pts',(19.8995447047212,-20.7218072092279,-13.813283852132));
#82562=CARTESIAN_POINT('Ctrl Pts',(19.9777804815814,-20.6677291293636,-13.8072854825148));
#82563=CARTESIAN_POINT('Ctrl Pts',(20.0629632242982,-20.599949473611,-13.8006424328673));
#82564=CARTESIAN_POINT('Ctrl Pts',(20.0737134013628,-20.5912219909517,-13.7998017261266));
#82565=CARTESIAN_POINT('Ctrl Pts',(20.0907890903852,-20.5770789752718,-13.7984623470531));
#82566=CARTESIAN_POINT('Ctrl Pts',(20.0971694851617,-20.5717306163295,-13.7979609737402));
#82567=CARTESIAN_POINT('Ctrl Pts',(20.1084262674509,-20.5621810023959,-13.7970747294757));
#82568=CARTESIAN_POINT('Ctrl Pts',(20.1133153272138,-20.5579949111587,-13.7966892445521));
#82569=CARTESIAN_POINT('Ctrl Pts',(20.1234463589306,-20.5492401711612,-13.7958892194195));
#82570=CARTESIAN_POINT('Ctrl Pts',(20.1286850718637,-20.5446678564001,-13.7954748374623));
#82571=CARTESIAN_POINT('Ctrl Pts',(20.1421976389473,-20.5327563778492,-13.7944041255413));
#82572=CARTESIAN_POINT('Ctrl Pts',(20.1504367454304,-20.5253779805447,-13.7937494415916));
#82573=CARTESIAN_POINT('Ctrl Pts',(20.1856586860754,-20.4933346360438,-13.7909422385269));
#82574=CARTESIAN_POINT('Ctrl Pts',(20.2120589428686,-20.4680367406241,-13.7888166847188));
#82575=CARTESIAN_POINT('Ctrl Pts',(20.280153144947,-20.3993153055432,-13.7832614867172));
#82576=CARTESIAN_POINT('Ctrl Pts',(20.3206739306244,-20.3547750297984,-13.7798800177396));
#82577=CARTESIAN_POINT('Ctrl Pts',(20.46575545344,-20.1809590007894,-13.7673401953335));
#82578=CARTESIAN_POINT('Ctrl Pts',(20.5568583641458,-20.0412645572718,-13.7585865664522));
#82579=CARTESIAN_POINT('Ctrl Pts',(20.6550421577045,-19.8432314989794,-13.7461710994383));
#82580=CARTESIAN_POINT('Ctrl Pts',(20.6774818553897,-19.7931740223842,-13.7430275873579));
#82581=CARTESIAN_POINT('Ctrl Pts',(20.7012280681046,-19.7341635254107,-13.7392532697357));
#82582=CARTESIAN_POINT('Ctrl Pts',(20.7044542604594,-19.7260000347712,-13.7387296372469));
#82583=CARTESIAN_POINT('Ctrl Pts',(20.7092558086628,-19.7136256962134,-13.7379333127725));
#82584=CARTESIAN_POINT('Ctrl Pts',(20.7108687182033,-19.7094293900563,-13.7376628193084));
#82585=CARTESIAN_POINT('Ctrl Pts',(20.713736592851,-19.7018964800839,-13.7371763904588));
#82586=CARTESIAN_POINT('Ctrl Pts',(20.7149965068341,-19.6985618176279,-13.736960755355));
#82587=CARTESIAN_POINT('Ctrl Pts',(20.717712138022,-19.6913189744351,-13.7364917291835));
#82588=CARTESIAN_POINT('Ctrl Pts',(20.7191647117576,-19.6874097218526,-13.7362381603033));
#82589=CARTESIAN_POINT('Ctrl Pts',(20.7232031762802,-19.6764420145384,-13.7355256387335));
#82590=CARTESIAN_POINT('Ctrl Pts',(20.725763006085,-19.6693741232079,-13.7350651794537));
#82591=CARTESIAN_POINT('Ctrl Pts',(20.7406603587333,-19.627546914277,-13.7323332428803));
#82592=CARTESIAN_POINT('Ctrl Pts',(20.7521246085084,-19.5924858398115,-13.7300149275892));
#82593=CARTESIAN_POINT('Ctrl Pts',(20.7864934904204,-19.4772689882757,-13.7223447811041));
#82594=CARTESIAN_POINT('Ctrl Pts',(20.8055806134706,-19.3960596634728,-13.7168607867334));
#82595=CARTESIAN_POINT('Ctrl Pts',(20.8507313997309,-19.1358614713703,-13.6994180044698));
#82596=CARTESIAN_POINT('Ctrl Pts',(20.8587061194251,-18.9545165082085,-13.6875290487399));
#82597=CARTESIAN_POINT('Ctrl Pts',(20.8416388849935,-18.7518591691525,-13.6750162408764));
#82598=CARTESIAN_POINT('Ctrl Pts',(20.8393861924423,-18.7294083015744,-13.6736393190221));
#82599=CARTESIAN_POINT('Ctrl Pts',(20.8356783785468,-18.6975854290503,-13.6717001354661));
#82600=CARTESIAN_POINT('Ctrl Pts',(20.834518606021,-18.6881811775329,-13.671128625746));
#82601=CARTESIAN_POINT('Ctrl Pts',(20.832527306908,-18.6728806841485,-13.6702012459747));
#82602=CARTESIAN_POINT('Ctrl Pts',(20.8317339844724,-18.666979681716,-13.6698441748107));
#82603=CARTESIAN_POINT('Ctrl Pts',(20.8300175932237,-18.6546080560707,-13.6690967837867));
#82604=CARTESIAN_POINT('Ctrl Pts',(20.8290894309414,-18.6481381938249,-13.668706629148));
#82605=CARTESIAN_POINT('Ctrl Pts',(20.8268028522558,-18.6327080474139,-13.6677777629402));
#82606=CARTESIAN_POINT('Ctrl Pts',(20.8254168264631,-18.6237519363779,-13.6672399310146));
#82607=CARTESIAN_POINT('Ctrl Pts',(20.8205160816352,-18.5933765669102,-13.6654200705167));
#82608=CARTESIAN_POINT('Ctrl Pts',(20.8167294085277,-18.5720021209686,-13.6641466639462));
#82609=CARTESIAN_POINT('Ctrl Pts',(20.7940292327281,-18.4544251627964,-13.6571759896299));
#82610=CARTESIAN_POINT('Ctrl Pts',(20.7687782534887,-18.359562754452,-13.651686062569));
#82611=CARTESIAN_POINT('Ctrl Pts',(20.6889378443015,-18.1261717353152,-13.6381338850067));
#82612=CARTESIAN_POINT('Ctrl Pts',(20.6261682832087,-17.9910277673772,-13.6302573691986));
#82613=CARTESIAN_POINT('Ctrl Pts',(20.5220671428842,-17.8173596474118,-13.6188753705984));
#82614=CARTESIAN_POINT('Ctrl Pts',(20.4926096792223,-17.7722187550602,-13.6157844445076));
#82615=CARTESIAN_POINT('Ctrl Pts',(20.4564131292788,-17.7211229134234,-13.6120686740366));
#82616=CARTESIAN_POINT('Ctrl Pts',(20.451316812386,-17.7140224759269,-13.6115472680799));
#82617=CARTESIAN_POINT('Ctrl Pts',(20.4435375838022,-17.7033245468187,-13.6107536743237));
#82618=CARTESIAN_POINT('Ctrl Pts',(20.4408868881438,-17.6997035941757,-13.6104836626105));
#82619=CARTESIAN_POINT('Ctrl Pts',(20.4361102326022,-17.6932218384384,-13.6099977473655));
#82620=CARTESIAN_POINT('Ctrl Pts',(20.4339885445472,-17.6903579540658,-13.6097821413715));
#82621=CARTESIAN_POINT('Ctrl Pts',(20.42936489799,-17.6841497302213,-13.6093127659561));
#82622=CARTESIAN_POINT('Ctrl Pts',(20.4268603049836,-17.6808074768039,-13.6090588164771));
#82623=CARTESIAN_POINT('Ctrl Pts',(20.4198030966434,-17.6714478319911,-13.6083441729457));
#82624=CARTESIAN_POINT('Ctrl Pts',(20.4152282293877,-17.6654474078308,-13.6078819581185));
#82625=CARTESIAN_POINT('Ctrl Pts',(20.3878059956778,-17.6298762682055,-13.6051182811268));
#82626=CARTESIAN_POINT('Ctrl Pts',(20.3642124774657,-17.6008921895516,-13.6027687304478));
#82627=CARTESIAN_POINT('Ctrl Pts',(20.2843343202899,-17.5079032402282,-13.5949452046279));
#82628=CARTESIAN_POINT('Ctrl Pts',(20.2249529747154,-17.4466730207191,-13.5893336312393));
#82629=CARTESIAN_POINT('Ctrl Pts',(20.0306366376107,-17.2691124492177,-13.5719446161163));
#82630=CARTESIAN_POINT('Ctrl Pts',(19.8845760090526,-17.1660614841348,-13.5602467270275));
#82631=CARTESIAN_POINT('Ctrl Pts',(19.7071878283161,-17.0718101274938,-13.5478850412963));
#82632=CARTESIAN_POINT('Ctrl Pts',(19.6868879283737,-17.0614410441462,-13.5464938043774));
#82633=CARTESIAN_POINT('Ctrl Pts',(19.65788285135,-17.0472113020174,-13.5445381840105));
#82634=CARTESIAN_POINT('Ctrl Pts',(19.6493135602774,-17.0430786820891,-13.5439643377366));
#82635=CARTESIAN_POINT('Ctrl Pts',(19.635330110926,-17.0364508454563,-13.5430342102175));
#82636=CARTESIAN_POINT('Ctrl Pts',(19.629932829043,-17.0339205179901,-13.5426767135916));
#82637=CARTESIAN_POINT('Ctrl Pts',(19.6186009854747,-17.0286662448261,-13.5419292622041));
#82638=CARTESIAN_POINT('Ctrl Pts',(19.6126643554615,-17.025946888269,-13.541539469021));
#82639=CARTESIAN_POINT('Ctrl Pts',(19.598489721046,-17.0195331742507,-13.5406129797373));
#82640=CARTESIAN_POINT('Ctrl Pts',(19.5902404356889,-17.0158639431713,-13.5400771513667));
#82641=CARTESIAN_POINT('Ctrl Pts',(19.5622666238311,-17.0036351185028,-13.5382712670726));
#82642=CARTESIAN_POINT('Ctrl Pts',(19.542434844009,-16.9953231067151,-13.5370096516184));
#82643=CARTESIAN_POINT('Ctrl Pts',(19.3557094266094,-16.9203853492735,-13.5252950445415));
#82644=CARTESIAN_POINT('Ctrl Pts',(19.1810999362263,-16.8749614081036,-13.5156412900567));
#82645=CARTESIAN_POINT('Ctrl Pts',(18.8835838187848,-16.8368716329855,-13.4993166157163));
#82646=CARTESIAN_POINT('Ctrl Pts',(18.7632637349034,-16.8317928083396,-13.4927195868004));
#82647=CARTESIAN_POINT('Ctrl Pts',(18.6336873316197,-16.8373566003335,-13.4850331194839));
#82648=CARTESIAN_POINT('Ctrl Pts',(18.6241944420691,-16.8378282777837,-13.4844665819589));
#82649=CARTESIAN_POINT('Ctrl Pts',(18.6101301512917,-16.8386220738344,-13.4836217296178));
#82650=CARTESIAN_POINT('Ctrl Pts',(18.6055559505523,-16.8388951461229,-13.4833460921917));
#82651=CARTESIAN_POINT('Ctrl Pts',(18.5974177730034,-16.8394075039179,-13.4828541018001));
#82652=CARTESIAN_POINT('Ctrl Pts',(18.5938534796924,-16.8396409604782,-13.4826380783304));
#82653=CARTESIAN_POINT('Ctrl Pts',(18.5861900995733,-16.8401623835543,-13.4821724296963));
#82654=CARTESIAN_POINT('Ctrl Pts',(18.5820913155066,-16.8404532598564,-13.4819226493064));
#82655=CARTESIAN_POINT('Ctrl Pts',(18.5707761194048,-16.8412893758241,-13.4812311418009));
#82656=CARTESIAN_POINT('Ctrl Pts',(18.5635616956397,-16.8418596835451,-13.4807880453361));
#82657=CARTESIAN_POINT('Ctrl Pts',(18.523994794911,-16.8451917203648,-13.4783463696751));
#82658=CARTESIAN_POINT('Ctrl Pts',(18.4917080993436,-16.8486603506387,-13.4763115998307));
#82659=CARTESIAN_POINT('Ctrl Pts',(18.2981304459386,-16.8739727174034,-13.4639070236209));
#82660=CARTESIAN_POINT('Ctrl Pts',(18.13972130921,-16.9136152437953,-13.4529462357759));
#82661=CARTESIAN_POINT('Ctrl Pts',(17.8781151470345,-17.0122076422301,-13.4346849232696));
#82662=CARTESIAN_POINT('Ctrl Pts',(17.7723945378792,-17.062382045708,-13.4272441800145));
#82663=CARTESIAN_POINT('Ctrl Pts',(17.6578777315532,-17.1288455590383,-13.4191593261585));
#82664=CARTESIAN_POINT('Ctrl Pts',(17.6445025247068,-17.1368067530198,-13.4182143261785));
#82665=CARTESIAN_POINT('Ctrl Pts',(17.6244411519992,-17.1490493197416,-13.4167955644284));
#82666=CARTESIAN_POINT('Ctrl Pts',(17.6176894899693,-17.153221847894,-13.4163178422648));
#82667=CARTESIAN_POINT('Ctrl Pts',(17.6057065981157,-17.1607207292496,-13.415469498479));
#82668=CARTESIAN_POINT('Ctrl Pts',(17.6004662421755,-17.164032257647,-13.4150983360449));
#82669=CARTESIAN_POINT('Ctrl Pts',(17.5902140547062,-17.1705740927647,-13.4143718399567));
#82670=CARTESIAN_POINT('Ctrl Pts',(17.5852011793017,-17.1738026481008,-13.4140164459822));
#82671=CARTESIAN_POINT('Ctrl Pts',(17.5714896433962,-17.1827157804008,-13.4130438407229));
#82672=CARTESIAN_POINT('Ctrl Pts',(17.562819017157,-17.1884433408034,-13.4124282396084));
#82673=CARTESIAN_POINT('Ctrl Pts',(17.5285817782131,-17.2114233183363,-13.4099948154214));
#82674=CARTESIAN_POINT('Ctrl Pts',(17.5033505548447,-17.2291702459126,-13.4081956962966));
#82675=CARTESIAN_POINT('Ctrl Pts',(17.4401260604431,-17.2757385457438,-13.4036643613956));
#82676=CARTESIAN_POINT('Ctrl Pts',(17.402701510518,-17.3053042146353,-13.4009603597374));
#82677=CARTESIAN_POINT('Ctrl Pts',(17.2129193101145,-17.465936499037,-13.3870466588676));
#82678=CARTESIAN_POINT('Ctrl Pts',(17.0788208989739,-17.6169206488171,-13.3766113981987));
#82679=CARTESIAN_POINT('Ctrl Pts',(16.9454163218237,-17.81871376139,-13.3628534654534));
#82680=CARTESIAN_POINT('Ctrl Pts',(16.9238101457127,-17.853554977078,-13.3604799994511));
#82681=CARTESIAN_POINT('Ctrl Pts',(16.8995229162862,-17.8953840110384,-13.3576059848227));
#82682=CARTESIAN_POINT('Ctrl Pts',(16.8958488670851,-17.9017886271043,-13.3571652684421));
#82683=CARTESIAN_POINT('Ctrl Pts',(16.8899474763337,-17.9122017894717,-13.3564474244174));
#82684=CARTESIAN_POINT('Ctrl Pts',(16.8876994874731,-17.9161986458817,-13.3561715901209));
#82685=CARTESIAN_POINT('Ctrl Pts',(16.8837234237483,-17.9233220363606,-13.3556793842589));
#82686=CARTESIAN_POINT('Ctrl Pts',(16.8819902588821,-17.9264456718049,-13.355463343305));
#82687=CARTESIAN_POINT('Ctrl Pts',(16.8782815021483,-17.9331699240814,-13.3549978120319));
#82688=CARTESIAN_POINT('Ctrl Pts',(16.8763085082727,-17.9367718543269,-13.354748167305));
#82689=CARTESIAN_POINT('Ctrl Pts',(16.870892553817,-17.9467279602914,-13.3540574089041));
#82690=CARTESIAN_POINT('Ctrl Pts',(16.8674716687201,-17.9530939909571,-13.3536149306657));
#82691=CARTESIAN_POINT('Ctrl Pts',(16.8489285518339,-17.9880292930581,-13.3511828650674));
#82692=CARTESIAN_POINT('Ctrl Pts',(16.834430467357,-18.0169228828917,-13.3491574153013));
#82693=CARTESIAN_POINT('Ctrl Pts',(16.7509029235034,-18.1933526890104,-13.3367559519128));
#82694=CARTESIAN_POINT('Ctrl Pts',(16.6984298740533,-18.3481176259676,-13.3257865964695));
#82695=CARTESIAN_POINT('Ctrl Pts',(16.6510960514021,-18.5684579652946,-13.3110654529574));
#82696=CARTESIAN_POINT('Ctrl Pts',(16.6406827342214,-18.6301037482727,-13.3070327355362));
#82697=CARTESIAN_POINT('Ctrl Pts',(16.6297590815427,-18.7184169347304,-13.3013962992466));
#82698=CARTESIAN_POINT('Ctrl Pts',(16.6270006057081,-18.7447693600014,-13.2997318572692));
#82699=CARTESIAN_POINT('Ctrl Pts',(16.6216845006033,-18.8067773718103,-13.2958565756987));
#82700=CARTESIAN_POINT('Ctrl Pts',(16.6195337088767,-18.8424603781411,-13.2936584428369));
#82701=CARTESIAN_POINT('Ctrl Pts',(16.6178981528545,-18.8893377127938,-13.2908108214091));
#82702=CARTESIAN_POINT('Ctrl Pts',(16.6175971716164,-18.9004959689164,-13.2901359625467));
#82703=CARTESIAN_POINT('Ctrl Pts',(16.6172522422916,-18.9185925226664,-13.2890461501006));
#82704=CARTESIAN_POINT('Ctrl Pts',(16.6171541289577,-18.9255294627886,-13.288629507179));
#82705=CARTESIAN_POINT('Ctrl Pts',(16.6170502015161,-18.9367926100214,-13.2879547992264));
#82706=CARTESIAN_POINT('Ctrl Pts',(16.6170235456918,-18.9411185320172,-13.2876960836696));
#82707=CARTESIAN_POINT('Ctrl Pts',(16.6170034293768,-18.9476147918886,-13.2873081980846));
#82708=CARTESIAN_POINT('Ctrl Pts',(16.6170000462454,-18.9497850674194,-13.2871787183687));
#82709=CARTESIAN_POINT('Ctrl Pts',(16.6170000004709,-18.9519553492827,-13.287049342907));
#82710=CARTESIAN_POINT('Ctrl Pts',(16.6170000013281,-18.9520749873283,-13.2890562789747));
#82711=CARTESIAN_POINT('Ctrl Pts',(16.6170027225446,-19.0288988399567,-13.2844612169082));
#82712=CARTESIAN_POINT('Ctrl Pts',(16.6211915380442,-19.1056371710189,-13.2798661548417));
#82713=CARTESIAN_POINT('Ctrl Pts',(16.6295128869012,-19.1818325277265,-13.2752710927752));
#82714=CARTESIAN_POINT('Ctrl Pts',(16.6378461991752,-19.2581374287929,-13.2706694244908));
#82715=CARTESIAN_POINT('Ctrl Pts',(16.6503238258348,-19.3338973983149,-13.2660677562064));
#82716=CARTESIAN_POINT('Ctrl Pts',(16.6668410730001,-19.4086650528829,-13.261466087922));
#82717=CARTESIAN_POINT('Ctrl Pts',(16.6833972601622,-19.4836089748522,-13.2568535710412));
#82718=CARTESIAN_POINT('Ctrl Pts',(16.7040119873824,-19.5575555160791,-13.2522410541604));
#82719=CARTESIAN_POINT('Ctrl Pts',(16.7285306582113,-19.6300720604371,-13.2476285372796));
#82720=CARTESIAN_POINT('Ctrl Pts',(16.7339690427624,-19.6461566539819,-13.2466054540659));
#82721=CARTESIAN_POINT('Ctrl Pts',(16.739599307015,-19.662170977234,-13.2455823708523));
#82722=CARTESIAN_POINT('Ctrl Pts',(16.7454194499637,-19.6781104571739,-13.2445592876386));
#82723=CARTESIAN_POINT('Origin',(18.734,-18.952,0.));
#82724=CARTESIAN_POINT('',(16.7437496527793,-19.6787359237804,-12.4443820746906));
#82725=CARTESIAN_POINT('',(16.7454195349593,-19.6781106899492,-12.6679318731853));
#82726=CARTESIAN_POINT('',(16.7454194499637,-19.6781104571739,0.));
#82727=CARTESIAN_POINT('Ctrl Pts',(16.7454195349593,-19.6781106899492,-12.6679318731853));
#82728=CARTESIAN_POINT('Ctrl Pts',(16.705203908673,-19.5679731999918,-12.6745735390896));
#82729=CARTESIAN_POINT('Ctrl Pts',(16.6741842980992,-19.4546217778048,-12.6809438288943));
#82730=CARTESIAN_POINT('Ctrl Pts',(16.6289120093902,-19.2112807481602,-12.6943852262644));
#82731=CARTESIAN_POINT('Ctrl Pts',(16.6169601911292,-19.0814434066492,-12.7014276312587));
#82732=CARTESIAN_POINT('Ctrl Pts',(16.6170011043058,-18.9480754918077,-12.7092186189957));
#82733=CARTESIAN_POINT('Ctrl Pts',(16.6170097089921,-18.9448004415573,-12.7094102891661));
#82734=CARTESIAN_POINT('Ctrl Pts',(16.6171033910119,-18.9258667099555,-12.7105204682452));
#82735=CARTESIAN_POINT('Ctrl Pts',(16.6173545994999,-18.9102098313582,-12.7114467924583));
#82736=CARTESIAN_POINT('Ctrl Pts',(16.6179364418611,-18.8887742899,-12.7127280957681));
#82737=CARTESIAN_POINT('Ctrl Pts',(16.6181171311767,-18.8829916227347,-12.7130750584379));
#82738=CARTESIAN_POINT('Ctrl Pts',(16.6184419953724,-18.873801800889,-12.7136286293193));
#82739=CARTESIAN_POINT('Ctrl Pts',(16.6185707048855,-18.8703940793869,-12.713834377607));
#82740=CARTESIAN_POINT('Ctrl Pts',(16.6188536040123,-18.8633550108911,-12.7142603867494));
#82741=CARTESIAN_POINT('Ctrl Pts',(16.6190089114769,-18.8597237558016,-12.7144807118296));
#82742=CARTESIAN_POINT('Ctrl Pts',(16.619401390337,-18.851069284925,-12.7150071270833));
#82743=CARTESIAN_POINT('Ctrl Pts',(16.6196471101571,-18.8460464948671,-12.7153136921317));
#82744=CARTESIAN_POINT('Ctrl Pts',(16.6205368798928,-18.8290963045789,-12.7163516784865));
#82745=CARTESIAN_POINT('Ctrl Pts',(16.6212639670735,-18.8171737470573,-12.7170875273693));
#82746=CARTESIAN_POINT('Ctrl Pts',(16.6311147089677,-18.6754017636838,-12.7259008176317));
#82747=CARTESIAN_POINT('Ctrl Pts',(16.6520942072658,-18.546667431601,-12.7345184188496));
#82748=CARTESIAN_POINT('Ctrl Pts',(16.7254963566545,-18.2635581636166,-12.7538450628526));
#82749=CARTESIAN_POINT('Ctrl Pts',(16.7841810481341,-18.1116049299082,-12.7644509320186));
#82750=CARTESIAN_POINT('Ctrl Pts',(16.870698255241,-17.9468342438934,-12.7759141291557));
#82751=CARTESIAN_POINT('Ctrl Pts',(16.8820773745263,-17.926020346037,-12.7773627665996));
#82752=CARTESIAN_POINT('Ctrl Pts',(16.8985833941536,-17.8969984203578,-12.7793842792735));
#82753=CARTESIAN_POINT('Ctrl Pts',(16.903420087807,-17.8886281741606,-12.7799675007672));
#82754=CARTESIAN_POINT('Ctrl Pts',(16.9113458117626,-17.875126480648,-12.7809086731479));
#82755=CARTESIAN_POINT('Ctrl Pts',(16.9143995407292,-17.8699745676057,-12.781267897193));
#82756=CARTESIAN_POINT('Ctrl Pts',(16.9208163406894,-17.8592528430474,-12.7820157145292));
#82757=CARTESIAN_POINT('Ctrl Pts',(16.9241833133214,-17.8536854305361,-12.7824041604479));
#82758=CARTESIAN_POINT('Ctrl Pts',(16.9322154953229,-17.8405411526983,-12.7833216135196));
#82759=CARTESIAN_POINT('Ctrl Pts',(16.9369029358397,-17.8329779643774,-12.7838497980817));
#82760=CARTESIAN_POINT('Ctrl Pts',(16.9526722795969,-17.8078887681429,-12.7856030771217));
#82761=CARTESIAN_POINT('Ctrl Pts',(16.9639641920581,-17.7904956986808,-12.7868203958941));
#82762=CARTESIAN_POINT('Ctrl Pts',(17.0256057783288,-17.6985355508069,-12.7932713109868));
#82763=CARTESIAN_POINT('Ctrl Pts',(17.0804177574797,-17.6270651376852,-12.7983319640066));
#82764=CARTESIAN_POINT('Ctrl Pts',(17.2287617866374,-17.4572396203864,-12.8107688205488));
#82765=CARTESIAN_POINT('Ctrl Pts',(17.3274941930707,-17.3639855649346,-12.8179810344386));
#82766=CARTESIAN_POINT('Ctrl Pts',(17.4939762702954,-17.2345266456223,-12.8296568863137));
#82767=CARTESIAN_POINT('Ctrl Pts',(17.5559186344873,-17.191461641878,-12.8339175550008));
#82768=CARTESIAN_POINT('Ctrl Pts',(17.628087431752,-17.14680293386,-12.8389474843062));
#82769=CARTESIAN_POINT('Ctrl Pts',(17.6361904509646,-17.1418637502464,-12.8395131452152));
#82770=CARTESIAN_POINT('Ctrl Pts',(17.6482524532083,-17.1346221537431,-12.840356937765));
#82771=CARTESIAN_POINT('Ctrl Pts',(17.6521862699813,-17.1322777618361,-12.8406324017569));
#82772=CARTESIAN_POINT('Ctrl Pts',(17.659201726931,-17.1281276279674,-12.8411242025125));
#82773=CARTESIAN_POINT('Ctrl Pts',(17.6622803605305,-17.1263169028005,-12.8413402107637));
#82774=CARTESIAN_POINT('Ctrl Pts',(17.6689124561005,-17.1224387343665,-12.8418059635862));
#82775=CARTESIAN_POINT('Ctrl Pts',(17.6724673101804,-17.1203738785831,-12.8420558641062));
#82776=CARTESIAN_POINT('Ctrl Pts',(17.682304247197,-17.1146982975689,-12.8427480350089));
#82777=CARTESIAN_POINT('Ctrl Pts',(17.6885988189649,-17.111109490107,-12.8431916789839));
#82778=CARTESIAN_POINT('Ctrl Pts',(17.7233141666129,-17.0915522363204,-12.8456419033174));
#82779=CARTESIAN_POINT('Ctrl Pts',(17.7520807967276,-17.0762105281185,-12.8476849676134));
#82780=CARTESIAN_POINT('Ctrl Pts',(17.9264334001353,-16.9883349739594,-12.8600923397222));
#82781=CARTESIAN_POINT('Ctrl Pts',(18.0796267753151,-16.9321139217962,-12.8710455363536));
#82782=CARTESIAN_POINT('Ctrl Pts',(18.3512832304712,-16.8666085870997,-12.8892984222841));
#82783=CARTESIAN_POINT('Ctrl Pts',(18.466906264726,-16.8486697335391,-12.8967379837458));
#82784=CARTESIAN_POINT('Ctrl Pts',(18.5976891560913,-16.8393446726929,-12.9047438507408));
#82785=CARTESIAN_POINT('Ctrl Pts',(18.6119522531885,-16.8384727251865,-12.9056118112131));
#82786=CARTESIAN_POINT('Ctrl Pts',(18.6346668420434,-16.8373148221815,-12.9069860999014));
#82787=CARTESIAN_POINT('Ctrl Pts',(18.6431129150329,-16.8369349847864,-12.9074953560532));
#82788=CARTESIAN_POINT('Ctrl Pts',(18.6580129430798,-16.8363543169417,-12.9083907290304));
#82789=CARTESIAN_POINT('Ctrl Pts',(18.6644659235801,-16.8361323995316,-12.9087775019588));
#82790=CARTESIAN_POINT('Ctrl Pts',(18.6778148994949,-16.8357344641797,-12.9095755717601));
#82791=CARTESIAN_POINT('Ctrl Pts',(18.684710949815,-16.8355626220266,-12.9099867332395));
#82792=CARTESIAN_POINT('Ctrl Pts',(18.7024144005585,-16.8352080452256,-12.9110394527732));
#82793=CARTESIAN_POINT('Ctrl Pts',(18.7132226678653,-16.8350743662287,-12.9116794694701));
#82794=CARTESIAN_POINT('Ctrl Pts',(18.7583375662738,-16.8348619304341,-12.9143402112538));
#82795=CARTESIAN_POINT('Ctrl Pts',(18.7926436655862,-16.8355343045908,-12.916337405879));
#82796=CARTESIAN_POINT('Ctrl Pts',(18.8819742592859,-16.8394590026465,-12.9214816934866));
#82797=CARTESIAN_POINT('Ctrl Pts',(18.9369158048235,-16.8440266442537,-12.9245893932608));
#82798=CARTESIAN_POINT('Ctrl Pts',(19.1001555303925,-16.8640401745045,-12.933734049447));
#82799=CARTESIAN_POINT('Ctrl Pts',(19.2075002585101,-16.8857365865225,-12.9396222772934));
#82800=CARTESIAN_POINT('Ctrl Pts',(19.3568799015149,-16.9281867031771,-12.9480771552648));
#82801=CARTESIAN_POINT('Ctrl Pts',(19.4006500509014,-16.9421798337911,-12.9505892003355));
#82802=CARTESIAN_POINT('Ctrl Pts',(19.4649308619058,-16.9650611373605,-12.9543731912886));
#82803=CARTESIAN_POINT('Ctrl Pts',(19.4858128918095,-16.9728680448278,-12.9556176889191));
#82804=CARTESIAN_POINT('Ctrl Pts',(19.5544199653136,-16.9997598042307,-12.9597686828353));
#82805=CARTESIAN_POINT('Ctrl Pts',(19.6015696907667,-17.0202514108216,-12.962722046598));
#82806=CARTESIAN_POINT('Ctrl Pts',(19.655028173563,-17.0458367978539,-12.966239644708));
#82807=CARTESIAN_POINT('Ctrl Pts',(19.662114325814,-17.0492769924216,-12.9667094238342));
#82808=CARTESIAN_POINT('Ctrl Pts',(19.6733817024066,-17.0548250103043,-12.9674622631931));
#82809=CARTESIAN_POINT('Ctrl Pts',(19.6775754958605,-17.0569073355133,-12.9677437783263));
#82810=CARTESIAN_POINT('Ctrl Pts',(19.6849751951,-17.0606121263562,-12.9682428623996));
#82811=CARTESIAN_POINT('Ctrl Pts',(19.6881839214519,-17.0622288619646,-12.9684600714186));
#82812=CARTESIAN_POINT('Ctrl Pts',(19.6949590056986,-17.065664182877,-12.9689203964719));
#82813=CARTESIAN_POINT('Ctrl Pts',(19.6985242700208,-17.0674846889663,-12.9691636273886));
#82814=CARTESIAN_POINT('Ctrl Pts',(19.7080948112366,-17.0724059010699,-12.9698191827902));
#82815=CARTESIAN_POINT('Ctrl Pts',(19.7140903794447,-17.0755252404361,-12.9702326551764));
#82816=CARTESIAN_POINT('Ctrl Pts',(19.7432952134849,-17.0908979102039,-12.972259997549));
#82817=CARTESIAN_POINT('Ctrl Pts',(19.7662890636642,-17.1035528249061,-12.9738973123395));
#82818=CARTESIAN_POINT('Ctrl Pts',(19.831477636975,-17.1410257200416,-12.9786454183624));
#82819=CARTESIAN_POINT('Ctrl Pts',(19.8730532935303,-17.1668832060134,-12.9818037835828));
#82820=CARTESIAN_POINT('Ctrl Pts',(19.993943561746,-17.2480129179584,-12.9913042266508));
#82821=CARTESIAN_POINT('Ctrl Pts',(20.0704112864608,-17.3073011131475,-12.9977331014421));
#82822=CARTESIAN_POINT('Ctrl Pts',(20.2478325446529,-17.4654316091008,-13.0133685743738));
#82823=CARTESIAN_POINT('Ctrl Pts',(20.3434827441866,-17.5695553533997,-13.0224360878211));
#82824=CARTESIAN_POINT('Ctrl Pts',(20.4366434862985,-17.6938671981591,-13.0319214172026));
#82825=CARTESIAN_POINT('Ctrl Pts',(20.4450929332443,-17.70538298664,-13.0327889690181));
#82826=CARTESIAN_POINT('Ctrl Pts',(20.4583563904069,-17.7238487536606,-13.0341627349987));
#82827=CARTESIAN_POINT('Ctrl Pts',(20.4632463177956,-17.730743425545,-13.0346718736355));
#82828=CARTESIAN_POINT('Ctrl Pts',(20.4717983283495,-17.7429558920469,-13.0355671099326));
#82829=CARTESIAN_POINT('Ctrl Pts',(20.4754775983943,-17.7482614649711,-13.0359538630655));
#82830=CARTESIAN_POINT('Ctrl Pts',(20.4830379644293,-17.7592708633556,-13.0367519590075));
#82831=CARTESIAN_POINT('Ctrl Pts',(20.4869155702732,-17.7649770012162,-13.037163166093));
#82832=CARTESIAN_POINT('Ctrl Pts',(20.4967986024945,-17.7796745358065,-13.0382161410989));
#82833=CARTESIAN_POINT('Ctrl Pts',(20.5027632109011,-17.7886932402494,-13.0388563661931));
#82834=CARTESIAN_POINT('Ctrl Pts',(20.5273801485272,-17.8265420060082,-13.0415191343029));
#82835=CARTESIAN_POINT('Ctrl Pts',(20.5453993771964,-17.8557789699148,-13.0435181010877));
#82836=CARTESIAN_POINT('Ctrl Pts',(20.5904983054417,-17.9331047852169,-13.0486679860457));
#82837=CARTESIAN_POINT('Ctrl Pts',(20.6164237228005,-17.9818376464868,-13.0517793984954));
#82838=CARTESIAN_POINT('Ctrl Pts',(20.6879862345602,-18.1300533123686,-13.0609305311442));
#82839=CARTESIAN_POINT('Ctrl Pts',(20.727847880218,-18.2321180169854,-13.0668215445066));
#82840=CARTESIAN_POINT('Ctrl Pts',(20.7744330181973,-18.3855083481516,-13.0755497076273));
#82841=CARTESIAN_POINT('Ctrl Pts',(20.7874623617863,-18.4347266943472,-13.0783341369971));
#82842=CARTESIAN_POINT('Ctrl Pts',(20.8021800539444,-18.4997083215456,-13.0820409998631));
#82843=CARTESIAN_POINT('Ctrl Pts',(20.8054839908773,-18.5150897620407,-13.0829206782023));
#82844=CARTESIAN_POINT('Ctrl Pts',(20.8191178946672,-18.5821966201499,-13.0867737076442));
#82845=CARTESIAN_POINT('Ctrl Pts',(20.8276832347021,-18.6342568668373,-13.08980165725));
#82846=CARTESIAN_POINT('Ctrl Pts',(20.8353850232781,-18.695201363867,-13.0934472532827));
#82847=CARTESIAN_POINT('Ctrl Pts',(20.8364216869795,-18.7038315091866,-13.0939658392605));
#82848=CARTESIAN_POINT('Ctrl Pts',(20.8379117367722,-18.716916080413,-13.0947559733477));
#82849=CARTESIAN_POINT('Ctrl Pts',(20.8384042010401,-18.7213660840759,-13.0950253736331));
#82850=CARTESIAN_POINT('Ctrl Pts',(20.8392632774873,-18.7293607590349,-13.0955106389907));
#82851=CARTESIAN_POINT('Ctrl Pts',(20.8396350588734,-18.7329048204634,-13.0957262100106));
#82852=CARTESIAN_POINT('Ctrl Pts',(20.8404239568868,-18.7406126208114,-13.0961960375615));
#82853=CARTESIAN_POINT('Ctrl Pts',(20.8408376718702,-18.744776608666,-13.0964504770346));
#82854=CARTESIAN_POINT('Ctrl Pts',(20.8419662927908,-18.7564888838651,-13.0971678554369));
#82855=CARTESIAN_POINT('Ctrl Pts',(20.8426529878658,-18.7640397359935,-13.097632333511));
#82856=CARTESIAN_POINT('Ctrl Pts',(20.8465378410405,-18.8094612654796,-13.100437644118));
#82857=CARTESIAN_POINT('Ctrl Pts',(20.8487560509632,-18.8474062613524,-13.1028282312516));
#82858=CARTESIAN_POINT('Ctrl Pts',(20.8527120532288,-18.9730690375215,-13.1108564341275));
#82859=CARTESIAN_POINT('Ctrl Pts',(20.8500194555176,-19.0608319706576,-13.1166390368668));
#82860=CARTESIAN_POINT('Ctrl Pts',(20.8257290822401,-19.3218395735466,-13.1339593892005));
#82861=CARTESIAN_POINT('Ctrl Pts',(20.7881616401392,-19.4928834194246,-13.1454065362316));
#82862=CARTESIAN_POINT('Ctrl Pts',(20.7223354015534,-19.6791474167087,-13.1575672063208));
#82863=CARTESIAN_POINT('Ctrl Pts',(20.7142945423085,-19.7007687403044,-13.1589753661778));
#82864=CARTESIAN_POINT('Ctrl Pts',(20.7024239030545,-19.7311583289424,-13.1609503969806));
#82865=CARTESIAN_POINT('Ctrl Pts',(20.6988858337083,-19.7400380884553,-13.1615269876774));
#82866=CARTESIAN_POINT('Ctrl Pts',(20.6930408000488,-19.7544236867725,-13.1624603452406));
#82867=CARTESIAN_POINT('Ctrl Pts',(20.690770505534,-19.7599441930948,-13.1628183443127));
#82868=CARTESIAN_POINT('Ctrl Pts',(20.6859705830224,-19.7714768983658,-13.1635658828843));
#82869=CARTESIAN_POINT('Ctrl Pts',(20.6834364534085,-19.7774871649704,-13.1639552650303));
#82870=CARTESIAN_POINT('Ctrl Pts',(20.6773439872508,-19.791752314378,-13.1648790281169));
#82871=CARTESIAN_POINT('Ctrl Pts',(20.6737607535061,-19.799996477139,-13.1654125549704));
#82872=CARTESIAN_POINT('Ctrl Pts',(20.6615229563997,-19.8276692370202,-13.1672024814055));
#82873=CARTESIAN_POINT('Ctrl Pts',(20.6526279719372,-19.8469905664031,-13.1684506452609));
#82874=CARTESIAN_POINT('Ctrl Pts',(20.5767438129362,-20.0054902695259,-13.1786845902747));
#82875=CARTESIAN_POINT('Ctrl Pts',(20.4949977213949,-20.1370911318832,-13.1871018764965));
#82876=CARTESIAN_POINT('Ctrl Pts',(20.3152312142637,-20.3662502057235,-13.2029185793079));
#82877=CARTESIAN_POINT('Ctrl Pts',(20.2205947451412,-20.4654138490875,-13.2103041963936));
#82878=CARTESIAN_POINT('Ctrl Pts',(20.1052748682238,-20.5649281362042,-13.2192364240755));
#82879=CARTESIAN_POINT('Ctrl Pts',(20.0933629325293,-20.5749800745963,-13.2201585288741));
#82880=CARTESIAN_POINT('Ctrl Pts',(20.0768874313485,-20.5885743771724,-13.2214348812018));
#82881=CARTESIAN_POINT('Ctrl Pts',(20.0724184152457,-20.5922312304195,-13.2217811920167));
#82882=CARTESIAN_POINT('Ctrl Pts',(20.0652881973517,-20.5980171172175,-13.222333979641));
#82883=CARTESIAN_POINT('Ctrl Pts',(20.0626366811656,-20.6001581185257,-13.2225396008818));
#82884=CARTESIAN_POINT('Ctrl Pts',(20.057145599092,-20.6045701026581,-13.2229655689635));
#82885=CARTESIAN_POINT('Ctrl Pts',(20.0543053566104,-20.6068401690569,-13.2231859810243));
#82886=CARTESIAN_POINT('Ctrl Pts',(20.0475167370122,-20.6122373777806,-13.2237129696987));
#82887=CARTESIAN_POINT('Ctrl Pts',(20.0435630325112,-20.6153577581711,-13.2240200239175));
#82888=CARTESIAN_POINT('Ctrl Pts',(20.0301588734137,-20.6258593036124,-13.2250613688593));
#82889=CARTESIAN_POINT('Ctrl Pts',(20.0206570535133,-20.633174114956,-13.2258001254407));
#82890=CARTESIAN_POINT('Ctrl Pts',(19.9093804162313,-20.7173425996273,-13.2344534122617));
#82891=CARTESIAN_POINT('Ctrl Pts',(19.8009334406734,-20.7849211402687,-13.242886937252));
#82892=CARTESIAN_POINT('Ctrl Pts',(19.5396963320284,-20.9166338298046,-13.262220692687));
#82893=CARTESIAN_POINT('Ctrl Pts',(19.3841004551618,-20.9734652468898,-13.2730159395898));
#82894=CARTESIAN_POINT('Ctrl Pts',(19.20049174163,-21.0170984707196,-13.2846391271698));
#82895=CARTESIAN_POINT('Ctrl Pts',(19.1774350585562,-21.0221718910315,-13.286080754895));
#82896=CARTESIAN_POINT('Ctrl Pts',(19.1448415986351,-21.0287742452012,-13.288094211721));
#82897=CARTESIAN_POINT('Ctrl Pts',(19.1353725087011,-21.0306250741248,-13.2886762773883));
#82898=CARTESIAN_POINT('Ctrl Pts',(19.1200090256569,-21.0335191224342,-13.2896160865066));
#82899=CARTESIAN_POINT('Ctrl Pts',(19.1141223600509,-21.0346021745597,-13.2899750959463));
#82900=CARTESIAN_POINT('Ctrl Pts',(19.101824633021,-21.0368108802772,-13.2907228579707));
#82901=CARTESIAN_POINT('Ctrl Pts',(19.0954128061921,-21.0379319624952,-13.2911114614653));
#82902=CARTESIAN_POINT('Ctrl Pts',(19.0802087498384,-21.0405181226784,-13.2920299871718));
#82903=CARTESIAN_POINT('Ctrl Pts',(19.0714121924375,-21.0419572874384,-13.2925590814457));
#82904=CARTESIAN_POINT('Ctrl Pts',(19.0426192480071,-21.0464814445051,-13.2942834838662));
#82905=CARTESIAN_POINT('Ctrl Pts',(19.0225873094142,-21.0493353971963,-13.2954714804212));
#82906=CARTESIAN_POINT('Ctrl Pts',(18.9749216392829,-21.0554304646181,-13.2982724891217));
#82907=CARTESIAN_POINT('Ctrl Pts',(18.947258561768,-21.0584149263371,-13.2998775423216));
#82908=CARTESIAN_POINT('Ctrl Pts',(18.750836523532,-21.0756967747023,-13.3111481661307));
#82909=CARTESIAN_POINT('Ctrl Pts',(18.5809630246235,-21.0702430855674,-13.320175318181));
#82910=CARTESIAN_POINT('Ctrl Pts',(18.3107914109264,-21.028870241372,-13.3351121817024));
#82911=CARTESIAN_POINT('Ctrl Pts',(18.2093467407402,-21.0055892059446,-13.3408765441184));
#82912=CARTESIAN_POINT('Ctrl Pts',(18.100779628979,-20.9721026746093,-13.3476075994602));
#82913=CARTESIAN_POINT('Ctrl Pts',(18.091542052835,-20.9691838370138,-13.3481849116236));
#82914=CARTESIAN_POINT('Ctrl Pts',(18.0779311492103,-20.9647801643989,-13.3490427800663));
#82915=CARTESIAN_POINT('Ctrl Pts',(18.0735419745929,-20.9633442079671,-13.3493205378534));
#82916=CARTESIAN_POINT('Ctrl Pts',(18.0657629024586,-20.96077100891,-13.3498148582613));
#82917=CARTESIAN_POINT('Ctrl Pts',(18.0623711506552,-20.9596395277255,-13.3500310793731));
#82918=CARTESIAN_POINT('Ctrl Pts',(18.0551094862089,-20.957196590331,-13.3504955064512));
#82919=CARTESIAN_POINT('Ctrl Pts',(18.0512405574551,-20.9558825411071,-13.3507438590022));
#82920=CARTESIAN_POINT('Ctrl Pts',(18.0406289262692,-20.9522440904301,-13.3514274927815));
#82921=CARTESIAN_POINT('Ctrl Pts',(18.0338942003764,-20.949896827462,-13.3518640934334));
#82922=CARTESIAN_POINT('Ctrl Pts',(17.9984774555781,-20.937351918409,-13.3541740180201));
#82923=CARTESIAN_POINT('Ctrl Pts',(17.9700075772509,-20.9265710947681,-13.3560790445638));
#82924=CARTESIAN_POINT('Ctrl Pts',(17.7914208839187,-20.8545045692563,-13.3682924779572));
#82925=CARTESIAN_POINT('Ctrl Pts',(17.648533283028,-20.776757592915,-13.3792084718668));
#82926=CARTESIAN_POINT('Ctrl Pts',(17.4180928158084,-20.6146437362195,-13.3976307292246));
#82927=CARTESIAN_POINT('Ctrl Pts',(17.3262603531878,-20.5376460354167,-13.4052583400663));
#82928=CARTESIAN_POINT('Ctrl Pts',(17.2302711961142,-20.4422132351479,-13.4135235262956));
#82929=CARTESIAN_POINT('Ctrl Pts',(17.2192537705425,-20.4310130773836,-13.4144773329668));
#82930=CARTESIAN_POINT('Ctrl Pts',(17.2027731928931,-20.4138818164368,-13.4159122608872));
#82931=CARTESIAN_POINT('Ctrl Pts',(17.1972177502792,-20.4080406243576,-13.4163973987769));
#82932=CARTESIAN_POINT('Ctrl Pts',(17.1873222616745,-20.3975164254442,-13.4172641882906));
#82933=CARTESIAN_POINT('Ctrl Pts',(17.1829698046474,-20.3928452716892,-13.4176463725963));
#82934=CARTESIAN_POINT('Ctrl Pts',(17.17377904543,-20.3828916397041,-13.4184554318016));
#82935=CARTESIAN_POINT('Ctrl Pts',(17.168946279822,-20.3776041408986,-13.4188820679075));
#82936=CARTESIAN_POINT('Ctrl Pts',(17.1591628939954,-20.3667904910308,-13.4197482784963));
#82937=CARTESIAN_POINT('Ctrl Pts',(17.1542142980577,-20.3612626377019,-13.4201877647381));
#82938=CARTESIAN_POINT('Ctrl Pts',(17.1324256429663,-20.3366645202445,-13.4221289594741));
#82939=CARTESIAN_POINT('Ctrl Pts',(17.1159006368997,-20.3173171016113,-13.4236175617699));
#82940=CARTESIAN_POINT('Ctrl Pts',(17.0457285969941,-20.2320958290432,-13.4300186821377));
#82941=CARTESIAN_POINT('Ctrl Pts',(16.9957224725482,-20.1633212222884,-13.4347859059221));
#82942=CARTESIAN_POINT('Ctrl Pts',(16.9128101395665,-20.0335375559321,-13.4432735523562));
#82943=CARTESIAN_POINT('Ctrl Pts',(16.8785074225223,-19.9735692052281,-13.4470186833148));
#82944=CARTESIAN_POINT('Ctrl Pts',(16.8085769131631,-19.8361307746912,-13.4553932932223));
#82945=CARTESIAN_POINT('Ctrl Pts',(16.7745951536274,-19.7580132150682,-13.460014549721));
#82946=CARTESIAN_POINT('Ctrl Pts',(16.7454194853472,-19.6781105540779,-13.4647888353055));
#82947=CARTESIAN_POINT('',(16.6170008459317,-18.9538925311169,-12.4890563034236));
#82948=CARTESIAN_POINT('Ctrl Pts',(16.7454194499637,-19.6781104571739,-13.2445592876386));
#82949=CARTESIAN_POINT('Ctrl Pts',(16.7717392418346,-19.7501918129489,-13.2399327110257));
#82950=CARTESIAN_POINT('Ctrl Pts',(16.8019456368363,-19.820740464874,-13.2353061344128));
#82951=CARTESIAN_POINT('Ctrl Pts',(16.8358258581282,-19.8893494157086,-13.2306795577999));
#82952=CARTESIAN_POINT('Ctrl Pts',(16.8465556082421,-19.911077635595,-13.229214336823));
#82953=CARTESIAN_POINT('Ctrl Pts',(16.8576534978601,-19.9326115175269,-13.2277491158461));
#82954=CARTESIAN_POINT('Ctrl Pts',(16.8691118619909,-19.9539387370059,-13.2262838948692));
#82955=CARTESIAN_POINT('Ctrl Pts',(16.9034286623953,-20.017811897754,-13.2218956859383));
#82956=CARTESIAN_POINT('Ctrl Pts',(16.9410977666971,-20.0800446523181,-13.2175074770074));
#82957=CARTESIAN_POINT('Ctrl Pts',(16.9819381659419,-20.1402627359456,-13.2131192680765));
#82958=CARTESIAN_POINT('Ctrl Pts',(17.0227179512628,-20.2003914459526,-13.2087375719752));
#82959=CARTESIAN_POINT('Ctrl Pts',(17.0666594195118,-20.2585110248676,-13.2043558758739));
#82960=CARTESIAN_POINT('Ctrl Pts',(17.1135357879723,-20.3142719029391,-13.1999741797727));
#82961=CARTESIAN_POINT('Ctrl Pts',(17.1603570729693,-20.3699672575413,-13.195597632513));
#82962=CARTESIAN_POINT('Ctrl Pts',(17.2101060983655,-20.4233090498181,-13.1912210852534));
#82963=CARTESIAN_POINT('Ctrl Pts',(17.2625139124404,-20.4739782173601,-13.1868445379937));
#82964=CARTESIAN_POINT('Ctrl Pts',(17.3148884902414,-20.5246152512525,-13.1824707662767));
#82965=CARTESIAN_POINT('Ctrl Pts',(17.3699181652074,-20.5725826889237,-13.1780969945598));
#82966=CARTESIAN_POINT('Ctrl Pts',(17.427295955156,-20.6175970518671,-13.1737232228428));
#82967=CARTESIAN_POINT('Ctrl Pts',(17.4846562848506,-20.6625977167887,-13.1693507820792));
#82968=CARTESIAN_POINT('Ctrl Pts',(17.5443629316538,-20.7046467934755,-13.1649783413157));
#82969=CARTESIAN_POINT('Ctrl Pts',(17.6060758346845,-20.743501068182,-13.1606059005521));
#82970=CARTESIAN_POINT('Ctrl Pts',(17.667790315721,-20.7823563363967,-13.1562333479848));
#82971=CARTESIAN_POINT('Ctrl Pts',(17.7315107455617,-20.8180163851248,-13.1518607954174));
#82972=CARTESIAN_POINT('Ctrl Pts',(17.7968695201153,-20.8502822402559,-13.1474882428501));
#82973=CARTESIAN_POINT('Ctrl Pts',(17.8622961264704,-20.8825815821085,-13.1431111522827));
#82974=CARTESIAN_POINT('Ctrl Pts',(17.9293640389074,-20.9114794832211,-13.1387340617154));
#82975=CARTESIAN_POINT('Ctrl Pts',(17.9976833250409,-20.9368241116475,-13.134356971148));
#82976=CARTESIAN_POINT('Ctrl Pts',(18.0660399228722,-20.9621825817161,-13.1299774900891));
#82977=CARTESIAN_POINT('Ctrl Pts',(18.135648794438,-20.9839837711618,-13.1255980090301));
#82978=CARTESIAN_POINT('Ctrl Pts',(18.2061050046745,-21.0021258190439,-13.1212185279712));
#82979=CARTESIAN_POINT('Ctrl Pts',(18.2766860980708,-21.0203000235841,-13.1168312843115));
#82980=CARTESIAN_POINT('Ctrl Pts',(18.3481170562253,-21.0348020386144,-13.1124440406517));
#82981=CARTESIAN_POINT('Ctrl Pts',(18.4199835016935,-21.0455812950042,-13.108056796992));
#82982=CARTESIAN_POINT('Ctrl Pts',(18.4688457595767,-21.0529101506624,-13.1050738940573));
#82983=CARTESIAN_POINT('Ctrl Pts',(18.517909182164,-21.0585191746184,-13.1020909911225));
#82984=CARTESIAN_POINT('Ctrl Pts',(18.5670433388759,-21.0624062341896,-13.0991080881877));
#82985=CARTESIAN_POINT('Ctrl Pts',(18.6393255921073,-21.0681245662635,-13.0947198792568));
#82986=CARTESIAN_POINT('Ctrl Pts',(18.7120430618562,-21.0701362205188,-13.0903316703259));
#82987=CARTESIAN_POINT('Ctrl Pts',(18.7847830739802,-21.0683908144285,-13.085943461395));
#82988=CARTESIAN_POINT('Ctrl Pts',(18.8574151278658,-21.0666479988102,-13.0815617652938));
#82989=CARTESIAN_POINT('Ctrl Pts',(18.9300691794577,-21.0611592036426,-13.0771800691925));
#82990=CARTESIAN_POINT('Ctrl Pts',(19.0023285427326,-21.0519259018249,-13.0727983730912));
#82991=CARTESIAN_POINT('Ctrl Pts',(19.074502995505,-21.0427034498716,-13.0684218258316));
#82992=CARTESIAN_POINT('Ctrl Pts',(19.14628320517,-21.0297452929198,-13.064045278572));
#82993=CARTESIAN_POINT('Ctrl Pts',(19.2172553122691,-21.0131048743729,-13.0596687313123));
#82994=CARTESIAN_POINT('Ctrl Pts',(19.2881824098894,-20.9964750089376,-13.0552949595954));
#82995=CARTESIAN_POINT('Ctrl Pts',(19.358301953298,-20.9761676251632,-13.0509211878784));
#82996=CARTESIAN_POINT('Ctrl Pts',(19.4272094182993,-20.9522874049449,-13.0465474161614));
#82997=CARTESIAN_POINT('Ctrl Pts',(19.4960959145276,-20.9284144515578,-13.0421749753979));
#82998=CARTESIAN_POINT('Ctrl Pts',(19.563770609099,-20.9009709780648,-13.0378025346343));
#82999=CARTESIAN_POINT('Ctrl Pts',(19.6298449292376,-20.8701112748637,-13.0334300938708));
#83000=CARTESIAN_POINT('Ctrl Pts',(19.6959209389039,-20.8392507825766,-13.0290575413034));
#83001=CARTESIAN_POINT('Ctrl Pts',(19.7603960566783,-20.8049740930876,-13.0246849887361));
#83002=CARTESIAN_POINT('Ctrl Pts',(19.8229039996999,-20.7674826023506,-13.0203124361687));
#83003=CARTESIAN_POINT('Ctrl Pts',(19.8854768158225,-20.7299522015303,-13.0159353456014));
#83004=CARTESIAN_POINT('Ctrl Pts',(19.9460779664247,-20.6892005866783,-13.0115582550341));
#83005=CARTESIAN_POINT('Ctrl Pts',(20.0043687218632,-20.6454734454699,-13.0071811644668));
#83006=CARTESIAN_POINT('Ctrl Pts',(20.0626913120466,-20.6017224232467,-13.0028016834078));
#83007=CARTESIAN_POINT('Ctrl Pts',(20.1187006241993,-20.5549929484574,-12.9984222023489));
#83008=CARTESIAN_POINT('Ctrl Pts',(20.1720918257202,-20.505570372013,-12.9940427212899));
#83009=CARTESIAN_POINT('Ctrl Pts',(20.2255776627874,-20.4560601943837,-12.9896554776302));
#83010=CARTESIAN_POINT('Ctrl Pts',(20.276435785288,-20.4038477284535,-12.9852682339705));
#83011=CARTESIAN_POINT('Ctrl Pts',(20.3243993779345,-20.3492540279655,-12.9808809903108));
#83012=CARTESIAN_POINT('Ctrl Pts',(20.3570099991733,-20.3121355722701,-12.977898087376));
#83013=CARTESIAN_POINT('Ctrl Pts',(20.3882834007586,-20.2739170566123,-12.9749151844411));
#83014=CARTESIAN_POINT('Ctrl Pts',(20.4181471898432,-20.2347069980878,-12.9719322815063));
#83015=CARTESIAN_POINT('Ctrl Pts',(20.4620804149045,-20.1770242867296,-12.9675440725754));
#83016=CARTESIAN_POINT('Ctrl Pts',(20.5031324849612,-20.1169692727542,-12.9631558636445));
#83017=CARTESIAN_POINT('Ctrl Pts',(20.541037663595,-20.0548616787019,-12.9587676547136));
#83018=CARTESIAN_POINT('Ctrl Pts',(20.578886584659,-19.9928462626168,-12.9543859586124));
#83019=CARTESIAN_POINT('Ctrl Pts',(20.6135976366773,-19.9287847222599,-12.9500042625111));
#83020=CARTESIAN_POINT('Ctrl Pts',(20.6449465138838,-19.8630282218874,-12.9456225664098));
#83021=CARTESIAN_POINT('Ctrl Pts',(20.6762585536647,-19.7973489906359,-12.9412460191502));
#83022=CARTESIAN_POINT('Ctrl Pts',(20.7042160604134,-19.7299791891849,-12.9368694718905));
#83023=CARTESIAN_POINT('Ctrl Pts',(20.728639957299,-19.661295735745,-12.9324929246309));
#83024=CARTESIAN_POINT('Ctrl Pts',(20.7530483649043,-19.5926558403532,-12.9281191529139));
#83025=CARTESIAN_POINT('Ctrl Pts',(20.7739274477879,-19.5227043993277,-12.9237453811969));
#83026=CARTESIAN_POINT('Ctrl Pts',(20.7911462655829,-19.4518382158243,-12.91937160948));
#83027=CARTESIAN_POINT('Ctrl Pts',(20.8083598436337,-19.3809935971386,-12.9149991687164));
#83028=CARTESIAN_POINT('Ctrl Pts',(20.8219152540694,-19.3092352570616,-12.9106267279528));
#83029=CARTESIAN_POINT('Ctrl Pts',(20.8317319036236,-19.2369734382707,-12.9062542871893));
#83030=CARTESIAN_POINT('Ctrl Pts',(20.8415488041906,-19.1647097717371,-12.9018817346219));
#83031=CARTESIAN_POINT('Ctrl Pts',(20.847626691118,-19.0919430791858,-12.8975091820546));
#83032=CARTESIAN_POINT('Ctrl Pts',(20.8499366445659,-19.0190903583475,-12.8931366294872));
#83033=CARTESIAN_POINT('Ctrl Pts',(20.8522489953706,-18.9461620282076,-12.8887595389199));
#83034=CARTESIAN_POINT('Ctrl Pts',(20.8507855897922,-18.8731479746872,-12.8843824483526));
#83035=CARTESIAN_POINT('Ctrl Pts',(20.8455696643532,-18.8004660018902,-12.8800053577853));
#83036=CARTESIAN_POINT('Ctrl Pts',(20.8403508903038,-18.7277443347703,-12.8756258767263));
#83037=CARTESIAN_POINT('Ctrl Pts',(20.8313755754733,-18.6553555885068,-12.8712463956674));
#83038=CARTESIAN_POINT('Ctrl Pts',(20.8187186547149,-18.5837105341125,-12.8668669146084));
#83039=CARTESIAN_POINT('Ctrl Pts',(20.8060392996494,-18.5119384893402,-12.8624796709487));
#83040=CARTESIAN_POINT('Ctrl Pts',(20.789665415713,-18.4409132392693,-12.858092427289));
#83041=CARTESIAN_POINT('Ctrl Pts',(20.769722536241,-18.371032913634,-12.8537051836293));
#83042=CARTESIAN_POINT('Ctrl Pts',(20.7561632998913,-18.3235210258541,-12.8507222806944));
#83043=CARTESIAN_POINT('Ctrl Pts',(20.7409552755656,-18.27653808659,-12.8477393777596));
#83044=CARTESIAN_POINT('Ctrl Pts',(20.7241505240927,-18.2302037050152,-12.8447564748248));
#83045=CARTESIAN_POINT('Ctrl Pts',(20.6994287137936,-18.1620402577033,-12.8403682658939));
#83046=CARTESIAN_POINT('Ctrl Pts',(20.6711526578599,-18.0950153233851,-12.835980056963));
#83047=CARTESIAN_POINT('Ctrl Pts',(20.6394473542677,-18.0295254040819,-12.8315918480321));
#83048=CARTESIAN_POINT('Ctrl Pts',(20.6077891066029,-17.9641326826773,-12.8272101519309));
#83049=CARTESIAN_POINT('Ctrl Pts',(20.5727119232316,-17.9002708843009,-12.8228284558296));
#83050=CARTESIAN_POINT('Ctrl Pts',(20.5343896652636,-17.8383186931567,-12.8184467597283));
#83051=CARTESIAN_POINT('Ctrl Pts',(20.4961124389984,-17.7764393007675,-12.8140702124687));
#83052=CARTESIAN_POINT('Ctrl Pts',(20.4545979656273,-17.7164654662072,-12.8096936652091));
#83053=CARTESIAN_POINT('Ctrl Pts',(20.410066242825,-17.6587517834296,-12.8053171179494));
#83054=CARTESIAN_POINT('Ctrl Pts',(20.365562761394,-17.6010747018308,-12.8009433462325));
#83055=CARTESIAN_POINT('Ctrl Pts',(20.318046121109,-17.5456553090191,-12.7965695745155));
#83056=CARTESIAN_POINT('Ctrl Pts',(20.2677790950911,-17.4928184871437,-12.7921958027985));
#83057=CARTESIAN_POINT('Ctrl Pts',(20.217527365498,-17.4399977436906,-12.787823362035));
#83058=CARTESIAN_POINT('Ctrl Pts',(20.1645272440669,-17.3897583602253,-12.7834509212714));
#83059=CARTESIAN_POINT('Ctrl Pts',(20.1090800563607,-17.342390159511,-12.7790784805079));
#83060=CARTESIAN_POINT('Ctrl Pts',(20.0536314508638,-17.2950207475865,-12.7747059279405));
#83061=CARTESIAN_POINT('Ctrl Pts',(19.9957360229245,-17.2505229759785,-12.7703333753732));
#83062=CARTESIAN_POINT('Ctrl Pts',(19.9357287478822,-17.2091468746583,-12.7659608228059));
#83063=CARTESIAN_POINT('Ctrl Pts',(19.8756591950264,-17.1677278316594,-12.7615837322385));
#83064=CARTESIAN_POINT('Ctrl Pts',(19.8134738170564,-17.1294372018124,-12.7572066416712));
#83065=CARTESIAN_POINT('Ctrl Pts',(19.7495364985935,-17.0944815963161,-12.7528295511039));
#83066=CARTESIAN_POINT('Ctrl Pts',(19.6855642615879,-17.0595069002662,-12.7484500700449));
#83067=CARTESIAN_POINT('Ctrl Pts',(19.6198386140604,-17.027871064273,-12.744070588986));
#83068=CARTESIAN_POINT('Ctrl Pts',(19.5527455102415,-16.999733422542,-12.7396911079271));
#83069=CARTESIAN_POINT('Ctrl Pts',(19.4855334843464,-16.9715459070299,-12.7353038642674));
#83070=CARTESIAN_POINT('Ctrl Pts',(19.4169496162068,-16.9468691314342,-12.7309166206076));
#83071=CARTESIAN_POINT('Ctrl Pts',(19.3473966187373,-16.9258130421598,-12.7265293769479));
#83072=CARTESIAN_POINT('Ctrl Pts',(19.3001072825687,-16.9114969304131,-12.7235464740131));
#83073=CARTESIAN_POINT('Ctrl Pts',(19.2523702507342,-16.8988534982272,-12.7205635710783));
#83074=CARTESIAN_POINT('Ctrl Pts',(19.2043142751595,-16.8879037128609,-12.7175806681434));
#83075=CARTESIAN_POINT('Ctrl Pts',(19.1336181560408,-16.8717952618032,-12.7131924592126));
#83076=CARTESIAN_POINT('Ctrl Pts',(19.061955500426,-16.8592916243426,-12.7088042502817));
#83077=CARTESIAN_POINT('Ctrl Pts',(18.9897273628005,-16.8505023159863,-12.7044160413508));
#83078=CARTESIAN_POINT('Ctrl Pts',(18.917606423707,-16.8417260524208,-12.7000343452495));
#83079=CARTESIAN_POINT('Ctrl Pts',(18.8449221435538,-16.8366532323251,-12.6956526491482));
#83080=CARTESIAN_POINT('Ctrl Pts',(18.7720870435493,-16.8353426405973,-12.691270953047));
#83081=CARTESIAN_POINT('Ctrl Pts',(18.6993375305838,-16.8340335889191,-12.6868944057873));
#83082=CARTESIAN_POINT('Ctrl Pts',(18.6264380297321,-16.8364779920626,-12.6825178585277));
#83083=CARTESIAN_POINT('Ctrl Pts',(18.5538057789625,-16.8426828017805,-12.6781413112681));
#83084=CARTESIAN_POINT('Ctrl Pts',(18.4812195905107,-16.8488836764982,-12.6737675395511));
#83085=CARTESIAN_POINT('Ctrl Pts',(18.4089007953032,-16.8588401850895,-12.6693937678341));
#83086=CARTESIAN_POINT('Ctrl Pts',(18.3372648019203,-16.8725072294897,-12.6650199961172));
#83087=CARTESIAN_POINT('Ctrl Pts',(18.2656506076109,-16.8861701149623,-12.6606475553536));
#83088=CARTESIAN_POINT('Ctrl Pts',(18.1947192761675,-16.9035412042303,-12.6562751145901));
#83089=CARTESIAN_POINT('Ctrl Pts',(18.1248776044808,-16.9245240057458,-12.6519026738265));
#83090=CARTESIAN_POINT('Ctrl Pts',(18.0550341469347,-16.9455073437939,-12.6475301212592));
#83091=CARTESIAN_POINT('Ctrl Pts',(17.9862808658674,-16.9701024367363,-12.6431575686918));
#83092=CARTESIAN_POINT('Ctrl Pts',(17.9190093127146,-16.998162959805,-12.6387850161245));
#83093=CARTESIAN_POINT('Ctrl Pts',(17.8516679426066,-17.0262526051429,-12.6344079255571));
#83094=CARTESIAN_POINT('Ctrl Pts',(17.7858118168726,-17.0578146752693,-12.6300308349898));
#83095=CARTESIAN_POINT('Ctrl Pts',(17.7218116266778,-17.0926550355269,-12.6256537444225));
#83096=CARTESIAN_POINT('Ctrl Pts',(17.6577764836039,-17.1275144233984,-12.6212742633635));
#83097=CARTESIAN_POINT('Ctrl Pts',(17.5955997055921,-17.1656554136578,-12.6168947823046));
#83098=CARTESIAN_POINT('Ctrl Pts',(17.5356241771988,-17.2068397244592,-12.6125153012457));
#83099=CARTESIAN_POINT('Ctrl Pts',(17.475542342584,-17.2480970341751,-12.6081280575859));
#83100=CARTESIAN_POINT('Ctrl Pts',(17.4176699324644,-17.2924081430501,-12.6037408139262));
#83101=CARTESIAN_POINT('Ctrl Pts',(17.3623173752297,-17.3394939451577,-12.5993535702665));
#83102=CARTESIAN_POINT('Ctrl Pts',(17.3246829700697,-17.3715077534138,-12.5963706673317));
#83103=CARTESIAN_POINT('Ctrl Pts',(17.2882126945402,-17.404803392597,-12.5933877643969));
#83104=CARTESIAN_POINT('Ctrl Pts',(17.2529938697634,-17.4392839518926,-12.590404861462));
#83105=CARTESIAN_POINT('Ctrl Pts',(17.2019441492123,-17.4892635559153,-12.5860811407752));
#83106=CARTESIAN_POINT('Ctrl Pts',(17.1533139178898,-17.5419415318573,-12.5817574200883));
#83107=CARTESIAN_POINT('Ctrl Pts',(17.1074080252024,-17.5970507214202,-12.5774336994015));
#83108=CARTESIAN_POINT('Ctrl Pts',(17.061563088785,-17.652086734089,-12.5731157199795));
#83109=CARTESIAN_POINT('Ctrl Pts',(17.0184356374498,-17.7095471849219,-12.5687977405574));
#83110=CARTESIAN_POINT('Ctrl Pts',(16.9782947055966,-17.7691272599286,-12.5644797611354));
#83111=CARTESIAN_POINT('Ctrl Pts',(16.9381929308678,-17.8286492150987,-12.5601659938641));
#83112=CARTESIAN_POINT('Ctrl Pts',(16.9010721765566,-17.8902862851977,-12.5558522265929));
#83113=CARTESIAN_POINT('Ctrl Pts',(16.8671608676011,-17.9537011200325,-12.5515384593216));
#83114=CARTESIAN_POINT('Ctrl Pts',(16.8332706976895,-18.0170764244272,-12.5472273810918));
#83115=CARTESIAN_POINT('Ctrl Pts',(16.8025862384805,-18.0822268576,-12.542916302862));
#83116=CARTESIAN_POINT('Ctrl Pts',(16.7752912625976,-18.1487882707382,-12.5386052246321));
#83117=CARTESIAN_POINT('Ctrl Pts',(16.7479923079761,-18.2153593864121,-12.5342935179843));
#83118=CARTESIAN_POINT('Ctrl Pts',(16.7240840285399,-18.2833414390349,-12.5299818113365));
#83119=CARTESIAN_POINT('Ctrl Pts',(16.7037024934055,-18.3523492393766,-12.5256701046887));
#83120=CARTESIAN_POINT('Ctrl Pts',(16.6833204782339,-18.4213586650285,-12.5213582964892));
#83121=CARTESIAN_POINT('Ctrl Pts',(16.6664655033666,-18.4913934058167,-12.5170464882897));
#83122=CARTESIAN_POINT('Ctrl Pts',(16.6532233605848,-18.5620543924288,-12.5127346800901));
#83123=CARTESIAN_POINT('Ctrl Pts',(16.639966456221,-18.6327941478605,-12.5084180653339));
#83124=CARTESIAN_POINT('Ctrl Pts',(16.6303305065811,-18.7041610510436,-12.5041014505776));
#83125=CARTESIAN_POINT('Ctrl Pts',(16.6243497245845,-18.7757481477001,-12.4997848358213));
#83126=CARTESIAN_POINT('Ctrl Pts',(16.6193948377084,-18.8350557710035,-12.4962086583554));
#83127=CARTESIAN_POINT('Ctrl Pts',(16.6169477636251,-18.8945142745606,-12.4926324808895));
#83128=CARTESIAN_POINT('Ctrl Pts',(16.6170008459317,-18.9538925311169,-12.4890563034236));
#83129=CARTESIAN_POINT('Ctrl Pts',(16.6163526597653,-18.9538935158516,-12.4890562790225));
#83130=CARTESIAN_POINT('Ctrl Pts',(16.6150299521963,-19.0968822256806,-12.4804472042752));
#83131=CARTESIAN_POINT('Ctrl Pts',(16.6379358826496,-19.3437931578393,-12.4655558028313));
#83132=CARTESIAN_POINT('Ctrl Pts',(16.7071054598744,-19.5811888020602,-12.4506644013873));
#83133=CARTESIAN_POINT('Ctrl Pts',(16.7437496527793,-19.6787359237804,-12.4443820746906));
#83134=CARTESIAN_POINT('Origin',(18.734,-18.952,0.));
#83135=CARTESIAN_POINT('',(16.7454194494007,-19.678110455632,-11.6425492951846));
#83136=CARTESIAN_POINT('',(16.7454194500115,-19.678110457305,-11.8674650116542));
#83137=CARTESIAN_POINT('',(16.7454194499637,-19.6781104571739,0.));
#83138=CARTESIAN_POINT('',(16.6170006007775,-18.9504051045321,-11.9120634828057));
#83139=CARTESIAN_POINT('Ctrl Pts',(16.7454194500115,-19.678110457305,-11.8674650116542));
#83140=CARTESIAN_POINT('Ctrl Pts',(16.7321284699056,-19.6417107824854,-11.8699797021076));
#83141=CARTESIAN_POINT('Ctrl Pts',(16.7198387408441,-19.6049512409371,-11.8724726322167));
#83142=CARTESIAN_POINT('Ctrl Pts',(16.705693847586,-19.5584326133417,-11.8755657202205));
#83143=CARTESIAN_POINT('Ctrl Pts',(16.7028892951475,-19.548972086202,-11.8761916170213));
#83144=CARTESIAN_POINT('Ctrl Pts',(16.684621334253,-19.4857299258936,-11.8803545370693));
#83145=CARTESIAN_POINT('Ctrl Pts',(16.6712284886434,-19.4313695483551,-11.8838303862752));
#83146=CARTESIAN_POINT('Ctrl Pts',(16.6575927142468,-19.3647547060886,-11.8879694847778));
#83147=CARTESIAN_POINT('Ctrl Pts',(16.655281149068,-19.3529508846168,-11.8886984191902));
#83148=CARTESIAN_POINT('Ctrl Pts',(16.6516247940173,-19.3333978798055,-11.889898626918));
#83149=CARTESIAN_POINT('Ctrl Pts',(16.6502223868832,-19.3256598759411,-11.8903717274574));
#83150=CARTESIAN_POINT('Ctrl Pts',(16.6477625561846,-19.3116426982719,-11.8912254000915));
#83151=CARTESIAN_POINT('Ctrl Pts',(16.6466902882239,-19.3053662560213,-11.8916064401833));
#83152=CARTESIAN_POINT('Ctrl Pts',(16.6446635443308,-19.2931716702623,-11.8923444618685));
#83153=CARTESIAN_POINT('Ctrl Pts',(16.6437058571057,-19.2872541288255,-11.8927015420183));
#83154=CARTESIAN_POINT('Ctrl Pts',(16.6416603283115,-19.2742652384781,-11.8934830566531));
#83155=CARTESIAN_POINT('Ctrl Pts',(16.6405831698579,-19.2671922632905,-11.8939071501069));
#83156=CARTESIAN_POINT('Ctrl Pts',(16.6380228005234,-19.2497877047711,-11.8949471799295));
#83157=CARTESIAN_POINT('Ctrl Pts',(16.6365800904223,-19.2394502853674,-11.8955618403836));
#83158=CARTESIAN_POINT('Ctrl Pts',(16.6230153964929,-19.136710708443,-11.9016413870128));
#83159=CARTESIAN_POINT('Ctrl Pts',(16.6169303820547,-19.043610582272,-11.9069087499733));
#83160=CARTESIAN_POINT('Ctrl Pts',(16.6170006007775,-18.9504051045321,-11.9120634828057));
#83161=CARTESIAN_POINT('Ctrl Pts',(16.6170005988957,-18.9504076043165,-11.912063344555));
#83162=CARTESIAN_POINT('Ctrl Pts',(16.6171142130127,-18.7993641041209,-11.9204168148733));
#83163=CARTESIAN_POINT('Ctrl Pts',(16.6333918366525,-18.6487693419506,-11.9284162966799));
#83164=CARTESIAN_POINT('Ctrl Pts',(16.6785865590018,-18.4414036071667,-11.9402353573198));
#83165=CARTESIAN_POINT('Ctrl Pts',(16.6942013609097,-18.3822165259633,-11.9437094928887));
#83166=CARTESIAN_POINT('Ctrl Pts',(16.7161304297539,-18.3116460075593,-11.9480644897593));
#83167=CARTESIAN_POINT('Ctrl Pts',(16.7200147926183,-18.2995320660581,-11.9488197826088));
#83168=CARTESIAN_POINT('Ctrl Pts',(16.725627212657,-18.2825566830156,-11.9498900318538));
#83169=CARTESIAN_POINT('Ctrl Pts',(16.7272643113937,-18.2776651555869,-11.9501998191164));
#83170=CARTESIAN_POINT('Ctrl Pts',(16.7300928755629,-18.2693151405452,-11.9507310945633));
#83171=CARTESIAN_POINT('Ctrl Pts',(16.7312754716076,-18.26585362795,-11.9509520600016));
#83172=CARTESIAN_POINT('Ctrl Pts',(16.7335672004791,-18.259202034274,-11.9513780874896));
#83173=CARTESIAN_POINT('Ctrl Pts',(16.7346750010501,-18.2560115267365,-11.951583065312));
#83174=CARTESIAN_POINT('Ctrl Pts',(16.7376455275145,-18.2475219161551,-11.9521301409547));
#83175=CARTESIAN_POINT('Ctrl Pts',(16.7395217014979,-18.2422275959306,-11.9524730262259));
#83176=CARTESIAN_POINT('Ctrl Pts',(16.7463383467246,-18.2232323576625,-11.9537092606304));
#83177=CARTESIAN_POINT('Ctrl Pts',(16.7513989781569,-18.2095754005923,-11.9546093395308));
#83178=CARTESIAN_POINT('Ctrl Pts',(16.8132024685467,-18.0479276115216,-11.9653881411684));
#83179=CARTESIAN_POINT('Ctrl Pts',(16.8862469759508,-17.9067188523124,-11.976016176932));
#83180=CARTESIAN_POINT('Ctrl Pts',(17.0125880598064,-17.7178369517081,-11.9909701619109));
#83181=CARTESIAN_POINT('Ctrl Pts',(17.0535836430284,-17.6625739634773,-11.9954558897231));
#83182=CARTESIAN_POINT('Ctrl Pts',(17.1293346621576,-17.5702237030643,-12.0031050472166));
#83183=CARTESIAN_POINT('Ctrl Pts',(17.1628683974291,-17.532210326528,-12.0063038104558));
#83184=CARTESIAN_POINT('Ctrl Pts',(17.2125182539898,-17.4798438011907,-12.0107814371134));
#83185=CARTESIAN_POINT('Ctrl Pts',(17.2275370702007,-17.4644785476137,-12.0121046145792));
#83186=CARTESIAN_POINT('Ctrl Pts',(17.2544659617231,-17.4377547334978,-12.0144231779045));
#83187=CARTESIAN_POINT('Ctrl Pts',(17.2662792517708,-17.4263016265491,-12.0154226706571));
#83188=CARTESIAN_POINT('Ctrl Pts',(17.2841042396734,-17.4094187687792,-12.0169051143085));
#83189=CARTESIAN_POINT('Ctrl Pts',(17.2900153133673,-17.4038841134003,-12.0173925967246));
#83190=CARTESIAN_POINT('Ctrl Pts',(17.3006606305797,-17.3940307087213,-12.0182632244455));
#83191=CARTESIAN_POINT('Ctrl Pts',(17.3053829764859,-17.3896993048638,-12.018646908923));
#83192=CARTESIAN_POINT('Ctrl Pts',(17.3146944928213,-17.3812361708287,-12.0193985407608));
#83193=CARTESIAN_POINT('Ctrl Pts',(17.3192822152422,-17.3771029492464,-12.0197665493077));
#83194=CARTESIAN_POINT('Ctrl Pts',(17.3318231016589,-17.3659034935425,-12.0207662977765));
#83195=CARTESIAN_POINT('Ctrl Pts',(17.3398116206925,-17.3588769817433,-12.0213963690959));
#83196=CARTESIAN_POINT('Ctrl Pts',(17.3705138519407,-17.3322798321615,-12.0237926510791));
#83197=CARTESIAN_POINT('Ctrl Pts',(17.3935900721898,-17.3131317148734,-12.0255414533878));
#83198=CARTESIAN_POINT('Ctrl Pts',(17.4221564830299,-17.2904351184303,-12.0276474036579));
#83199=CARTESIAN_POINT('Ctrl Pts',(17.4272654717086,-17.2864141743747,-12.0280218100182));
#83200=CARTESIAN_POINT('Ctrl Pts',(17.5660775382317,-17.178196287701,-12.0381351746127));
#83201=CARTESIAN_POINT('Ctrl Pts',(17.7117917382368,-17.0904101355843,-12.0472020282944));
#83202=CARTESIAN_POINT('Ctrl Pts',(17.9387511016617,-16.9884432036371,-12.0607697065465));
#83203=CARTESIAN_POINT('Ctrl Pts',(18.0128412415804,-16.9600401139217,-12.0651327156219));
#83204=CARTESIAN_POINT('Ctrl Pts',(18.1224372702966,-16.9249426107655,-12.0717169269656));
#83205=CARTESIAN_POINT('Ctrl Pts',(18.1568007474809,-16.9148914334043,-12.0737996388527));
#83206=CARTESIAN_POINT('Ctrl Pts',(18.1986034450125,-16.9038068780349,-12.0763734115849));
#83207=CARTESIAN_POINT('Ctrl Pts',(18.2058166669621,-16.901934903738,-12.0768189588341));
#83208=CARTESIAN_POINT('Ctrl Pts',(18.2170679587025,-16.899078291979,-12.0775163727656));
#83209=CARTESIAN_POINT('Ctrl Pts',(18.2210993807744,-16.8980673748393,-12.0777667485368));
#83210=CARTESIAN_POINT('Ctrl Pts',(18.2285953757885,-16.8962111286051,-12.0782332440898));
#83211=CARTESIAN_POINT('Ctrl Pts',(18.2320591170933,-16.8953626796677,-12.0784491813962));
#83212=CARTESIAN_POINT('Ctrl Pts',(18.2399127524657,-16.8934599410253,-12.0789396480693));
#83213=CARTESIAN_POINT('Ctrl Pts',(18.2443038634695,-16.8924109449763,-12.0792144763959));
#83214=CARTESIAN_POINT('Ctrl Pts',(18.2556574693868,-16.8897370341274,-12.0799265564264));
#83215=CARTESIAN_POINT('Ctrl Pts',(18.2626248351889,-16.8881333454716,-12.0803649808801));
#83216=CARTESIAN_POINT('Ctrl Pts',(18.3056159411292,-16.87846706869,-12.0830785254479));
#83217=CARTESIAN_POINT('Ctrl Pts',(18.3418350182682,-16.8713131024546,-12.0854004639583));
#83218=CARTESIAN_POINT('Ctrl Pts',(18.546300494839,-16.8364551336416,-12.0986400980833));
#83219=CARTESIAN_POINT('Ctrl Pts',(18.7172256339539,-16.8282102320616,-12.1101449892438));
#83220=CARTESIAN_POINT('Ctrl Pts',(18.9821998790576,-16.8474476453823,-12.1274081236477));
#83221=CARTESIAN_POINT('Ctrl Pts',(19.0765437542806,-16.8607296223075,-12.1334532439658));
#83222=CARTESIAN_POINT('Ctrl Pts',(19.1905921974845,-16.8847145815008,-12.1406117801762));
#83223=CARTESIAN_POINT('Ctrl Pts',(19.2114320464133,-16.8894277879518,-12.1419139966346));
#83224=CARTESIAN_POINT('Ctrl Pts',(19.2409498845181,-16.8965750054515,-12.1437507242227));
#83225=CARTESIAN_POINT('Ctrl Pts',(19.2496886666514,-16.8987500647432,-12.1442935200281));
#83226=CARTESIAN_POINT('Ctrl Pts',(19.2647355391844,-16.9025973139173,-12.145226534528));
#83227=CARTESIAN_POINT('Ctrl Pts',(19.2710502136786,-16.9042430193638,-12.1456176025372));
#83228=CARTESIAN_POINT('Ctrl Pts',(19.2831230418729,-16.9074490776931,-12.1463643757414));
#83229=CARTESIAN_POINT('Ctrl Pts',(19.2888823973331,-16.9090046218179,-12.1467202324011));
#83230=CARTESIAN_POINT('Ctrl Pts',(19.3038343433411,-16.9131108835994,-12.1476430979305));
#83231=CARTESIAN_POINT('Ctrl Pts',(19.313016470345,-16.9156994476686,-12.1482088732589));
#83232=CARTESIAN_POINT('Ctrl Pts',(19.3442298136422,-16.9247271036667,-12.1501291029125));
#83233=CARTESIAN_POINT('Ctrl Pts',(19.366174156515,-16.9314625175157,-12.151473904434));
#83234=CARTESIAN_POINT('Ctrl Pts',(19.5553830930014,-16.99292114255,-12.1630344564364));
#83235=CARTESIAN_POINT('Ctrl Pts',(19.7153269906489,-17.0679447543458,-12.1724942695172));
#83236=CARTESIAN_POINT('Ctrl Pts',(19.9374236258115,-17.2081626030476,-12.1867867608847));
#83237=CARTESIAN_POINT('Ctrl Pts',(20.0077788230461,-17.2588719996558,-12.1915315574814));
#83238=CARTESIAN_POINT('Ctrl Pts',(20.1040235862784,-17.3376431034679,-12.1986330642438));
#83239=CARTESIAN_POINT('Ctrl Pts',(20.1325777323996,-17.3623167780314,-12.200825045838));
#83240=CARTESIAN_POINT('Ctrl Pts',(20.166046291059,-17.3928368676148,-12.203519995948));
#83241=CARTESIAN_POINT('Ctrl Pts',(20.1716098033111,-17.3979651539841,-12.2039722950571));
#83242=CARTESIAN_POINT('Ctrl Pts',(20.180204699436,-17.405973334838,-12.2046779931552));
#83243=CARTESIAN_POINT('Ctrl Pts',(20.1832553092452,-17.408832630596,-12.2049298433318));
#83244=CARTESIAN_POINT('Ctrl Pts',(20.1888904274041,-17.4141457983619,-12.2053976622854));
#83245=CARTESIAN_POINT('Ctrl Pts',(20.1914772173847,-17.416597166386,-12.2056134395859));
#83246=CARTESIAN_POINT('Ctrl Pts',(20.1973029608044,-17.4221459124098,-12.2061017116667));
#83247=CARTESIAN_POINT('Ctrl Pts',(20.2005382573396,-17.4252470326474,-12.2063744939988));
#83248=CARTESIAN_POINT('Ctrl Pts',(20.2100341785665,-17.4344071655437,-12.2071798626863));
#83249=CARTESIAN_POINT('Ctrl Pts',(20.2162671857352,-17.4404944950187,-12.2077145813135));
#83250=CARTESIAN_POINT('Ctrl Pts',(20.2603081210546,-17.4840404918751,-12.2115351001895));
#83251=CARTESIAN_POINT('Ctrl Pts',(20.2967260186452,-17.5228716087308,-12.2149175238978));
#83252=CARTESIAN_POINT('Ctrl Pts',(20.3436243467728,-17.5768155874372,-12.2195368360917));
#83253=CARTESIAN_POINT('Ctrl Pts',(20.3554306175602,-17.5907559249953,-12.2207238628777));
#83254=CARTESIAN_POINT('Ctrl Pts',(20.3976007705015,-17.6418757082568,-12.2250479487909));
#83255=CARTESIAN_POINT('Ctrl Pts',(20.426877799154,-17.6799317190139,-12.2282124605792));
#83256=CARTESIAN_POINT('Ctrl Pts',(20.5185421579863,-17.8078576836956,-12.2386083352236));
#83257=CARTESIAN_POINT('Ctrl Pts',(20.5752678670104,-17.9015770083348,-12.245840722962));
#83258=CARTESIAN_POINT('Ctrl Pts',(20.6492938150994,-18.0484658175535,-12.2564135071761));
#83259=CARTESIAN_POINT('Ctrl Pts',(20.6721600232126,-18.0986179271779,-12.2599022836881));
#83260=CARTESIAN_POINT('Ctrl Pts',(20.7060456980323,-18.1813500792953,-12.2654593465495));
#83261=CARTESIAN_POINT('Ctrl Pts',(20.7182736332477,-18.2134041023121,-12.2675660629028));
#83262=CARTESIAN_POINT('Ctrl Pts',(20.7333235416322,-18.2559316183104,-12.2703024289393));
#83263=CARTESIAN_POINT('Ctrl Pts',(20.736851244059,-18.2661481814058,-12.2709554164735));
#83264=CARTESIAN_POINT('Ctrl Pts',(20.7425019779367,-18.2829287135742,-12.2720208956252));
#83265=CARTESIAN_POINT('Ctrl Pts',(20.7446714096475,-18.2894767431454,-12.2724349165719));
#83266=CARTESIAN_POINT('Ctrl Pts',(20.7488094835661,-18.3021743043541,-12.2732344294919));
#83267=CARTESIAN_POINT('Ctrl Pts',(20.7507820698173,-18.3083224611045,-12.2736200477828));
#83268=CARTESIAN_POINT('Ctrl Pts',(20.7552726157238,-18.3225419026711,-12.2745084783195));
#83269=CARTESIAN_POINT('Ctrl Pts',(20.7577704237983,-18.33061947384,-12.2750106244516));
#83270=CARTESIAN_POINT('Ctrl Pts',(20.7643596515241,-18.3523893782569,-12.2763572728471));
#83271=CARTESIAN_POINT('Ctrl Pts',(20.7683609784959,-18.366108682152,-12.2771988334378));
#83272=CARTESIAN_POINT('Ctrl Pts',(20.803809115014,-18.4923927836866,-12.2848829072953));
#83273=CARTESIAN_POINT('Ctrl Pts',(20.8260248908665,-18.6073470023685,-12.2914085157882));
#83274=CARTESIAN_POINT('Ctrl Pts',(20.8562170107502,-18.885511157645,-12.3067257190411));
#83275=CARTESIAN_POINT('Ctrl Pts',(20.855041894869,-19.0489286551452,-12.3153337760523));
#83276=CARTESIAN_POINT('Ctrl Pts',(20.8312013426985,-19.2426549725124,-12.3265434425329));
#83277=CARTESIAN_POINT('Ctrl Pts',(20.8265193606268,-19.2746395096073,-12.3284289516276));
#83278=CARTESIAN_POINT('Ctrl Pts',(20.8198971723483,-19.3136271763478,-12.3307836283437));
#83279=CARTESIAN_POINT('Ctrl Pts',(20.8186505332077,-19.3207456837112,-12.3312158647962));
#83280=CARTESIAN_POINT('Ctrl Pts',(20.8166383401881,-19.3318992111781,-12.3318969324655));
#83281=CARTESIAN_POINT('Ctrl Pts',(20.8158974373662,-19.3359387012328,-12.3321443840855));
#83282=CARTESIAN_POINT('Ctrl Pts',(20.8144900990948,-19.3434878149372,-12.3326083465005));
#83283=CARTESIAN_POINT('Ctrl Pts',(20.813826532938,-19.3469979163289,-12.3328246929655));
#83284=CARTESIAN_POINT('Ctrl Pts',(20.8122908633305,-19.3550100698432,-12.3333199291672));
#83285=CARTESIAN_POINT('Ctrl Pts',(20.8114130169764,-19.3595109630199,-12.3335991422247));
#83286=CARTESIAN_POINT('Ctrl Pts',(20.8086674370288,-19.3733486567015,-12.3344605977594));
#83287=CARTESIAN_POINT('Ctrl Pts',(20.8067513590226,-19.3826755863278,-12.3350454933105));
#83288=CARTESIAN_POINT('Ctrl Pts',(20.7886241521695,-19.4679897984925,-12.3404326124482));
#83289=CARTESIAN_POINT('Ctrl Pts',(20.7683057282506,-19.5430358612127,-12.3454391348783));
#83290=CARTESIAN_POINT('Ctrl Pts',(20.7421027582796,-19.6222578030818,-12.3509004679087));
#83291=CARTESIAN_POINT('Ctrl Pts',(20.7402707671355,-19.6277217021486,-12.3512780632711));
#83292=CARTESIAN_POINT('Ctrl Pts',(20.6967115457058,-19.7558979180641,-12.3601569558555));
#83293=CARTESIAN_POINT('Ctrl Pts',(20.643820775992,-19.8745382004949,-12.3688045984896));
#83294=CARTESIAN_POINT('Ctrl Pts',(20.5373315123358,-20.0644025179968,-12.3828981078083));
#83295=CARTESIAN_POINT('Ctrl Pts',(20.4894988782859,-20.1384531113537,-12.388473695247));
#83296=CARTESIAN_POINT('Ctrl Pts',(20.4250114412864,-20.2258090596826,-12.3951372191672));
#83297=CARTESIAN_POINT('Ctrl Pts',(20.4125974797899,-20.2421239329334,-12.3963859637133));
#83298=CARTESIAN_POINT('Ctrl Pts',(20.3944831927711,-20.2652261840257,-12.3981608992562));
#83299=CARTESIAN_POINT('Ctrl Pts',(20.3889744822571,-20.2721616986906,-12.3986946352222));
#83300=CARTESIAN_POINT('Ctrl Pts',(20.3793483276385,-20.2841261647521,-12.3996169958875));
#83301=CARTESIAN_POINT('Ctrl Pts',(20.3752509819665,-20.289171063752,-12.4000064188428));
#83302=CARTESIAN_POINT('Ctrl Pts',(20.3673274996418,-20.298835646141,-12.4007534494684));
#83303=CARTESIAN_POINT('Ctrl Pts',(20.3635048390014,-20.3034580865175,-12.4011111922957));
#83304=CARTESIAN_POINT('Ctrl Pts',(20.3534377956224,-20.3155265525876,-12.4020464236606));
#83305=CARTESIAN_POINT('Ctrl Pts',(20.3471616531898,-20.3229459941818,-12.4026226113669));
#83306=CARTESIAN_POINT('Ctrl Pts',(20.3251950817667,-20.3485544114356,-12.4046158938871));
#83307=CARTESIAN_POINT('Ctrl Pts',(20.3092459722625,-20.3665197801725,-12.4060223004146));
#83308=CARTESIAN_POINT('Ctrl Pts',(20.1927900405548,-20.4932847509891,-12.4160147034109));
#83309=CARTESIAN_POINT('Ctrl Pts',(20.0814139780325,-20.5915454622472,-12.4240913569344));
#83310=CARTESIAN_POINT('Ctrl Pts',(19.92306194943,-20.704127586379,-12.4346429237359));
#83311=CARTESIAN_POINT('Ctrl Pts',(19.8845798500898,-20.7296347508308,-12.4371469729059));
#83312=CARTESIAN_POINT('Ctrl Pts',(19.7845284304216,-20.7913412476687,-12.443577247717));
#83313=CARTESIAN_POINT('Ctrl Pts',(19.7219089482267,-20.8257183800168,-12.4475276267364));
#83314=CARTESIAN_POINT('Ctrl Pts',(19.6274684418929,-20.8715130524845,-12.4535471089138));
#83315=CARTESIAN_POINT('Ctrl Pts',(19.5969164200343,-20.8854402450819,-12.455503677789));
#83316=CARTESIAN_POINT('Ctrl Pts',(19.5593254338195,-20.901507727772,-12.4579373746384));
#83317=CARTESIAN_POINT('Ctrl Pts',(19.5525879556011,-20.9043463339668,-12.4583745854735));
#83318=CARTESIAN_POINT('Ctrl Pts',(19.5420260195811,-20.9087319618677,-12.459061764027));
#83319=CARTESIAN_POINT('Ctrl Pts',(19.5382114393127,-20.9103028313123,-12.4593103109883));
#83320=CARTESIAN_POINT('Ctrl Pts',(19.5310874965847,-20.9132121930863,-12.4597752071622));
#83321=CARTESIAN_POINT('Ctrl Pts',(19.5277793318029,-20.9145534681338,-12.4599913851981));
#83322=CARTESIAN_POINT('Ctrl Pts',(19.5202392216401,-20.9175883760441,-12.4604847658428));
#83323=CARTESIAN_POINT('Ctrl Pts',(19.5160052057855,-20.9192767052226,-12.4607622823588));
#83324=CARTESIAN_POINT('Ctrl Pts',(19.5049829143421,-20.9236306785164,-12.4614858839157));
#83325=CARTESIAN_POINT('Ctrl Pts',(19.4981863242547,-20.9262749162593,-12.4619332043162));
#83326=CARTESIAN_POINT('Ctrl Pts',(19.4548256337707,-20.9428871005031,-12.4647935735592));
#83327=CARTESIAN_POINT('Ctrl Pts',(19.4178962004824,-20.9558728953422,-12.4672592521349));
#83328=CARTESIAN_POINT('Ctrl Pts',(19.3688752846647,-20.9715976798468,-12.4705516760663));
#83329=CARTESIAN_POINT('Ctrl Pts',(19.3570870694893,-20.9752656544818,-12.4713448815229));
#83330=CARTESIAN_POINT('Ctrl Pts',(19.3221513106599,-20.9858018597544,-12.4736986988017));
#83331=CARTESIAN_POINT('Ctrl Pts',(19.2989179826717,-20.9923773130897,-12.4752679913389));
#83332=CARTESIAN_POINT('Ctrl Pts',(19.1362196285474,-21.0354320514022,-12.4862637369298));
#83333=CARTESIAN_POINT('Ctrl Pts',(18.9934448152859,-21.0579827098367,-12.4959108586062));
#83334=CARTESIAN_POINT('Ctrl Pts',(18.787768864821,-21.069219491202,-12.5092191102238));
#83335=CARTESIAN_POINT('Ctrl Pts',(18.7259288608117,-21.0698870253441,-12.5131507017069));
#83336=CARTESIAN_POINT('Ctrl Pts',(18.6269048272022,-21.0666176610075,-12.519324324455));
#83337=CARTESIAN_POINT('Ctrl Pts',(18.5897034246201,-21.0644052649368,-12.5216162715323));
#83338=CARTESIAN_POINT('Ctrl Pts',(18.5414838674283,-21.0602576991223,-12.5245533668829));
#83339=CARTESIAN_POINT('Ctrl Pts',(18.5303974160802,-21.0592159316148,-12.5252263474334));
#83340=CARTESIAN_POINT('Ctrl Pts',(18.5123855121962,-21.0573799179716,-12.526316098293));
#83341=CARTESIAN_POINT('Ctrl Pts',(18.5054549621993,-21.0566388639639,-12.526734534482));
#83342=CARTESIAN_POINT('Ctrl Pts',(18.4921372980245,-21.0551483038057,-12.5275369584271));
#83343=CARTESIAN_POINT('Ctrl Pts',(18.4857497015159,-21.0544038967618,-12.5279211021013));
#83344=CARTESIAN_POINT('Ctrl Pts',(18.4711367121289,-21.052633380565,-12.5287982954899));
#83345=CARTESIAN_POINT('Ctrl Pts',(18.4629137220155,-21.0515880406703,-12.5292907332649));
#83346=CARTESIAN_POINT('Ctrl Pts',(18.4410945126435,-21.0486839725328,-12.53059438916));
#83347=CARTESIAN_POINT('Ctrl Pts',(18.4275097253491,-21.0467412799608,-12.5314029555338));
#83348=CARTESIAN_POINT('Ctrl Pts',(18.3247120750064,-21.0310192586882,-12.5374997932277));
#83349=CARTESIAN_POINT('Ctrl Pts',(18.2364379676942,-21.0116777835986,-12.5426055755362));
#83350=CARTESIAN_POINT('Ctrl Pts',(18.0155892361036,-20.9482545548448,-12.555325549663));
#83351=CARTESIAN_POINT('Ctrl Pts',(17.885658518111,-20.8965979403468,-12.5627450119146));
#83352=CARTESIAN_POINT('Ctrl Pts',(17.7126395596302,-20.8071466337983,-12.5735037478294));
#83353=CARTESIAN_POINT('Ctrl Pts',(17.6645406130502,-20.7798407894458,-12.5766018537881));
#83354=CARTESIAN_POINT('Ctrl Pts',(17.5933680194416,-20.73566449179,-12.5814337385233));
#83355=CARTESIAN_POINT('Ctrl Pts',(17.5694739215502,-20.7201569972724,-12.5831003841649));
#83356=CARTESIAN_POINT('Ctrl Pts',(17.5401543117035,-20.7002762041451,-12.5852110044489));
#83357=CARTESIAN_POINT('Ctrl Pts',(17.5344266223332,-20.6963511464121,-12.5856264965314));
#83358=CARTESIAN_POINT('Ctrl Pts',(17.5253935809179,-20.690095475009,-12.5862869789817));
#83359=CARTESIAN_POINT('Ctrl Pts',(17.5220753621259,-20.6877834046841,-12.586530724476));
#83360=CARTESIAN_POINT('Ctrl Pts',(17.5158296039964,-20.6834048421044,-12.5869916797798));
#83361=CARTESIAN_POINT('Ctrl Pts',(17.5129006790311,-20.6813404200953,-12.587208748946));
#83362=CARTESIAN_POINT('Ctrl Pts',(17.5062161289511,-20.6766034365492,-12.5877062175575));
#83363=CARTESIAN_POINT('Ctrl Pts',(17.5024639863758,-20.6739260418452,-12.5879869464144));
#83364=CARTESIAN_POINT('Ctrl Pts',(17.4925254501348,-20.6667851575629,-12.5887344346488));
#83365=CARTESIAN_POINT('Ctrl Pts',(17.4863544531645,-20.6623004940654,-12.5892025991234));
#83366=CARTESIAN_POINT('Ctrl Pts',(17.4432974653334,-20.6306525525968,-12.5924967344648));
#83367=CARTESIAN_POINT('Ctrl Pts',(17.4072802149826,-20.6023337083128,-12.595394769147));
#83368=CARTESIAN_POINT('Ctrl Pts',(17.3434298627298,-20.5486893666001,-12.6007562033481));
#83369=CARTESIAN_POINT('Ctrl Pts',(17.3152972309215,-20.5237456750931,-12.6032035622074));
#83370=CARTESIAN_POINT('Ctrl Pts',(17.1921807401655,-20.4085853896196,-12.6142536775164));
#83371=CARTESIAN_POINT('Ctrl Pts',(17.1050207763708,-20.3104101007053,-12.6229968788456));
#83372=CARTESIAN_POINT('Ctrl Pts',(16.9752027140399,-20.1335790198954,-12.6372013472694));
#83373=CARTESIAN_POINT('Ctrl Pts',(16.9274171686245,-20.0591399059462,-12.6427967463797));
#83374=CARTESIAN_POINT('Ctrl Pts',(16.8744284137836,-19.9639803676304,-12.6494812540878));
#83375=CARTESIAN_POINT('Ctrl Pts',(16.8646987212428,-19.9458931152881,-12.6507323074442));
#83376=CARTESIAN_POINT('Ctrl Pts',(16.8511486113747,-19.9198007064132,-12.6525099172039));
#83377=CARTESIAN_POINT('Ctrl Pts',(16.8471131304768,-19.9119091125399,-12.6530440498365));
#83378=CARTESIAN_POINT('Ctrl Pts',(16.8402042038597,-19.8981864167954,-12.6539668755691));
#83379=CARTESIAN_POINT('Ctrl Pts',(16.8373078570708,-19.8923670396287,-12.6543563691484));
#83380=CARTESIAN_POINT('Ctrl Pts',(16.8317911218727,-19.881153563582,-12.6551033824457));
#83381=CARTESIAN_POINT('Ctrl Pts',(16.8291667639058,-19.8757614976569,-12.6554610380493));
#83382=CARTESIAN_POINT('Ctrl Pts',(16.8223533114919,-19.8616099239209,-12.6563957027042));
#83383=CARTESIAN_POINT('Ctrl Pts',(16.818201475293,-19.8528325554072,-12.6569714140286));
#83384=CARTESIAN_POINT('Ctrl Pts',(16.8040088662289,-19.8222861123193,-12.6589613888741));
#83385=CARTESIAN_POINT('Ctrl Pts',(16.7942773404032,-19.8003747794809,-12.6603650119482));
#83386=CARTESIAN_POINT('Ctrl Pts',(16.7708981679383,-19.7452280274813,-12.6638421844087));
#83387=CARTESIAN_POINT('Ctrl Pts',(16.7577281088485,-19.7118198611918,-12.6658990953057));
#83388=CARTESIAN_POINT('Ctrl Pts',(16.7454195349593,-19.6781106899492,-12.6679318731853));
#83389=CARTESIAN_POINT('',(16.6141771461173,-18.9509225630941,-11.6890562790225));
#83390=CARTESIAN_POINT('Ctrl Pts',(16.7437496527793,-19.6787359237804,-12.4443820746906));
#83391=CARTESIAN_POINT('Ctrl Pts',(16.9543734450167,-20.2394180692954,-12.4082724658268));
#83392=CARTESIAN_POINT('Ctrl Pts',(17.9482901965323,-21.2712729007906,-12.3297709214024));
#83393=CARTESIAN_POINT('Ctrl Pts',(20.2082246479652,-20.9751142883798,-12.2088774414178));
#83394=CARTESIAN_POINT('Ctrl Pts',(21.2330887928116,-18.8074837650725,-12.0817016347363));
#83395=CARTESIAN_POINT('Ctrl Pts',(19.9651940811972,-16.7724379176221,-11.9545258280548));
#83396=CARTESIAN_POINT('Ctrl Pts',(17.5677552166072,-16.7370050018739,-11.8273500213735));
#83397=CARTESIAN_POINT('Ctrl Pts',(16.6440838383059,-18.1263146735576,-11.7388601716959));
#83398=CARTESIAN_POINT('Ctrl Pts',(16.6137960417384,-18.8895339291486,-11.692762257579));
#83399=CARTESIAN_POINT('Ctrl Pts',(16.6141771461173,-18.9509225630941,-11.6890562790225));
#83400=CARTESIAN_POINT('Ctrl Pts',(16.6170002227512,-18.951028851869,-11.6906772973237));
#83401=CARTESIAN_POINT('Ctrl Pts',(16.6169204646911,-19.1248929515366,-11.6794936821839));
#83402=CARTESIAN_POINT('Ctrl Pts',(16.6382580402862,-19.2981155640509,-11.66776312738));
#83403=CARTESIAN_POINT('Ctrl Pts',(16.6953875256918,-19.5259976394338,-11.6525929584797));
#83404=CARTESIAN_POINT('Ctrl Pts',(16.7127834335452,-19.5845336305672,-11.648712703421));
#83405=CARTESIAN_POINT('Ctrl Pts',(16.7368231144309,-19.6542353438915,-11.6441197397871));
#83406=CARTESIAN_POINT('Ctrl Pts',(16.7410677156335,-19.666192471166,-11.6433327722891));
#83407=CARTESIAN_POINT('Ctrl Pts',(16.7454194494007,-19.678110455632,-11.6425492951846));
#83408=CARTESIAN_POINT('Origin',(18.734,-18.952,0.));
#83409=CARTESIAN_POINT('',(16.7454194496957,-19.67811045644,-10.8441190240937));
#83410=CARTESIAN_POINT('',(16.745419450227,-19.678110457895,-11.0644158965713));
#83411=CARTESIAN_POINT('',(16.7454194499637,-19.6781104571739,0.));
#83412=CARTESIAN_POINT('Ctrl Pts',(16.745419450227,-19.678110457895,-11.0644158965713));
#83413=CARTESIAN_POINT('Ctrl Pts',(16.7100155218545,-19.581150604774,-11.0708124074204));
#83414=CARTESIAN_POINT('Ctrl Pts',(16.6817531145212,-19.4817385259306,-11.0775606813504));
#83415=CARTESIAN_POINT('Ctrl Pts',(16.6317924848945,-19.2401187266275,-11.0938351403994));
#83416=CARTESIAN_POINT('Ctrl Pts',(16.6170952308914,-19.0969558973671,-11.1033537401525));
#83417=CARTESIAN_POINT('Ctrl Pts',(16.6169595358669,-18.8914033897129,-11.1164063607099));
#83418=CARTESIAN_POINT('Ctrl Pts',(16.6196417425704,-18.8294329463025,-11.1202674028607));
#83419=CARTESIAN_POINT('Ctrl Pts',(16.626121995978,-18.755293290851,-11.1248001906107));
#83420=CARTESIAN_POINT('Ctrl Pts',(16.6273121369964,-18.7429319071468,-11.125553102198));
#83421=CARTESIAN_POINT('Ctrl Pts',(16.629446086491,-18.7226409476578,-11.126784473422));
#83422=CARTESIAN_POINT('Ctrl Pts',(16.6303260988315,-18.7147050990314,-11.12726492884));
#83423=CARTESIAN_POINT('Ctrl Pts',(16.6319896971568,-18.7004401578214,-11.1281265731885));
#83424=CARTESIAN_POINT('Ctrl Pts',(16.6327570212934,-18.6941092997592,-11.1285082696425));
#83425=CARTESIAN_POINT('Ctrl Pts',(16.6344530088088,-18.6806267538166,-11.1293196853172));
#83426=CARTESIAN_POINT('Ctrl Pts',(16.6353896346168,-18.6734761352318,-11.1297491481872));
#83427=CARTESIAN_POINT('Ctrl Pts',(16.6380125558554,-18.6542163446122,-11.1309035864619));
#83428=CARTESIAN_POINT('Ctrl Pts',(16.6397672552717,-18.6421166480973,-11.1316263951854));
#83429=CARTESIAN_POINT('Ctrl Pts',(16.6490971421965,-18.5814843962378,-11.1352369299879));
#83430=CARTESIAN_POINT('Ctrl Pts',(16.6582553372663,-18.5332084216257,-11.1380741371182));
#83431=CARTESIAN_POINT('Ctrl Pts',(16.6895710826044,-18.3946543047097,-11.1461497795195));
#83432=CARTESIAN_POINT('Ctrl Pts',(16.7160033266981,-18.30545898715,-11.1512603837602));
#83433=CARTESIAN_POINT('Ctrl Pts',(16.8056500674886,-18.0628317947687,-11.1653489073645));
#83434=CARTESIAN_POINT('Ctrl Pts',(16.8811330566578,-17.9146858719793,-11.1741493553049));
#83435=CARTESIAN_POINT('Ctrl Pts',(16.9808578003806,-17.7652494132739,-11.1847107322291));
#83436=CARTESIAN_POINT('Ctrl Pts',(16.9887344573945,-17.7536959110232,-11.185539392666));
#83437=CARTESIAN_POINT('Ctrl Pts',(16.9998805495105,-17.7376898139786,-11.186705694803));
#83438=CARTESIAN_POINT('Ctrl Pts',(17.0030540299258,-17.733170420623,-11.1870370642763));
#83439=CARTESIAN_POINT('Ctrl Pts',(17.0081863112416,-17.7259219452459,-11.1875719448114));
#83440=CARTESIAN_POINT('Ctrl Pts',(17.0101340136098,-17.7231849833039,-11.1877746979201));
#83441=CARTESIAN_POINT('Ctrl Pts',(17.0142251822704,-17.7174648363681,-11.1882001205937));
#83442=CARTESIAN_POINT('Ctrl Pts',(17.0163699008623,-17.7144825917355,-11.1884228794976));
#83443=CARTESIAN_POINT('Ctrl Pts',(17.0215923833771,-17.7072604270757,-11.1889646472359));
#83444=CARTESIAN_POINT('Ctrl Pts',(17.0246781354636,-17.703026336571,-11.1892842039935));
#83445=CARTESIAN_POINT('Ctrl Pts',(17.035608726877,-17.6881443901401,-11.1904140998444));
#83446=CARTESIAN_POINT('Ctrl Pts',(17.0435374121948,-17.6775588918596,-11.191229976263));
#83447=CARTESIAN_POINT('Ctrl Pts',(17.0915650943686,-17.6146744264093,-11.1961467226523));
#83448=CARTESIAN_POINT('Ctrl Pts',(17.1339858171065,-17.5642013661841,-11.2003844556965));
#83449=CARTESIAN_POINT('Ctrl Pts',(17.2439182099723,-17.4451520632016,-11.2109620933829));
#83450=CARTESIAN_POINT('Ctrl Pts',(17.3138862301183,-17.3790374597029,-11.2173577648922));
#83451=CARTESIAN_POINT('Ctrl Pts',(17.4967378723479,-17.2284345152286,-11.2329413052017));
#83452=CARTESIAN_POINT('Ctrl Pts',(17.6140381009902,-17.1500027268374,-11.2419898436872));
#83453=CARTESIAN_POINT('Ctrl Pts',(17.7508858952365,-17.0770653821329,-11.2514584928521));
#83454=CARTESIAN_POINT('Ctrl Pts',(17.7635632824206,-17.0704724936505,-11.252326423371));
#83455=CARTESIAN_POINT('Ctrl Pts',(17.783846444058,-17.0601837575227,-11.2537006737471));
#83456=CARTESIAN_POINT('Ctrl Pts',(17.791409118207,-17.0564043395359,-11.2542099212861));
#83457=CARTESIAN_POINT('Ctrl Pts',(17.804787123036,-17.049818589606,-11.2551052842454));
#83458=CARTESIAN_POINT('Ctrl Pts',(17.8105929943291,-17.0469933879183,-11.2554920557224));
#83459=CARTESIAN_POINT('Ctrl Pts',(17.8226282444429,-17.0412048493931,-11.2562901274364));
#83460=CARTESIAN_POINT('Ctrl Pts',(17.8288593707787,-17.0382453063481,-11.256701292256));
#83461=CARTESIAN_POINT('Ctrl Pts',(17.8448911760841,-17.0307266371575,-11.2577540305011));
#83462=CARTESIAN_POINT('Ctrl Pts',(17.8547125844484,-17.0262119839024,-11.2583940624616));
#83463=CARTESIAN_POINT('Ctrl Pts',(17.8958499793224,-17.0076824792482,-11.2610549526072));
#83464=CARTESIAN_POINT('Ctrl Pts',(17.9274707769542,-16.9943542486712,-11.2630522769814));
#83465=CARTESIAN_POINT('Ctrl Pts',(18.0106938754143,-16.9616345434039,-11.2681969743295));
#83466=CARTESIAN_POINT('Ctrl Pts',(18.0627550143649,-16.9434788486161,-11.2713049458654));
#83467=CARTESIAN_POINT('Ctrl Pts',(18.2200495552602,-16.8954247017299,-11.2804500761598));
#83468=CARTESIAN_POINT('Ctrl Pts',(18.3269519425295,-16.8716250869388,-11.2863385079318));
#83469=CARTESIAN_POINT('Ctrl Pts',(18.481091160126,-16.8496504561494,-11.2948153762593));
#83470=CARTESIAN_POINT('Ctrl Pts',(18.5271693679278,-16.8446183718685,-11.2973493544173));
#83471=CARTESIAN_POINT('Ctrl Pts',(18.5947046835901,-16.8394793624749,-11.3011064816897));
#83472=CARTESIAN_POINT('Ctrl Pts',(18.616058174059,-16.8381796878557,-11.3023007363443));
#83473=CARTESIAN_POINT('Ctrl Pts',(18.689228025621,-16.8348383636923,-11.3064251625996));
#83474=CARTESIAN_POINT('Ctrl Pts',(18.7410938586039,-16.8343771210788,-11.3094038306521));
#83475=CARTESIAN_POINT('Ctrl Pts',(18.8015714509149,-16.8360609618551,-11.3129946089349));
#83476=CARTESIAN_POINT('Ctrl Pts',(18.8102216668728,-16.8363549055115,-11.3135110167586));
#83477=CARTESIAN_POINT('Ctrl Pts',(18.8233353012831,-16.8368810487547,-11.314298477698));
#83478=CARTESIAN_POINT('Ctrl Pts',(18.8278003077781,-16.8370743570067,-11.3145674047013));
#83479=CARTESIAN_POINT('Ctrl Pts',(18.8358238711881,-16.8374471879692,-11.3150521684942));
#83480=CARTESIAN_POINT('Ctrl Pts',(18.8393826131848,-16.8376215570191,-11.3152677139316));
#83481=CARTESIAN_POINT('Ctrl Pts',(18.8471261343323,-16.8380205677217,-11.3157378982348));
#83482=CARTESIAN_POINT('Ctrl Pts',(18.851310637997,-16.838248648522,-11.3159927223016));
#83483=CARTESIAN_POINT('Ctrl Pts',(18.8630926444103,-16.8389259328327,-11.3167122498838));
#83484=CARTESIAN_POINT('Ctrl Pts',(18.8706883516572,-16.8394036791997,-11.3171785070507));
#83485=CARTESIAN_POINT('Ctrl Pts',(18.9167070206829,-16.8425473269248,-11.3200171271687));
#83486=CARTESIAN_POINT('Ctrl Pts',(18.9550513628164,-16.8462202633494,-11.3224405987897));
#83487=CARTESIAN_POINT('Ctrl Pts',(19.0823659376831,-16.8619308840319,-11.3306355105033));
#83488=CARTESIAN_POINT('Ctrl Pts',(19.1706657035548,-16.8785804052242,-11.336558067772));
#83489=CARTESIAN_POINT('Ctrl Pts',(19.4238492837337,-16.943213248176,-11.3538251334834));
#83490=CARTESIAN_POINT('Ctrl Pts',(19.5843224133701,-17.0056983747675,-11.3650716078246));
#83491=CARTESIAN_POINT('Ctrl Pts',(19.7560025096065,-17.0978854440289,-11.3770690612865));
#83492=CARTESIAN_POINT('Ctrl Pts',(19.7763108052372,-17.1092254154925,-11.3784891007252));
#83493=CARTESIAN_POINT('Ctrl Pts',(19.8047237132041,-17.1257109485089,-11.38047776238));
#83494=CARTESIAN_POINT('Ctrl Pts',(19.8129859695544,-17.1305801549745,-11.3810562864926));
#83495=CARTESIAN_POINT('Ctrl Pts',(19.8263416371281,-17.1385738377566,-11.3819919211739));
#83496=CARTESIAN_POINT('Ctrl Pts',(19.8314553405053,-17.1416639884136,-11.3823502758451));
#83497=CARTESIAN_POINT('Ctrl Pts',(19.8421198935967,-17.1481702459721,-11.3830978859057));
#83498=CARTESIAN_POINT('Ctrl Pts',(19.8476681945754,-17.1515904260537,-11.3834869868843));
#83499=CARTESIAN_POINT('Ctrl Pts',(19.8608077281338,-17.159774104919,-11.384408870361));
#83500=CARTESIAN_POINT('Ctrl Pts',(19.8683847211791,-17.1645603161789,-11.384940808165));
#83501=CARTESIAN_POINT('Ctrl Pts',(19.8937059951239,-17.1807810409493,-11.3867197769175));
#83502=CARTESIAN_POINT('Ctrl Pts',(19.9113099570464,-17.1924330338004,-11.3879587111698));
#83503=CARTESIAN_POINT('Ctrl Pts',(20.0055405439043,-17.2568512942767,-11.3946073015226));
#83504=CARTESIAN_POINT('Ctrl Pts',(20.0788040825999,-17.3143647018779,-11.3998313584646));
#83505=CARTESIAN_POINT('Ctrl Pts',(20.2632223604968,-17.4798868380565,-11.4134779554991));
#83506=CARTESIAN_POINT('Ctrl Pts',(20.3667005746358,-17.5955632781556,-11.4216615554222));
#83507=CARTESIAN_POINT('Ctrl Pts',(20.4878034878973,-17.7650979442364,-11.4333758771198));
#83508=CARTESIAN_POINT('Ctrl Pts',(20.5172944170812,-17.8098865409465,-11.4364515234528));
#83509=CARTESIAN_POINT('Ctrl Pts',(20.5495766267374,-17.8632177062726,-11.4401508612578));
#83510=CARTESIAN_POINT('Ctrl Pts',(20.5540555868417,-17.8707215781585,-11.440672201567));
#83511=CARTESIAN_POINT('Ctrl Pts',(20.5607638284928,-17.8821200765634,-11.441465714825));
#83512=CARTESIAN_POINT('Ctrl Pts',(20.5630274603093,-17.8859945195991,-11.441735712348));
#83513=CARTESIAN_POINT('Ctrl Pts',(20.5670669568691,-17.8929592852595,-11.4422216125198));
#83514=CARTESIAN_POINT('Ctrl Pts',(20.5688473494059,-17.896046919637,-11.442437217712));
#83515=CARTESIAN_POINT('Ctrl Pts',(20.5726972193058,-17.9027626669011,-11.442906603626));
#83516=CARTESIAN_POINT('Ctrl Pts',(20.5747637321573,-17.9063923646366,-11.4431605644725));
#83517=CARTESIAN_POINT('Ctrl Pts',(20.5805337598745,-17.9165971691968,-11.4438752712907));
#83518=CARTESIAN_POINT('Ctrl Pts',(20.5842128351908,-17.9231859210976,-11.4443375384607));
#83519=CARTESIAN_POINT('Ctrl Pts',(20.6059073569254,-17.9625307639731,-11.4471021682087));
#83520=CARTESIAN_POINT('Ctrl Pts',(20.6230866320162,-17.995737576871,-11.4494526570944));
#83521=CARTESIAN_POINT('Ctrl Pts',(20.6765427211136,-18.1061339463082,-11.4572808214052));
#83522=CARTESIAN_POINT('Ctrl Pts',(20.7090346744814,-18.1850594753952,-11.462896260796));
#83523=CARTESIAN_POINT('Ctrl Pts',(20.7943566477514,-18.4340440717106,-11.480283677724));
#83524=CARTESIAN_POINT('Ctrl Pts',(20.830598246833,-18.6090013489265,-11.4919758281924));
#83525=CARTESIAN_POINT('Ctrl Pts',(20.846300249462,-18.8091838028158,-11.5043329499581));
#83526=CARTESIAN_POINT('Ctrl Pts',(20.847715871368,-18.8319413102655,-11.5057246001045));
#83527=CARTESIAN_POINT('Ctrl Pts',(20.8492008518456,-18.8642225299582,-11.5076806946153));
#83528=CARTESIAN_POINT('Ctrl Pts',(20.849573999591,-18.8737300519176,-11.5082546080407));
#83529=CARTESIAN_POINT('Ctrl Pts',(20.8500766583254,-18.8891978439929,-11.5091848146042));
#83530=CARTESIAN_POINT('Ctrl Pts',(20.8502451105319,-18.8951566363744,-11.5095423235335));
#83531=CARTESIAN_POINT('Ctrl Pts',(20.8505453361092,-18.9076437695096,-11.5102897769738));
#83532=CARTESIAN_POINT('Ctrl Pts',(20.8506720795346,-18.9141721771657,-11.5106795600102));
#83533=CARTESIAN_POINT('Ctrl Pts',(20.8509020826932,-18.9297274789792,-11.5116059820139));
#83534=CARTESIAN_POINT('Ctrl Pts',(20.8509778125364,-18.9387546998574,-11.5121417535886));
#83535=CARTESIAN_POINT('Ctrl Pts',(20.8510386248689,-18.9692778580766,-11.5139472425122));
#83536=CARTESIAN_POINT('Ctrl Pts',(20.8507540561398,-18.9907734375804,-11.5152085244988));
#83537=CARTESIAN_POINT('Ctrl Pts',(20.8450325209335,-19.1916906175374,-11.5269113883742));
#83538=CARTESIAN_POINT('Ctrl Pts',(20.8171253807949,-19.3697385869319,-11.5365557069102));
#83539=CARTESIAN_POINT('Ctrl Pts',(20.7335064491919,-19.6578110194735,-11.5528807639419));
#83540=CARTESIAN_POINT('Ctrl Pts',(20.6901264942475,-19.7703861615986,-11.5594887378648));
#83541=CARTESIAN_POINT('Ctrl Pts',(20.6332651972428,-19.8871849646391,-11.5671876724371));
#83542=CARTESIAN_POINT('Ctrl Pts',(20.6290505370366,-19.8956962763619,-11.567753802325));
#83543=CARTESIAN_POINT('Ctrl Pts',(20.6227183965027,-19.9082702570294,-11.5685981618811));
#83544=CARTESIAN_POINT('Ctrl Pts',(20.6206447032474,-19.9123550117381,-11.5688737186914));
#83545=CARTESIAN_POINT('Ctrl Pts',(20.6169305648842,-19.9196126529449,-11.5693656209368));
#83546=CARTESIAN_POINT('Ctrl Pts',(20.6152953318631,-19.9227881501101,-11.5695816373332));
#83547=CARTESIAN_POINT('Ctrl Pts',(20.6117611639355,-19.9296087681366,-11.5700473343768));
#83548=CARTESIAN_POINT('Ctrl Pts',(20.6098596759973,-19.9332524484686,-11.5702971705856));
#83549=CARTESIAN_POINT('Ctrl Pts',(20.6045788323012,-19.9433002904242,-11.5709889862551));
#83550=CARTESIAN_POINT('Ctrl Pts',(20.6011772477073,-19.9496926158906,-11.571432337035));
#83551=CARTESIAN_POINT('Ctrl Pts',(20.5823143017834,-19.9847058911838,-11.5738779785628));
#83552=CARTESIAN_POINT('Ctrl Pts',(20.5662285129147,-20.0129833284871,-11.5759165958648));
#83553=CARTESIAN_POINT('Ctrl Pts',(20.4658095905838,-20.1804130868523,-11.5883224672041));
#83554=CARTESIAN_POINT('Ctrl Pts',(20.3663158597173,-20.3098321079309,-11.5992797311881));
#83555=CARTESIAN_POINT('Ctrl Pts',(20.1716352093816,-20.5103752205316,-11.6175362417707));
#83556=CARTESIAN_POINT('Ctrl Pts',(20.0834833576251,-20.5873075526402,-11.6249755958214));
#83557=CARTESIAN_POINT('Ctrl Pts',(19.9779040037503,-20.6650663736084,-11.6329821437773));
#83558=CARTESIAN_POINT('Ctrl Pts',(19.9663016505822,-20.6734314475657,-11.6338509499323));
#83559=CARTESIAN_POINT('Ctrl Pts',(19.9477042969118,-20.6865553967925,-11.63522632025));
#83560=CARTESIAN_POINT('Ctrl Pts',(19.9407641663374,-20.6913909264373,-11.6357358195233));
#83561=CARTESIAN_POINT('Ctrl Pts',(19.9284749774271,-20.6998444512602,-11.6366314753259));
#83562=CARTESIAN_POINT('Ctrl Pts',(19.9231380320171,-20.7034797857082,-11.6370182892629));
#83563=CARTESIAN_POINT('Ctrl Pts',(19.9120669961836,-20.7109470469126,-11.6378163052585));
#83564=CARTESIAN_POINT('Ctrl Pts',(19.9063306407073,-20.7147754910734,-11.6382273726062));
#83565=CARTESIAN_POINT('Ctrl Pts',(19.8915621430436,-20.7245280127199,-11.6392795647702));
#83566=CARTESIAN_POINT('Ctrl Pts',(19.8825031142347,-20.730411165626,-11.6399191512599));
#83567=CARTESIAN_POINT('Ctrl Pts',(19.8445396250015,-20.7546545086083,-11.6425757148039));
#83568=CARTESIAN_POINT('Ctrl Pts',(19.8152359218099,-20.7723819964638,-11.6445692556177));
#83569=CARTESIAN_POINT('Ctrl Pts',(19.7378073837054,-20.8166932775471,-11.6497020092391));
#83570=CARTESIAN_POINT('Ctrl Pts',(19.6890536395695,-20.8421278977151,-11.6528020600797));
#83571=CARTESIAN_POINT('Ctrl Pts',(19.4687993257244,-20.9463325689024,-11.6663519919665));
#83572=CARTESIAN_POINT('Ctrl Pts',(19.2882366847939,-21.0038528895329,-11.6761989408021));
#83573=CARTESIAN_POINT('Ctrl Pts',(19.0615074184092,-21.0439268018128,-11.6892860114667));
#83574=CARTESIAN_POINT('Ctrl Pts',(19.0203493023044,-21.0499567236923,-11.6916931577766));
#83575=CARTESIAN_POINT('Ctrl Pts',(18.9716775158194,-21.0556286253397,-11.6946045340791));
#83576=CARTESIAN_POINT('Ctrl Pts',(18.9643071724426,-21.0564482881614,-11.6950471458896));
#83577=CARTESIAN_POINT('Ctrl Pts',(18.9523629445168,-21.0577131196342,-11.6957674754418));
#83578=CARTESIAN_POINT('Ctrl Pts',(18.9477915774475,-21.0581821569458,-11.6960438851429));
#83579=CARTESIAN_POINT('Ctrl Pts',(18.9396629915502,-21.0589894404498,-11.6965367218354));
#83580=CARTESIAN_POINT('Ctrl Pts',(18.9361064069539,-21.0593335683528,-11.6967528149547));
#83581=CARTESIAN_POINT('Ctrl Pts',(18.9284664178618,-21.060053278984,-11.6972180080085));
#83582=CARTESIAN_POINT('Ctrl Pts',(18.9243828489696,-21.0604259970107,-11.6974672599795));
#83583=CARTESIAN_POINT('Ctrl Pts',(18.9131280453586,-21.0614202892363,-11.6981558507593));
#83584=CARTESIAN_POINT('Ctrl Pts',(18.9059547614629,-21.0620171491854,-11.6985965403282));
#83585=CARTESIAN_POINT('Ctrl Pts',(18.866967454166,-21.0650609975284,-11.7010010584365));
#83586=CARTESIAN_POINT('Ctrl Pts',(18.8351060686448,-21.0668249173981,-11.7029998170707));
#83587=CARTESIAN_POINT('Ctrl Pts',(18.640068020497,-21.0732054446071,-11.7153925258526));
#83588=CARTESIAN_POINT('Ctrl Pts',(18.4768518915982,-21.0596552023776,-11.7263866294886));
#83589=CARTESIAN_POINT('Ctrl Pts',(18.20214747427,-21.0044380104952,-11.7446901734978));
#83590=CARTESIAN_POINT('Ctrl Pts',(18.0895730541209,-20.9719234247227,-11.752141069334));
#83591=CARTESIAN_POINT('Ctrl Pts',(17.9668806515865,-20.9251754744995,-11.760158164));
#83592=CARTESIAN_POINT('Ctrl Pts',(17.9535675725374,-20.9199478625717,-11.7610269205312));
#83593=CARTESIAN_POINT('Ctrl Pts',(17.9324669848438,-20.9114145468859,-11.7624022273827));
#83594=CARTESIAN_POINT('Ctrl Pts',(17.9246447269608,-20.908196458994,-11.7629117123923));
#83595=CARTESIAN_POINT('Ctrl Pts',(17.9108849996322,-20.9024390257515,-11.7638073516));
#83596=CARTESIAN_POINT('Ctrl Pts',(17.904939508024,-20.8999192486042,-11.764194163129));
#83597=CARTESIAN_POINT('Ctrl Pts',(17.89353031424,-20.895022184358,-11.7649361137698));
#83598=CARTESIAN_POINT('Ctrl Pts',(17.8880649449864,-20.8926489598597,-11.7652913866667));
#83599=CARTESIAN_POINT('Ctrl Pts',(17.8736608268599,-20.8863218551937,-11.7662273757033));
#83600=CARTESIAN_POINT('Ctrl Pts',(17.8647392476091,-20.8823290604288,-11.7668067564509));
#83601=CARTESIAN_POINT('Ctrl Pts',(17.8317010607084,-20.8672675359174,-11.7689512987458));
#83602=CARTESIAN_POINT('Ctrl Pts',(17.8077649311691,-20.8558071856561,-11.7705029736344));
#83603=CARTESIAN_POINT('Ctrl Pts',(17.748947324973,-20.8262740102284,-11.7743156114004));
#83604=CARTESIAN_POINT('Ctrl Pts',(17.714340864297,-20.8076743647222,-11.7765585129559));
#83605=CARTESIAN_POINT('Ctrl Pts',(17.5863822921762,-20.7342403812065,-11.7848824047792));
#83606=CARTESIAN_POINT('Ctrl Pts',(17.4967606950483,-20.6732345109063,-11.7907660949882));
#83607=CARTESIAN_POINT('Ctrl Pts',(17.3058049119968,-20.5205977406213,-11.8040416219604));
#83608=CARTESIAN_POINT('Ctrl Pts',(17.2078836688361,-20.4254988128732,-11.8113988900472));
#83609=CARTESIAN_POINT('Ctrl Pts',(17.1096883063368,-20.309771757951,-11.8202986764722));
#83610=CARTESIAN_POINT('Ctrl Pts',(17.0997220685116,-20.2977593527334,-11.8212220650879));
#83611=CARTESIAN_POINT('Ctrl Pts',(17.0862500243317,-20.2811510078491,-11.8224999238372));
#83612=CARTESIAN_POINT('Ctrl Pts',(17.0826285854063,-20.276648947179,-11.8228464330432));
#83613=CARTESIAN_POINT('Ctrl Pts',(17.0769000682388,-20.2694674323153,-11.8233994590358));
#83614=CARTESIAN_POINT('Ctrl Pts',(17.0747809226385,-20.2667975783345,-11.8236051189291));
#83615=CARTESIAN_POINT('Ctrl Pts',(17.0704149017473,-20.2612695820176,-11.8240310993708));
#83616=CARTESIAN_POINT('Ctrl Pts',(17.0681689443871,-20.2584107741834,-11.8242514848359));
#83617=CARTESIAN_POINT('Ctrl Pts',(17.0628304826103,-20.2515794661267,-11.8247782984213));
#83618=CARTESIAN_POINT('Ctrl Pts',(17.0597447725791,-20.2476017045694,-11.8250852033133));
#83619=CARTESIAN_POINT('Ctrl Pts',(17.049365876814,-20.2341233650724,-11.8261255221791));
#83620=CARTESIAN_POINT('Ctrl Pts',(17.0421392933951,-20.22457211446,-11.8268633902977));
#83621=CARTESIAN_POINT('Ctrl Pts',(16.9597880278116,-20.1137885334449,-11.8354244059807));
#83622=CARTESIAN_POINT('Ctrl Pts',(16.8937766098522,-20.0061119203458,-11.8437552230649));
#83623=CARTESIAN_POINT('Ctrl Pts',(16.8040373496761,-19.8253154296891,-11.8570939438366));
#83624=CARTESIAN_POINT('Ctrl Pts',(16.7740037979316,-19.7556488786253,-11.8620971149624));
#83625=CARTESIAN_POINT('Ctrl Pts',(16.746983787129,-19.6823839726103,-11.8671696135929));
#83626=CARTESIAN_POINT('Ctrl Pts',(16.7461998923975,-19.680247835349,-11.8673173497811));
#83627=CARTESIAN_POINT('Ctrl Pts',(16.7454194500115,-19.678110457305,-11.8674650116542));
#83628=CARTESIAN_POINT('Ctrl Pts',(16.7454194494007,-19.678110455632,-11.6425492951846));
#83629=CARTESIAN_POINT('Ctrl Pts',(16.7537320415196,-19.7008759438364,-11.641052713373));
#83630=CARTESIAN_POINT('Ctrl Pts',(16.7624355372938,-19.7234986099059,-11.6395688907372));
#83631=CARTESIAN_POINT('Ctrl Pts',(16.7756890193127,-19.7562576066727,-11.6374244257199));
#83632=CARTESIAN_POINT('Ctrl Pts',(16.7799326697562,-19.7665140092076,-11.6367536253212));
#83633=CARTESIAN_POINT('Ctrl Pts',(16.7869691239472,-19.7831487461488,-11.6356665220664));
#83634=CARTESIAN_POINT('Ctrl Pts',(16.7897130352974,-19.7895474143097,-11.6352485684289));
#83635=CARTESIAN_POINT('Ctrl Pts',(16.7950530958861,-19.8018325072886,-11.6344464789995));
#83636=CARTESIAN_POINT('Ctrl Pts',(16.7976446063523,-19.8077208530353,-11.6340621904555));
#83637=CARTESIAN_POINT('Ctrl Pts',(16.8036434320464,-19.8211843944791,-11.6331838465548));
#83638=CARTESIAN_POINT('Ctrl Pts',(16.8070685823025,-19.8287515643208,-11.6326904086965));
#83639=CARTESIAN_POINT('Ctrl Pts',(16.8162945366403,-19.8488191900349,-11.6313823452923));
#83640=CARTESIAN_POINT('Ctrl Pts',(16.8221730716316,-19.8612836263645,-11.6305704005356));
#83641=CARTESIAN_POINT('Ctrl Pts',(16.8684507528882,-19.956974427592,-11.6243391614861));
#83642=CARTESIAN_POINT('Ctrl Pts',(16.9141469455404,-20.0375346612341,-11.6191121174511));
#83643=CARTESIAN_POINT('Ctrl Pts',(17.0421776798662,-20.2323052295042,-11.6062233171191));
#83644=CARTESIAN_POINT('Ctrl Pts',(17.1308833385095,-20.3417693801885,-11.5987519067365));
#83645=CARTESIAN_POINT('Ctrl Pts',(17.2669684822215,-20.4791872697837,-11.5880489464911));
#83646=CARTESIAN_POINT('Ctrl Pts',(17.3055494660927,-20.5153332152072,-11.585081337342));
#83647=CARTESIAN_POINT('Ctrl Pts',(17.3592981732938,-20.5620375674297,-11.5809699964668));
#83648=CARTESIAN_POINT('Ctrl Pts',(17.3733124438585,-20.5738987049384,-11.579899980928));
#83649=CARTESIAN_POINT('Ctrl Pts',(17.3942413803745,-20.5911499772119,-11.5783018611282));
#83650=CARTESIAN_POINT('Ctrl Pts',(17.4010384686044,-20.5966821445999,-11.5777828157609));
#83651=CARTESIAN_POINT('Ctrl Pts',(17.4133462435462,-20.6065730627821,-11.5768425119513));
#83652=CARTESIAN_POINT('Ctrl Pts',(17.4188446926063,-20.6109469186219,-11.5764222765148));
#83653=CARTESIAN_POINT('Ctrl Pts',(17.4275603138112,-20.6178093795621,-11.5757557276745));
#83654=CARTESIAN_POINT('Ctrl Pts',(17.4307631168861,-20.6203162675398,-11.5755106941243));
#83655=CARTESIAN_POINT('Ctrl Pts',(17.4339824273816,-20.622821148724,-11.5752642839514));
#83656=CARTESIAN_POINT('Ctrl Pts',(17.4339917617322,-20.6228284114701,-11.5752635694872));
#83657=CARTESIAN_POINT('Ctrl Pts',(17.4340104667637,-20.6228429649781,-11.5752621377762));
#83658=CARTESIAN_POINT('Ctrl Pts',(17.4340198369046,-20.622850255319,-11.5752614205706));
#83659=CARTESIAN_POINT('Ctrl Pts',(17.434038613452,-20.622864863963,-11.5752599833818));
#83660=CARTESIAN_POINT('Ctrl Pts',(17.4340480202258,-20.6228721825511,-11.5752592633703));
#83661=CARTESIAN_POINT('Ctrl Pts',(17.43406687066,-20.62288684817,-11.5752578205222));
#83662=CARTESIAN_POINT('Ctrl Pts',(17.4340763137596,-20.6228941947635,-11.5752570977284));
#83663=CARTESIAN_POINT('Ctrl Pts',(17.4340959153776,-20.6229094442691,-11.5752555973791));
#83664=CARTESIAN_POINT('Ctrl Pts',(17.4341060746042,-20.622917347712,-11.5752548197693));
#83665=CARTESIAN_POINT('Ctrl Pts',(17.4341265700933,-20.622933292024,-11.5752532509966));
#83666=CARTESIAN_POINT('Ctrl Pts',(17.4341369060107,-20.6229413326195,-11.5752524598602));
#83667=CARTESIAN_POINT('Ctrl Pts',(17.4341577587443,-20.622957554226,-11.5752508637384));
#83668=CARTESIAN_POINT('Ctrl Pts',(17.4341682755815,-20.6229657352479,-11.5752500587515));
#83669=CARTESIAN_POINT('Ctrl Pts',(17.4341894938998,-20.6229822406045,-11.5752484346421));
#83670=CARTESIAN_POINT('Ctrl Pts',(17.4342001953889,-20.6229905649394,-11.5752476155189));
#83671=CARTESIAN_POINT('Ctrl Pts',(17.4342217871971,-20.6230073601613,-11.5752459628165));
#83672=CARTESIAN_POINT('Ctrl Pts',(17.4342326771934,-20.6230158307911,-11.5752451292618));
#83673=CARTESIAN_POINT('Ctrl Pts',(17.434254650104,-20.6230329217645,-11.5752434473833));
#83674=CARTESIAN_POINT('Ctrl Pts',(17.434265732831,-20.6230415419563,-11.5752425990738));
#83675=CARTESIAN_POINT('Ctrl Pts',(17.4342880948555,-20.6230589348763,-11.5752408874057));
#83676=CARTESIAN_POINT('Ctrl Pts',(17.4342993746865,-20.623067708013,-11.5752400240064));
#83677=CARTESIAN_POINT('Ctrl Pts',(17.4343221353084,-20.6230854102177,-11.5752382818227));
#83678=CARTESIAN_POINT('Ctrl Pts',(17.4343336161257,-20.6230943392994,-11.5752374030362));
#83679=CARTESIAN_POINT('Ctrl Pts',(17.4343567834148,-20.6231123570255,-11.5752356297187));
#83680=CARTESIAN_POINT('Ctrl Pts',(17.4343684697384,-20.6231214455476,-11.575234735199));
#83681=CARTESIAN_POINT('Ctrl Pts',(17.4343920522796,-20.6231397854306,-11.5752329300904));
#83682=CARTESIAN_POINT('Ctrl Pts',(17.4344039488733,-20.6231490370769,-11.5752320194727));
#83683=CARTESIAN_POINT('Ctrl Pts',(17.4344279569348,-20.6231677070596,-11.5752301817866));
#83684=CARTESIAN_POINT('Ctrl Pts',(17.4344400680302,-20.6231771250989,-11.5752292547467));
#83685=CARTESIAN_POINT('Ctrl Pts',(17.4344645098804,-20.6231961315667,-11.5752273838499));
#83686=CARTESIAN_POINT('Ctrl Pts',(17.4344768406379,-20.6232057199895,-11.5752264399927));
#83687=CARTESIAN_POINT('Ctrl Pts',(17.4345017265397,-20.6232250708766,-11.5752245350993));
#83688=CARTESIAN_POINT('Ctrl Pts',(17.4345142817885,-20.6232348334143,-11.5752235740549));
#83689=CARTESIAN_POINT('Ctrl Pts',(17.4345396217877,-20.623254536484,-11.5752216343955));
#83690=CARTESIAN_POINT('Ctrl Pts',(17.4345524065069,-20.6232644769836,-11.5752206557827));
#83691=CARTESIAN_POINT('Ctrl Pts',(17.4372579127235,-20.6253680387425,-11.5750135610604));
#83692=CARTESIAN_POINT('Ctrl Pts',(17.4399556321339,-20.6274551045601,-11.5748069784263));
#83693=CARTESIAN_POINT('Ctrl Pts',(17.4462816455741,-20.6323247742902,-11.5743223663908));
#83694=CARTESIAN_POINT('Ctrl Pts',(17.4499139066277,-20.6351021393012,-11.5740439728026));
#83695=CARTESIAN_POINT('Ctrl Pts',(17.4610839464052,-20.643585972655,-11.5731874952056));
#83696=CARTESIAN_POINT('Ctrl Pts',(17.4686508572441,-20.6492536409409,-11.5726068015111));
#83697=CARTESIAN_POINT('Ctrl Pts',(17.5750299268252,-20.7278255136771,-11.5644392897217));
#83698=CARTESIAN_POINT('Ctrl Pts',(17.6799538290228,-20.7920401182624,-11.5563501677246));
#83699=CARTESIAN_POINT('Ctrl Pts',(17.8839337949351,-20.8936821142843,-11.5412917490764));
#83700=CARTESIAN_POINT('Ctrl Pts',(17.9814010562225,-20.9334994232368,-11.534347998024));
#83701=CARTESIAN_POINT('Ctrl Pts',(18.1338418360431,-20.9828950547948,-11.5240479729228));
#83702=CARTESIAN_POINT('Ctrl Pts',(18.1869009012604,-20.9978269580655,-11.520559119859));
#83703=CARTESIAN_POINT('Ctrl Pts',(18.2738420581457,-21.0186688752732,-11.5150019494289));
#83704=CARTESIAN_POINT('Ctrl Pts',(18.3073890142597,-21.0258536241991,-11.5128952001977));
#83705=CARTESIAN_POINT('Ctrl Pts',(18.3517178012349,-21.0342262456084,-11.5101587984258));
#83706=CARTESIAN_POINT('Ctrl Pts',(18.3623535907935,-21.0361508512346,-11.5095058072679));
#83707=CARTESIAN_POINT('Ctrl Pts',(18.3798007419064,-21.0391702056683,-11.5084403237669));
#83708=CARTESIAN_POINT('Ctrl Pts',(18.3866034436415,-21.0403132466768,-11.5080263020698));
#83709=CARTESIAN_POINT('Ctrl Pts',(18.3997843219157,-21.0424618078854,-11.507226788781));
#83710=CARTESIAN_POINT('Ctrl Pts',(18.4061617425628,-21.0434714361165,-11.5068411708662));
#83711=CARTESIAN_POINT('Ctrl Pts',(18.4209004478961,-21.0457356932661,-11.5059527427402));
#83712=CARTESIAN_POINT('Ctrl Pts',(18.4292648647372,-21.0469694468616,-11.5054505986319));
#83713=CARTESIAN_POINT('Ctrl Pts',(18.4517859894326,-21.0501535837854,-11.5041039590927));
#83714=CARTESIAN_POINT('Ctrl Pts',(18.4659555796157,-21.0520108124781,-11.5032624052741));
#83715=CARTESIAN_POINT('Ctrl Pts',(18.5961652861964,-21.0677381954921,-11.4955788498022));
#83716=CARTESIAN_POINT('Ctrl Pts',(18.7131556084473,-21.0721220006379,-11.4890537017563));
#83717=CARTESIAN_POINT('Ctrl Pts',(18.9926300454236,-21.0594457029593,-11.4737384312352));
#83718=CARTESIAN_POINT('Ctrl Pts',(19.1539211072279,-21.0333147873812,-11.4651317675645));
#83719=CARTESIAN_POINT('Ctrl Pts',(19.3417341561108,-20.9801506513749,-11.4539222201374));
#83720=CARTESIAN_POINT('Ctrl Pts',(19.372658243819,-20.9706260820052,-11.4520348788544));
#83721=CARTESIAN_POINT('Ctrl Pts',(19.4102082543697,-20.9581115764149,-11.4496781635906));
#83722=CARTESIAN_POINT('Ctrl Pts',(19.4170546614957,-20.9557908040222,-11.4492457962696));
#83723=CARTESIAN_POINT('Ctrl Pts',(19.4277721090722,-20.9520965305072,-11.4485645678286));
#83724=CARTESIAN_POINT('Ctrl Pts',(19.4316513414119,-20.9507467262863,-11.4483170873816));
#83725=CARTESIAN_POINT('Ctrl Pts',(19.4388970201079,-20.948201881626,-11.4478531006819));
#83726=CARTESIAN_POINT('Ctrl Pts',(19.4422643782183,-20.9470096067571,-11.4476367589405));
#83727=CARTESIAN_POINT('Ctrl Pts',(19.4499468844092,-20.944267572622,-11.4471415728569));
#83728=CARTESIAN_POINT('Ctrl Pts',(19.4542600107789,-20.9427123192907,-11.4468624054466));
#83729=CARTESIAN_POINT('Ctrl Pts',(19.4675111947637,-20.9378854247326,-11.4460012274905));
#83730=CARTESIAN_POINT('Ctrl Pts',(19.476432123959,-20.9345675591387,-11.4454165662993));
#83731=CARTESIAN_POINT('Ctrl Pts',(19.5577862152014,-20.9036843226468,-11.4400418365533));
#83732=CARTESIAN_POINT('Ctrl Pts',(19.6286695134842,-20.8722237390315,-11.4350484837293));
#83733=CARTESIAN_POINT('Ctrl Pts',(19.73407924571,-20.8183342422861,-11.4273007178977));
#83734=CARTESIAN_POINT('Ctrl Pts',(19.7699503063158,-20.798664245764,-11.4246034109206));
#83735=CARTESIAN_POINT('Ctrl Pts',(19.8995680070527,-20.7226223033766,-11.4146765282574));
#83736=CARTESIAN_POINT('Ctrl Pts',(19.9894839907786,-20.6600443598228,-11.4074442175789));
#83737=CARTESIAN_POINT('Ctrl Pts',(20.1168138872927,-20.5559170891765,-11.3968715951581));
#83738=CARTESIAN_POINT('Ctrl Pts',(20.1580871526203,-20.5193866397022,-11.3933829028324));
#83739=CARTESIAN_POINT('Ctrl Pts',(20.2226688194853,-20.4575665516544,-11.3878259584399));
#83740=CARTESIAN_POINT('Ctrl Pts',(20.2468675784327,-20.433248595597,-11.3857192784057));
#83741=CARTESIAN_POINT('Ctrl Pts',(20.2779010987559,-20.400507926076,-11.3829829519992));
#83742=CARTESIAN_POINT('Ctrl Pts',(20.2852762497047,-20.3926067536049,-11.3823299686178));
#83743=CARTESIAN_POINT('Ctrl Pts',(20.2972587535368,-20.3795708917489,-11.3812644945531));
#83744=CARTESIAN_POINT('Ctrl Pts',(20.3019020239034,-20.3744696224067,-11.3808504745681));
#83745=CARTESIAN_POINT('Ctrl Pts',(20.3108431706396,-20.3645495761415,-11.380050962339));
#83746=CARTESIAN_POINT('Ctrl Pts',(20.3151440917833,-20.3597336581523,-11.3796653437835));
#83747=CARTESIAN_POINT('Ctrl Pts',(20.3250258065048,-20.3485662773322,-11.3787769109711));
#83748=CARTESIAN_POINT('Ctrl Pts',(20.3305907420744,-20.3422008809634,-11.3782747628394));
#83749=CARTESIAN_POINT('Ctrl Pts',(20.3454585502765,-20.3249874567626,-11.3769281053858));
#83750=CARTESIAN_POINT('Ctrl Pts',(20.3546900645286,-20.3140781715222,-11.3760865377999));
#83751=CARTESIAN_POINT('Ctrl Pts',(20.4384059652236,-20.2130912128594,-11.3684019128798));
#83752=CARTESIAN_POINT('Ctrl Pts',(20.5054258000469,-20.1170779562622,-11.3618758147859));
#83753=CARTESIAN_POINT('Ctrl Pts',(20.6460722948785,-19.8751547911064,-11.3465565665481));
#83754=CARTESIAN_POINT('Ctrl Pts',(20.7114169631579,-19.7253339817636,-11.3379470373315));
#83755=CARTESIAN_POINT('Ctrl Pts',(20.7683513185978,-19.5386398338669,-11.3267372466973));
#83756=CARTESIAN_POINT('Ctrl Pts',(20.7770615655289,-19.5075454664342,-11.3248536759389));
#83757=CARTESIAN_POINT('Ctrl Pts',(20.7868459593231,-19.4692665286364,-11.322501156041));
#83758=CARTESIAN_POINT('Ctrl Pts',(20.7885992210691,-19.4622580050491,-11.3220690583001));
#83759=CARTESIAN_POINT('Ctrl Pts',(20.7912926926222,-19.4512520799288,-11.3213881610939));
#83760=CARTESIAN_POINT('Ctrl Pts',(20.7922572222017,-19.4472606071817,-11.3211407400853));
#83761=CARTESIAN_POINT('Ctrl Pts',(20.7940391320323,-19.4397914889639,-11.3206768035368));
#83762=CARTESIAN_POINT('Ctrl Pts',(20.7948593248133,-19.4363145722366,-11.320460452135));
#83763=CARTESIAN_POINT('Ctrl Pts',(20.7967124502302,-19.4283689576754,-11.3199651629888));
#83764=CARTESIAN_POINT('Ctrl Pts',(20.7977396600296,-19.4238989837647,-11.3196859016558));
#83765=CARTESIAN_POINT('Ctrl Pts',(20.8008555854555,-19.4101350561564,-11.3188241522013));
#83766=CARTESIAN_POINT('Ctrl Pts',(20.8028960697313,-19.40083046428,-11.3182390084326));
#83767=CARTESIAN_POINT('Ctrl Pts',(20.8297138336639,-19.274471861711,-11.3102604968273));
#83768=CARTESIAN_POINT('Ctrl Pts',(20.8445842122161,-19.155549064988,-11.3023899189407));
#83769=CARTESIAN_POINT('Ctrl Pts',(20.8564950518746,-18.8556874059274,-11.2825645407231));
#83770=CARTESIAN_POINT('Ctrl Pts',(20.8405691200868,-18.6751359406159,-11.2707105169302));
#83771=CARTESIAN_POINT('Ctrl Pts',(20.7973522962586,-18.4779529803882,-11.2583119260309));
#83772=CARTESIAN_POINT('Ctrl Pts',(20.7924749720833,-18.4572029540042,-11.2570128401839));
#83773=CARTESIAN_POINT('Ctrl Pts',(20.7850943720238,-18.427803647045,-11.255179722248));
#83774=CARTESIAN_POINT('Ctrl Pts',(20.7828481455969,-18.4190917343587,-11.2546374496952));
#83775=CARTESIAN_POINT('Ctrl Pts',(20.7788773590873,-18.4040874629557,-11.2537050522803));
#83776=CARTESIAN_POINT('Ctrl Pts',(20.7771791354058,-18.397788321957,-11.2533140810688));
#83777=CARTESIAN_POINT('Ctrl Pts',(20.7738718502158,-18.3857425983033,-11.2525673006876));
#83778=CARTESIAN_POINT('Ctrl Pts',(20.772267558791,-18.3799947813332,-11.2522113409767));
#83779=CARTESIAN_POINT('Ctrl Pts',(20.7680328005942,-18.3650666463349,-11.2512877930991));
#83780=CARTESIAN_POINT('Ctrl Pts',(20.7653644631293,-18.3558971414135,-11.2507214421635));
#83781=CARTESIAN_POINT('Ctrl Pts',(20.7560548436776,-18.3246940293383,-11.2487971282787));
#83782=CARTESIAN_POINT('Ctrl Pts',(20.7491162434409,-18.3027503113763,-11.2474488748676));
#83783=CARTESIAN_POINT('Ctrl Pts',(20.6862858652122,-18.1147655702311,-11.2359316270504));
#83784=CARTESIAN_POINT('Ctrl Pts',(20.610342576037,-17.9561451711754,-11.226510631122));
#83785=CARTESIAN_POINT('Ctrl Pts',(20.4686207712067,-17.7352895460093,-11.212232970457));
#83786=CARTESIAN_POINT('Ctrl Pts',(20.4170386329782,-17.6648822502407,-11.2074595508535));
#83787=CARTESIAN_POINT('Ctrl Pts',(20.3370414771626,-17.5687496806177,-11.2003194528138));
#83788=CARTESIAN_POINT('Ctrl Pts',(20.3120403183255,-17.5402947274221,-11.1981195543073));
#83789=CARTESIAN_POINT('Ctrl Pts',(20.2811408986288,-17.5069735593155,-11.1954158292783));
#83790=CARTESIAN_POINT('Ctrl Pts',(20.2759608043423,-17.5014472610656,-11.1949630568863));
#83791=CARTESIAN_POINT('Ctrl Pts',(20.2678743007375,-17.4929125707651,-11.1942567783261));
#83792=CARTESIAN_POINT('Ctrl Pts',(20.2649883835013,-17.4898847290643,-11.1940048250653));
#83793=CARTESIAN_POINT('Ctrl Pts',(20.2596271493294,-17.4842931146069,-11.1935369125596));
#83794=CARTESIAN_POINT('Ctrl Pts',(20.2571543251906,-17.4817270317136,-11.1933211454175));
#83795=CARTESIAN_POINT('Ctrl Pts',(20.2515587020548,-17.4759496451661,-11.1928330220693));
#83796=CARTESIAN_POINT('Ctrl Pts',(20.2484322014706,-17.4727420203078,-11.1925603790894));
#83797=CARTESIAN_POINT('Ctrl Pts',(20.2392018825856,-17.4633321331643,-11.1917557943067));
#83798=CARTESIAN_POINT('Ctrl Pts',(20.2330700610129,-17.4571576433272,-11.1912217263059));
#83799=CARTESIAN_POINT('Ctrl Pts',(20.1893037431093,-17.4136268759787,-11.1874139730482));
#83800=CARTESIAN_POINT('Ctrl Pts',(20.150318558489,-17.3776615438736,-11.184044363763));
#83801=CARTESIAN_POINT('Ctrl Pts',(20.0956697262834,-17.330919632673,-11.1793977600611));
#83802=CARTESIAN_POINT('Ctrl Pts',(20.0811475307665,-17.3188314534767,-11.1781699099195));
#83803=CARTESIAN_POINT('Ctrl Pts',(19.9523449682026,-17.2145039755766,-11.1673523549762));
#83804=CARTESIAN_POINT('Ctrl Pts',(19.8289029615913,-17.134185476818,-11.1575172365772));
#83805=CARTESIAN_POINT('Ctrl Pts',(19.6432086155032,-17.0391915892997,-11.1440421205149));
#83806=CARTESIAN_POINT('Ctrl Pts',(19.5870697377721,-17.0135032962788,-11.1401175683879));
#83807=CARTESIAN_POINT('Ctrl Pts',(19.4954010172047,-16.9763121910109,-11.1339536533744));
#83808=CARTESIAN_POINT('Ctrl Pts',(19.4605532315251,-16.9632329183491,-11.1316645689448));
#83809=CARTESIAN_POINT('Ctrl Pts',(19.4148571025361,-16.9474435690025,-11.128730560912));
#83810=CARTESIAN_POINT('Ctrl Pts',(19.4043086281309,-16.943891629022,-11.1280578773836));
#83811=CARTESIAN_POINT('Ctrl Pts',(19.3871106333284,-16.9382512406276,-11.1269684872809));
#83812=CARTESIAN_POINT('Ctrl Pts',(19.3804780510407,-16.9361121815512,-11.1265501168865));
#83813=CARTESIAN_POINT('Ctrl Pts',(19.3677046436966,-16.9320621832838,-11.1257477388487));
#83814=CARTESIAN_POINT('Ctrl Pts',(19.3615654459575,-16.9301464021121,-11.1253635757175));
#83815=CARTESIAN_POINT('Ctrl Pts',(19.3474914930732,-16.9258248017762,-11.1244862267832));
#83816=CARTESIAN_POINT('Ctrl Pts',(19.3395511111717,-16.9234375531636,-11.123993653672));
#83817=CARTESIAN_POINT('Ctrl Pts',(19.3184249267719,-16.9172211358404,-11.1226894014822));
#83818=CARTESIAN_POINT('Ctrl Pts',(19.3052154127258,-16.9134734520792,-11.1218803780707));
#83819=CARTESIAN_POINT('Ctrl Pts',(19.204594536313,-16.8859810703903,-11.1157650702585));
#83820=CARTESIAN_POINT('Ctrl Pts',(19.1157711315264,-16.8677382295575,-11.1106426004892));
#83821=CARTESIAN_POINT('Ctrl Pts',(18.8872940776131,-16.8359152511998,-11.0978743564297));
#83822=CARTESIAN_POINT('Ctrl Pts',(18.7469761208272,-16.8304101750477,-11.0904248980446));
#83823=CARTESIAN_POINT('Ctrl Pts',(18.5526132765211,-16.8420776196516,-11.0796641828763));
#83824=CARTESIAN_POINT('Ctrl Pts',(18.4982307953527,-16.8474607033818,-11.0766013706266));
#83825=CARTESIAN_POINT('Ctrl Pts',(18.4161300202232,-16.8588095725219,-11.0718193560586));
#83826=CARTESIAN_POINT('Ctrl Pts',(18.3882204273055,-16.8632386922141,-11.070165651825));
#83827=CARTESIAN_POINT('Ctrl Pts',(18.3535925120223,-16.8694469737997,-11.0680695012531));
#83828=CARTESIAN_POINT('Ctrl Pts',(18.3467817566077,-16.8707025698366,-11.0676550730619));
#83829=CARTESIAN_POINT('Ctrl Pts',(18.3360076676299,-16.8727435397262,-11.0669958992063));
#83830=CARTESIAN_POINT('Ctrl Pts',(18.332040141934,-16.8735068929412,-11.0667523900545));
#83831=CARTESIAN_POINT('Ctrl Pts',(18.3245570934836,-16.8749688607651,-11.0662916177653));
#83832=CARTESIAN_POINT('Ctrl Pts',(18.3210411510002,-16.8756650474065,-11.0660744937299));
#83833=CARTESIAN_POINT('Ctrl Pts',(18.3130009792761,-16.8772782995604,-11.0655765552337));
#83834=CARTESIAN_POINT('Ctrl Pts',(18.308477975333,-16.8782012355781,-11.0652954091011));
#83835=CARTESIAN_POINT('Ctrl Pts',(18.2964661197226,-16.880693250898,-11.0645460883637));
#83836=CARTESIAN_POINT('Ctrl Pts',(18.2889827743871,-16.8822881335517,-11.0640764979191));
#83837=CARTESIAN_POINT('Ctrl Pts',(18.2362947215605,-16.8938161902402,-11.0607515242731));
#83838=CARTESIAN_POINT('Ctrl Pts',(18.191421248772,-16.9051881548201,-11.0578225841764));
#83839=CARTESIAN_POINT('Ctrl Pts',(18.14178032646,-16.919515331774,-11.0544997195492));
#83840=CARTESIAN_POINT('Ctrl Pts',(18.1366060246779,-16.921030156378,-11.054152343825));
#83841=CARTESIAN_POINT('Ctrl Pts',(18.1271058068358,-16.9238508790084,-11.053512739365));
#83842=CARTESIAN_POINT('Ctrl Pts',(18.1227781631577,-16.9251508974827,-11.0532206875028));
#83843=CARTESIAN_POINT('Ctrl Pts',(18.0946975268686,-16.9336843962723,-11.0513212923962));
#83844=CARTESIAN_POINT('Ctrl Pts',(18.0710697440528,-16.9413212731072,-11.0497027884841));
#83845=CARTESIAN_POINT('Ctrl Pts',(18.0104644642029,-16.9620942411824,-11.0455069299301));
#83846=CARTESIAN_POINT('Ctrl Pts',(17.9737080802997,-16.9758459856872,-11.0429190771497));
#83847=CARTESIAN_POINT('Ctrl Pts',(17.8360959793658,-17.0317389663027,-11.0331074211231));
#83848=CARTESIAN_POINT('Ctrl Pts',(17.7381652476012,-17.0806500375686,-11.02588107901));
#83849=CARTESIAN_POINT('Ctrl Pts',(17.5972933601307,-17.1652119986825,-11.015320990367));
#83850=CARTESIAN_POINT('Ctrl Pts',(17.5512599991049,-17.1953440138584,-11.0118388218654));
#83851=CARTESIAN_POINT('Ctrl Pts',(17.4785407929527,-17.2470998284689,-11.0062910529837));
#83852=CARTESIAN_POINT('Ctrl Pts',(17.4511174492235,-17.2676381054598,-11.0041871826606));
#83853=CARTESIAN_POINT('Ctrl Pts',(17.4157162757556,-17.2955176652298,-11.0014539166859));
#83854=CARTESIAN_POINT('Ctrl Pts',(17.4072804090453,-17.3022664346126,-11.0008012492629));
#83855=CARTESIAN_POINT('Ctrl Pts',(17.3935441124593,-17.3134291045566,-10.999736158596));
#83856=CARTESIAN_POINT('Ctrl Pts',(17.3882130164572,-17.3178047966921,-10.9993222081741));
#83857=CARTESIAN_POINT('Ctrl Pts',(17.377932189508,-17.3263275886207,-10.9985227389518));
#83858=CARTESIAN_POINT('Ctrl Pts',(17.372979868802,-17.3304714311267,-10.9981370943185));
#83859=CARTESIAN_POINT('Ctrl Pts',(17.3615850302572,-17.3400950145774,-10.9972484708676));
#83860=CARTESIAN_POINT('Ctrl Pts',(17.3551562084127,-17.3455908576044,-10.996746159093));
#83861=CARTESIAN_POINT('Ctrl Pts',(17.3379467303153,-17.3604822465446,-10.9953987729137));
#83862=CARTESIAN_POINT('Ctrl Pts',(17.3272279335409,-17.369948844274,-10.9945566452876));
#83863=CARTESIAN_POINT('Ctrl Pts',(17.2292160340306,-17.4582945268088,-10.9868265710336));
#83864=CARTESIAN_POINT('Ctrl Pts',(17.1485393408821,-17.5442178203698,-10.980260094241));
#83865=CARTESIAN_POINT('Ctrl Pts',(16.9737389814325,-17.7645919269791,-10.964865573814));
#83866=CARTESIAN_POINT('Ctrl Pts',(16.8872806441647,-17.9041106665782,-10.9562204796831));
#83867=CARTESIAN_POINT('Ctrl Pts',(16.8045807838236,-18.0802252941688,-10.9450299580342));
#83868=CARTESIAN_POINT('Ctrl Pts',(16.7920251371487,-18.1085647309433,-10.9432200679027));
#83869=CARTESIAN_POINT('Ctrl Pts',(16.7773512455334,-18.1437515631972,-10.9409495882056));
#83870=CARTESIAN_POINT('Ctrl Pts',(16.7746389808509,-18.1503490302559,-10.9405228834263));
#83871=CARTESIAN_POINT('Ctrl Pts',(16.7704255502637,-18.1607471465774,-10.9398486139372));
#83872=CARTESIAN_POINT('Ctrl Pts',(16.7689019287588,-18.1645387200241,-10.9396023836658));
#83873=CARTESIAN_POINT('Ctrl Pts',(16.7660657187922,-18.1716561979109,-10.9391394394251));
#83874=CARTESIAN_POINT('Ctrl Pts',(16.7647505755518,-18.1749810245281,-10.9389228820742));
#83875=CARTESIAN_POINT('Ctrl Pts',(16.7617562476082,-18.1826074444657,-10.9384254716461));
#83876=CARTESIAN_POINT('Ctrl Pts',(16.7600827149832,-18.1869111983962,-10.9381442843083));
#83877=CARTESIAN_POINT('Ctrl Pts',(16.7549425689768,-18.2002590221147,-10.9372707676825));
#83878=CARTESIAN_POINT('Ctrl Pts',(16.751523990189,-18.2093212838226,-10.9366756787059));
#83879=CARTESIAN_POINT('Ctrl Pts',(16.7114754927785,-18.3177322694258,-10.9295352455752));
#83880=CARTESIAN_POINT('Ctrl Pts',(16.682291093586,-18.41965971884,-10.9226144770236));
#83881=CARTESIAN_POINT('Ctrl Pts',(16.631792491142,-18.6638812142766,-10.906164778877));
#83882=CARTESIAN_POINT('Ctrl Pts',(16.6170952312567,-18.8070440704221,-10.8966461771693));
#83883=CARTESIAN_POINT('Ctrl Pts',(16.6169595357191,-19.0125966091521,-10.8835935545742));
#83884=CARTESIAN_POINT('Ctrl Pts',(16.6196417426175,-19.0745670565041,-10.8797325121679));
#83885=CARTESIAN_POINT('Ctrl Pts',(16.6261219965063,-19.1487067147389,-10.8751997242484));
#83886=CARTESIAN_POINT('Ctrl Pts',(16.6273121374462,-19.1610680973189,-10.8744468127296));
#83887=CARTESIAN_POINT('Ctrl Pts',(16.6294460867429,-19.1813590546165,-10.8732154416387));
#83888=CARTESIAN_POINT('Ctrl Pts',(16.6303260989716,-19.1892949021742,-10.8727349862853));
#83889=CARTESIAN_POINT('Ctrl Pts',(16.6319896970467,-19.2035598412311,-10.8718733420666));
#83890=CARTESIAN_POINT('Ctrl Pts',(16.6327570210474,-19.2098906982097,-10.8714916456779));
#83891=CARTESIAN_POINT('Ctrl Pts',(16.6344530082202,-19.2233732415897,-10.870680230157));
#83892=CARTESIAN_POINT('Ctrl Pts',(16.6353896338161,-19.2305238586969,-10.8702507673755));
#83893=CARTESIAN_POINT('Ctrl Pts',(16.6380125543551,-19.2497836446978,-10.8690963293766));
#83894=CARTESIAN_POINT('Ctrl Pts',(16.6397672532445,-19.261883338077,-10.8683735208393));
#83895=CARTESIAN_POINT('Ctrl Pts',(16.6490971357875,-19.3225155647284,-10.8647629875313));
#83896=CARTESIAN_POINT('Ctrl Pts',(16.6582553255207,-19.3707915175288,-10.8619257816648));
#83897=CARTESIAN_POINT('Ctrl Pts',(16.688975743057,-19.5067116773627,-10.8540036597052));
#83898=CARTESIAN_POINT('Ctrl Pts',(16.7144720710822,-19.5933556444856,-10.8490363862048));
#83899=CARTESIAN_POINT('Ctrl Pts',(16.7454194496957,-19.67811045644,-10.8441190240937));
#83900=CARTESIAN_POINT('Origin',(18.734,-18.952,0.));
#83901=CARTESIAN_POINT('',(16.7454194499602,-19.6781104571642,-10.0464611570501));
#83902=CARTESIAN_POINT('',(16.7460269997162,-19.677879090888,-10.2662522551303));
#83903=CARTESIAN_POINT('',(16.7454194499637,-19.6781104571739,0.));
#83904=CARTESIAN_POINT('',(16.614176999282,-18.9530774369803,-10.3109437209775));
#83905=CARTESIAN_POINT('Ctrl Pts',(16.7460269997163,-19.6778790908883,-10.2662522551303));
#83906=CARTESIAN_POINT('Ctrl Pts',(16.6804601656347,-19.5036328070715,-10.2774434318562));
#83907=CARTESIAN_POINT('Ctrl Pts',(16.6235838006535,-19.2611105659415,-10.2923405871386));
#83908=CARTESIAN_POINT('Ctrl Pts',(16.6137958948767,-19.0144660751781,-10.307237742421));
#83909=CARTESIAN_POINT('Ctrl Pts',(16.614176999282,-18.9530774369803,-10.3109437209775));
#83910=CARTESIAN_POINT('Ctrl Pts',(16.6170002227488,-18.9529711427249,-10.3093226184743));
#83911=CARTESIAN_POINT('Ctrl Pts',(16.616920601068,-18.7794033692573,-10.3204871727274));
#83912=CARTESIAN_POINT('Ctrl Pts',(16.6381853782203,-18.6064738253141,-10.3321971334834));
#83913=CARTESIAN_POINT('Ctrl Pts',(16.6951945281285,-18.3786675872106,-10.347362818657));
#83914=CARTESIAN_POINT('Ctrl Pts',(16.7126292170894,-18.3199406142348,-10.3512558888495));
#83915=CARTESIAN_POINT('Ctrl Pts',(16.7446483001179,-18.2270596950899,-10.3573763525111));
#83916=CARTESIAN_POINT('Ctrl Pts',(16.7576257037044,-18.1923925068387,-10.3596526032797));
#83917=CARTESIAN_POINT('Ctrl Pts',(16.7756718658497,-18.1477840385356,-10.3625727652533));
#83918=CARTESIAN_POINT('Ctrl Pts',(16.7799187407749,-18.1375192860528,-10.3632441131218));
#83919=CARTESIAN_POINT('Ctrl Pts',(16.7869592378109,-18.1208743967158,-10.364331881253));
#83920=CARTESIAN_POINT('Ctrl Pts',(16.7897038552785,-18.114473880118,-10.3647499560836));
#83921=CARTESIAN_POINT('Ctrl Pts',(16.795044322094,-18.1021875158721,-10.3655521292429));
#83922=CARTESIAN_POINT('Ctrl Pts',(16.7976355092999,-18.0962997372738,-10.3659363811201));
#83923=CARTESIAN_POINT('Ctrl Pts',(16.803632170112,-18.0828406585491,-10.3668144346507));
#83924=CARTESIAN_POINT('Ctrl Pts',(16.8070554379508,-18.0752773658198,-10.3673076202088));
#83925=CARTESIAN_POINT('Ctrl Pts',(16.8162731215175,-18.0552268295972,-10.3686145711229));
#83926=CARTESIAN_POINT('Ctrl Pts',(16.8221450549382,-18.0427755051673,-10.3694256630356));
#83927=CARTESIAN_POINT('Ctrl Pts',(16.86816945609,-17.9475992362546,-10.3756234047571));
#83928=CARTESIAN_POINT('Ctrl Pts',(16.9135543444935,-17.8675069712912,-10.3808202622217));
#83929=CARTESIAN_POINT('Ctrl Pts',(17.0412308323666,-17.6729240859934,-10.3936931494177));
#83930=CARTESIAN_POINT('Ctrl Pts',(17.129993379071,-17.5632368212038,-10.4011754664971));
#83931=CARTESIAN_POINT('Ctrl Pts',(17.2663405273322,-17.4254068468746,-10.4119025284124));
#83932=CARTESIAN_POINT('Ctrl Pts',(17.3051057925353,-17.3890631632552,-10.414884573204));
#83933=CARTESIAN_POINT('Ctrl Pts',(17.3590975317378,-17.3421330583069,-10.4190145946725));
#83934=CARTESIAN_POINT('Ctrl Pts',(17.3731579458471,-17.3302302185466,-10.4200881377047));
#83935=CARTESIAN_POINT('Ctrl Pts',(17.3941500956425,-17.3129245248535,-10.4216910836558));
#83936=CARTESIAN_POINT('Ctrl Pts',(17.4009633778602,-17.3073786035323,-10.4222113642647));
#83937=CARTESIAN_POINT('Ctrl Pts',(17.4132981893964,-17.2974652353411,-10.4231537311002));
#83938=CARTESIAN_POINT('Ctrl Pts',(17.4188074014079,-17.2930825863118,-10.4235747878974));
#83939=CARTESIAN_POINT('Ctrl Pts',(17.4275362937868,-17.2862094511804,-10.4242423503102));
#83940=CARTESIAN_POINT('Ctrl Pts',(17.4307415303657,-17.2837005877618,-10.4244875695442));
#83941=CARTESIAN_POINT('Ctrl Pts',(17.4339632609263,-17.2811937643168,-10.4247341645007));
#83942=CARTESIAN_POINT('Ctrl Pts',(17.4339725707876,-17.2811865204534,-10.4247348770892));
#83943=CARTESIAN_POINT('Ctrl Pts',(17.4339912262073,-17.2811720052016,-10.4247363050002));
#83944=CARTESIAN_POINT('Ctrl Pts',(17.434000571806,-17.2811647337827,-10.4247370203259));
#83945=CARTESIAN_POINT('Ctrl Pts',(17.434019299241,-17.2811501630023,-10.424738453753));
#83946=CARTESIAN_POINT('Ctrl Pts',(17.4340286808851,-17.2811428637912,-10.4247391718396));
#83947=CARTESIAN_POINT('Ctrl Pts',(17.4340474803129,-17.2811282375055,-10.424740610781));
#83948=CARTESIAN_POINT('Ctrl Pts',(17.4340568986222,-17.2811209100229,-10.424741331676));
#83949=CARTESIAN_POINT('Ctrl Pts',(17.4340757716204,-17.2811062270105,-10.4247427762524));
#83950=CARTESIAN_POINT('Ctrl Pts',(17.4340852265746,-17.2810988712752,-10.4247434999543));
#83951=CARTESIAN_POINT('Ctrl Pts',(17.4341048926039,-17.281083571828,-10.424745005235));
#83952=CARTESIAN_POINT('Ctrl Pts',(17.434115103232,-17.2810756284853,-10.4247457867799));
#83953=CARTESIAN_POINT('Ctrl Pts',(17.4341357027151,-17.2810596034516,-10.4247473635138));
#83954=CARTESIAN_POINT('Ctrl Pts',(17.4341460916624,-17.2810515216941,-10.42474815871));
#83955=CARTESIAN_POINT('Ctrl Pts',(17.4341670515367,-17.2810352169275,-10.424749763034));
#83956=CARTESIAN_POINT('Ctrl Pts',(17.4341776223344,-17.2810269940244,-10.4247505721519));
#83957=CARTESIAN_POINT('Ctrl Pts',(17.4341989499914,-17.2810104038079,-10.4247522046319));
#83958=CARTESIAN_POINT('Ctrl Pts',(17.4342097065417,-17.2810020367405,-10.4247530279704));
#83959=CARTESIAN_POINT('Ctrl Pts',(17.4342314092451,-17.2809851554581,-10.4247546891626));
#83960=CARTESIAN_POINT('Ctrl Pts',(17.4342423558561,-17.2809766408928,-10.4247555270515));
#83961=CARTESIAN_POINT('Ctrl Pts',(17.4342644429403,-17.2809594613194,-10.4247572176708));
#83962=CARTESIAN_POINT('Ctrl Pts',(17.4342755832488,-17.2809507964456,-10.4247580703887));
#83963=CARTESIAN_POINT('Ctrl Pts',(17.4342980620022,-17.2809333129492,-10.4247597909932));
#83964=CARTESIAN_POINT('Ctrl Pts',(17.4343094004992,-17.2809244942925,-10.4247606588839));
#83965=CARTESIAN_POINT('Ctrl Pts',(17.4343322799526,-17.2809066998876,-10.4247624101651));
#83966=CARTESIAN_POINT('Ctrl Pts',(17.4343438208572,-17.2808977241864,-10.4247632935517));
#83967=CARTESIAN_POINT('Ctrl Pts',(17.4343671095064,-17.2808796123054,-10.4247650761604));
#83968=CARTESIAN_POINT('Ctrl Pts',(17.4343788573469,-17.280870476058,-10.4247659753897));
#83969=CARTESIAN_POINT('Ctrl Pts',(17.434402564613,-17.2808520394157,-10.4247677900471));
#83970=CARTESIAN_POINT('Ctrl Pts',(17.4344145237941,-17.2808427392181,-10.4247687054565));
#83971=CARTESIAN_POINT('Ctrl Pts',(17.4344386581191,-17.2808239712925,-10.4247705528093));
#83972=CARTESIAN_POINT('Ctrl Pts',(17.4344508336627,-17.2808145032613,-10.4247714847833));
#83973=CARTESIAN_POINT('Ctrl Pts',(17.4344754055093,-17.2807953959613,-10.4247733656326));
#83974=CARTESIAN_POINT('Ctrl Pts',(17.4344878019324,-17.2807857566069,-10.4247743145172));
#83975=CARTESIAN_POINT('Ctrl Pts',(17.4345128210006,-17.2807663024365,-10.4247762296059));
#83976=CARTESIAN_POINT('Ctrl Pts',(17.4345254431522,-17.2807564880123,-10.4247771957724));
#83977=CARTESIAN_POINT('Ctrl Pts',(17.4372271946654,-17.2786557752162,-10.4249840025462));
#83978=CARTESIAN_POINT('Ctrl Pts',(17.4399213086497,-17.2765714150477,-10.4251903083905));
#83979=CARTESIAN_POINT('Ctrl Pts',(17.4462368379433,-17.2717095883662,-10.4256741155736));
#83980=CARTESIAN_POINT('Ctrl Pts',(17.4498621993395,-17.2689373342052,-10.425951979191));
#83981=CARTESIAN_POINT('Ctrl Pts',(17.4609904117718,-17.2604846590334,-10.4268052458496));
#83982=CARTESIAN_POINT('Ctrl Pts',(17.4685220801027,-17.2548426156722,-10.4273832307782));
#83983=CARTESIAN_POINT('Ctrl Pts',(17.5765591998817,-17.1750299844123,-10.4356779870282));
#83984=CARTESIAN_POINT('Ctrl Pts',(17.6833880856362,-17.1098547430657,-10.4439142034803));
#83985=CARTESIAN_POINT('Ctrl Pts',(17.8826759478233,-17.0112696685007,-10.4586062915951));
#83986=CARTESIAN_POINT('Ctrl Pts',(17.9729143846822,-16.9741380379784,-10.4650412392758));
#83987=CARTESIAN_POINT('Ctrl Pts',(18.1416604209499,-16.9179686062853,-10.4765055227985));
#83988=CARTESIAN_POINT('Ctrl Pts',(18.2193165345692,-16.8969444210316,-10.4815759029189));
#83989=CARTESIAN_POINT('Ctrl Pts',(18.3170891144227,-16.8763662908325,-10.4877013480118));
#83990=CARTESIAN_POINT('Ctrl Pts',(18.3362445541117,-16.8726105159288,-10.4888895556492));
#83991=CARTESIAN_POINT('Ctrl Pts',(18.3639933366125,-16.8675673497193,-10.4905941701789));
#83992=CARTESIAN_POINT('Ctrl Pts',(18.372546528857,-16.8660671640207,-10.4911173242951));
#83993=CARTESIAN_POINT('Ctrl Pts',(18.3874880658084,-16.8635411573442,-10.4920273312611));
#83994=CARTESIAN_POINT('Ctrl Pts',(18.3938722857777,-16.8624919245277,-10.4924149234685));
#83995=CARTESIAN_POINT('Ctrl Pts',(18.4062270690838,-16.8605195665339,-10.4931626430057));
#83996=CARTESIAN_POINT('Ctrl Pts',(18.4121969636911,-16.859592701026,-10.4935228855141));
#83997=CARTESIAN_POINT('Ctrl Pts',(18.4263967206974,-16.8574503040577,-10.4943772674956));
#83998=CARTESIAN_POINT('Ctrl Pts',(18.4346299808463,-16.8562576969376,-10.4948706781073));
#83999=CARTESIAN_POINT('Ctrl Pts',(18.4639119574695,-16.8521922131341,-10.4966186771941));
#84000=CARTESIAN_POINT('Ctrl Pts',(18.4849970837712,-16.8495876026577,-10.4978648075283));
#84001=CARTESIAN_POINT('Ctrl Pts',(18.6982442863204,-16.8264987417738,-10.5103509151992));
#84002=CARTESIAN_POINT('Ctrl Pts',(18.8923053065221,-16.8320993687426,-10.5206475254935));
#84003=CARTESIAN_POINT('Ctrl Pts',(19.1571395370831,-16.8763546464686,-10.535311059684));
#84004=CARTESIAN_POINT('Ctrl Pts',(19.2306353052451,-16.8927034381921,-10.5394629962477));
#84005=CARTESIAN_POINT('Ctrl Pts',(19.3365015837663,-16.9222503823116,-10.5457590964919));
#84006=CARTESIAN_POINT('Ctrl Pts',(19.3696682606981,-16.9323918157137,-10.5477783634753));
#84007=CARTESIAN_POINT('Ctrl Pts',(19.4095734103534,-16.9456739873161,-10.5502817122309));
#84008=CARTESIAN_POINT('Ctrl Pts',(19.4165657738856,-16.9480420506849,-10.5507231426473));
#84009=CARTESIAN_POINT('Ctrl Pts',(19.427460711142,-16.9517954128764,-10.5514155028952));
#84010=CARTESIAN_POINT('Ctrl Pts',(19.4313719268296,-16.9531556980988,-10.5516649766447));
#84011=CARTESIAN_POINT('Ctrl Pts',(19.4386455321873,-16.9557093388463,-10.5521306772596));
#84012=CARTESIAN_POINT('Ctrl Pts',(19.4420089049835,-16.9568997218985,-10.5523467272029));
#84013=CARTESIAN_POINT('Ctrl Pts',(19.4496413340499,-16.9596227629318,-10.5528386034226));
#84014=CARTESIAN_POINT('Ctrl Pts',(19.4539084644299,-16.9611606353738,-10.5531147359161));
#84015=CARTESIAN_POINT('Ctrl Pts',(19.4668804961102,-16.9658829101426,-10.5539575614396));
#84016=CARTESIAN_POINT('Ctrl Pts',(19.4755693197067,-16.9691107310093,-10.5545267469936));
#84017=CARTESIAN_POINT('Ctrl Pts',(19.5466869728538,-16.9960631127908,-10.5592221120239));
#84018=CARTESIAN_POINT('Ctrl Pts',(19.6079763409848,-17.0226703956028,-10.563499844617));
#84019=CARTESIAN_POINT('Ctrl Pts',(19.7958056823339,-17.1149994914483,-10.5771311150576));
#84020=CARTESIAN_POINT('Ctrl Pts',(19.9170382670057,-17.190629420154,-10.5866767413016));
#84021=CARTESIAN_POINT('Ctrl Pts',(20.1022093346365,-17.3339498669711,-10.6018648834506));
#84022=CARTESIAN_POINT('Ctrl Pts',(20.1709520703969,-17.3946767971232,-10.6076755134377));
#84023=CARTESIAN_POINT('Ctrl Pts',(20.2503104294872,-17.4745257827171,-10.6145874309149));
#84024=CARTESIAN_POINT('Ctrl Pts',(20.2648490943437,-17.4895949668145,-10.6158632641936));
#84025=CARTESIAN_POINT('Ctrl Pts',(20.2852682725264,-17.5113975090061,-10.617669540498));
#84026=CARTESIAN_POINT('Ctrl Pts',(20.2913330592761,-17.5179558804858,-10.6182078991199));
#84027=CARTESIAN_POINT('Ctrl Pts',(20.3017474166265,-17.5293617995574,-10.6191356876734));
#84028=CARTESIAN_POINT('Ctrl Pts',(20.3061164277123,-17.5341913560407,-10.6195259418367));
#84029=CARTESIAN_POINT('Ctrl Pts',(20.3144551459166,-17.5434950103503,-10.6202728057281));
#84030=CARTESIAN_POINT('Ctrl Pts',(20.3184283077977,-17.5479659146936,-10.6206295590185));
#84031=CARTESIAN_POINT('Ctrl Pts',(20.3287454958181,-17.5596751665547,-10.6215583331246));
#84032=CARTESIAN_POINT('Ctrl Pts',(20.3350592468498,-17.5669400984122,-10.6221290883625));
#84033=CARTESIAN_POINT('Ctrl Pts',(20.3565958212548,-17.5920652561579,-10.6240844688312));
#84034=CARTESIAN_POINT('Ctrl Pts',(20.3715714382808,-17.6101357908146,-10.625458948499));
#84035=CARTESIAN_POINT('Ctrl Pts',(20.4912072645767,-17.7594825403026,-10.6365730948589));
#84036=CARTESIAN_POINT('Ctrl Pts',(20.5802124526461,-17.9025326194117,-10.6456351875857));
#84037=CARTESIAN_POINT('Ctrl Pts',(20.7043933598906,-18.1678606626902,-10.6615584261013));
#84038=CARTESIAN_POINT('Ctrl Pts',(20.7472529126862,-18.2855704868649,-10.6683819374743));
#84039=CARTESIAN_POINT('Ctrl Pts',(20.7825424261936,-18.4178607171359,-10.6764615540531));
#84040=CARTESIAN_POINT('Ctrl Pts',(20.7855149006615,-18.4293936059608,-10.6771693176561));
#84041=CARTESIAN_POINT('Ctrl Pts',(20.7896023678436,-18.4458249959643,-10.6781833096697));
#84042=CARTESIAN_POINT('Ctrl Pts',(20.7907975402753,-18.4507035741912,-10.6784850706102));
#84043=CARTESIAN_POINT('Ctrl Pts',(20.7928273553902,-18.4591185503303,-10.6790068518931));
#84044=CARTESIAN_POINT('Ctrl Pts',(20.7936702849524,-18.4626529658149,-10.6792263965169));
#84045=CARTESIAN_POINT('Ctrl Pts',(20.7952870548881,-18.4695102925572,-10.6796531279984));
#84046=CARTESIAN_POINT('Ctrl Pts',(20.7960619635383,-18.472832911623,-10.6798602462165));
#84047=CARTESIAN_POINT('Ctrl Pts',(20.7981311318241,-18.4818029778892,-10.6804203235951));
#84048=CARTESIAN_POINT('Ctrl Pts',(20.7994102334984,-18.4874538402772,-10.6807741385661));
#84049=CARTESIAN_POINT('Ctrl Pts',(20.8040723066368,-18.5084500364147,-10.6820922292244));
#84050=CARTESIAN_POINT('Ctrl Pts',(20.8073074901412,-18.5238272044843,-10.6830644290956));
#84051=CARTESIAN_POINT('Ctrl Pts',(20.8364705749624,-18.6705302663026,-10.6923954376812));
#84052=CARTESIAN_POINT('Ctrl Pts',(20.8500563621851,-18.8039898226102,-10.7012896479728));
#84053=CARTESIAN_POINT('Ctrl Pts',(20.85200493925,-19.0949893046459,-10.7205093060345));
#84054=CARTESIAN_POINT('Ctrl Pts',(20.8355523653503,-19.2518099903764,-10.7307324171897));
#84055=CARTESIAN_POINT('Ctrl Pts',(20.7973240968224,-19.4261680364127,-10.7416955699171));
#84056=CARTESIAN_POINT('Ctrl Pts',(20.7924544485282,-19.4468807841091,-10.7429923041802));
#84057=CARTESIAN_POINT('Ctrl Pts',(20.7850840122204,-19.4762367769593,-10.7448227101385));
#84058=CARTESIAN_POINT('Ctrl Pts',(20.7828392362414,-19.4849424091192,-10.7453645891602));
#84059=CARTESIAN_POINT('Ctrl Pts',(20.778870192563,-19.4999392688035,-10.7462965226963));
#84060=CARTESIAN_POINT('Ctrl Pts',(20.7771721921213,-19.5062372610626,-10.7466874213306));
#84061=CARTESIAN_POINT('Ctrl Pts',(20.7738647143941,-19.5182831212043,-10.7474342079286));
#84062=CARTESIAN_POINT('Ctrl Pts',(20.7722599857531,-19.5240322176176,-10.7477902457368));
#84063=CARTESIAN_POINT('Ctrl Pts',(20.768022622609,-19.5389687456063,-10.7487143097512));
#84064=CARTESIAN_POINT('Ctrl Pts',(20.765352031739,-19.5481453390798,-10.7492810959347));
#84065=CARTESIAN_POINT('Ctrl Pts',(20.7560266021084,-19.5793986564589,-10.7512084953934));
#84066=CARTESIAN_POINT('Ctrl Pts',(20.7490731321349,-19.6013850840226,-10.7525593561758));
#84067=CARTESIAN_POINT('Ctrl Pts',(20.6864103406826,-19.7888132639802,-10.7640423281161));
#84068=CARTESIAN_POINT('Ctrl Pts',(20.6107963541032,-19.94688932184,-10.7734326648572));
#84069=CARTESIAN_POINT('Ctrl Pts',(20.4693507240146,-20.1677007465341,-10.7876988016149));
#84070=CARTESIAN_POINT('Ctrl Pts',(20.4175422226478,-20.238488862108,-10.7924949457549));
#84071=CARTESIAN_POINT('Ctrl Pts',(20.3372095521348,-20.3350585564626,-10.799665664081));
#84072=CARTESIAN_POINT('Ctrl Pts',(20.3121378317858,-20.3635992414914,-10.8018718214812));
#84073=CARTESIAN_POINT('Ctrl Pts',(20.2811592323296,-20.3970068442711,-10.8045824834124));
#84074=CARTESIAN_POINT('Ctrl Pts',(20.275974882188,-20.4025378067928,-10.8050356285985));
#84075=CARTESIAN_POINT('Ctrl Pts',(20.2678831509599,-20.4110781292601,-10.805742364404));
#84076=CARTESIAN_POINT('Ctrl Pts',(20.2649963053727,-20.4141069797807,-10.8059943988872));
#84077=CARTESIAN_POINT('Ctrl Pts',(20.2596342273632,-20.4196995277286,-10.8064623852762));
#84078=CARTESIAN_POINT('Ctrl Pts',(20.257161494037,-20.4222655412884,-10.8066781445864));
#84079=CARTESIAN_POINT('Ctrl Pts',(20.2515672091084,-20.4280416031312,-10.8071661514529));
#84080=CARTESIAN_POINT('Ctrl Pts',(20.248441963686,-20.4312479799241,-10.8074386851726));
#84081=CARTESIAN_POINT('Ctrl Pts',(20.2392187044678,-20.4406508099476,-10.808242655362));
#84082=CARTESIAN_POINT('Ctrl Pts',(20.2330927510674,-20.4468195543203,-10.8087762132711));
#84083=CARTESIAN_POINT('Ctrl Pts',(20.1894856228256,-20.4901936433746,-10.8125701295656));
#84084=CARTESIAN_POINT('Ctrl Pts',(20.1506648572465,-20.5260196174447,-10.8159256372911));
#84085=CARTESIAN_POINT('Ctrl Pts',(20.0984360446275,-20.5707209440942,-10.8203670826831));
#84086=CARTESIAN_POINT('Ctrl Pts',(20.0862062638983,-20.5809510171277,-10.821402165138));
#84087=CARTESIAN_POINT('Ctrl Pts',(19.9575080993183,-20.6861575006348,-10.8322348412543));
#84088=CARTESIAN_POINT('Ctrl Pts',(19.831354046004,-20.7686160568631,-10.8423075176814));
#84089=CARTESIAN_POINT('Ctrl Pts',(19.6427152026762,-20.8650379480273,-10.8559924833463));
#84090=CARTESIAN_POINT('Ctrl Pts',(19.5867096702835,-20.8906502639685,-10.8599069390703));
#84091=CARTESIAN_POINT('Ctrl Pts',(19.4952389926382,-20.9277490093902,-10.8660569255437));
#84092=CARTESIAN_POINT('Ctrl Pts',(19.4604517634608,-20.9408029217722,-10.8683418998437));
#84093=CARTESIAN_POINT('Ctrl Pts',(19.4148238994026,-20.9565676695649,-10.8712714745627));
#84094=CARTESIAN_POINT('Ctrl Pts',(19.4042819849423,-20.9601172256424,-10.8719437311783));
#84095=CARTESIAN_POINT('Ctrl Pts',(19.3870920281101,-20.9657547880979,-10.8730326028818));
#84096=CARTESIAN_POINT('Ctrl Pts',(19.3804608932809,-20.9678933153896,-10.8734508788304));
#84097=CARTESIAN_POINT('Ctrl Pts',(19.367688445844,-20.9719428999078,-10.8742531913098));
#84098=CARTESIAN_POINT('Ctrl Pts',(19.3615487544839,-20.9738587802908,-10.874637382709));
#84099=CARTESIAN_POINT('Ctrl Pts',(19.347471098241,-20.9781813869704,-10.8755149562976));
#84100=CARTESIAN_POINT('Ctrl Pts',(19.3395274966263,-20.9805695095562,-10.8760077247103));
#84101=CARTESIAN_POINT('Ctrl Pts',(19.3183871484546,-20.9867897909643,-10.87731283719));
#84102=CARTESIAN_POINT('Ctrl Pts',(19.3051666407347,-20.9905402901307,-10.8781225199301));
#84103=CARTESIAN_POINT('Ctrl Pts',(19.2041077209126,-21.0181491759718,-10.8842643076848));
#84104=CARTESIAN_POINT('Ctrl Pts',(19.1148437982584,-21.0364506741887,-10.8894106888243));
#84105=CARTESIAN_POINT('Ctrl Pts',(18.8852420271653,-21.0682770240549,-10.9022378076773));
#84106=CARTESIAN_POINT('Ctrl Pts',(18.7442412702683,-21.0736492610361,-10.9097208562789));
#84107=CARTESIAN_POINT('Ctrl Pts',(18.5500364719464,-21.0616784187743,-10.9204806198787));
#84108=CARTESIAN_POINT('Ctrl Pts',(18.4964676334484,-21.0563201251308,-10.9235000316635));
#84109=CARTESIAN_POINT('Ctrl Pts',(18.4154529922025,-21.0450837387864,-10.9282206389264));
#84110=CARTESIAN_POINT('Ctrl Pts',(18.3878213029995,-21.0406914258585,-10.9298583197723));
#84111=CARTESIAN_POINT('Ctrl Pts',(18.3534916153607,-21.0345345188211,-10.931936547882));
#84112=CARTESIAN_POINT('Ctrl Pts',(18.3467030292591,-21.0332827069673,-10.9323496466053));
#84113=CARTESIAN_POINT('Ctrl Pts',(18.3359559927064,-21.0312465587741,-10.933007185181));
#84114=CARTESIAN_POINT('Ctrl Pts',(18.3319933853742,-21.0304840545665,-10.9332503989365));
#84115=CARTESIAN_POINT('Ctrl Pts',(18.3245141947058,-21.0290226840651,-10.9337109442059));
#84116=CARTESIAN_POINT('Ctrl Pts',(18.3209971978838,-21.0283262122265,-10.9339281385505));
#84117=CARTESIAN_POINT('Ctrl Pts',(18.3129476165207,-21.0267108904733,-10.9344266719472));
#84118=CARTESIAN_POINT('Ctrl Pts',(18.3084162667374,-21.0257861205361,-10.9347083455272));
#84119=CARTESIAN_POINT('Ctrl Pts',(18.2963676932262,-21.0232860629597,-10.9354599845175));
#84120=CARTESIAN_POINT('Ctrl Pts',(18.2888560309,-21.0216847183123,-10.9359313794122));
#84121=CARTESIAN_POINT('Ctrl Pts',(18.2355596493348,-21.0100193747706,-10.9392950048503));
#84122=CARTESIAN_POINT('Ctrl Pts',(18.190115148787,-20.998478699073,-10.942262682062));
#84123=CARTESIAN_POINT('Ctrl Pts',(18.1409667008456,-20.9842448129227,-10.9455548968351));
#84124=CARTESIAN_POINT('Ctrl Pts',(18.1368419365551,-20.9830366122723,-10.9458318392832));
#84125=CARTESIAN_POINT('Ctrl Pts',(18.1279297894155,-20.9803966251375,-10.9464315701298));
#84126=CARTESIAN_POINT('Ctrl Pts',(18.1231437445308,-20.978960434628,-10.9467544893002));
#84127=CARTESIAN_POINT('Ctrl Pts',(18.094639858601,-20.9702969009925,-10.9486825761938));
#84128=CARTESIAN_POINT('Ctrl Pts',(18.0710459346062,-20.9626704396908,-10.9502987800727));
#84129=CARTESIAN_POINT('Ctrl Pts',(18.0104709079159,-20.9419081673084,-10.9544925318567));
#84130=CARTESIAN_POINT('Ctrl Pts',(17.9737113750762,-20.9281553479168,-10.9570806034525));
#84131=CARTESIAN_POINT('Ctrl Pts',(17.836096163845,-20.8722611214751,-10.9668924806917));
#84132=CARTESIAN_POINT('Ctrl Pts',(17.7381654037347,-20.8233500470731,-10.9741188246851));
#84133=CARTESIAN_POINT('Ctrl Pts',(17.5972934615871,-20.7387880667882,-10.9846789172014));
#84134=CARTESIAN_POINT('Ctrl Pts',(17.551260073831,-20.708656037397,-10.9881610876758));
#84135=CARTESIAN_POINT('Ctrl Pts',(17.4785408295698,-20.6569001987935,-10.9937088594141));
#84136=CARTESIAN_POINT('Ctrl Pts',(17.4511174735847,-20.6363619133967,-10.9958127306643));
#84137=CARTESIAN_POINT('Ctrl Pts',(17.4157162859835,-20.6084823429287,-10.998545997722));
#84138=CARTESIAN_POINT('Ctrl Pts',(17.4072804169872,-20.6017335717931,-10.9991986653204));
#84139=CARTESIAN_POINT('Ctrl Pts',(17.3935441170201,-20.5905708991804,-11.000263756248));
#84140=CARTESIAN_POINT('Ctrl Pts',(17.3882130199049,-20.5861952061532,-11.000677706756));
#84141=CARTESIAN_POINT('Ctrl Pts',(17.3779321910357,-20.5776724126579,-11.0014771761271));
#84142=CARTESIAN_POINT('Ctrl Pts',(17.3729798695196,-20.5735285694797,-11.0018628208234));
#84143=CARTESIAN_POINT('Ctrl Pts',(17.3615850294236,-20.563904984718,-11.0027514443956));
#84144=CARTESIAN_POINT('Ctrl Pts',(17.3551562068402,-20.558409141051,-11.0032537562283));
#84145=CARTESIAN_POINT('Ctrl Pts',(17.3379467274318,-20.5435177509331,-11.0046011425119));
#84146=CARTESIAN_POINT('Ctrl Pts',(17.3272279300886,-20.5340511526633,-11.0054432701842));
#84147=CARTESIAN_POINT('Ctrl Pts',(17.2292160839547,-20.4457055177877,-11.0131733402474));
#84148=CARTESIAN_POINT('Ctrl Pts',(17.1485394364045,-20.3597822811603,-11.0197398132545));
#84149=CARTESIAN_POINT('Ctrl Pts',(16.9737390657472,-20.1394082055912,-11.0351343331842));
#84150=CARTESIAN_POINT('Ctrl Pts',(16.887280690716,-19.9998894240454,-11.0437794300367));
#84151=CARTESIAN_POINT('Ctrl Pts',(16.8045807977523,-19.8237747371058,-11.0549699554387));
#84152=CARTESIAN_POINT('Ctrl Pts',(16.7920251456033,-19.7954352889854,-11.0567798462889));
#84153=CARTESIAN_POINT('Ctrl Pts',(16.7773512483217,-19.7602484435683,-11.0590503268335));
#84154=CARTESIAN_POINT('Ctrl Pts',(16.7746389829561,-19.7536509749048,-11.0594770317163));
#84155=CARTESIAN_POINT('Ctrl Pts',(16.7704255513855,-19.7432528562106,-11.0601513013589));
#84156=CARTESIAN_POINT('Ctrl Pts',(16.7689019295681,-19.7394612819996,-11.0603975316799));
#84157=CARTESIAN_POINT('Ctrl Pts',(16.7660657190618,-19.7323438027719,-11.0608604760077));
#84158=CARTESIAN_POINT('Ctrl Pts',(16.7647505755928,-19.7290189755786,-11.0610770333961));
#84159=CARTESIAN_POINT('Ctrl Pts',(16.7617562471679,-19.7213925544098,-11.0615744439044));
#84160=CARTESIAN_POINT('Ctrl Pts',(16.7600827142915,-19.7170887998233,-11.061855631285));
#84161=CARTESIAN_POINT('Ctrl Pts',(16.7549425676338,-19.7037409743647,-11.0627291480247));
#84162=CARTESIAN_POINT('Ctrl Pts',(16.7515239884571,-19.6946787115692,-11.0633242370727));
#84163=CARTESIAN_POINT('Ctrl Pts',(16.7472469472791,-19.6831007927047,-11.0640868106714));
#84164=CARTESIAN_POINT('Ctrl Pts',(16.7463308324829,-19.6806064376839,-11.0642512349997));
#84165=CARTESIAN_POINT('Ctrl Pts',(16.745419450227,-19.678110457895,-11.0644158965713));
#84166=CARTESIAN_POINT('',(16.617000600774,-18.9535948907958,-10.0879364327122));
#84167=CARTESIAN_POINT('Ctrl Pts',(16.7454194496957,-19.67811045644,-10.8441190240937));
#84168=CARTESIAN_POINT('Ctrl Pts',(16.7463456800211,-19.6806471002713,-10.843971851373));
#84169=CARTESIAN_POINT('Ctrl Pts',(16.7472767931095,-19.6831820516202,-10.8438247185697));
#84170=CARTESIAN_POINT('Ctrl Pts',(16.8056499896822,-19.8411680552622,-10.8346510169722));
#84171=CARTESIAN_POINT('Ctrl Pts',(16.8811330167863,-19.9893140728775,-10.8258505642691));
#84172=CARTESIAN_POINT('Ctrl Pts',(16.9808578145588,-20.1387506075834,-10.8152891817525));
#84173=CARTESIAN_POINT('Ctrl Pts',(16.9887344675016,-20.1503041036104,-10.81446052175));
#84174=CARTESIAN_POINT('Ctrl Pts',(16.9998805544108,-20.1663101930112,-10.8132942201619));
#84175=CARTESIAN_POINT('Ctrl Pts',(17.0030540337989,-20.1708295848692,-10.8129628507967));
#84176=CARTESIAN_POINT('Ctrl Pts',(17.0081863136465,-20.1780780581372,-10.8124279704154));
#84177=CARTESIAN_POINT('Ctrl Pts',(17.0101340155851,-20.1808150194652,-10.8122252173516));
#84178=CARTESIAN_POINT('Ctrl Pts',(17.0142251835164,-20.1865351653663,-10.8117997947541));
#84179=CARTESIAN_POINT('Ctrl Pts',(17.0163699018095,-20.1895174095777,-10.8115770358813));
#84180=CARTESIAN_POINT('Ctrl Pts',(17.0215923838734,-20.1967395736061,-10.8110352681897));
#84181=CARTESIAN_POINT('Ctrl Pts',(17.0246781358097,-20.2009736639017,-10.8107157114476));
#84182=CARTESIAN_POINT('Ctrl Pts',(17.0356087281591,-20.215855611602,-10.8095858154991));
#84183=CARTESIAN_POINT('Ctrl Pts',(17.0435374145915,-20.2264411113385,-10.8087699389654));
#84184=CARTESIAN_POINT('Ctrl Pts',(17.0915651139364,-20.2893255989126,-10.8038531908166));
#84185=CARTESIAN_POINT('Ctrl Pts',(17.1339858546124,-20.3397986782992,-10.7996154560109));
#84186=CARTESIAN_POINT('Ctrl Pts',(17.2439182575073,-20.4588479826325,-10.7890378176297));
#84187=CARTESIAN_POINT('Ctrl Pts',(17.3138862660322,-20.5249625715988,-10.782642147312));
#84188=CARTESIAN_POINT('Ctrl Pts',(17.4967378907325,-20.6755654973935,-10.7670586086159));
#84189=CARTESIAN_POINT('Ctrl Pts',(17.6140381141675,-20.7539972808021,-10.75801007058));
#84190=CARTESIAN_POINT('Ctrl Pts',(17.7508859013276,-20.826934621051,-10.7485414219303));
#84191=CARTESIAN_POINT('Ctrl Pts',(17.7635632873743,-20.8335275088946,-10.7476734914909));
#84192=CARTESIAN_POINT('Ctrl Pts',(17.7838464468635,-20.8438162438814,-10.7462992412623));
#84193=CARTESIAN_POINT('Ctrl Pts',(17.7914091200073,-20.8475956613542,-10.7457899937914));
#84194=CARTESIAN_POINT('Ctrl Pts',(17.8047871228581,-20.8541814103034,-10.7448946309647));
#84195=CARTESIAN_POINT('Ctrl Pts',(17.8105929931825,-20.8570066115222,-10.744507859552));
#84196=CARTESIAN_POINT('Ctrl Pts',(17.8226282410899,-20.8627951490027,-10.7437097879834));
#84197=CARTESIAN_POINT('Ctrl Pts',(17.8288593661852,-20.8657546914745,-10.7432986232449));
#84198=CARTESIAN_POINT('Ctrl Pts',(17.8448911678738,-20.8732733590284,-10.7422458852346));
#84199=CARTESIAN_POINT('Ctrl Pts',(17.8547125738495,-20.8777880112437,-10.7416058534271));
#84200=CARTESIAN_POINT('Ctrl Pts',(17.8958499548665,-20.8963175099897,-10.738944964163));
#84201=CARTESIAN_POINT('Ctrl Pts',(17.9274707408071,-20.9096457362182,-10.7369476405012));
#84202=CARTESIAN_POINT('Ctrl Pts',(18.0106938037344,-20.9423654298589,-10.731802945253));
#84203=CARTESIAN_POINT('Ctrl Pts',(18.0627549184162,-20.9605211186356,-10.7286949750687));
#84204=CARTESIAN_POINT('Ctrl Pts',(18.2200494114054,-21.008575261138,-10.7195498472431));
#84205=CARTESIAN_POINT('Ctrl Pts',(18.3269517750913,-21.0323748791323,-10.7136614166043));
#84206=CARTESIAN_POINT('Ctrl Pts',(18.4810888454796,-21.0543492181285,-10.7051846664263));
#84207=CARTESIAN_POINT('Ctrl Pts',(18.5271649116022,-21.0593811436068,-10.7026508060785));
#84208=CARTESIAN_POINT('Ctrl Pts',(18.5947027529102,-21.064520557752,-10.6988935424562));
#84209=CARTESIAN_POINT('Ctrl Pts',(18.6160609289931,-21.0658205133526,-10.69769902599));
#84210=CARTESIAN_POINT('Ctrl Pts',(18.6892331614252,-21.0691616880528,-10.693574458071));
#84211=CARTESIAN_POINT('Ctrl Pts',(18.7410966719304,-21.069622812678,-10.6905959184217));
#84212=CARTESIAN_POINT('Ctrl Pts',(18.8015718440414,-21.0679390251815,-10.6870052830929));
#84213=CARTESIAN_POINT('Ctrl Pts',(18.8102219599894,-21.067645083519,-10.6864888811617));
#84214=CARTESIAN_POINT('Ctrl Pts',(18.8233354723751,-21.0671189439723,-10.6857014274819));
#84215=CARTESIAN_POINT('Ctrl Pts',(18.8278004568098,-21.0669256363369,-10.6854325017877));
#84216=CARTESIAN_POINT('Ctrl Pts',(18.8358239962299,-21.0665528060063,-10.6849477394157));
#84217=CARTESIAN_POINT('Ctrl Pts',(18.8393827362904,-21.066378436842,-10.6847321940829));
#84218=CARTESIAN_POINT('Ctrl Pts',(18.8471262713922,-21.0659794249753,-10.6842620089058));
#84219=CARTESIAN_POINT('Ctrl Pts',(18.8513107909387,-21.0657513430214,-10.6840071838548));
#84220=CARTESIAN_POINT('Ctrl Pts',(18.8630928885763,-21.0650740525226,-10.6832876506464));
#84221=CARTESIAN_POINT('Ctrl Pts',(18.8706886711193,-21.0645963004026,-10.6828213887988));
#84222=CARTESIAN_POINT('Ctrl Pts',(18.9167087806202,-21.0614525456349,-10.6799826793448));
#84223=CARTESIAN_POINT('Ctrl Pts',(18.9550544817785,-21.0577794342677,-10.6775591194044));
#84224=CARTESIAN_POINT('Ctrl Pts',(19.0823758889858,-21.0420676956464,-10.6693637562636));
#84225=CARTESIAN_POINT('Ctrl Pts',(19.1706810236437,-21.0254166085174,-10.6634408191298));
#84226=CARTESIAN_POINT('Ctrl Pts',(19.4238618436034,-20.9607817782371,-10.6461738940246));
#84227=CARTESIAN_POINT('Ctrl Pts',(19.5843274020447,-20.8982987635037,-10.6349279584136));
#84228=CARTESIAN_POINT('Ctrl Pts',(19.7560011913052,-20.806115288656,-10.6229309460918));
#84229=CARTESIAN_POINT('Ctrl Pts',(19.7763099133725,-20.7947750950297,-10.6215108768762));
#84230=CARTESIAN_POINT('Ctrl Pts',(19.8047233092177,-20.7782892887542,-10.6195221811033));
#84231=CARTESIAN_POINT('Ctrl Pts',(19.8129856342374,-20.7734200440766,-10.6189436521902));
#84232=CARTESIAN_POINT('Ctrl Pts',(19.8263413820472,-20.7654263159396,-10.6180080118978));
#84233=CARTESIAN_POINT('Ctrl Pts',(19.8314550974713,-20.7623361589624,-10.6176496563862));
#84234=CARTESIAN_POINT('Ctrl Pts',(19.8421196515338,-20.7558299026823,-10.6169020462657));
#84235=CARTESIAN_POINT('Ctrl Pts',(19.8476679415611,-20.7524097304032,-10.6165129460599));
#84236=CARTESIAN_POINT('Ctrl Pts',(19.8608074056511,-20.744226097483,-10.6155910674706));
#84237=CARTESIAN_POINT('Ctrl Pts',(19.8683843405866,-20.7394399250109,-10.6150591337573));
#84238=CARTESIAN_POINT('Ctrl Pts',(19.8937052192919,-20.7232194622086,-10.6132801928249));
#84239=CARTESIAN_POINT('Ctrl Pts',(19.9113088502268,-20.7115677019112,-10.6120412819522));
#84240=CARTESIAN_POINT('Ctrl Pts',(20.0055364049833,-20.6471516274508,-10.6053929064818));
#84241=CARTESIAN_POINT('Ctrl Pts',(20.0787974964785,-20.5896405171448,-10.600169027024));
#84242=CARTESIAN_POINT('Ctrl Pts',(20.2631896580524,-20.4241436645837,-10.5865244081878));
#84243=CARTESIAN_POINT('Ctrl Pts',(20.3666490248463,-20.3084950083429,-10.5783424624455));
#84244=CARTESIAN_POINT('Ctrl Pts',(20.4877603804611,-20.1389672088419,-10.5666285142275));
#84245=CARTESIAN_POINT('Ctrl Pts',(20.5172703927468,-20.0941524849342,-10.5635510937905));
#84246=CARTESIAN_POINT('Ctrl Pts',(20.5495710881144,-20.0407915516664,-10.5598496972577));
#84247=CARTESIAN_POINT('Ctrl Pts',(20.5540514973316,-20.0332853277824,-10.5593281942504));
#84248=CARTESIAN_POINT('Ctrl Pts',(20.5607614694286,-20.0218839538951,-10.5585344814504));
#84249=CARTESIAN_POINT('Ctrl Pts',(20.5630254087612,-20.018009002891,-10.5582644487195));
#84250=CARTESIAN_POINT('Ctrl Pts',(20.5670652343483,-20.011043696335,-10.557778511095));
#84251=CARTESIAN_POINT('Ctrl Pts',(20.5688456514959,-20.0079560308161,-10.5575629038588));
#84252=CARTESIAN_POINT('Ctrl Pts',(20.5726953256614,-20.0012406497307,-10.5570935438061));
#84253=CARTESIAN_POINT('Ctrl Pts',(20.5747616206543,-19.9976113507834,-10.5568396110304));
#84254=CARTESIAN_POINT('Ctrl Pts',(20.5805304195922,-19.9874087726088,-10.5561250606686));
#84255=CARTESIAN_POINT('Ctrl Pts',(20.5842085011695,-19.9808218578252,-10.555662922932));
#84256=CARTESIAN_POINT('Ctrl Pts',(20.6058848281407,-19.941510495461,-10.5529006498017));
#84257=CARTESIAN_POINT('Ctrl Pts',(20.62304856624,-19.9083362113267,-10.5505524815628));
#84258=CARTESIAN_POINT('Ctrl Pts',(20.6764341811795,-19.798101182503,-10.5427357876341));
#84259=CARTESIAN_POINT('Ctrl Pts',(20.7088849599637,-19.7193104245221,-10.5371299076634));
#84260=CARTESIAN_POINT('Ctrl Pts',(20.7942907005149,-19.4702879052617,-10.5197385422854));
#84261=CARTESIAN_POINT('Ctrl Pts',(20.8305934425447,-19.2951334505474,-10.5080322030861));
#84262=CARTESIAN_POINT('Ctrl Pts',(20.846303571535,-19.094764425315,-10.4956637956596));
#84263=CARTESIAN_POINT('Ctrl Pts',(20.8477177020219,-19.0720233280426,-10.494273165356));
#84264=CARTESIAN_POINT('Ctrl Pts',(20.849201512472,-19.0397612553451,-10.4923182409659));
#84265=CARTESIAN_POINT('Ctrl Pts',(20.8495744870978,-19.0302564403979,-10.4917444932049));
#84266=CARTESIAN_POINT('Ctrl Pts',(20.8500769629108,-19.0147918458448,-10.4908144815772));
#84267=CARTESIAN_POINT('Ctrl Pts',(20.8502453729272,-19.008833542559,-10.4904570029324));
#84268=CARTESIAN_POINT('Ctrl Pts',(20.8505455421904,-18.9963464602995,-10.4897095543487));
#84269=CARTESIAN_POINT('Ctrl Pts',(20.8506722633026,-18.9898176142333,-10.4893197461409));
#84270=CARTESIAN_POINT('Ctrl Pts',(20.8509022301395,-18.9742594753132,-10.4883931576885));
#84271=CARTESIAN_POINT('Ctrl Pts',(20.8509779193418,-18.965229855517,-10.4878572456708));
#84272=CARTESIAN_POINT('Ctrl Pts',(20.8510385074532,-18.934690040024,-10.4860507794607));
#84273=CARTESIAN_POINT('Ctrl Pts',(20.8507533513592,-18.9131802055577,-10.4847886732546));
#84274=CARTESIAN_POINT('Ctrl Pts',(20.8450116479682,-18.7117574967599,-10.4730565259586));
#84275=CARTESIAN_POINT('Ctrl Pts',(20.8169604240109,-18.5332286439743,-10.4633886770937));
#84276=CARTESIAN_POINT('Ctrl Pts',(20.7331466816762,-18.2452622428535,-10.4470646166408));
#84277=CARTESIAN_POINT('Ctrl Pts',(20.6899232829007,-18.1332073185101,-10.4404840010678));
#84278=CARTESIAN_POINT('Ctrl Pts',(20.6332945078128,-18.0168743813086,-10.4328161849434));
#84279=CARTESIAN_POINT('Ctrl Pts',(20.6290720821249,-18.0083468083841,-10.432248994846));
#84280=CARTESIAN_POINT('Ctrl Pts',(20.6227304272447,-17.9957534881795,-10.4314033536339));
#84281=CARTESIAN_POINT('Ctrl Pts',(20.6206551817095,-17.9916655569072,-10.4311275871715));
#84282=CARTESIAN_POINT('Ctrl Pts',(20.6169393466316,-17.9844044348876,-10.4306354555728));
#84283=CARTESIAN_POINT('Ctrl Pts',(20.6153039880556,-17.9812286237139,-10.4304194206636));
#84284=CARTESIAN_POINT('Ctrl Pts',(20.6117708027984,-17.9744097559684,-10.4299538490456));
#84285=CARTESIAN_POINT('Ctrl Pts',(20.6098704367621,-17.9707681329637,-10.4297041576473));
#84286=CARTESIAN_POINT('Ctrl Pts',(20.6045957604759,-17.9607317313824,-10.4290131415603));
#84287=CARTESIAN_POINT('Ctrl Pts',(20.6011993056273,-17.9543487437641,-10.4285704506624));
#84288=CARTESIAN_POINT('Ctrl Pts',(20.5824161322064,-17.9194812725726,-10.426135084562));
#84289=CARTESIAN_POINT('Ctrl Pts',(20.5664111408816,-17.891336874562,-10.4241064343963));
#84290=CARTESIAN_POINT('Ctrl Pts',(20.4660460361725,-17.7239028978663,-10.4117039053007));
#84291=CARTESIAN_POINT('Ctrl Pts',(20.3664914526004,-17.594363255682,-10.4007374961109));
#84292=CARTESIAN_POINT('Ctrl Pts',(20.1716622478777,-17.3936422461894,-10.3824656027845));
#84293=CARTESIAN_POINT('Ctrl Pts',(20.0834341901537,-17.3166447432572,-10.3750198855405));
#84294=CARTESIAN_POINT('Ctrl Pts',(19.9777935127396,-17.2388536621923,-10.3670094790559));
#84295=CARTESIAN_POINT('Ctrl Pts',(19.966216060809,-17.2305075451167,-10.3661425986559));
#84296=CARTESIAN_POINT('Ctrl Pts',(19.9476512198721,-17.2174075095098,-10.3647696915688));
#84297=CARTESIAN_POINT('Ctrl Pts',(19.9407183925265,-17.2125773613254,-10.3642607460972));
#84298=CARTESIAN_POINT('Ctrl Pts',(19.9284377145922,-17.2041300894364,-10.3633657344842));
#84299=CARTESIAN_POINT('Ctrl Pts',(19.9231019223148,-17.2004957042379,-10.362979013906));
#84300=CARTESIAN_POINT('Ctrl Pts',(19.9120289162187,-17.1930274349134,-10.3621808749664));
#84301=CARTESIAN_POINT('Ctrl Pts',(19.9062894096267,-17.1891970745472,-10.3617695928719));
#84302=CARTESIAN_POINT('Ctrl Pts',(19.8915035832794,-17.1794336434102,-10.3607161975162));
#84303=CARTESIAN_POINT('Ctrl Pts',(19.8824302564333,-17.1735416826635,-10.3600756294999));
#84304=CARTESIAN_POINT('Ctrl Pts',(19.8443282302194,-17.1492124946661,-10.3574095230887));
#84305=CARTESIAN_POINT('Ctrl Pts',(19.8148966791519,-17.1314137935271,-10.3554076364386));
#84306=CARTESIAN_POINT('Ctrl Pts',(19.7370493198039,-17.0868892843295,-10.3502485244327));
#84307=CARTESIAN_POINT('Ctrl Pts',(19.6879962624945,-17.0613287695323,-10.3471309907069));
#84308=CARTESIAN_POINT('Ctrl Pts',(19.4673567208315,-16.9571345621667,-10.333565480744));
#84309=CARTESIAN_POINT('Ctrl Pts',(19.2867325213103,-16.8997395542983,-10.323717755979));
#84310=CARTESIAN_POINT('Ctrl Pts',(19.0604234464957,-16.8599132088181,-10.3106505323397));
#84311=CARTESIAN_POINT('Ctrl Pts',(19.0197350572528,-16.8539689264304,-10.308270138831));
#84312=CARTESIAN_POINT('Ctrl Pts',(18.9715618323872,-16.8483583972142,-10.3053884392312));
#84313=CARTESIAN_POINT('Ctrl Pts',(18.9642168017775,-16.8475419135218,-10.3049473304845));
#84314=CARTESIAN_POINT('Ctrl Pts',(18.9523055510701,-16.8462809462173,-10.3042289718892));
#84315=CARTESIAN_POINT('Ctrl Pts',(18.9477418248774,-16.8458128101993,-10.3039530184238));
#84316=CARTESIAN_POINT('Ctrl Pts',(18.939621626224,-16.8450065235706,-10.3034606820463));
#84317=CARTESIAN_POINT('Ctrl Pts',(18.9360657836174,-16.8446625372875,-10.3032446304212));
#84318=CARTESIAN_POINT('Ctrl Pts',(18.9284215214995,-16.8439425700486,-10.3027791697893));
#84319=CARTESIAN_POINT('Ctrl Pts',(18.9243329342682,-16.8435694866877,-10.3025296068684));
#84320=CARTESIAN_POINT('Ctrl Pts',(18.9130503213187,-16.8425730338913,-10.3018393000788));
#84321=CARTESIAN_POINT('Ctrl Pts',(18.9058542301965,-16.8419745823775,-10.3013971945268));
#84322=CARTESIAN_POINT('Ctrl Pts',(18.8665155855769,-16.8389056173192,-10.2989708999703));
#84323=CARTESIAN_POINT('Ctrl Pts',(18.8343247265084,-16.8371328794595,-10.296951044929));
#84324=CARTESIAN_POINT('Ctrl Pts',(18.6392355953626,-16.8308532261554,-10.2845514364748));
#84325=CARTESIAN_POINT('Ctrl Pts',(18.4763071486216,-16.8444331058325,-10.2735769198782));
#84326=CARTESIAN_POINT('Ctrl Pts',(18.201972448026,-16.8996123972514,-10.2552981298976));
#84327=CARTESIAN_POINT('Ctrl Pts',(18.0894856773053,-16.9321095838726,-10.2478531342966));
#84328=CARTESIAN_POINT('Ctrl Pts',(17.9668770166934,-16.9788259451453,-10.239841513944));
#84329=CARTESIAN_POINT('Ctrl Pts',(17.9535647796046,-16.9840532515357,-10.2389728125279));
#84330=CARTESIAN_POINT('Ctrl Pts',(17.93246527165,-16.9925861550501,-10.2375975762118));
#84331=CARTESIAN_POINT('Ctrl Pts',(17.9246432569934,-16.9958041503149,-10.2370881070898));
#84332=CARTESIAN_POINT('Ctrl Pts',(17.910883813538,-17.0015614749432,-10.2361924864194));
#84333=CARTESIAN_POINT('Ctrl Pts',(17.904938363605,-17.0040812386209,-10.2358056776252));
#84334=CARTESIAN_POINT('Ctrl Pts',(17.893529214847,-17.0089782912008,-10.2350637299531));
#84335=CARTESIAN_POINT('Ctrl Pts',(17.8880638490885,-17.0113515178532,-10.2347084573019));
#84336=CARTESIAN_POINT('Ctrl Pts',(17.8736594437266,-17.0176787583741,-10.2337724496465));
#84337=CARTESIAN_POINT('Ctrl Pts',(17.8647375755608,-17.0216716909042,-10.2331930501737));
#84338=CARTESIAN_POINT('Ctrl Pts',(17.8316970723038,-17.0367343119883,-10.2310483576716));
#84339=CARTESIAN_POINT('Ctrl Pts',(17.8077589493055,-17.0481956933715,-10.2294965538034));
#84340=CARTESIAN_POINT('Ctrl Pts',(17.7489355835763,-17.0777320697137,-10.2256835427367));
#84341=CARTESIAN_POINT('Ctrl Pts',(17.7143254322945,-17.0963340230601,-10.2234404015519));
#84342=CARTESIAN_POINT('Ctrl Pts',(17.5863677572753,-17.1697692514696,-10.2151165562411));
#84343=CARTESIAN_POINT('Ctrl Pts',(17.4967503337795,-17.2307732200334,-10.2092331185111));
#84344=CARTESIAN_POINT('Ctrl Pts',(17.305801030502,-17.3834060554229,-10.1959580002686));
#84345=CARTESIAN_POINT('Ctrl Pts',(17.2078821415528,-17.478503047627,-10.1886008824204));
#84346=CARTESIAN_POINT('Ctrl Pts',(17.1096885973165,-17.5942278921786,-10.1797012658975));
#84347=CARTESIAN_POINT('Ctrl Pts',(17.0997222590636,-17.6062404140771,-10.178777868324));
#84348=CARTESIAN_POINT('Ctrl Pts',(17.0862501024277,-17.6228488952362,-10.1774999990982));
#84349=CARTESIAN_POINT('Ctrl Pts',(17.0826286489866,-17.6273509734594,-10.1771534885434));
#84350=CARTESIAN_POINT('Ctrl Pts',(17.076900114816,-17.6345325090898,-10.1766004609545));
#84351=CARTESIAN_POINT('Ctrl Pts',(17.0747809665971,-17.6372023661811,-10.1763948008226));
#84352=CARTESIAN_POINT('Ctrl Pts',(17.0704149452737,-17.642730362687,-10.1759688203684));
#84353=CARTESIAN_POINT('Ctrl Pts',(17.0681689900703,-17.6455891675752,-10.1757484351316));
#84354=CARTESIAN_POINT('Ctrl Pts',(17.0628305414498,-17.65242045828,-10.1752216228868));
#84355=CARTESIAN_POINT('Ctrl Pts',(17.0597448423315,-17.6563982053628,-10.1749147191133));
#84356=CARTESIAN_POINT('Ctrl Pts',(17.0493660199558,-17.669876447815,-10.173874407744));
#84357=CARTESIAN_POINT('Ctrl Pts',(17.0421394977139,-17.6794276148764,-10.1731365460881));
#84358=CARTESIAN_POINT('Ctrl Pts',(16.9597945784962,-17.7902026100249,-10.1645761939436));
#84359=CARTESIAN_POINT('Ctrl Pts',(16.8937878918033,-17.8978696484181,-10.1562461149533));
#84360=CARTESIAN_POINT('Ctrl Pts',(16.8040458319401,-18.0786648961684,-10.1429073852356));
#84361=CARTESIAN_POINT('Ctrl Pts',(16.774007504723,-18.1483410710766,-10.1379034961777));
#84362=CARTESIAN_POINT('Ctrl Pts',(16.7335752732272,-18.2579732852734,-10.1303131054882));
#84363=CARTESIAN_POINT('Ctrl Pts',(16.7205007736768,-18.2968715188803,-10.127672050771));
#84364=CARTESIAN_POINT('Ctrl Pts',(16.7056936910043,-18.3455679011222,-10.1244341607967));
#84365=CARTESIAN_POINT('Ctrl Pts',(16.7028889806927,-18.3550289742907,-10.1238082280434));
#84366=CARTESIAN_POINT('Ctrl Pts',(16.6846210484773,-18.4182712229377,-10.119645304547));
#84367=CARTESIAN_POINT('Ctrl Pts',(16.6712283446651,-18.472631128594,-10.116169486635));
#84368=CARTESIAN_POINT('Ctrl Pts',(16.6575926819898,-18.5392454571761,-10.1120304203273));
#84369=CARTESIAN_POINT('Ctrl Pts',(16.6552811241882,-18.5510492453933,-10.1113014880045));
#84370=CARTESIAN_POINT('Ctrl Pts',(16.6516247783754,-18.570602205829,-10.1101012830394));
#84371=CARTESIAN_POINT('Ctrl Pts',(16.650222373548,-18.5783401986623,-10.109628183187));
#84372=CARTESIAN_POINT('Ctrl Pts',(16.6477625455389,-18.5923573635147,-10.1087745113515));
#84373=CARTESIAN_POINT('Ctrl Pts',(16.6466902780684,-18.5986338039992,-10.1083934713747));
#84374=CARTESIAN_POINT('Ctrl Pts',(16.6446635347929,-18.6108283881455,-10.1076554498014));
#84375=CARTESIAN_POINT('Ctrl Pts',(16.6437058477124,-18.6167459297388,-10.1072983696492));
#84376=CARTESIAN_POINT('Ctrl Pts',(16.6416603183947,-18.6297348257842,-10.1065168546868));
#84377=CARTESIAN_POINT('Ctrl Pts',(16.6405831593277,-18.6368078065209,-10.1060927609098));
#84378=CARTESIAN_POINT('Ctrl Pts',(16.6380227876596,-18.654212385253,-10.1050527299054));
#84379=CARTESIAN_POINT('Ctrl Pts',(16.6365800759984,-18.6645498193423,-10.1044380685977));
#84380=CARTESIAN_POINT('Ctrl Pts',(16.6230153914468,-18.7672893702876,-10.0983585237394));
#84381=CARTESIAN_POINT('Ctrl Pts',(16.6169303822883,-18.8603894548246,-10.0930911632084));
#84382=CARTESIAN_POINT('Ctrl Pts',(16.617000600774,-18.9535948907958,-10.0879364327122));
#84383=CARTESIAN_POINT('Ctrl Pts',(16.617000598892,-18.9535923908226,-10.0879365709734));
#84384=CARTESIAN_POINT('Ctrl Pts',(16.6171096392611,-19.0985557959938,-10.0799193607352));
#84385=CARTESIAN_POINT('Ctrl Pts',(16.6321076022928,-19.2431231720195,-10.0722250138809));
#84386=CARTESIAN_POINT('Ctrl Pts',(16.6753573988837,-19.4500950284509,-10.0604951744654));
#84387=CARTESIAN_POINT('Ctrl Pts',(16.6920108411014,-19.5144825012199,-10.056735958022));
#84388=CARTESIAN_POINT('Ctrl Pts',(16.7155915269103,-19.5906648131193,-10.0520405658893));
#84389=CARTESIAN_POINT('Ctrl Pts',(16.7196392101853,-19.6033187361381,-10.0512522809237));
#84390=CARTESIAN_POINT('Ctrl Pts',(16.7254517172716,-19.6209172932602,-10.0501431585338));
#84391=CARTESIAN_POINT('Ctrl Pts',(16.7271163361503,-19.6258950272122,-10.0498280068219));
#84392=CARTESIAN_POINT('Ctrl Pts',(16.7299779737093,-19.6343475839671,-10.0492903272845));
#84393=CARTESIAN_POINT('Ctrl Pts',(16.7311655755179,-19.6378256156405,-10.0490683541719));
#84394=CARTESIAN_POINT('Ctrl Pts',(16.7334553551712,-19.6444748336374,-10.0486425620907));
#84395=CARTESIAN_POINT('Ctrl Pts',(16.7345560270915,-19.6476465122525,-10.0484388371499));
#84396=CARTESIAN_POINT('Ctrl Pts',(16.7374836519418,-19.6560183603001,-10.0478994731463));
#84397=CARTESIAN_POINT('Ctrl Pts',(16.7393233626526,-19.6612139948961,-10.0475630863369));
#84398=CARTESIAN_POINT('Ctrl Pts',(16.7425839020076,-19.6703092302424,-10.0469713956746));
#84399=CARTESIAN_POINT('Ctrl Pts',(16.743995952389,-19.6742119599656,-10.0467165876099));
#84400=CARTESIAN_POINT('Ctrl Pts',(16.7454194499602,-19.6781104571642,-10.0464611570501));
#84401=CARTESIAN_POINT('Origin',(18.734,-18.952,0.));
#84402=CARTESIAN_POINT('',(16.7454193049359,-19.6781100599899,-9.24346979696294));
#84403=CARTESIAN_POINT('',(16.7454194499637,-19.6781104571739,-9.46634969428706));
#84404=CARTESIAN_POINT('',(16.7454194499637,-19.6781104571739,0.));
#84405=CARTESIAN_POINT('',(16.6163914686439,-18.9501065431989,-9.51094371951101));
#84406=CARTESIAN_POINT('Ctrl Pts',(16.7454194499637,-19.6781104571739,-9.46634969428706));
#84407=CARTESIAN_POINT('Ctrl Pts',(16.720738363517,-19.6105169829623,-9.47066127906487));
#84408=CARTESIAN_POINT('Ctrl Pts',(16.6995057447712,-19.5416582823502,-9.47497286384268));
#84409=CARTESIAN_POINT('Ctrl Pts',(16.6818386273343,-19.4719256682822,-9.4792844486205));
#84410=CARTESIAN_POINT('Ctrl Pts',(16.6641689582128,-19.4021829826427,-9.48359665612607));
#84411=CARTESIAN_POINT('Ctrl Pts',(16.6500659224548,-19.3315666185462,-9.48790886363164));
#84412=CARTESIAN_POINT('Ctrl Pts',(16.6395956396387,-19.2604791326809,-9.49222107113721));
#84413=CARTESIAN_POINT('Ctrl Pts',(16.6291143284222,-19.1893167700171,-9.49653782071216));
#84414=CARTESIAN_POINT('Ctrl Pts',(16.6222734602416,-19.1176827900521,-9.5008545702871));
#84415=CARTESIAN_POINT('Ctrl Pts',(16.6190872658347,-19.045984716126,-9.50517131986205));
#84416=CARTESIAN_POINT('Ctrl Pts',(16.6176670680628,-19.0140263884681,-9.50709544543166));
#84417=CARTESIAN_POINT('Ctrl Pts',(16.6169722855429,-18.9820553302898,-9.50901957100126));
#84418=CARTESIAN_POINT('Ctrl Pts',(16.6170008459316,-18.9501074689745,-9.51094369657087));
#84419=CARTESIAN_POINT('Ctrl Pts',(16.6163525130807,-18.950106484017,-9.51094372097751));
#84420=CARTESIAN_POINT('Ctrl Pts',(16.6150298054201,-18.8071177642836,-9.51955279572482));
#84421=CARTESIAN_POINT('Ctrl Pts',(16.6934794852886,-17.9614815818345,-9.57055380603263));
#84422=CARTESIAN_POINT('Ctrl Pts',(17.8308508267527,-16.6173368175504,-9.66394675190085));
#84423=CARTESIAN_POINT('Ctrl Pts',(20.2082247500812,-16.9288855714837,-9.79112255858234));
#84424=CARTESIAN_POINT('Ctrl Pts',(21.2330889659179,-19.0965162449378,-9.91829836526374));
#84425=CARTESIAN_POINT('Ctrl Pts',(19.9651941664791,-21.1315622333511,-10.0454741719452));
#84426=CARTESIAN_POINT('Ctrl Pts',(17.7787242232772,-21.1638771367373,-10.1614588019006));
#84427=CARTESIAN_POINT('Ctrl Pts',(16.9288259160256,-20.1636739641463,-10.2350514962957));
#84428=CARTESIAN_POINT('Ctrl Pts',(16.7460269997163,-19.6778790908883,-10.2662522551303));
#84429=CARTESIAN_POINT('Ctrl Pts',(16.7454194499602,-19.6781104571642,-10.0464611570501));
#84430=CARTESIAN_POINT('Ctrl Pts',(16.7487705800937,-19.6872881134538,-10.0458598346008));
#84431=CARTESIAN_POINT('Ctrl Pts',(16.7521851509511,-19.6964423129619,-10.0452550625254));
#84432=CARTESIAN_POINT('Ctrl Pts',(16.8148899433013,-19.8610598294149,-10.0342936653091));
#84433=CARTESIAN_POINT('Ctrl Pts',(16.8922364625482,-20.0090121106089,-10.0231059329381));
#84434=CARTESIAN_POINT('Ctrl Pts',(17.0314061086661,-20.2126792326606,-10.0069007354659));
#84435=CARTESIAN_POINT('Ctrl Pts',(17.0804528128878,-20.2763571406402,-10.0016885341233));
#84436=CARTESIAN_POINT('Ctrl Pts',(17.1587312159261,-20.3668369246799,-9.99410804453697));
#84437=CARTESIAN_POINT('Ctrl Pts',(17.1852837348339,-20.3958537006746,-9.99164686094173));
#84438=CARTESIAN_POINT('Ctrl Pts',(17.2310837946067,-20.4431861352719,-9.98758039807538));
#84439=CARTESIAN_POINT('Ctrl Pts',(17.2498945865422,-20.4619087497938,-9.98595738198995));
#84440=CARTESIAN_POINT('Ctrl Pts',(17.2761201267121,-20.4870475910786,-9.98375697301453));
#84441=CARTESIAN_POINT('Ctrl Pts',(17.2832341192949,-20.4937727446786,-9.98316616620807));
#84442=CARTESIAN_POINT('Ctrl Pts',(17.2947526968862,-20.5045114175436,-9.98221919500483));
#84443=CARTESIAN_POINT('Ctrl Pts',(17.2991279619979,-20.5085560500066,-9.9818616964551));
#84444=CARTESIAN_POINT('Ctrl Pts',(17.308279409707,-20.5169445606849,-9.98111848350948));
#84445=CARTESIAN_POINT('Ctrl Pts',(17.3130585100684,-20.5212851758742,-9.98073291007807));
#84446=CARTESIAN_POINT('Ctrl Pts',(17.3241384488046,-20.5312564099933,-9.97984480770873));
#84447=CARTESIAN_POINT('Ctrl Pts',(17.3304533192749,-20.5368713260791,-9.97934294330554));
#84448=CARTESIAN_POINT('Ctrl Pts',(17.3475251730836,-20.551868836075,-9.97799754901092));
#84449=CARTESIAN_POINT('Ctrl Pts',(17.358343826291,-20.5611807993244,-9.97715695212527));
#84450=CARTESIAN_POINT('Ctrl Pts',(17.4588253890171,-20.6459145261259,-9.96945662525717));
#84451=CARTESIAN_POINT('Ctrl Pts',(17.5545157297192,-20.7138850312153,-9.96291554066431));
#84452=CARTESIAN_POINT('Ctrl Pts',(17.7962403809785,-20.8570211747457,-9.94753795322736));
#84453=CARTESIAN_POINT('Ctrl Pts',(17.9463144762433,-20.9238108435326,-9.93888737341477));
#84454=CARTESIAN_POINT('Ctrl Pts',(18.1324876106429,-20.9819888684044,-9.92767339637413));
#84455=CARTESIAN_POINT('Ctrl Pts',(18.1626149728676,-20.9906738030423,-9.92584312774557));
#84456=CARTESIAN_POINT('Ctrl Pts',(18.1998433757607,-21.0005157923087,-9.92354994607645));
#84457=CARTESIAN_POINT('Ctrl Pts',(18.2067736724179,-21.0023103781449,-9.92312172551355));
#84458=CARTESIAN_POINT('Ctrl Pts',(18.2176792610823,-21.0050754098504,-9.92244559294023));
#84459=CARTESIAN_POINT('Ctrl Pts',(18.2216485659944,-21.0060695585567,-9.92219902767828));
#84460=CARTESIAN_POINT('Ctrl Pts',(18.2290907245816,-21.0079106015636,-9.9217358066966));
#84461=CARTESIAN_POINT('Ctrl Pts',(18.2325628494293,-21.0087602099854,-9.92151930971906));
#84462=CARTESIAN_POINT('Ctrl Pts',(18.2405165857451,-21.0106851048478,-9.92102250717175));
#84463=CARTESIAN_POINT('Ctrl Pts',(18.2449995541821,-21.0117545494863,-9.92074187039057));
#84464=CARTESIAN_POINT('Ctrl Pts',(18.2588699155176,-21.0150155912093,-9.91987172683355));
#84465=CARTESIAN_POINT('Ctrl Pts',(18.268268658918,-21.0171576783912,-9.91927949039792));
#84466=CARTESIAN_POINT('Ctrl Pts',(18.3638848060111,-21.0382638455474,-9.91323026294764));
#84467=CARTESIAN_POINT('Ctrl Pts',(18.4511844512886,-21.0518794793575,-9.90751051502923));
#84468=CARTESIAN_POINT('Ctrl Pts',(18.6668380104197,-21.07182149918,-9.89328340561099));
#84469=CARTESIAN_POINT('Ctrl Pts',(18.795428898532,-21.0719963152216,-9.88473130295712));
#84470=CARTESIAN_POINT('Ctrl Pts',(18.9852673388954,-21.0549577562344,-9.87241271069616));
#84471=CARTESIAN_POINT('Ctrl Pts',(19.0470167231885,-21.0466570805686,-9.86845064721064));
#84472=CARTESIAN_POINT('Ctrl Pts',(19.1451810672345,-21.0290224095671,-9.86223503603126));
#84473=CARTESIAN_POINT('Ctrl Pts',(19.1818664647965,-21.0214221103261,-9.85993072719303));
#84474=CARTESIAN_POINT('Ctrl Pts',(19.229192757228,-21.0102996832341,-9.85698030549256));
#84475=CARTESIAN_POINT('Ctrl Pts',(19.2400325336125,-21.0076615809032,-9.85630604686218));
#84476=CARTESIAN_POINT('Ctrl Pts',(19.2576146247104,-21.0032350838827,-9.85521474389727));
#84477=CARTESIAN_POINT('Ctrl Pts',(19.2643697398668,-21.0014988620166,-9.85479602480717));
#84478=CARTESIAN_POINT('Ctrl Pts',(19.2773351036564,-20.9980980671859,-9.85399340316984));
#84479=CARTESIAN_POINT('Ctrl Pts',(19.2835465814626,-20.9964385272289,-9.85360934285446));
#84480=CARTESIAN_POINT('Ctrl Pts',(19.2977391837189,-20.9925772899423,-9.85273281632792));
#84481=CARTESIAN_POINT('Ctrl Pts',(19.305715177932,-20.9903570103843,-9.85224095883366));
#84482=CARTESIAN_POINT('Ctrl Pts',(19.3268436071897,-20.984341713223,-9.85093985787687));
#84483=CARTESIAN_POINT('Ctrl Pts',(19.3399727434232,-20.9804657821252,-9.85013324939695));
#84484=CARTESIAN_POINT('Ctrl Pts',(19.4381168812101,-20.9504541337861,-9.84411603218965));
#84485=CARTESIAN_POINT('Ctrl Pts',(19.5214522269294,-20.9191098740275,-9.83908225683098));
#84486=CARTESIAN_POINT('Ctrl Pts',(19.7313864581444,-20.8246610824248,-9.82633015447441));
#84487=CARTESIAN_POINT('Ctrl Pts',(19.8540672755892,-20.7539674384573,-9.81882079775667));
#84488=CARTESIAN_POINT('Ctrl Pts',(20.0134925739095,-20.6394881366564,-9.80797731963053));
#84489=CARTESIAN_POINT('Ctrl Pts',(20.0569216447132,-20.6056610715429,-9.80489312583969));
#84490=CARTESIAN_POINT('Ctrl Pts',(20.1206848305545,-20.5518751353147,-9.8000808919658));
#84491=CARTESIAN_POINT('Ctrl Pts',(20.1420174350213,-20.5331331355077,-9.79841933814992));
#84492=CARTESIAN_POINT('Ctrl Pts',(20.168083384129,-20.5092867310699,-9.79631441044709));
#84493=CARTESIAN_POINT('Ctrl Pts',(20.173178181235,-20.5045795551338,-9.79589933593127));
#84494=CARTESIAN_POINT('Ctrl Pts',(20.1812055337909,-20.4970894753331,-9.79523936709984));
#84495=CARTESIAN_POINT('Ctrl Pts',(20.1841534605497,-20.4943230154693,-9.79499571437365));
#84496=CARTESIAN_POINT('Ctrl Pts',(20.1896996377925,-20.4890882888963,-9.79453483107102));
#84497=CARTESIAN_POINT('Ctrl Pts',(20.1922995514029,-20.4866218625421,-9.79431774053349));
#84498=CARTESIAN_POINT('Ctrl Pts',(20.1982311387073,-20.4809661357236,-9.79382008819772));
#84499=CARTESIAN_POINT('Ctrl Pts',(20.2015586570383,-20.4777725449662,-9.79353919610343));
#84500=CARTESIAN_POINT('Ctrl Pts',(20.2103686539848,-20.4692616548018,-9.79279099112213));
#84501=CARTESIAN_POINT('Ctrl Pts',(20.2158327804624,-20.4639255730068,-9.79232226894043));
#84502=CARTESIAN_POINT('Ctrl Pts',(20.2539995434603,-20.4262475560296,-9.78901607269487));
#84503=CARTESIAN_POINT('Ctrl Pts',(20.2856669391502,-20.392879412843,-9.7861059525481));
#84504=CARTESIAN_POINT('Ctrl Pts',(20.4208039546154,-20.2408601972975,-9.77302745189414));
#84505=CARTESIAN_POINT('Ctrl Pts',(20.5119397262914,-20.111914263051,-9.76243943244153));
#84506=CARTESIAN_POINT('Ctrl Pts',(20.6351493005773,-19.8884198288713,-9.74583522376284));
#84507=CARTESIAN_POINT('Ctrl Pts',(20.6763731026431,-19.7996096085827,-9.73961548559119));
#84508=CARTESIAN_POINT('Ctrl Pts',(20.7190560586598,-19.6880103771488,-9.73227405897855));
#84509=CARTESIAN_POINT('Ctrl Pts',(20.7264880543991,-19.6676467279378,-9.73095259784948));
#84510=CARTESIAN_POINT('Ctrl Pts',(20.7365804918525,-19.6386166417251,-9.72909370309057));
#84511=CARTESIAN_POINT('Ctrl Pts',(20.7394998699028,-19.6300422662695,-9.72854771052524));
#84512=CARTESIAN_POINT('Ctrl Pts',(20.7444307264143,-19.6152495772273,-9.72761092211941));
#84513=CARTESIAN_POINT('Ctrl Pts',(20.7464685874899,-19.6090402523865,-9.72721925879928));
#84514=CARTESIAN_POINT('Ctrl Pts',(20.7503084077861,-19.5971549169186,-9.72647251146765));
#84515=CARTESIAN_POINT('Ctrl Pts',(20.7521152305639,-19.5914805543681,-9.7261172703924));
#84516=CARTESIAN_POINT('Ctrl Pts',(20.756736511254,-19.5767526642914,-9.72519849665849));
#84517=CARTESIAN_POINT('Ctrl Pts',(20.7595141571454,-19.5676876555111,-9.72463617547587));
#84518=CARTESIAN_POINT('Ctrl Pts',(20.7687051334847,-19.536956871973,-9.72274038793743));
#84519=CARTESIAN_POINT('Ctrl Pts',(20.7748326166676,-19.5152067213116,-9.72141623835557));
#84520=CARTESIAN_POINT('Ctrl Pts',(20.8267419806815,-19.3189641531164,-9.70961601923621));
#84521=CARTESIAN_POINT('Ctrl Pts',(20.8503939628842,-19.1393891766988,-9.69994105044149));
#84522=CARTESIAN_POINT('Ctrl Pts',(20.8512640462748,-18.8753638286044,-9.68556286600716));
#84523=CARTESIAN_POINT('Ctrl Pts',(20.8465857594597,-18.7918146282843,-9.68097533658553));
#84524=CARTESIAN_POINT('Ctrl Pts',(20.83273510524,-18.6720618887445,-9.67408633509576));
#84525=CARTESIAN_POINT('Ctrl Pts',(20.8275295954145,-18.6354753608906,-9.67193852902863));
#84526=CARTESIAN_POINT('Ctrl Pts',(20.8201158532339,-18.5916304462376,-9.66929255327628));
#84527=CARTESIAN_POINT('Ctrl Pts',(20.8188224028559,-18.58422138032,-9.66884293404462));
#84528=CARTESIAN_POINT('Ctrl Pts',(20.8167502737151,-18.5727142277777,-9.66814052339554));
#84529=CARTESIAN_POINT('Ctrl Pts',(20.815998901674,-18.5686111994208,-9.66788925769288));
#84530=CARTESIAN_POINT('Ctrl Pts',(20.8145829340087,-18.561005930782,-9.66742196685207));
#84531=CARTESIAN_POINT('Ctrl Pts',(20.8139216170854,-18.557503138619,-9.66720612963331));
#84532=CARTESIAN_POINT('Ctrl Pts',(20.8124064858603,-18.5495876740574,-9.66671700346674));
#84533=CARTESIAN_POINT('Ctrl Pts',(20.8115474688085,-18.5451760644671,-9.6664434225099));
#84534=CARTESIAN_POINT('Ctrl Pts',(20.8089703108162,-18.5321617353532,-9.6656335535975));
#84535=CARTESIAN_POINT('Ctrl Pts',(20.8072127619355,-18.5235670450785,-9.66509509832949));
#84536=CARTESIAN_POINT('Ctrl Pts',(20.7941088895004,-18.4614563504302,-9.66117891153828));
#84537=CARTESIAN_POINT('Ctrl Pts',(20.7807463196187,-18.4083915891833,-9.65769912493189));
#84538=CARTESIAN_POINT('Ctrl Pts',(20.7569451113049,-18.3272823588542,-9.65223131095082));
#84539=CARTESIAN_POINT('Ctrl Pts',(20.7479407525649,-18.2988372357528,-9.65028466107274));
#84540=CARTESIAN_POINT('Ctrl Pts',(20.6966405512842,-18.147939258153,-9.63983111712647));
#84541=CARTESIAN_POINT('Ctrl Pts',(20.6437683453331,-18.0293624064292,-9.63118798340045));
#84542=CARTESIAN_POINT('Ctrl Pts',(20.5373132122674,-17.8395688736772,-9.61709965361327));
#84543=CARTESIAN_POINT('Ctrl Pts',(20.4894868974471,-17.7655301540048,-9.61152494773811));
#84544=CARTESIAN_POINT('Ctrl Pts',(20.425008091196,-17.6781865198193,-9.60486235783854));
#84545=CARTESIAN_POINT('Ctrl Pts',(20.4125951025672,-17.6618730005151,-9.60361371622558));
#84546=CARTESIAN_POINT('Ctrl Pts',(20.3944819989994,-17.6387723084949,-9.60183889997603));
#84547=CARTESIAN_POINT('Ctrl Pts',(20.3889734634666,-17.6318370260897,-9.60130518176159));
#84548=CARTESIAN_POINT('Ctrl Pts',(20.3793475157917,-17.619872832764,-9.60038284195804));
#84549=CARTESIAN_POINT('Ctrl Pts',(20.375250199588,-17.6148279762034,-9.59999342221179));
#84550=CARTESIAN_POINT('Ctrl Pts',(20.3673267025798,-17.6051633869561,-9.59924639093293));
#84551=CARTESIAN_POINT('Ctrl Pts',(20.3635039969832,-17.6005408979361,-9.59888864427572));
#84552=CARTESIAN_POINT('Ctrl Pts',(20.3534366718736,-17.5884721101804,-9.59795338779382));
#84553=CARTESIAN_POINT('Ctrl Pts',(20.347160289299,-17.5810523983983,-9.59737717893864));
#84554=CARTESIAN_POINT('Ctrl Pts',(20.3251920539414,-17.5554421017974,-9.59538374936086));
#84555=CARTESIAN_POINT('Ctrl Pts',(20.3092414694154,-17.537475168864,-9.59397721905543));
#84556=CARTESIAN_POINT('Ctrl Pts',(20.1932899243854,-17.4112603013938,-9.58402816140778));
#84557=CARTESIAN_POINT('Ctrl Pts',(20.0825309530204,-17.3134406247597,-9.57598921309175));
#84558=CARTESIAN_POINT('Ctrl Pts',(19.924281372916,-17.2006801613959,-9.56543632537456));
#84559=CARTESIAN_POINT('Ctrl Pts',(19.8851714750098,-17.1747281987349,-9.5628909327256));
#84560=CARTESIAN_POINT('Ctrl Pts',(19.7844797586393,-17.1126316795459,-9.55641959030261));
#84561=CARTESIAN_POINT('Ctrl Pts',(19.7218759288467,-17.0782649224539,-9.55247019126166));
#84562=CARTESIAN_POINT('Ctrl Pts',(19.6274567465628,-17.0324815993257,-9.54645205774746));
#84563=CARTESIAN_POINT('Ctrl Pts',(19.5969096306861,-17.0185568195946,-9.54449579895512));
#84564=CARTESIAN_POINT('Ctrl Pts',(19.5593239837972,-17.0024916597132,-9.54206244678197));
#84565=CARTESIAN_POINT('Ctrl Pts',(19.5525868360795,-16.9996531979863,-9.54162525725391));
#84566=CARTESIAN_POINT('Ctrl Pts',(19.5420253048286,-16.9952677431455,-9.5409381048969));
#84567=CARTESIAN_POINT('Ctrl Pts',(19.5382107975635,-16.9936969053098,-9.54068956264767));
#84568=CARTESIAN_POINT('Ctrl Pts',(19.5310869187825,-16.9907875720626,-9.54022467057551));
#84569=CARTESIAN_POINT('Ctrl Pts',(19.5277787447478,-16.9894462944071,-9.54000849190005));
#84570=CARTESIAN_POINT('Ctrl Pts',(19.5202385190781,-16.9864113426655,-9.53951510361877));
#84571=CARTESIAN_POINT('Ctrl Pts',(19.5160043967038,-16.9847229728984,-9.53923758006645));
#84572=CARTESIAN_POINT('Ctrl Pts',(19.5049816460905,-16.9803688241527,-9.53851394819959));
#84573=CARTESIAN_POINT('Ctrl Pts',(19.4981847022136,-16.9777244545004,-9.53806660435822));
#84574=CARTESIAN_POINT('Ctrl Pts',(19.4548181590024,-16.9611100777212,-9.53520584775666));
#84575=CARTESIAN_POINT('Ctrl Pts',(19.4178831164481,-16.9481225246284,-9.53273978951299));
#84576=CARTESIAN_POINT('Ctrl Pts',(19.3688624524125,-16.9323983247203,-9.52944737596279));
#84577=CARTESIAN_POINT('Ctrl Pts',(19.3570802245899,-16.928732275929,-9.52865457279627));
#84578=CARTESIAN_POINT('Ctrl Pts',(19.3221509476063,-16.9181980410258,-9.52630119208308));
#84579=CARTESIAN_POINT('Ctrl Pts',(19.2989180870275,-16.9116227215546,-9.52473193113092));
#84580=CARTESIAN_POINT('Ctrl Pts',(19.136220013105,-16.8685680083954,-9.51373620452499));
#84581=CARTESIAN_POINT('Ctrl Pts',(18.9934449950039,-16.8460172980108,-9.50408906827816));
#84582=CARTESIAN_POINT('Ctrl Pts',(18.7877688399188,-16.8347805082826,-9.49078080342547));
#84583=CARTESIAN_POINT('Ctrl Pts',(18.7259288399144,-16.8341129748524,-9.48684921219987));
#84584=CARTESIAN_POINT('Ctrl Pts',(18.6269048133701,-16.8373823397465,-9.48067558989718));
#84585=CARTESIAN_POINT('Ctrl Pts',(18.5897034138333,-16.8395947358536,-9.47838364300904));
#84586=CARTESIAN_POINT('Ctrl Pts',(18.5414838612195,-16.8437423014528,-9.47544654793898));
#84587=CARTESIAN_POINT('Ctrl Pts',(18.5303974114124,-16.8447840688444,-9.47477356748234));
#84588=CARTESIAN_POINT('Ctrl Pts',(18.5123855101946,-16.8466200822429,-9.47368381678425));
#84589=CARTESIAN_POINT('Ctrl Pts',(18.5054549613242,-16.8473611361349,-9.47326538066321));
#84590=CARTESIAN_POINT('Ctrl Pts',(18.4921372994333,-16.8488516960358,-9.47246295685561));
#84591=CARTESIAN_POINT('Ctrl Pts',(18.4857497040793,-16.8495961029391,-9.47207881325076));
#84592=CARTESIAN_POINT('Ctrl Pts',(18.4711367175062,-16.8513666187687,-9.47120162003065));
#84593=CARTESIAN_POINT('Ctrl Pts',(18.4629137290526,-16.8524119584277,-9.47070918235473));
#84594=CARTESIAN_POINT('Ctrl Pts',(18.4410945244786,-16.8553160258346,-9.46940552674511));
#84595=CARTESIAN_POINT('Ctrl Pts',(18.4275097403157,-16.8572587178701,-9.46859696055655));
#84596=CARTESIAN_POINT('Ctrl Pts',(18.3247121567189,-16.8729807280252,-9.46250012681056));
#84597=CARTESIAN_POINT('Ctrl Pts',(18.2364381115432,-16.8923221844788,-9.45739434800246));
#84598=CARTESIAN_POINT('Ctrl Pts',(18.0155894357492,-16.9557453733172,-9.44467437709994));
#84599=CARTESIAN_POINT('Ctrl Pts',(17.8856587127161,-17.0074019747641,-9.43725491486124));
#84600=CARTESIAN_POINT('Ctrl Pts',(17.712639698633,-17.0968532881045,-9.42649617652613));
#84601=CARTESIAN_POINT('Ctrl Pts',(17.664540704521,-17.1241591554437,-9.42339806776635));
#84602=CARTESIAN_POINT('Ctrl Pts',(17.5933680507303,-17.1683354879316,-9.41856617912751));
#84603=CARTESIAN_POINT('Ctrl Pts',(17.5694739384615,-17.1838429913178,-9.41689953252225));
#84604=CARTESIAN_POINT('Ctrl Pts',(17.5401543141684,-17.2037237941696,-9.41478891120607));
#84605=CARTESIAN_POINT('Ctrl Pts',(17.5344266243528,-17.2076488521969,-9.41437341909254));
#84606=CARTESIAN_POINT('Ctrl Pts',(17.5253935827557,-17.2139045237138,-9.41371293663021));
#84607=CARTESIAN_POINT('Ctrl Pts',(17.5220753642248,-17.2162165938512,-9.41346919115557));
#84608=CARTESIAN_POINT('Ctrl Pts',(17.5158296069448,-17.2205951558227,-9.41300823591552));
#84609=CARTESIAN_POINT('Ctrl Pts',(17.5129006825669,-17.2226595774096,-9.41279116679348));
#84610=CARTESIAN_POINT('Ctrl Pts',(17.5062161343094,-17.2273965596402,-9.41229369831953));
#84611=CARTESIAN_POINT('Ctrl Pts',(17.5024639929694,-17.2300739534431,-9.41201296955642));
#84612=CARTESIAN_POINT('Ctrl Pts',(17.4925254610199,-17.2372148345733,-9.41126548164981));
#84613=CARTESIAN_POINT('Ctrl Pts',(17.4863544670865,-17.2416994957955,-9.41079731741055));
#84614=CARTESIAN_POINT('Ctrl Pts',(17.4432975305892,-17.2733473988742,-9.40750318604318));
#84615=CARTESIAN_POINT('Ctrl Pts',(17.4072803261857,-17.3016662039632,-9.40460515528195));
#84616=CARTESIAN_POINT('Ctrl Pts',(17.3434297880869,-17.3553106914298,-9.39924370613024));
#84617=CARTESIAN_POINT('Ctrl Pts',(17.3152969373005,-17.3802545828514,-9.39679632781525));
#84618=CARTESIAN_POINT('Ctrl Pts',(17.192180394829,-17.4954149916012,-9.38574620355505));
#84619=CARTESIAN_POINT('Ctrl Pts',(17.1050205672822,-17.5935901668398,-9.37700301427132));
#84620=CARTESIAN_POINT('Ctrl Pts',(16.9752026480569,-17.7704210816275,-9.36279856028141));
#84621=CARTESIAN_POINT('Ctrl Pts',(16.9274171300745,-17.8448601604884,-9.35720316407805));
#84622=CARTESIAN_POINT('Ctrl Pts',(16.8744284015705,-17.9400196549519,-9.35051865954794));
#84623=CARTESIAN_POINT('Ctrl Pts',(16.8646987124888,-17.958106901319,-9.34926760661699));
#84624=CARTESIAN_POINT('Ctrl Pts',(16.8511486069233,-17.9841993022664,-9.34748999740643));
#84625=CARTESIAN_POINT('Ctrl Pts',(16.8471131270219,-17.992090894271,-9.34695586490234));
#84626=CARTESIAN_POINT('Ctrl Pts',(16.8402042019512,-18.0058135870329,-9.34603303937244));
#84627=CARTESIAN_POINT('Ctrl Pts',(16.837307855725,-18.0116329630942,-9.34564354586782));
#84628=CARTESIAN_POINT('Ctrl Pts',(16.8317911214945,-18.0228464371983,-9.34489653270058));
#84629=CARTESIAN_POINT('Ctrl Pts',(16.829166763936,-18.0282385022869,-9.34453887715261));
#84630=CARTESIAN_POINT('Ctrl Pts',(16.8223533123695,-18.0423900742458,-9.34360421261495));
#84631=CARTESIAN_POINT('Ctrl Pts',(16.8182014766042,-18.0511674418156,-9.34302850135214));
#84632=CARTESIAN_POINT('Ctrl Pts',(16.8040088680704,-18.0817138836066,-9.34103852658906));
#84633=CARTESIAN_POINT('Ctrl Pts',(16.7942773423429,-18.1036252160942,-9.33963490353653));
#84634=CARTESIAN_POINT('Ctrl Pts',(16.7250855536645,-18.2668346877018,-9.3293440439758));
#84635=CARTESIAN_POINT('Ctrl Pts',(16.6807559356853,-18.4140553695192,-9.32100721039236));
#84636=CARTESIAN_POINT('Ctrl Pts',(16.6289120188436,-18.6927191509291,-9.30561469461767));
#84637=CARTESIAN_POINT('Ctrl Pts',(16.6169601914202,-18.8225565402336,-9.29857228728212));
#84638=CARTESIAN_POINT('Ctrl Pts',(16.6170011042386,-18.9559243141497,-9.29078130781142));
#84639=CARTESIAN_POINT('Ctrl Pts',(16.6170097079818,-18.9591991753601,-9.2905896487255));
#84640=CARTESIAN_POINT('Ctrl Pts',(16.6171033846654,-18.9781328626562,-9.28947947249069));
#84641=CARTESIAN_POINT('Ctrl Pts',(16.617354592849,-18.9937898859883,-9.28855313985671));
#84642=CARTESIAN_POINT('Ctrl Pts',(16.6179364383181,-19.015225593477,-9.28727182670056));
#84643=CARTESIAN_POINT('Ctrl Pts',(16.6181171280115,-19.0210082820074,-9.28692486276551));
#84644=CARTESIAN_POINT('Ctrl Pts',(16.618441992775,-19.0301981290071,-9.28637129038767));
#84645=CARTESIAN_POINT('Ctrl Pts',(16.6185707023212,-19.0336058543001,-9.28616554187761));
#84646=CARTESIAN_POINT('Ctrl Pts',(16.6188536012539,-19.0406449231496,-9.28573953272618));
#84647=CARTESIAN_POINT('Ctrl Pts',(16.6190089084551,-19.0442761748026,-9.28551920786138));
#84648=CARTESIAN_POINT('Ctrl Pts',(16.6194013860905,-19.0529306252594,-9.28499279386702));
#84649=CARTESIAN_POINT('Ctrl Pts',(16.6196471048459,-19.0579533983379,-9.28468622986837));
#84650=CARTESIAN_POINT('Ctrl Pts',(16.6205368676228,-19.0749034750163,-9.28364825052643));
#84651=CARTESIAN_POINT('Ctrl Pts',(16.6212639473949,-19.0868259360013,-9.28291240768569));
#84652=CARTESIAN_POINT('Ctrl Pts',(16.631113687836,-19.2285839076868,-9.27409998991241));
#84653=CARTESIAN_POINT('Ctrl Pts',(16.6520896332326,-19.3573045948984,-9.265483365158));
#84654=CARTESIAN_POINT('Ctrl Pts',(16.701839122724,-19.5492021999487,-9.25238340889672));
#84655=CARTESIAN_POINT('Ctrl Pts',(16.7220914885675,-19.6142227130923,-9.24789463062267));
#84656=CARTESIAN_POINT('Ctrl Pts',(16.7454193049359,-19.6781100599899,-9.24346979696294));
#84657=CARTESIAN_POINT('Origin',(18.734,-18.952,0.));
#84658=CARTESIAN_POINT('',(16.7454194499637,-19.6781104571739,-8.4444886490522));
#84659=CARTESIAN_POINT('',(16.7454194712032,-19.678110515342,-8.66553666923996));
#84660=CARTESIAN_POINT('',(16.7454194499637,-19.6781104571739,0.));
#84661=CARTESIAN_POINT('',(16.6170000013281,-18.9519250126714,-8.71094372102528));
#84662=CARTESIAN_POINT('Ctrl Pts',(16.7454194712032,-19.678110515342,-8.66553666923996));
#84663=CARTESIAN_POINT('Ctrl Pts',(16.6904356127053,-19.527527610816,-8.67608242901258));
#84664=CARTESIAN_POINT('Ctrl Pts',(16.6527074043694,-19.3711105565511,-8.68676264432225));
#84665=CARTESIAN_POINT('Ctrl Pts',(16.6297591054065,-19.1855832829213,-8.69860360219042));
#84666=CARTESIAN_POINT('Ctrl Pts',(16.6270006245378,-19.1592308344624,-8.70026804571858));
#84667=CARTESIAN_POINT('Ctrl Pts',(16.6216845085739,-19.0972227551114,-8.70414333167712));
#84668=CARTESIAN_POINT('Ctrl Pts',(16.6195337123929,-19.0615397043015,-8.70634146733557));
#84669=CARTESIAN_POINT('Ctrl Pts',(16.617898153749,-19.0146623185697,-8.70918909189148));
#84670=CARTESIAN_POINT('Ctrl Pts',(16.6175971721877,-19.0035040559628,-8.70986395115042));
#84671=CARTESIAN_POINT('Ctrl Pts',(16.6172522425384,-18.9854074934492,-8.71095376412891));
#84672=CARTESIAN_POINT('Ctrl Pts',(16.6171541291233,-18.9784705510505,-8.71137040718873));
#84673=CARTESIAN_POINT('Ctrl Pts',(16.6170502016031,-18.967207401971,-8.71204511525387));
#84674=CARTESIAN_POINT('Ctrl Pts',(16.6170235457565,-18.9628814804057,-8.71230383078575));
#84675=CARTESIAN_POINT('Ctrl Pts',(16.617003429385,-18.9563852150012,-8.71269171670242));
#84676=CARTESIAN_POINT('Ctrl Pts',(16.6170000462402,-18.9542149335066,-8.71282119677421));
#84677=CARTESIAN_POINT('Ctrl Pts',(16.6170000004708,-18.9520446456796,-8.71295057259137));
#84678=CARTESIAN_POINT('Ctrl Pts',(16.6170000013281,-18.9519250126714,-8.71094372102528));
#84679=CARTESIAN_POINT('Ctrl Pts',(16.6170027209272,-18.8751468230115,-8.71553605185447));
#84680=CARTESIAN_POINT('Ctrl Pts',(16.6211865549027,-18.7984540523296,-8.72012838268367));
#84681=CARTESIAN_POINT('Ctrl Pts',(16.6294980530145,-18.7223033410468,-8.72472071351286));
#84682=CARTESIAN_POINT('Ctrl Pts',(16.637833810921,-18.6459303592898,-8.7293264485445));
#84683=CARTESIAN_POINT('Ctrl Pts',(16.6503212662752,-18.570103004567,-8.73393218357614));
#84684=CARTESIAN_POINT('Ctrl Pts',(16.6668554550744,-18.4952698494906,-8.73853791860778));
#84685=CARTESIAN_POINT('Ctrl Pts',(16.683415117402,-18.4203214021236,-8.74315074950144));
#84686=CARTESIAN_POINT('Ctrl Pts',(16.7040338351227,-18.3463705997984,-8.74776358039509));
#84687=CARTESIAN_POINT('Ctrl Pts',(16.7285569647209,-18.2738501402711,-8.75237641128874));
#84688=CARTESIAN_POINT('Ctrl Pts',(16.7531478646367,-18.2011292685346,-8.75700198986265));
#84689=CARTESIAN_POINT('Ctrl Pts',(16.7816645931624,-18.1298470190276,-8.76162756843655));
#84690=CARTESIAN_POINT('Ctrl Pts',(16.8139044122095,-18.060416053449,-8.76625314701046));
#84691=CARTESIAN_POINT('Ctrl Pts',(16.831243102243,-18.0230758317455,-8.76874079971725));
#84692=CARTESIAN_POINT('Ctrl Pts',(16.8496578472076,-17.9862706239721,-8.77122845242405));
#84693=CARTESIAN_POINT('Ctrl Pts',(16.8691118619909,-17.9500612629941,-8.77371610513084));
#84694=CARTESIAN_POINT('Ctrl Pts',(16.9034286623952,-17.8861881022462,-8.77810431406174));
#84695=CARTESIAN_POINT('Ctrl Pts',(16.9410977666969,-17.8239553476821,-8.78249252299263));
#84696=CARTESIAN_POINT('Ctrl Pts',(16.9819381659417,-17.7637372640547,-8.78688073192353));
#84697=CARTESIAN_POINT('Ctrl Pts',(17.0227179512625,-17.7036085540478,-8.79126242802479));
#84698=CARTESIAN_POINT('Ctrl Pts',(17.0666594195114,-17.6454889751329,-8.79564412412606));
#84699=CARTESIAN_POINT('Ctrl Pts',(17.1135357879719,-17.5897280970614,-8.80002582022733));
#84700=CARTESIAN_POINT('Ctrl Pts',(17.1603570729688,-17.5340327424593,-8.80440236748697));
#84701=CARTESIAN_POINT('Ctrl Pts',(17.2101060983649,-17.4806909501826,-8.80877891474661));
#84702=CARTESIAN_POINT('Ctrl Pts',(17.2625139124397,-17.4300217826406,-8.81315546200624));
#84703=CARTESIAN_POINT('Ctrl Pts',(17.3148884902405,-17.3793847487483,-8.81752923372322));
#84704=CARTESIAN_POINT('Ctrl Pts',(17.3699181652065,-17.331417311077,-8.82190300544019));
#84705=CARTESIAN_POINT('Ctrl Pts',(17.4272959551551,-17.2864029481336,-8.82627677715716));
#84706=CARTESIAN_POINT('Ctrl Pts',(17.4846562848495,-17.2414022832121,-8.83064921792072));
#84707=CARTESIAN_POINT('Ctrl Pts',(17.5443629316526,-17.1993532065252,-8.83502165868427));
#84708=CARTESIAN_POINT('Ctrl Pts',(17.6060758346833,-17.1604989318187,-8.83939409944782));
#84709=CARTESIAN_POINT('Ctrl Pts',(17.6677903157198,-17.1216436636041,-8.84376665201517));
#84710=CARTESIAN_POINT('Ctrl Pts',(17.7315107455603,-17.085983614876,-8.84813920458252));
#84711=CARTESIAN_POINT('Ctrl Pts',(17.7968695201138,-17.0537177597448,-8.85251175714986));
#84712=CARTESIAN_POINT('Ctrl Pts',(17.8622961264687,-17.0214184178922,-8.85688884771719));
#84713=CARTESIAN_POINT('Ctrl Pts',(17.9293640389057,-16.9925205167796,-8.86126593828452));
#84714=CARTESIAN_POINT('Ctrl Pts',(17.997683325039,-16.9671758883532,-8.86564302885184));
#84715=CARTESIAN_POINT('Ctrl Pts',(18.0660399228703,-16.9418174182846,-8.87002250991079));
#84716=CARTESIAN_POINT('Ctrl Pts',(18.135648794436,-16.9200162288388,-8.87440199096972));
#84717=CARTESIAN_POINT('Ctrl Pts',(18.2061050046724,-16.9018741809567,-8.87878147202867));
#84718=CARTESIAN_POINT('Ctrl Pts',(18.2766860980686,-16.8836999764164,-8.88316871568839));
#84719=CARTESIAN_POINT('Ctrl Pts',(18.348117056223,-16.869197961386,-8.88755595934811));
#84720=CARTESIAN_POINT('Ctrl Pts',(18.4199835016911,-16.8584187049962,-8.89194320300783));
#84721=CARTESIAN_POINT('Ctrl Pts',(18.4688457595752,-16.8510898493378,-8.89492610594264));
#84722=CARTESIAN_POINT('Ctrl Pts',(18.5179091821632,-16.8454808253817,-8.89790900887746));
#84723=CARTESIAN_POINT('Ctrl Pts',(18.567043338876,-16.8415937658104,-8.90089191181228));
#84724=CARTESIAN_POINT('Ctrl Pts',(18.6393255921073,-16.8358754337365,-8.90528012074317));
#84725=CARTESIAN_POINT('Ctrl Pts',(18.7120430618562,-16.8338637794812,-8.90966832967407));
#84726=CARTESIAN_POINT('Ctrl Pts',(18.7847830739803,-16.8356091855716,-8.91405653860496));
#84727=CARTESIAN_POINT('Ctrl Pts',(18.8574151278658,-16.8373520011898,-8.91843823470623));
#84728=CARTESIAN_POINT('Ctrl Pts',(18.9300691794578,-16.8428407963575,-8.9228199308075));
#84729=CARTESIAN_POINT('Ctrl Pts',(19.0023285427326,-16.8520740981751,-8.92720162690877));
#84730=CARTESIAN_POINT('Ctrl Pts',(19.074502995505,-16.8612965501284,-8.9315781741684));
#84731=CARTESIAN_POINT('Ctrl Pts',(19.1462832051701,-16.8742547070802,-8.93595472142804));
#84732=CARTESIAN_POINT('Ctrl Pts',(19.2172553122691,-16.8908951256271,-8.94033126868768));
#84733=CARTESIAN_POINT('Ctrl Pts',(19.2881824098894,-16.9075249910624,-8.94470504040465));
#84734=CARTESIAN_POINT('Ctrl Pts',(19.358301953298,-16.9278323748368,-8.94907881212162));
#84735=CARTESIAN_POINT('Ctrl Pts',(19.4272094182993,-16.9517125950551,-8.95345258383859));
#84736=CARTESIAN_POINT('Ctrl Pts',(19.4960959145276,-16.9755855484422,-8.95782502460214));
#84737=CARTESIAN_POINT('Ctrl Pts',(19.5637706090989,-17.0030290219352,-8.96219746536569));
#84738=CARTESIAN_POINT('Ctrl Pts',(19.6298449292375,-17.0338887251363,-8.96656990612924));
#84739=CARTESIAN_POINT('Ctrl Pts',(19.6959209389038,-17.0647492174234,-8.97094245869659));
#84740=CARTESIAN_POINT('Ctrl Pts',(19.7603960566782,-17.0990259069124,-8.97531501126393));
#84741=CARTESIAN_POINT('Ctrl Pts',(19.8229039996998,-17.1365173976494,-8.97968756383127));
#84742=CARTESIAN_POINT('Ctrl Pts',(19.8854768158224,-17.1740477984696,-8.9840646543986));
#84743=CARTESIAN_POINT('Ctrl Pts',(19.9460779664246,-17.2147994133216,-8.98844174496592));
#84744=CARTESIAN_POINT('Ctrl Pts',(20.004368721863,-17.25852655453,-8.99281883553325));
#84745=CARTESIAN_POINT('Ctrl Pts',(20.0626913120465,-17.3022775767531,-8.99719831659219));
#84746=CARTESIAN_POINT('Ctrl Pts',(20.1187006241991,-17.3490070515424,-9.00157779765113));
#84747=CARTESIAN_POINT('Ctrl Pts',(20.17209182572,-17.3984296279868,-9.00595727871007));
#84748=CARTESIAN_POINT('Ctrl Pts',(20.2255776627872,-17.4479398056161,-9.01034452236979));
#84749=CARTESIAN_POINT('Ctrl Pts',(20.2764357852878,-17.5001522715463,-9.01473176602951));
#84750=CARTESIAN_POINT('Ctrl Pts',(20.3243993779342,-17.5547459720343,-9.01911900968923));
#84751=CARTESIAN_POINT('Ctrl Pts',(20.3570099991731,-17.5918644277298,-9.02210191262405));
#84752=CARTESIAN_POINT('Ctrl Pts',(20.3882834007585,-17.6300829433876,-9.02508481555887));
#84753=CARTESIAN_POINT('Ctrl Pts',(20.4181471898432,-17.6692930019122,-9.0280677184937));
#84754=CARTESIAN_POINT('Ctrl Pts',(20.4620804149045,-17.7269757132704,-9.03245592742459));
#84755=CARTESIAN_POINT('Ctrl Pts',(20.5031324849612,-17.7870307272458,-9.03684413635549));
#84756=CARTESIAN_POINT('Ctrl Pts',(20.541037663595,-17.8491383212981,-9.04123234528639));
#84757=CARTESIAN_POINT('Ctrl Pts',(20.578886584659,-17.9111537373832,-9.04561404138766));
#84758=CARTESIAN_POINT('Ctrl Pts',(20.6135976366774,-17.9752152777401,-9.04999573748892));
#84759=CARTESIAN_POINT('Ctrl Pts',(20.6449465138838,-18.0409717781126,-9.05437743359019));
#84760=CARTESIAN_POINT('Ctrl Pts',(20.6762585536648,-18.1066510093641,-9.05875398084983));
#84761=CARTESIAN_POINT('Ctrl Pts',(20.7042160604134,-18.1740208108152,-9.06313052810947));
#84762=CARTESIAN_POINT('Ctrl Pts',(20.728639957299,-18.242704264255,-9.06750707536911));
#84763=CARTESIAN_POINT('Ctrl Pts',(20.7530483649043,-18.3113441596469,-9.07188084708609));
#84764=CARTESIAN_POINT('Ctrl Pts',(20.7739274477879,-18.3812956006723,-9.07625461880306));
#84765=CARTESIAN_POINT('Ctrl Pts',(20.7911462655829,-18.4521617841757,-9.08062839052004));
#84766=CARTESIAN_POINT('Ctrl Pts',(20.8083598436337,-18.5230064028614,-9.08500083128359));
#84767=CARTESIAN_POINT('Ctrl Pts',(20.8219152540694,-18.5947647429384,-9.08937327204714));
#84768=CARTESIAN_POINT('Ctrl Pts',(20.8317319036236,-18.6670265617294,-9.0937457128107));
#84769=CARTESIAN_POINT('Ctrl Pts',(20.8415488041906,-18.739290228263,-9.09811826537804));
#84770=CARTESIAN_POINT('Ctrl Pts',(20.847626691118,-18.8120569208142,-9.10249081794539));
#84771=CARTESIAN_POINT('Ctrl Pts',(20.8499366445659,-18.8849096416525,-9.10686337051273));
#84772=CARTESIAN_POINT('Ctrl Pts',(20.8522489953706,-18.9578379717924,-9.11124046108006));
#84773=CARTESIAN_POINT('Ctrl Pts',(20.8507855897922,-19.0308520253128,-9.11561755164739));
#84774=CARTESIAN_POINT('Ctrl Pts',(20.8455696643532,-19.1035339981098,-9.11999464221472));
#84775=CARTESIAN_POINT('Ctrl Pts',(20.8403508903038,-19.1762556652297,-9.12437412327366));
#84776=CARTESIAN_POINT('Ctrl Pts',(20.8313755754733,-19.2486444114932,-9.1287536043326));
#84777=CARTESIAN_POINT('Ctrl Pts',(20.8187186547149,-19.3202894658875,-9.13313308539154));
#84778=CARTESIAN_POINT('Ctrl Pts',(20.8060392996494,-19.3920615106598,-9.13752032905126));
#84779=CARTESIAN_POINT('Ctrl Pts',(20.789665415713,-19.4630867607306,-9.14190757271098));
#84780=CARTESIAN_POINT('Ctrl Pts',(20.769722536241,-19.532967086366,-9.14629481637071));
#84781=CARTESIAN_POINT('Ctrl Pts',(20.7561632998913,-19.5804789741458,-9.14927771930552));
#84782=CARTESIAN_POINT('Ctrl Pts',(20.7409552755656,-19.6274619134099,-9.15226062224033));
#84783=CARTESIAN_POINT('Ctrl Pts',(20.7241505240927,-19.6737962949846,-9.15524352517514));
#84784=CARTESIAN_POINT('Ctrl Pts',(20.6994287137937,-19.7419597422966,-9.15963173410604));
#84785=CARTESIAN_POINT('Ctrl Pts',(20.6711526578599,-19.8089846766148,-9.16401994303694));
#84786=CARTESIAN_POINT('Ctrl Pts',(20.6394473542677,-19.8744745959181,-9.16840815196783));
#84787=CARTESIAN_POINT('Ctrl Pts',(20.6077891066028,-19.9398673173227,-9.1727898480691));
#84788=CARTESIAN_POINT('Ctrl Pts',(20.5727119232316,-20.0037291156991,-9.17717154417037));
#84789=CARTESIAN_POINT('Ctrl Pts',(20.5343896652635,-20.0656813068433,-9.18155324027163));
#84790=CARTESIAN_POINT('Ctrl Pts',(20.4961124389984,-20.1275606992326,-9.18592978753127));
#84791=CARTESIAN_POINT('Ctrl Pts',(20.4545979656272,-20.187534533793,-9.19030633479091));
#84792=CARTESIAN_POINT('Ctrl Pts',(20.4100662428249,-20.2452482165706,-9.19468288205055));
#84793=CARTESIAN_POINT('Ctrl Pts',(20.3655627613939,-20.3029252981693,-9.19905665376752));
#84794=CARTESIAN_POINT('Ctrl Pts',(20.3180461211088,-20.3583446909811,-9.20343042548449));
#84795=CARTESIAN_POINT('Ctrl Pts',(20.2677790950909,-20.4111815128565,-9.20780419720147));
#84796=CARTESIAN_POINT('Ctrl Pts',(20.2175273654978,-20.4640022563096,-9.21217663796502));
#84797=CARTESIAN_POINT('Ctrl Pts',(20.1645272440667,-20.5142416397749,-9.21654907872857));
#84798=CARTESIAN_POINT('Ctrl Pts',(20.1090800563605,-20.5616098404892,-9.22092151949212));
#84799=CARTESIAN_POINT('Ctrl Pts',(20.0536314508636,-20.6089792524137,-9.22529407205947));
#84800=CARTESIAN_POINT('Ctrl Pts',(19.9957360229243,-20.6534770240217,-9.22966662462681));
#84801=CARTESIAN_POINT('Ctrl Pts',(19.9357287478819,-20.6948531253419,-9.23403917719415));
#84802=CARTESIAN_POINT('Ctrl Pts',(19.8756591950261,-20.7362721683408,-9.23841626776148));
#84803=CARTESIAN_POINT('Ctrl Pts',(19.8134738170561,-20.7745627981878,-9.24279335832881));
#84804=CARTESIAN_POINT('Ctrl Pts',(19.7495364985931,-20.8095184036841,-9.24717044889614));
#84805=CARTESIAN_POINT('Ctrl Pts',(19.6855642615875,-20.844493099734,-9.25154992995508));
#84806=CARTESIAN_POINT('Ctrl Pts',(19.61983861406,-20.8761289357272,-9.25592941101402));
#84807=CARTESIAN_POINT('Ctrl Pts',(19.552745510241,-20.9042665774582,-9.26030889207296));
#84808=CARTESIAN_POINT('Ctrl Pts',(19.4855334843459,-20.9324540929702,-9.26469613573268));
#84809=CARTESIAN_POINT('Ctrl Pts',(19.4169496162063,-20.957130868566,-9.2690833793924));
#84810=CARTESIAN_POINT('Ctrl Pts',(19.3473966187367,-20.9781869578404,-9.27347062305212));
#84811=CARTESIAN_POINT('Ctrl Pts',(19.3001072825683,-20.992503069587,-9.27645352598693));
#84812=CARTESIAN_POINT('Ctrl Pts',(19.2523702507339,-21.0051465017728,-9.27943642892175));
#84813=CARTESIAN_POINT('Ctrl Pts',(19.2043142751594,-21.0160962871391,-9.28241933185657));
#84814=CARTESIAN_POINT('Ctrl Pts',(19.1336181560407,-21.0322047381968,-9.28680754078747));
#84815=CARTESIAN_POINT('Ctrl Pts',(19.0619555004258,-21.0447083756574,-9.29119574971836));
#84816=CARTESIAN_POINT('Ctrl Pts',(18.9897273628003,-21.0534976840138,-9.29558395864926));
#84817=CARTESIAN_POINT('Ctrl Pts',(18.9176064237068,-21.0622739475792,-9.29996565475053));
#84818=CARTESIAN_POINT('Ctrl Pts',(18.8449221435535,-21.0673467676749,-9.30434735085179));
#84819=CARTESIAN_POINT('Ctrl Pts',(18.772087043549,-21.0686573594027,-9.30872904695306));
#84820=CARTESIAN_POINT('Ctrl Pts',(18.6993375305834,-21.0699664110809,-9.3131055942127));
#84821=CARTESIAN_POINT('Ctrl Pts',(18.6264380297317,-21.0675220079374,-9.31748214147234));
#84822=CARTESIAN_POINT('Ctrl Pts',(18.5538057789621,-21.0613171982195,-9.32185868873198));
#84823=CARTESIAN_POINT('Ctrl Pts',(18.4812195905103,-21.0551163235017,-9.32623246044895));
#84824=CARTESIAN_POINT('Ctrl Pts',(18.4089007953027,-21.0451598149104,-9.33060623216593));
#84825=CARTESIAN_POINT('Ctrl Pts',(18.3372648019199,-21.0314927705102,-9.3349800038829));
#84826=CARTESIAN_POINT('Ctrl Pts',(18.2656506076104,-21.0178298850376,-9.33935244464645));
#84827=CARTESIAN_POINT('Ctrl Pts',(18.194719276167,-21.0004587957696,-9.34372488541));
#84828=CARTESIAN_POINT('Ctrl Pts',(18.1248776044803,-20.979475994254,-9.34809732617356));
#84829=CARTESIAN_POINT('Ctrl Pts',(18.0550341469343,-20.9584926562059,-9.3524698787409));
#84830=CARTESIAN_POINT('Ctrl Pts',(17.9862808658671,-20.9338975632636,-9.35684243130824));
#84831=CARTESIAN_POINT('Ctrl Pts',(17.9190093127144,-20.9058370401949,-9.36121498387559));
#84832=CARTESIAN_POINT('Ctrl Pts',(17.8516679426063,-20.877747394857,-9.36559207444291));
#84833=CARTESIAN_POINT('Ctrl Pts',(17.7858118168723,-20.8461853247306,-9.36996916501024));
#84834=CARTESIAN_POINT('Ctrl Pts',(17.7218116266775,-20.8113449644729,-9.37434625557757));
#84835=CARTESIAN_POINT('Ctrl Pts',(17.6577764836036,-20.7764855766014,-9.37872573663651));
#84836=CARTESIAN_POINT('Ctrl Pts',(17.5955997055917,-20.738344586342,-9.38310521769546));
#84837=CARTESIAN_POINT('Ctrl Pts',(17.5356241771984,-20.6971602755405,-9.3874846987544));
#84838=CARTESIAN_POINT('Ctrl Pts',(17.4755423425837,-20.6559029658246,-9.39187194241412));
#84839=CARTESIAN_POINT('Ctrl Pts',(17.417669932464,-20.6115918569496,-9.39625918607384));
#84840=CARTESIAN_POINT('Ctrl Pts',(17.3623173752293,-20.564506054842,-9.40064642973356));
#84841=CARTESIAN_POINT('Ctrl Pts',(17.3246829700694,-20.532492246586,-9.40362933266838));
#84842=CARTESIAN_POINT('Ctrl Pts',(17.2882126945401,-20.4991966074029,-9.40661223560319));
#84843=CARTESIAN_POINT('Ctrl Pts',(17.2529938697634,-20.4647160481073,-9.40959513853801));
#84844=CARTESIAN_POINT('Ctrl Pts',(17.201926340437,-20.4147190086213,-9.41392036756161));
#84845=CARTESIAN_POINT('Ctrl Pts',(17.153279990606,-20.3620217118529,-9.41824559658522));
#84846=CARTESIAN_POINT('Ctrl Pts',(17.1073599831676,-20.3068916029112,-9.42257082560882));
#84847=CARTESIAN_POINT('Ctrl Pts',(17.0615168757444,-20.2518538176963,-9.4268888113806));
#84848=CARTESIAN_POINT('Ctrl Pts',(17.0183913618816,-20.194391687294,-9.43120679715237));
#84849=CARTESIAN_POINT('Ctrl Pts',(16.9782524640737,-20.1348100397311,-9.43552478292415));
#84850=CARTESIAN_POINT('Ctrl Pts',(16.9381523085283,-20.075285900669,-9.43983860095472));
#84851=CARTESIAN_POINT('Ctrl Pts',(16.9010333312299,-20.0136467098988,-9.44415241898528));
#84852=CARTESIAN_POINT('Ctrl Pts',(16.8671239501054,-19.9502298404326,-9.44846623701585));
#84853=CARTESIAN_POINT('Ctrl Pts',(16.8332351489702,-19.886851459386,-9.45277743694118));
#84854=CARTESIAN_POINT('Ctrl Pts',(16.8025523148356,-19.8216979770288,-9.4570886368665));
#84855=CARTESIAN_POINT('Ctrl Pts',(16.7752592184707,-19.755133582148,-9.46139983679183));
#84856=CARTESIAN_POINT('Ctrl Pts',(16.7648137941534,-19.729658519163,-9.46304978929024));
#84857=CARTESIAN_POINT('Ctrl Pts',(16.7548643808522,-19.7039770531934,-9.46469974178865));
#84858=CARTESIAN_POINT('Ctrl Pts',(16.7454194499637,-19.6781104571739,-9.46634969428706));
#84859=CARTESIAN_POINT('',(16.6170008950802,-18.9500532671891,-8.48905627902251));
#84860=CARTESIAN_POINT('Ctrl Pts',(16.7454193049359,-19.6781100599899,-9.24346979696294));
#84861=CARTESIAN_POINT('Ctrl Pts',(16.7776919679286,-19.7664944498252,-9.23734829963788));
#84862=CARTESIAN_POINT('Ctrl Pts',(16.8158509947677,-19.8527102299079,-9.23135282091049));
#84863=CARTESIAN_POINT('Ctrl Pts',(16.870699146144,-19.9571673936568,-9.22408567207777));
#84864=CARTESIAN_POINT('Ctrl Pts',(16.8820779974327,-19.9779807646683,-9.22263707125759));
#84865=CARTESIAN_POINT('Ctrl Pts',(16.8985836849794,-20.0070020846846,-9.22061560073741));
#84866=CARTESIAN_POINT('Ctrl Pts',(16.9034203307547,-20.0153722431622,-9.22003238534716));
#84867=CARTESIAN_POINT('Ctrl Pts',(16.9113459968973,-20.0288738325939,-9.21909122021068));
#84868=CARTESIAN_POINT('Ctrl Pts',(16.9143997169755,-20.0340257286749,-9.21873199734405));
#84869=CARTESIAN_POINT('Ctrl Pts',(16.9208165154469,-20.0447474470033,-9.21798418043392));
#84870=CARTESIAN_POINT('Ctrl Pts',(16.9241834957213,-20.0503148701018,-9.21759573377162));
#84871=CARTESIAN_POINT('Ctrl Pts',(16.9322157277914,-20.0634592247858,-9.21667827532294));
#84872=CARTESIAN_POINT('Ctrl Pts',(16.9369032114755,-20.0710224789062,-9.21615008615486));
#84873=CARTESIAN_POINT('Ctrl Pts',(16.9526728496646,-20.0961121277849,-9.21439677543285));
#84874=CARTESIAN_POINT('Ctrl Pts',(16.9639650239576,-20.1135055772994,-9.21317942997755));
#84875=CARTESIAN_POINT('Ctrl Pts',(17.0256090451949,-20.2054691714003,-9.20672827219186));
#84876=CARTESIAN_POINT('Ctrl Pts',(17.0804235748791,-20.2769423779121,-9.20166741840291));
#84877=CARTESIAN_POINT('Ctrl Pts',(17.2287762363623,-20.4467756329287,-9.18922995126064));
#84878=CARTESIAN_POINT('Ctrl Pts',(17.3275154071975,-20.5400338848918,-9.18201734532298));
#84879=CARTESIAN_POINT('Ctrl Pts',(17.4939965849843,-20.6694875077123,-9.17034163101494));
#84880=CARTESIAN_POINT('Ctrl Pts',(17.5559297040637,-20.7125452644636,-9.16608158963595));
#84881=CARTESIAN_POINT('Ctrl Pts',(17.628088335483,-20.7571976182767,-9.16105236809672));
#84882=CARTESIAN_POINT('Ctrl Pts',(17.6361911110664,-20.7621366485825,-9.16048672412422));
#84883=CARTESIAN_POINT('Ctrl Pts',(17.6482528193402,-20.7693780648497,-9.15964295207999));
#84884=CARTESIAN_POINT('Ctrl Pts',(17.6521865875829,-20.7717224268327,-9.15936749146939));
#84885=CARTESIAN_POINT('Ctrl Pts',(17.6592019909693,-20.7758725276173,-9.15887569444401));
#84886=CARTESIAN_POINT('Ctrl Pts',(17.6622806197075,-20.7776832493309,-9.15865968652276));
#84887=CARTESIAN_POINT('Ctrl Pts',(17.6689127423215,-20.7815614323407,-9.15819393177831));
#84888=CARTESIAN_POINT('Ctrl Pts',(17.6724676284311,-20.7836263059437,-9.15794402899267));
#84889=CARTESIAN_POINT('Ctrl Pts',(17.6823047444223,-20.7893019877147,-9.15725184545361));
#84890=CARTESIAN_POINT('Ctrl Pts',(17.688599463882,-20.7928908767911,-9.15680819102671));
#84891=CARTESIAN_POINT('Ctrl Pts',(17.7233171356835,-20.8124494202391,-9.15435780236056));
#84892=CARTESIAN_POINT('Ctrl Pts',(17.7520859964798,-20.8277922370323,-9.15231457852842));
#84893=CARTESIAN_POINT('Ctrl Pts',(17.9264392723837,-20.9156672650139,-9.139907154325));
#84894=CARTESIAN_POINT('Ctrl Pts',(18.0796307715685,-20.9718872018195,-9.12895410545955));
#84895=CARTESIAN_POINT('Ctrl Pts',(18.3512845860962,-21.0373916249034,-9.11070140547799));
#84896=CARTESIAN_POINT('Ctrl Pts',(18.4669069766484,-21.0553303203647,-9.1032618877738));
#84897=CARTESIAN_POINT('Ctrl Pts',(18.5976892024241,-21.0646553302264,-9.09525606163682));
#84898=CARTESIAN_POINT('Ctrl Pts',(18.6119522891808,-21.0655272768218,-9.09438810180259));
#84899=CARTESIAN_POINT('Ctrl Pts',(18.6346668639344,-21.0666851788318,-9.09301381397604));
#84900=CARTESIAN_POINT('Ctrl Pts',(18.6431129331723,-21.067065015978,-9.09250455805295));
#84901=CARTESIAN_POINT('Ctrl Pts',(18.6580129559602,-21.0676456835164,-9.09160918539496));
#84902=CARTESIAN_POINT('Ctrl Pts',(18.6644659349539,-21.0678676008376,-9.09122241255801));
#84903=CARTESIAN_POINT('Ctrl Pts',(18.6778149090636,-21.0682655360733,-9.09042434286681));
#84904=CARTESIAN_POINT('Ctrl Pts',(18.6847109590881,-21.0684373781884,-9.09001318140611));
#84905=CARTESIAN_POINT('Ctrl Pts',(18.7024144118008,-21.0687919549537,-9.08896046175823));
#84906=CARTESIAN_POINT('Ctrl Pts',(18.7132226813714,-21.0689256339154,-9.08832044492973));
#84907=CARTESIAN_POINT('Ctrl Pts',(18.7583376119597,-21.0691380695254,-9.08565970126129));
#84908=CARTESIAN_POINT('Ctrl Pts',(18.7926437411782,-21.0684656937997,-9.0836625049292));
#84909=CARTESIAN_POINT('Ctrl Pts',(18.881974433319,-21.0645409869583,-9.07851821178175));
#84910=CARTESIAN_POINT('Ctrl Pts',(18.9369160470631,-21.0599733342275,-9.07541050829213));
#84911=CARTESIAN_POINT('Ctrl Pts',(19.1001558930883,-21.0399597647981,-9.06626584573491));
#84912=CARTESIAN_POINT('Ctrl Pts',(19.2075006717982,-21.0182633217052,-9.0603776152195));
#84913=CARTESIAN_POINT('Ctrl Pts',(19.3568854813903,-20.9758117003682,-9.05192244406373));
#84914=CARTESIAN_POINT('Ctrl Pts',(19.4006606512077,-20.9618167718137,-9.04941010653216));
#84915=CARTESIAN_POINT('Ctrl Pts',(19.4649346690079,-20.9389373236352,-9.0456264925304));
#84916=CARTESIAN_POINT('Ctrl Pts',(19.4858051398379,-20.9311347608811,-9.04438268387586));
#84917=CARTESIAN_POINT('Ctrl Pts',(19.5544069538365,-20.9042458326511,-9.04023204677506));
#84918=CARTESIAN_POINT('Ctrl Pts',(19.6015626744835,-20.8837519108841,-9.0372783279366));
#84919=CARTESIAN_POINT('Ctrl Pts',(19.6550271847821,-20.858163680944,-9.03376033623064));
#84920=CARTESIAN_POINT('Ctrl Pts',(19.6621135638716,-20.8547233802766,-9.03329054236549));
#84921=CARTESIAN_POINT('Ctrl Pts',(19.6733812317493,-20.8491752229195,-9.03253768384218));
#84922=CARTESIAN_POINT('Ctrl Pts',(19.677575090663,-20.8470928664156,-9.03225616440731));
#84923=CARTESIAN_POINT('Ctrl Pts',(19.6849748640897,-20.8433880400916,-9.03175707545887));
#84924=CARTESIAN_POINT('Ctrl Pts',(19.6881835993648,-20.8417713006821,-9.0315398658903));
#84925=CARTESIAN_POINT('Ctrl Pts',(19.6949586570297,-20.8383359946607,-9.0310795427533));
#84926=CARTESIAN_POINT('Ctrl Pts',(19.6985238859734,-20.8365155075098,-9.03083631431778));
#84927=CARTESIAN_POINT('Ctrl Pts',(19.7080942340707,-20.8315943974037,-9.0301807723508));
#84928=CARTESIAN_POINT('Ctrl Pts',(19.714089645224,-20.8284751424081,-9.02976731099744));
#84929=CARTESIAN_POINT('Ctrl Pts',(19.7432925091862,-20.8131035273658,-9.02774010670412));
#84930=CARTESIAN_POINT('Ctrl Pts',(19.7662845820032,-20.8004496487409,-9.02610292272586));
#84931=CARTESIAN_POINT('Ctrl Pts',(19.8314666132126,-20.7629808081381,-9.02135531277092));
#84932=CARTESIAN_POINT('Ctrl Pts',(19.8730376703919,-20.7371266082566,-9.01819732379401));
#84933=CARTESIAN_POINT('Ctrl Pts',(19.993928502925,-20.6559985117303,-9.00869694294965));
#84934=CARTESIAN_POINT('Ctrl Pts',(20.0704008099772,-20.5967077052518,-9.00226771860933));
#84935=CARTESIAN_POINT('Ctrl Pts',(20.2478287560177,-20.4385725247757,-8.98663170183146));
#84936=CARTESIAN_POINT('Ctrl Pts',(20.3434811410304,-20.3344468098612,-8.97756399134499));
#84937=CARTESIAN_POINT('Ctrl Pts',(20.4366435908121,-20.210132659946,-8.96807848728317));
#84938=CARTESIAN_POINT('Ctrl Pts',(20.4450930131601,-20.1986169032086,-8.96721093793812));
#84939=CARTESIAN_POINT('Ctrl Pts',(20.4583564388408,-20.1801511782516,-8.96583717516303));
#84940=CARTESIAN_POINT('Ctrl Pts',(20.4632463588114,-20.1732565162926,-8.96532803728183));
#84941=CARTESIAN_POINT('Ctrl Pts',(20.4717983602435,-20.1610440620952,-8.96443280191692));
#84942=CARTESIAN_POINT('Ctrl Pts',(20.4754776284878,-20.1557384914763,-8.96404604896419));
#84943=CARTESIAN_POINT('Ctrl Pts',(20.4830379944307,-20.1447290926685,-8.96324795301442));
#84944=CARTESIAN_POINT('Ctrl Pts',(20.4869156019338,-20.1390229520482,-8.96283674574297));
#84945=CARTESIAN_POINT('Ctrl Pts',(20.4967986457271,-20.1243253993542,-8.96178376947603));
#84946=CARTESIAN_POINT('Ctrl Pts',(20.5027632638387,-20.1153066794308,-8.96114354331472));
#84947=CARTESIAN_POINT('Ctrl Pts',(20.52738030171,-20.0774577550668,-8.95848076421811));
#84948=CARTESIAN_POINT('Ctrl Pts',(20.545399614189,-20.0482206437836,-8.95648178776577));
#84949=CARTESIAN_POINT('Ctrl Pts',(20.5904987951057,-19.9708943430114,-8.95133187211742));
#84950=CARTESIAN_POINT('Ctrl Pts',(20.6164243625228,-19.9221611337104,-8.94822043926862));
#84951=CARTESIAN_POINT('Ctrl Pts',(20.6879870509115,-19.7739447883822,-8.93906927114948));
#84952=CARTESIAN_POINT('Ctrl Pts',(20.7278487032641,-19.6718797507182,-8.93317824260384));
#84953=CARTESIAN_POINT('Ctrl Pts',(20.7744408176174,-19.5184657484256,-8.92444873437601));
#84954=CARTESIAN_POINT('Ctrl Pts',(20.7874754897926,-19.4692235853106,-8.92166296549719));
#84955=CARTESIAN_POINT('Ctrl Pts',(20.8021906400655,-19.40424238805,-8.91795609658116));
#84956=CARTESIAN_POINT('Ctrl Pts',(20.8054889807911,-19.3888856673185,-8.91707782644251));
#84957=CARTESIAN_POINT('Ctrl Pts',(20.8191178653758,-19.321803557602,-8.91322621815388));
#84958=CARTESIAN_POINT('Ctrl Pts',(20.8276832231,-19.2697432242618,-8.91019826366661));
#84959=CARTESIAN_POINT('Ctrl Pts',(20.8353850229457,-19.2087986388804,-8.9065526623584));
#84960=CARTESIAN_POINT('Ctrl Pts',(20.836421686752,-19.2001684927691,-8.90603407633398));
#84961=CARTESIAN_POINT('Ctrl Pts',(20.8379117366104,-19.1870839210295,-8.90524394221665));
#84962=CARTESIAN_POINT('Ctrl Pts',(20.8384042008505,-19.1826339176486,-8.90497454194854));
#84963=CARTESIAN_POINT('Ctrl Pts',(20.8392632772108,-19.1746392435701,-8.90448927664491));
#84964=CARTESIAN_POINT('Ctrl Pts',(20.839635058539,-19.1710951827401,-8.90427370566166));
#84965=CARTESIAN_POINT('Ctrl Pts',(20.8404239563872,-19.1633873841434,-8.90380387821813));
#84966=CARTESIAN_POINT('Ctrl Pts',(20.8408376712661,-19.1592233974523,-8.90354943881656));
#84967=CARTESIAN_POINT('Ctrl Pts',(20.8419662917948,-19.1475111267443,-8.90283206069093));
#84968=CARTESIAN_POINT('Ctrl Pts',(20.8426529866115,-19.1399602779432,-8.90236758282333));
#84969=CARTESIAN_POINT('Ctrl Pts',(20.8465378362426,-19.0945387942675,-8.89956227505961));
#84970=CARTESIAN_POINT('Ctrl Pts',(20.8487560451338,-19.0565938410345,-8.89717169067059));
#84971=CARTESIAN_POINT('Ctrl Pts',(20.8527120495246,-18.9309312712568,-8.88914350123471));
#84972=CARTESIAN_POINT('Ctrl Pts',(20.8500194730265,-18.8431685016411,-8.88336090965856));
#84973=CARTESIAN_POINT('Ctrl Pts',(20.825729171169,-18.5821608169637,-8.86604055244744));
#84974=CARTESIAN_POINT('Ctrl Pts',(20.7881616998726,-18.4111167304525,-8.85459338872171));
#84975=CARTESIAN_POINT('Ctrl Pts',(20.7223353808918,-18.2248525273578,-8.84243270523744));
#84976=CARTESIAN_POINT('Ctrl Pts',(20.714294527328,-18.2032312206241,-8.84102454648127));
#84977=CARTESIAN_POINT('Ctrl Pts',(20.7024238956251,-18.1728416523365,-8.83904951700229));
#84978=CARTESIAN_POINT('Ctrl Pts',(20.698885827654,-18.1639618964964,-8.83847292654427));
#84979=CARTESIAN_POINT('Ctrl Pts',(20.6930407959344,-18.1495763031934,-8.83753956930673));
#84980=CARTESIAN_POINT('Ctrl Pts',(20.6907705019473,-18.1440557982293,-8.83718157032278));
#84981=CARTESIAN_POINT('Ctrl Pts',(20.6859705802597,-18.1325230950597,-8.83643403188766));
#84982=CARTESIAN_POINT('Ctrl Pts',(20.6834364509379,-18.1265128292017,-8.83604464979026));
#84983=CARTESIAN_POINT('Ctrl Pts',(20.6773439849278,-18.1122476802427,-8.83512088673321));
#84984=CARTESIAN_POINT('Ctrl Pts',(20.6737607510275,-18.1040035171879,-8.83458735986114));
#84985=CARTESIAN_POINT('Ctrl Pts',(20.6615229506852,-18.0763307502198,-8.83279743296948));
#84986=CARTESIAN_POINT('Ctrl Pts',(20.6526279629415,-18.0570094141352,-8.83154926868361));
#84987=CARTESIAN_POINT('Ctrl Pts',(20.5767423400352,-17.8985066588994,-8.82131512662616));
#84988=CARTESIAN_POINT('Ctrl Pts',(20.4949941348804,-17.7669030984535,-8.81289767166638));
#84989=CARTESIAN_POINT('Ctrl Pts',(20.3152266158616,-17.5377449928549,-8.79708097714466));
#84990=CARTESIAN_POINT('Ctrl Pts',(20.2205923616352,-17.438584127056,-8.78969553452319));
#84991=CARTESIAN_POINT('Ctrl Pts',(20.105275088571,-17.3390720501843,-8.78076350845691));
#84992=CARTESIAN_POINT('Ctrl Pts',(20.0933630792143,-17.3290200473233,-8.77984139796247));
#84993=CARTESIAN_POINT('Ctrl Pts',(20.0768874921386,-17.3154256726584,-8.77856503898545));
#84994=CARTESIAN_POINT('Ctrl Pts',(20.0724184651143,-17.3117688102227,-8.77821872732565));
#84995=CARTESIAN_POINT('Ctrl Pts',(20.065288234416,-17.305982912755,-8.77766593871028));
#84996=CARTESIAN_POINT('Ctrl Pts',(20.0626367164115,-17.3038419098822,-8.77746031732908));
#84997=CARTESIAN_POINT('Ctrl Pts',(20.057145634574,-17.2994299257566,-8.77703434926696));
#84998=CARTESIAN_POINT('Ctrl Pts',(20.0543053941631,-17.29715986091,-8.7768139373675));
#84999=CARTESIAN_POINT('Ctrl Pts',(20.0475167861269,-17.2917626611136,-8.77628694959207));
#85000=CARTESIAN_POINT('Ctrl Pts',(20.0435630911632,-17.2886422880421,-8.77597989611487));
#85001=CARTESIAN_POINT('Ctrl Pts',(20.0301589952398,-17.2781407912089,-8.77493855608421));
#85002=CARTESIAN_POINT('Ctrl Pts',(20.0206572296242,-17.2708260203101,-8.77419980372735));
#85003=CARTESIAN_POINT('Ctrl Pts',(19.9093861176051,-17.1866616909484,-8.76554694658337));
#85004=CARTESIAN_POINT('Ctrl Pts',(19.8009453235383,-17.1190862529271,-8.75711389995272));
#85005=CARTESIAN_POINT('Ctrl Pts',(19.5397089949247,-16.9873707398854,-8.73778010492853));
#85006=CARTESIAN_POINT('Ctrl Pts',(19.3841063340161,-16.9305360372442,-8.72698434280298));
#85007=CARTESIAN_POINT('Ctrl Pts',(19.2004906969226,-16.8869012971584,-8.71536072261149));
#85008=CARTESIAN_POINT('Ctrl Pts',(19.1774343424353,-16.8818279594354,-8.71391911587544));
#85009=CARTESIAN_POINT('Ctrl Pts',(19.1448412695825,-16.8752256899708,-8.71190568322891));
#85010=CARTESIAN_POINT('Ctrl Pts',(19.1353722358856,-16.8733748734631,-8.71132362107856));
#85011=CARTESIAN_POINT('Ctrl Pts',(19.120008820235,-16.8704808395037,-8.71038381615215));
#85012=CARTESIAN_POINT('Ctrl Pts',(19.1141221656495,-16.8693977899901,-8.71002480740888));
#85013=CARTESIAN_POINT('Ctrl Pts',(19.1018244426444,-16.8671890861126,-8.70927704567564));
#85014=CARTESIAN_POINT('Ctrl Pts',(19.0954126087906,-16.8660680032807,-8.70888844178058));
#85015=CARTESIAN_POINT('Ctrl Pts',(19.0802085013706,-16.8634818359437,-8.70796991305197));
#85016=CARTESIAN_POINT('Ctrl Pts',(19.0714118998477,-16.8620426651347,-8.70744081617181));
#85017=CARTESIAN_POINT('Ctrl Pts',(19.0426186522532,-16.8575184651841,-8.70571639578555));
#85018=CARTESIAN_POINT('Ctrl Pts',(19.0225864536086,-16.8546644825232,-8.70452838408815));
#85019=CARTESIAN_POINT('Ctrl Pts',(18.974920071101,-16.848569349772,-8.70172733448518));
#85020=CARTESIAN_POINT('Ctrl Pts',(18.9472565402445,-16.8455848630125,-8.70012225584048));
#85021=CARTESIAN_POINT('Ctrl Pts',(18.7508329874053,-16.8283031137888,-8.68885155263308));
#85022=CARTESIAN_POINT('Ctrl Pts',(18.5809584419909,-16.8337571618947,-8.67982435317146));
#85023=CARTESIAN_POINT('Ctrl Pts',(18.310787758827,-16.8751305967414,-8.66488752605422));
#85024=CARTESIAN_POINT('Ctrl Pts',(18.2093449552684,-16.898411345124,-8.65912326062646));
#85025=CARTESIAN_POINT('Ctrl Pts',(18.1007796340158,-16.9318973238039,-8.65239231633011));
#85026=CARTESIAN_POINT('Ctrl Pts',(18.0915420562897,-16.9348161618779,-8.65181500406995));
#85027=CARTESIAN_POINT('Ctrl Pts',(18.0779311512388,-16.9392198349403,-8.65095713553893));
#85028=CARTESIAN_POINT('Ctrl Pts',(18.0735419767694,-16.9406557913186,-8.65067937776165));
#85029=CARTESIAN_POINT('Ctrl Pts',(18.0657629053151,-16.9432289901408,-8.65018505739779));
#85030=CARTESIAN_POINT('Ctrl Pts',(18.0623711540428,-16.9443604711422,-8.64996883632028));
#85031=CARTESIAN_POINT('Ctrl Pts',(18.0551094912353,-16.9468034079696,-8.64950440934813));
#85032=CARTESIAN_POINT('Ctrl Pts',(18.0512405635853,-16.9481174568066,-8.64925605686877));
#85033=CARTESIAN_POINT('Ctrl Pts',(18.0406289366111,-16.9517559059967,-8.64857242336353));
#85034=CARTESIAN_POINT('Ctrl Pts',(18.0338942138201,-16.9541031678388,-8.64813582291551));
#85035=CARTESIAN_POINT('Ctrl Pts',(17.9984775044218,-16.9666480640225,-8.64582590065809));
#85036=CARTESIAN_POINT('Ctrl Pts',(17.9700076578876,-16.9774288745619,-8.64392087630941));
#85037=CARTESIAN_POINT('Ctrl Pts',(17.7914210963493,-17.0494953350584,-8.63170745259291));
#85038=CARTESIAN_POINT('Ctrl Pts',(17.6485335844143,-17.1272422377809,-8.62079146652433));
#85039=CARTESIAN_POINT('Ctrl Pts',(17.4180930488449,-17.2893560683257,-8.60236920542641));
#85040=CARTESIAN_POINT('Ctrl Pts',(17.3262604599594,-17.3663538582294,-8.59474158434334));
#85041=CARTESIAN_POINT('Ctrl Pts',(17.2302711945353,-17.4617867664482,-8.58647638876815));
#85042=CARTESIAN_POINT('Ctrl Pts',(17.2192537691698,-17.4729869240252,-8.58552258211336));
#85043=CARTESIAN_POINT('Ctrl Pts',(17.2027731923366,-17.490118184151,-8.58408765426244));
#85044=CARTESIAN_POINT('Ctrl Pts',(17.1972177503297,-17.495959375594,-8.58360251642554));
#85045=CARTESIAN_POINT('Ctrl Pts',(17.1873222630543,-17.5064835730841,-8.58273572702831));
#85046=CARTESIAN_POINT('Ctrl Pts',(17.1829698067502,-17.5111547260519,-8.58235354278634));
#85047=CARTESIAN_POINT('Ctrl Pts',(17.1737790493218,-17.5211083560604,-8.58154448373944));
#85048=CARTESIAN_POINT('Ctrl Pts',(17.1689462847743,-17.5263958536727,-8.58111784772801));
#85049=CARTESIAN_POINT('Ctrl Pts',(17.1591629011719,-17.5372095009902,-8.58025163733869));
#85050=CARTESIAN_POINT('Ctrl Pts',(17.1542143063962,-17.54273735296,-8.57981215120182));
#85051=CARTESIAN_POINT('Ctrl Pts',(17.132425659083,-17.5673354613014,-8.57787095716848));
#85052=CARTESIAN_POINT('Ctrl Pts',(17.1159006593686,-17.5866828719498,-8.57638235546039));
#85053=CARTESIAN_POINT('Ctrl Pts',(17.0457286191984,-17.6719041411568,-8.56998123517883));
#85054=CARTESIAN_POINT('Ctrl Pts',(16.9957224890905,-17.7406787534278,-8.56521401094969));
#85055=CARTESIAN_POINT('Ctrl Pts',(16.9128101522339,-17.8704624229312,-8.55672636428035));
#85056=CARTESIAN_POINT('Ctrl Pts',(16.8785074359584,-17.9304307705728,-8.55298123350471));
#85057=CARTESIAN_POINT('Ctrl Pts',(16.7878577129973,-18.108589850488,-8.54212537034257));
#85058=CARTESIAN_POINT('Ctrl Pts',(16.7394673001256,-18.2304457765856,-8.53503483493165));
#85059=CARTESIAN_POINT('Ctrl Pts',(16.6982006722164,-18.3710882901915,-8.52644200352335));
#85060=CARTESIAN_POINT('Ctrl Pts',(16.6939331602486,-18.3862575020306,-8.52550990850784));
#85061=CARTESIAN_POINT('Ctrl Pts',(16.6883270785526,-18.4070734496436,-8.52422183350569));
#85062=CARTESIAN_POINT('Ctrl Pts',(16.6868416776032,-18.4126805695452,-8.52387397958134));
#85063=CARTESIAN_POINT('Ctrl Pts',(16.6845188928767,-18.4215965300107,-8.52331933758435));
#85064=CARTESIAN_POINT('Ctrl Pts',(16.6836664224205,-18.4249014611092,-8.52311341540417));
#85065=CARTESIAN_POINT('Ctrl Pts',(16.6819231281433,-18.4317282354038,-8.52268734811974));
#85066=CARTESIAN_POINT('Ctrl Pts',(16.6810333787528,-18.4352503040055,-8.52246714014281));
#85067=CARTESIAN_POINT('Ctrl Pts',(16.6789361654079,-18.4436430218554,-8.52194150042947));
#85068=CARTESIAN_POINT('Ctrl Pts',(16.6777369494926,-18.4485156929909,-8.52163559751192));
#85069=CARTESIAN_POINT('Ctrl Pts',(16.675232597529,-18.4588496058647,-8.5209853740746));
#85070=CARTESIAN_POINT('Ctrl Pts',(16.6739318448418,-18.4643118586532,-8.52064081548478));
#85071=CARTESIAN_POINT('Ctrl Pts',(16.6704195265389,-18.4793259488364,-8.51969147306472));
#85072=CARTESIAN_POINT('Ctrl Pts',(16.6682525934496,-18.4888879472955,-8.51908436631309));
#85073=CARTESIAN_POINT('Ctrl Pts',(16.6336164634003,-18.646807751159,-8.50902048411727));
#85074=CARTESIAN_POINT('Ctrl Pts',(16.6171414698365,-18.7982035803618,-8.49886432225171));
#85075=CARTESIAN_POINT('Ctrl Pts',(16.6170009071471,-18.950040188799,-8.48885784002949));
#85076=CARTESIAN_POINT('Ctrl Pts',(16.6170008950802,-18.9500532671891,-8.48905627902251));
#85077=CARTESIAN_POINT('Ctrl Pts',(16.6169347305481,-19.0220047205615,-8.48473008583426));
#85078=CARTESIAN_POINT('Ctrl Pts',(16.6205409900205,-19.09405109857,-8.48040389264601));
#85079=CARTESIAN_POINT('Ctrl Pts',(16.6278220014955,-19.1657831579326,-8.47607769945775));
#85080=CARTESIAN_POINT('Ctrl Pts',(16.6350980157525,-19.2374659850227,-8.47175447549029));
#85081=CARTESIAN_POINT('Ctrl Pts',(16.6460437282404,-19.3088344307521,-8.46743125152283));
#85082=CARTESIAN_POINT('Ctrl Pts',(16.6606094541866,-19.3794817476005,-8.46310802755537));
#85083=CARTESIAN_POINT('Ctrl Pts',(16.6751723924897,-19.4501155437014,-8.45878563098267));
#85084=CARTESIAN_POINT('Ctrl Pts',(16.6933538757661,-19.520027999392,-8.45446323440996));
#85085=CARTESIAN_POINT('Ctrl Pts',(16.7150529432357,-19.5888216249334,-8.45014083783726));
#85086=CARTESIAN_POINT('Ctrl Pts',(16.7245112166523,-19.6188076563883,-8.44825677490891));
#85087=CARTESIAN_POINT('Ctrl Pts',(16.7346371622268,-19.6485812753992,-8.44637271198055));
#85088=CARTESIAN_POINT('Ctrl Pts',(16.7454194499637,-19.6781104571739,-8.4444886490522));
#85089=CARTESIAN_POINT('Origin',(18.734,-18.952,0.));
#85090=CARTESIAN_POINT('',(16.7430902533864,-19.6789409674447,-7.64456001990001));
#85091=CARTESIAN_POINT('',(16.7454194590822,-19.6781104821466,-7.86510586795993));
#85092=CARTESIAN_POINT('',(16.7454194499637,-19.6781104571739,0.));
#85093=CARTESIAN_POINT('Ctrl Pts',(16.7454194590822,-19.6781104821466,-7.86510586795993));
#85094=CARTESIAN_POINT('Ctrl Pts',(16.7304230320966,-19.6370401442019,-7.86752224800844));
#85095=CARTESIAN_POINT('Ctrl Pts',(16.7166995414285,-19.5955068361058,-7.8699674126817));
#85096=CARTESIAN_POINT('Ctrl Pts',(16.6934926816934,-19.5172056306188,-7.8746296967584));
#85097=CARTESIAN_POINT('Ctrl Pts',(16.6836949864714,-19.4805607535186,-7.87683264517523));
#85098=CARTESIAN_POINT('Ctrl Pts',(16.6731275213978,-19.4363047058337,-7.87953975057152));
#85099=CARTESIAN_POINT('Ctrl Pts',(16.6714072156323,-19.4289249658938,-7.87999270481254));
#85100=CARTESIAN_POINT('Ctrl Pts',(16.6687987099737,-19.4174569087303,-7.8806992064329));
#85101=CARTESIAN_POINT('Ctrl Pts',(16.667882927276,-19.4133748403567,-7.88095119933021));
#85102=CARTESIAN_POINT('Ctrl Pts',(16.6662094742611,-19.4058105788483,-7.88141914790224));
#85103=CARTESIAN_POINT('Ctrl Pts',(16.6654484943428,-19.4023291770174,-7.88163491123376));
#85104=CARTESIAN_POINT('Ctrl Pts',(16.6637510201735,-19.3944683242684,-7.88212297776956));
#85105=CARTESIAN_POINT('Ctrl Pts',(16.6628196357975,-19.390087838844,-7.8823955674499));
#85106=CARTESIAN_POINT('Ctrl Pts',(16.660120228627,-19.3771909562168,-7.88319985232476));
#85107=CARTESIAN_POINT('Ctrl Pts',(16.6583908097984,-19.368666700081,-7.88373367139447));
#85108=CARTESIAN_POINT('Ctrl Pts',(16.6465062974476,-19.3081776448585,-7.88753627043884));
#85109=CARTESIAN_POINT('Ctrl Pts',(16.6382522153223,-19.255862929692,-7.89090069133754));
#85110=CARTESIAN_POINT('Ctrl Pts',(16.6301911620637,-19.1884349207003,-7.89528837021718));
#85111=CARTESIAN_POINT('Ctrl Pts',(16.6285718969084,-19.1735526702708,-7.89625999960626));
#85112=CARTESIAN_POINT('Ctrl Pts',(16.6204362928577,-19.0906084516964,-7.90168907697733));
#85113=CARTESIAN_POINT('Ctrl Pts',(16.6170625898356,-19.0222805698061,-7.90621169922116));
#85114=CARTESIAN_POINT('Ctrl Pts',(16.6168557120479,-18.7931414075279,-7.92135266217216));
#85115=CARTESIAN_POINT('Ctrl Pts',(16.6350247735661,-18.6328491686991,-7.93185066226681));
#85116=CARTESIAN_POINT('Ctrl Pts',(16.6765204031032,-18.4529688512325,-7.94322216467185));
#85117=CARTESIAN_POINT('Ctrl Pts',(16.6822553141319,-18.4298906288441,-7.94467444424136));
#85118=CARTESIAN_POINT('Ctrl Pts',(16.6908695970453,-18.3975626302714,-7.94670014317305));
#85119=CARTESIAN_POINT('Ctrl Pts',(16.6934253009823,-18.3882291750872,-7.94728396599734));
#85120=CARTESIAN_POINT('Ctrl Pts',(16.6976666647772,-18.3731464467184,-7.94822584779665));
#85121=CARTESIAN_POINT('Ctrl Pts',(16.6993128688492,-18.3673863089507,-7.94858518366482));
#85122=CARTESIAN_POINT('Ctrl Pts',(16.7027975180278,-18.3553863978649,-7.94933303086491));
#85123=CARTESIAN_POINT('Ctrl Pts',(16.7046403186936,-18.3491479465346,-7.94972139571439));
#85124=CARTESIAN_POINT('Ctrl Pts',(16.7090695324404,-18.3344041536795,-7.9506382951558));
#85125=CARTESIAN_POINT('Ctrl Pts',(16.7116808362905,-18.3259063715311,-7.95116600991541));
#85126=CARTESIAN_POINT('Ctrl Pts',(16.7205471826034,-18.2976875470883,-7.95291609207069));
#85127=CARTESIAN_POINT('Ctrl Pts',(16.7270379021795,-18.2780413836334,-7.95413072322058));
#85128=CARTESIAN_POINT('Ctrl Pts',(16.7631661561862,-18.1738417659314,-7.96055728524779));
#85129=CARTESIAN_POINT('Ctrl Pts',(16.7978624833675,-18.0911338970417,-7.96559779631823));
#85130=CARTESIAN_POINT('Ctrl Pts',(16.8976427994538,-17.8900855297674,-7.97797942744256));
#85131=CARTESIAN_POINT('Ctrl Pts',(16.9689850845162,-17.7753138247879,-7.98515787236621));
#85132=CARTESIAN_POINT('Ctrl Pts',(17.0971458320886,-17.607288592211,-7.99685013466944));
#85133=CARTESIAN_POINT('Ctrl Pts',(17.1467942734104,-17.5490332645751,-8.00116971420075));
#85134=CARTESIAN_POINT('Ctrl Pts',(17.2060220538967,-17.486714156302,-8.0062650856435));
#85135=CARTESIAN_POINT('Ctrl Pts',(17.2126111820274,-17.479873896548,-8.00683121545435));
#85136=CARTESIAN_POINT('Ctrl Pts',(17.22244624565,-17.4698005419395,-8.00767557491742));
#85137=CARTESIAN_POINT('Ctrl Pts',(17.2256571127177,-17.4665331645424,-8.00795113171247));
#85138=CARTESIAN_POINT('Ctrl Pts',(17.231390352827,-17.4607367748996,-8.00844303394105));
#85139=CARTESIAN_POINT('Ctrl Pts',(17.233908546069,-17.4582036993194,-8.008659050336));
#85140=CARTESIAN_POINT('Ctrl Pts',(17.2393381935503,-17.4527695385085,-8.00912474738892));
#85141=CARTESIAN_POINT('Ctrl Pts',(17.2422516463095,-17.4498705978107,-8.0093745836083));
#85142=CARTESIAN_POINT('Ctrl Pts',(17.2503213502874,-17.4418877200531,-8.01006639933602));
#85143=CARTESIAN_POINT('Ctrl Pts',(17.2554952156978,-17.436821781781,-8.010509750164));
#85144=CARTESIAN_POINT('Ctrl Pts',(17.284054844249,-17.4091434733207,-8.0129553924431));
#85145=CARTESIAN_POINT('Ctrl Pts',(17.3079320750152,-17.3870472144712,-8.01499401047398));
#85146=CARTESIAN_POINT('Ctrl Pts',(17.4542419685985,-17.2577796637008,-8.02739988205871));
#85147=CARTESIAN_POINT('Ctrl Pts',(17.588186180866,-17.1644671225473,-8.03835714537534));
#85148=CARTESIAN_POINT('Ctrl Pts',(17.8343783664717,-17.0321002963409,-8.05661523025183));
#85149=CARTESIAN_POINT('Ctrl Pts',(17.9416765750237,-16.9853873406102,-8.06405607123662));
#85150=CARTESIAN_POINT('Ctrl Pts',(18.0658261026039,-16.9431603278798,-8.07206312933223));
#85151=CARTESIAN_POINT('Ctrl Pts',(18.0794008224476,-16.9386959698272,-8.072931105485));
#85152=CARTESIAN_POINT('Ctrl Pts',(18.1010776394829,-16.9318094732524,-8.07430541422955));
#85153=CARTESIAN_POINT('Ctrl Pts',(18.1091506608241,-16.9292978999926,-8.07481467489004));
#85154=CARTESIAN_POINT('Ctrl Pts',(18.1234152326693,-16.9249536435684,-8.07571005311163));
#85155=CARTESIAN_POINT('Ctrl Pts',(18.1296004870851,-16.9231008109223,-8.0760968267999));
#85156=CARTESIAN_POINT('Ctrl Pts',(18.1424111095,-16.9193270878367,-8.07689489559987));
#85157=CARTESIAN_POINT('Ctrl Pts',(18.1490375905764,-16.9174102220598,-8.07730605533092));
#85158=CARTESIAN_POINT('Ctrl Pts',(18.1660708983198,-16.9125730308735,-8.07835876507018));
#85159=CARTESIAN_POINT('Ctrl Pts',(18.1764910164661,-16.9096999322398,-8.07899877377739));
#85160=CARTESIAN_POINT('Ctrl Pts',(18.2200727293667,-16.8980417234947,-8.0816594379043));
#85161=CARTESIAN_POINT('Ctrl Pts',(18.2534244813408,-16.8899832181597,-8.08365656461557));
#85162=CARTESIAN_POINT('Ctrl Pts',(18.3408211609655,-16.8711021270563,-8.08880063775893));
#85163=CARTESIAN_POINT('Ctrl Pts',(18.3951197442136,-16.8615726813116,-8.09190819529001));
#85164=CARTESIAN_POINT('Ctrl Pts',(18.558087537074,-16.8394895423993,-8.10105260331991));
#85165=CARTESIAN_POINT('Ctrl Pts',(18.6674213462009,-16.8332235147235,-8.10694072442736));
#85166=CARTESIAN_POINT('Ctrl Pts',(18.8224701916281,-16.8363551187521,-8.11538395477344));
#85167=CARTESIAN_POINT('Ctrl Pts',(18.8681477481271,-16.8387597432486,-8.11788438165609));
#85168=CARTESIAN_POINT('Ctrl Pts',(18.9364180536166,-16.8445761406398,-8.1216837269709));
#85169=CARTESIAN_POINT('Ctrl Pts',(18.9590926750583,-16.8468772892681,-8.12295598013379));
#85170=CARTESIAN_POINT('Ctrl Pts',(18.9827504056994,-16.8496647980315,-8.12429816534834));
#85171=CARTESIAN_POINT('Ctrl Pts',(18.9837755855149,-16.8497863518076,-8.12435635643155));
#85172=CARTESIAN_POINT('Ctrl Pts',(19.0030165219534,-16.8520819893648,-8.12544905957002));
#85173=CARTESIAN_POINT('Ctrl Pts',(19.0212028764875,-16.8544919516727,-8.12649116268315));
#85174=CARTESIAN_POINT('Ctrl Pts',(19.0724996166818,-16.8619691609641,-8.1294624883361));
#85175=CARTESIAN_POINT('Ctrl Pts',(19.1055227202059,-16.8675860572733,-8.13141308620021));
#85176=CARTESIAN_POINT('Ctrl Pts',(19.1451980358659,-16.8753071513822,-8.13381732359371));
#85177=CARTESIAN_POINT('Ctrl Pts',(19.1519928783091,-16.8766641325105,-8.13423123978184));
#85178=CARTESIAN_POINT('Ctrl Pts',(19.1631375823776,-16.8789467655288,-8.13491387024137));
#85179=CARTESIAN_POINT('Ctrl Pts',(19.1674914661766,-16.879852822437,-8.13518149102585));
#85180=CARTESIAN_POINT('Ctrl Pts',(19.1753272380623,-16.8815092476423,-8.13566487761919));
#85181=CARTESIAN_POINT('Ctrl Pts',(19.1788101114186,-16.8822546893133,-8.13588035953831));
#85182=CARTESIAN_POINT('Ctrl Pts',(19.18640402507,-16.8839000729682,-8.13635156049491));
#85183=CARTESIAN_POINT('Ctrl Pts',(19.1905142172713,-16.8848034735888,-8.13660747109534));
#85184=CARTESIAN_POINT('Ctrl Pts',(19.2021294427328,-16.8873927751305,-8.1373330825887));
#85185=CARTESIAN_POINT('Ctrl Pts',(19.2096279294223,-16.8891073133282,-8.13780437853594));
#85186=CARTESIAN_POINT('Ctrl Pts',(19.2560674190503,-16.8999924182554,-8.14074024373807));
#85187=CARTESIAN_POINT('Ctrl Pts',(19.2947486243764,-16.9102238107458,-8.143259982085));
#85188=CARTESIAN_POINT('Ctrl Pts',(19.4986171921126,-16.9703780099379,-8.15685569395482));
#85189=CARTESIAN_POINT('Ctrl Pts',(19.6575292055489,-17.0392628362193,-8.16850287167479));
#85190=CARTESIAN_POINT('Ctrl Pts',(19.8919426330622,-17.1769736794803,-8.18613287195658));
#85191=CARTESIAN_POINT('Ctrl Pts',(19.9739258016713,-17.2332392576233,-8.19241430282786));
#85192=CARTESIAN_POINT('Ctrl Pts',(20.0625882076603,-17.3037472530884,-8.19932817043001));
#85193=CARTESIAN_POINT('Ctrl Pts',(20.0734246214486,-17.3125411132536,-8.20017557044739));
#85194=CARTESIAN_POINT('Ctrl Pts',(20.0906103918501,-17.3267716814005,-8.20152353238014));
#85195=CARTESIAN_POINT('Ctrl Pts',(20.0970157400845,-17.3321398399048,-8.20202685024767));
#85196=CARTESIAN_POINT('Ctrl Pts',(20.1083013186278,-17.3417123318911,-8.20291533865471));
#85197=CARTESIAN_POINT('Ctrl Pts',(20.1131944332442,-17.3459012467546,-8.20330113353076));
#85198=CARTESIAN_POINT('Ctrl Pts',(20.1233191092686,-17.3546492042702,-8.20410063703401));
#85199=CARTESIAN_POINT('Ctrl Pts',(20.1285475322625,-17.3592117736433,-8.20451419318579));
#85200=CARTESIAN_POINT('Ctrl Pts',(20.1420024229867,-17.3710701857922,-8.20558029965285));
#85201=CARTESIAN_POINT('Ctrl Pts',(20.1501947191423,-17.3784046184098,-8.20623123097674));
#85202=CARTESIAN_POINT('Ctrl Pts',(20.1849394390229,-17.4100021266518,-8.20900020226171));
#85203=CARTESIAN_POINT('Ctrl Pts',(20.210929272352,-17.4348767857808,-8.21109219840875));
#85204=CARTESIAN_POINT('Ctrl Pts',(20.2777286433051,-17.5021542954613,-8.21653887715065));
#85205=CARTESIAN_POINT('Ctrl Pts',(20.3174268136529,-17.545617769574,-8.21984780785296));
#85206=CARTESIAN_POINT('Ctrl Pts',(20.4633879457798,-17.7194504503348,-8.23243226252002));
#85207=CARTESIAN_POINT('Ctrl Pts',(20.5557751105201,-17.8606297312796,-8.24128142180231));
#85208=CARTESIAN_POINT('Ctrl Pts',(20.6549175509313,-18.060491420903,-8.25381141611157));
#85209=CARTESIAN_POINT('Ctrl Pts',(20.677419578213,-18.1106730592126,-8.25696256627584));
#85210=CARTESIAN_POINT('Ctrl Pts',(20.7012202991938,-18.1698168744309,-8.26074538910701));
#85211=CARTESIAN_POINT('Ctrl Pts',(20.7044485520071,-18.1779853713692,-8.2612693404077));
#85212=CARTESIAN_POINT('Ctrl Pts',(20.7092525387811,-18.1903658166282,-8.26206605584896));
#85213=CARTESIAN_POINT('Ctrl Pts',(20.7108658822522,-18.1945632013353,-8.26233661824698));
#85214=CARTESIAN_POINT('Ctrl Pts',(20.7137342236981,-18.2020972649618,-8.26282312073175));
#85215=CARTESIAN_POINT('Ctrl Pts',(20.7149941770911,-18.2054320000536,-8.26303876014449));
#85216=CARTESIAN_POINT('Ctrl Pts',(20.7177095525902,-18.2126740933998,-8.26350773695192));
#85217=CARTESIAN_POINT('Ctrl Pts',(20.7191618364278,-18.2165825214845,-8.26376125184051));
#85218=CARTESIAN_POINT('Ctrl Pts',(20.7231986580862,-18.2275456210155,-8.26447347243599));
#85219=CARTESIAN_POINT('Ctrl Pts',(20.7257571703443,-18.2346097163639,-8.26493368272565));
#85220=CARTESIAN_POINT('Ctrl Pts',(20.7406307217082,-18.2763687755437,-8.26766115503635));
#85221=CARTESIAN_POINT('Ctrl Pts',(20.7520758182437,-18.3113643654059,-8.26997508052884));
#85222=CARTESIAN_POINT('Ctrl Pts',(20.7863631188612,-18.4262630177201,-8.27762383391845));
#85223=CARTESIAN_POINT('Ctrl Pts',(20.805414114031,-18.507212964824,-8.28309007395295));
#85224=CARTESIAN_POINT('Ctrl Pts',(20.850709648133,-18.7675115344248,-8.30054051516429));
#85225=CARTESIAN_POINT('Ctrl Pts',(20.8587385380537,-18.94924318391,-8.31245634036885));
#85226=CARTESIAN_POINT('Ctrl Pts',(20.8416283250973,-19.1522481744002,-8.32499026326175));
#85227=CARTESIAN_POINT('Ctrl Pts',(20.8393780671179,-19.1746650941409,-8.32636507902359));
#85228=CARTESIAN_POINT('Ctrl Pts',(20.8356742486542,-19.2064484738305,-8.32830184130312));
#85229=CARTESIAN_POINT('Ctrl Pts',(20.8345150314787,-19.2158470776419,-8.32887300444326));
#85230=CARTESIAN_POINT('Ctrl Pts',(20.8325244310284,-19.2311409152854,-8.32979997686675));
#85231=CARTESIAN_POINT('Ctrl Pts',(20.8317311848015,-19.2370409017061,-8.33015698515062));
#85232=CARTESIAN_POINT('Ctrl Pts',(20.8300146874149,-19.2494124442066,-8.33090436845387));
#85233=CARTESIAN_POINT('Ctrl Pts',(20.8290863255787,-19.2558832369165,-8.3312945777079));
#85234=CARTESIAN_POINT('Ctrl Pts',(20.8267986896732,-19.2713193809645,-8.3322238012155));
#85235=CARTESIAN_POINT('Ctrl Pts',(20.825411749673,-19.2802805504172,-8.3327619340338));
#85236=CARTESIAN_POINT('Ctrl Pts',(20.8205047426559,-19.3106912604255,-8.33458389999213));
#85237=CARTESIAN_POINT('Ctrl Pts',(20.8167118538631,-19.3320958391715,-8.33585908360513));
#85238=CARTESIAN_POINT('Ctrl Pts',(20.7939488841615,-19.4499590775858,-8.34284659366596));
#85239=CARTESIAN_POINT('Ctrl Pts',(20.7686067000857,-19.5450695713826,-8.34835040425284));
#85240=CARTESIAN_POINT('Ctrl Pts',(20.6933418744,-19.764774663746,-8.36110828161006));
#85241=CARTESIAN_POINT('Ctrl Pts',(20.6380203207323,-19.8870544231139,-8.36823789870716));
#85242=CARTESIAN_POINT('Ctrl Pts',(20.5637979768948,-20.0167865345906,-8.37655430229737));
#85243=CARTESIAN_POINT('Ctrl Pts',(20.555924355507,-20.0302034253452,-8.37742421158511));
#85244=CARTESIAN_POINT('Ctrl Pts',(20.5207030926731,-20.0887339815106,-8.38126781467058));
#85245=CARTESIAN_POINT('Ctrl Pts',(20.4918246986183,-20.1328994140527,-8.3842962425026));
#85246=CARTESIAN_POINT('Ctrl Pts',(20.4563044996808,-20.1830287443011,-8.38794236120464));
#85247=CARTESIAN_POINT('Ctrl Pts',(20.4512354442606,-20.1900900540865,-8.38846095849569));
#85248=CARTESIAN_POINT('Ctrl Pts',(20.4434898382314,-20.2007407812396,-8.38925110646511));
#85249=CARTESIAN_POINT('Ctrl Pts',(20.4408450791874,-20.2043533529137,-8.38952050920648));
#85250=CARTESIAN_POINT('Ctrl Pts',(20.43607472904,-20.2108261658927,-8.39000577717004));
#85251=CARTESIAN_POINT('Ctrl Pts',(20.4339533600845,-20.2136894516517,-8.39022134832604));
#85252=CARTESIAN_POINT('Ctrl Pts',(20.4293252254273,-20.2199033441032,-8.39069117404181));
#85253=CARTESIAN_POINT('Ctrl Pts',(20.4268157846041,-20.2232518352607,-8.3909456115316));
#85254=CARTESIAN_POINT('Ctrl Pts',(20.4197315604927,-20.23264655225,-8.39166297885597));
#85255=CARTESIAN_POINT('Ctrl Pts',(20.4151342531794,-20.2386756019387,-8.39212744776092));
#85256=CARTESIAN_POINT('Ctrl Pts',(20.3872994415457,-20.2747751808865,-8.39493258803806));
#85257=CARTESIAN_POINT('Ctrl Pts',(20.3632895852967,-20.3042382388064,-8.397323007135));
#85258=CARTESIAN_POINT('Ctrl Pts',(20.2812806025722,-20.3995170425488,-8.40535036437698));
#85259=CARTESIAN_POINT('Ctrl Pts',(20.2199865612467,-20.4623724231942,-8.41113225867746));
#85260=CARTESIAN_POINT('Ctrl Pts',(20.0256724758027,-20.6383272958077,-8.42845298969269));
#85261=CARTESIAN_POINT('Ctrl Pts',(19.8823664736713,-20.739007284665,-8.43990126181429));
#85262=CARTESIAN_POINT('Ctrl Pts',(19.7079463363748,-20.8318003800597,-8.45206277430418));
#85263=CARTESIAN_POINT('Ctrl Pts',(19.687408551335,-20.8422997474715,-8.45347080028325));
#85264=CARTESIAN_POINT('Ctrl Pts',(19.6581222052432,-20.8566728082937,-8.45544567752015));
#85265=CARTESIAN_POINT('Ctrl Pts',(19.6495132501926,-20.8608257778764,-8.45602224648443));
#85266=CARTESIAN_POINT('Ctrl Pts',(19.6354827951028,-20.8674773292086,-8.45695557845937));
#85267=CARTESIAN_POINT('Ctrl Pts',(19.6300784055993,-20.8700115017202,-8.45731357354201));
#85268=CARTESIAN_POINT('Ctrl Pts',(19.6187460598519,-20.8752670002481,-8.45806111135696));
#85269=CARTESIAN_POINT('Ctrl Pts',(19.6128160914703,-20.8779838585793,-8.45845049670276));
#85270=CARTESIAN_POINT('Ctrl Pts',(19.5986839755579,-20.8843797324103,-8.45937428110823));
#85271=CARTESIAN_POINT('Ctrl Pts',(19.5904707227049,-20.888034016427,-8.45990782597413));
#85272=CARTESIAN_POINT('Ctrl Pts',(19.562745838934,-20.9001585591861,-8.4616978768979));
#85273=CARTESIAN_POINT('Ctrl Pts',(19.543129496357,-20.9083872172852,-8.46294614564272));
#85274=CARTESIAN_POINT('Ctrl Pts',(19.3794566472617,-20.9741616773173,-8.47321885831932));
#85275=CARTESIAN_POINT('Ctrl Pts',(19.2295971413606,-21.0160114061446,-8.4816693188242));
#85276=CARTESIAN_POINT('Ctrl Pts',(18.9422190217862,-21.0631248601586,-8.49748366779995));
#85277=CARTESIAN_POINT('Ctrl Pts',(18.8061526482159,-21.0721384587118,-8.50483421515098));
#85278=CARTESIAN_POINT('Ctrl Pts',(18.6545760401514,-21.0675672259243,-8.51372642082399));
#85279=CARTESIAN_POINT('Ctrl Pts',(18.6389735479622,-21.0669238270284,-8.51465023432401));
#85280=CARTESIAN_POINT('Ctrl Pts',(18.6176090194386,-21.0658059363226,-8.51592859162525));
#85281=CARTESIAN_POINT('Ctrl Pts',(18.6118392565018,-21.0654803400444,-8.5162751664776));
#85282=CARTESIAN_POINT('Ctrl Pts',(18.602668315446,-21.0649251309896,-8.51682827134775));
#85283=CARTESIAN_POINT('Ctrl Pts',(18.5992661850041,-21.0647109171044,-8.51703394403361));
#85284=CARTESIAN_POINT('Ctrl Pts',(18.5922369100759,-21.0642512736052,-8.51745992859139));
#85285=CARTESIAN_POINT('Ctrl Pts',(18.5886098860117,-21.0640047183867,-8.51768030527992));
#85286=CARTESIAN_POINT('Ctrl Pts',(18.5799624978535,-21.0633945118143,-8.51820706103952));
#85287=CARTESIAN_POINT('Ctrl Pts',(18.5749427762321,-21.0630222961763,-8.51851391660689));
#85288=CARTESIAN_POINT('Ctrl Pts',(18.5579880449292,-21.0617042758174,-8.51955389670345));
#85289=CARTESIAN_POINT('Ctrl Pts',(18.5460599999924,-21.0606751482702,-8.52029147151354));
#85290=CARTESIAN_POINT('Ctrl Pts',(18.4091264926598,-21.0476897523819,-8.52882196998391));
#85291=CARTESIAN_POINT('Ctrl Pts',(18.2854270831029,-21.0247358854845,-8.53711883960778));
#85292=CARTESIAN_POINT('Ctrl Pts',(18.0034837829291,-20.9459874005889,-8.55646409421056));
#85293=CARTESIAN_POINT('Ctrl Pts',(17.848325523587,-20.8820882964693,-8.56740717984012));
#85294=CARTESIAN_POINT('Ctrl Pts',(17.681779601747,-20.7891370909323,-8.5791527797003));
#85295=CARTESIAN_POINT('Ctrl Pts',(17.6614651719961,-20.7773519030031,-8.58058682556847));
#85296=CARTESIAN_POINT('Ctrl Pts',(17.6332581851248,-20.76035442301,-8.5825807005051));
#85297=CARTESIAN_POINT('Ctrl Pts',(17.6251986285184,-20.7554239061748,-8.58315072412566));
#85298=CARTESIAN_POINT('Ctrl Pts',(17.6116111713855,-20.7469861194556,-8.58411233619252));
#85299=CARTESIAN_POINT('Ctrl Pts',(17.6060660970866,-20.7435068975004,-8.58450494908714));
#85300=CARTESIAN_POINT('Ctrl Pts',(17.5951046719161,-20.7365581537137,-8.58528144952721));
#85301=CARTESIAN_POINT('Ctrl Pts',(17.5896878206877,-20.7330895569855,-8.58566536572776));
#85302=CARTESIAN_POINT('Ctrl Pts',(17.5788372269676,-20.7260716133255,-8.58643481778078));
#85303=CARTESIAN_POINT('Ctrl Pts',(17.5734038300919,-20.7225218590102,-8.58682033293355));
#85304=CARTESIAN_POINT('Ctrl Pts',(17.5541553609242,-20.7098197421021,-8.58818691204402));
#85305=CARTESIAN_POINT('Ctrl Pts',(17.5404312927251,-20.7005300633227,-8.58916282533725));
#85306=CARTESIAN_POINT('Ctrl Pts',(17.422939699676,-20.6189732603783,-8.59753479661582));
#85307=CARTESIAN_POINT('Ctrl Pts',(17.3257253134569,-20.5377009495113,-8.6045571525512));
#85308=CARTESIAN_POINT('Ctrl Pts',(17.1406295607827,-20.3524273884892,-8.61884914417775));
#85309=CARTESIAN_POINT('Ctrl Pts',(17.0543431584248,-20.2476749032565,-8.62607107852499));
#85310=CARTESIAN_POINT('Ctrl Pts',(16.95247570486,-20.0965758266773,-8.63637781747498));
#85311=CARTESIAN_POINT('Ctrl Pts',(16.9275921294496,-20.056885753053,-8.63907800668033));
#85312=CARTESIAN_POINT('Ctrl Pts',(16.9001864898759,-20.009769336389,-8.64231459582629));
#85313=CARTESIAN_POINT('Ctrl Pts',(16.8963620362606,-20.0031111592495,-8.64277267689436));
#85314=CARTESIAN_POINT('Ctrl Pts',(16.8902925899454,-19.9924101927577,-8.64351027281511));
#85315=CARTESIAN_POINT('Ctrl Pts',(16.8880244351529,-19.9883805267096,-8.64378833912235));
#85316=CARTESIAN_POINT('Ctrl Pts',(16.8840211912224,-19.9812134186804,-8.64428351098323));
#85317=CARTESIAN_POINT('Ctrl Pts',(16.8822808489924,-19.9780789636951,-8.64450027573602));
#85318=CARTESIAN_POINT('Ctrl Pts',(16.8785983976439,-19.9714067788319,-8.64496215324987));
#85319=CARTESIAN_POINT('Ctrl Pts',(16.8766584699706,-19.9678679672834,-8.64520739347619));
#85320=CARTESIAN_POINT('Ctrl Pts',(16.8714269530806,-19.958259568714,-8.6458739381007));
#85321=CARTESIAN_POINT('Ctrl Pts',(16.8681549539663,-19.9521794518461,-8.64629645632944));
#85322=CARTESIAN_POINT('Ctrl Pts',(16.8517661886613,-19.9213651085607,-8.64844108093734));
#85323=CARTESIAN_POINT('Ctrl Pts',(16.8391119302808,-19.896389676674,-8.65018994855127));
#85324=CARTESIAN_POINT('Ctrl Pts',(16.8035648371587,-19.8226387218721,-8.6553692384259));
#85325=CARTESIAN_POINT('Ctrl Pts',(16.7820350890976,-19.7732331571053,-8.65885725237295));
#85326=CARTESIAN_POINT('Ctrl Pts',(16.7565777928111,-19.7081396808811,-8.663431461056));
#85327=CARTESIAN_POINT('Ctrl Pts',(16.7509125212525,-19.6931541927726,-8.66448311665522));
#85328=CARTESIAN_POINT('Ctrl Pts',(16.7454194712032,-19.678110515342,-8.66553666923996));
#85329=CARTESIAN_POINT('',(16.6172480955499,-18.9524633046122,-7.68905625083761));
#85330=CARTESIAN_POINT('Ctrl Pts',(16.7454194499637,-19.6781104571739,-8.4444886490522));
#85331=CARTESIAN_POINT('Ctrl Pts',(16.7701773775376,-19.7459143742589,-8.44016252692827));
#85332=CARTESIAN_POINT('Ctrl Pts',(16.798398965251,-19.8124279737233,-8.43583640480434));
#85333=CARTESIAN_POINT('Ctrl Pts',(16.8299125176285,-19.877278260566,-8.43151028268041));
#85334=CARTESIAN_POINT('Ctrl Pts',(16.8614397440995,-19.9421566866955,-8.42718228340223));
#85335=CARTESIAN_POINT('Ctrl Pts',(16.8962615401651,-20.0053699294018,-8.42285428412405));
#85336=CARTESIAN_POINT('Ctrl Pts',(16.9341606764734,-20.0665705044936,-8.41852628484587));
#85337=CARTESIAN_POINT('Ctrl Pts',(16.9721294353055,-20.1278835079655,-8.41419033482626));
#85338=CARTESIAN_POINT('Ctrl Pts',(17.0131865446795,-20.1871760506629,-8.40985438480666));
#85339=CARTESIAN_POINT('Ctrl Pts',(17.057072299101,-20.2441309863778,-8.40551843478705));
#85340=CARTESIAN_POINT('Ctrl Pts',(17.0972716608073,-20.2963017213222,-8.40154670351625));
#85341=CARTESIAN_POINT('Ctrl Pts',(17.1398437332676,-20.3465112515435,-8.39757497224546));
#85342=CARTESIAN_POINT('Ctrl Pts',(17.1845622179524,-20.3945434342034,-8.39360324097466));
#85343=CARTESIAN_POINT('Ctrl Pts',(17.2339699045481,-20.447612294745,-8.38921503204376));
#85344=CARTESIAN_POINT('Ctrl Pts',(17.2862036327227,-20.4982434590661,-8.38482682311286));
#85345=CARTESIAN_POINT('Ctrl Pts',(17.3409933109755,-20.5461208750697,-8.38043861418196));
#85346=CARTESIAN_POINT('Ctrl Pts',(17.3957016722616,-20.5939272330498,-8.37605691808069));
#85347=CARTESIAN_POINT('Ctrl Pts',(17.4529580928701,-20.6389876412174,-8.37167522197941));
#85348=CARTESIAN_POINT('Ctrl Pts',(17.5124544762694,-20.6810215537852,-8.36729352587814));
#85349=CARTESIAN_POINT('Ctrl Pts',(17.5718809466833,-20.7230060731605,-8.3629169786185));
#85350=CARTESIAN_POINT('Ctrl Pts',(17.6335417591178,-20.7619708847355,-8.35854043135886));
#85351=CARTESIAN_POINT('Ctrl Pts',(17.6970957742217,-20.7976756558407,-8.35416388409922));
#85352=CARTESIAN_POINT('Ctrl Pts',(17.7606094842929,-20.8333577834991,-8.34979011238225));
#85353=CARTESIAN_POINT('Ctrl Pts',(17.8260135952853,-20.8657837371302,-8.34541634066528));
#85354=CARTESIAN_POINT('Ctrl Pts',(17.8929392167478,-20.8947572568067,-8.34104256894831));
#85355=CARTESIAN_POINT('Ctrl Pts',(17.9598444725189,-20.923721959744,-8.33667012818475));
#85356=CARTESIAN_POINT('Ctrl Pts',(18.028269877152,-20.949236122938,-8.33229768742119));
#85357=CARTESIAN_POINT('Ctrl Pts',(18.097824766941,-20.9711508296416,-8.32792524665764));
#85358=CARTESIAN_POINT('Ctrl Pts',(18.1673814352561,-20.9930660967066,-8.32355269409029));
#85359=CARTESIAN_POINT('Ctrl Pts',(18.238067185385,-21.0113815814964,-8.31918014152294));
#85360=CARTESIAN_POINT('Ctrl Pts',(18.3094759435902,-21.0259981498375,-8.31480758895559));
#85361=CARTESIAN_POINT('Ctrl Pts',(18.3809588124981,-21.0406298878046,-8.31043049838827));
#85362=CARTESIAN_POINT('Ctrl Pts',(18.4531657140464,-21.0515549478117,-8.30605340782094));
#85363=CARTESIAN_POINT('Ctrl Pts',(18.5256809453891,-21.0587254618213,-8.30167631725361));
#85364=CARTESIAN_POINT('Ctrl Pts',(18.5982357799911,-21.0658998919146,-8.29729683619467));
#85365=CARTESIAN_POINT('Ctrl Pts',(18.6710987974685,-21.0693156708867,-8.29291735513573));
#85366=CARTESIAN_POINT('Ctrl Pts',(18.7438524696364,-21.0689770732916,-8.28853787407679));
#85367=CARTESIAN_POINT('Ctrl Pts',(18.8167350971998,-21.0686378755345,-8.28415063041707));
#85368=CARTESIAN_POINT('Ctrl Pts',(18.8895075103798,-21.064531039433,-8.27976338675735));
#85369=CARTESIAN_POINT('Ctrl Pts',(18.9617560690986,-21.0567128481075,-8.27537614309762));
#85370=CARTESIAN_POINT('Ctrl Pts',(19.0108781271724,-21.0513972313653,-8.27239324016283));
#85371=CARTESIAN_POINT('Ctrl Pts',(19.0597581560645,-21.0443670563134,-8.26941033722803));
#85372=CARTESIAN_POINT('Ctrl Pts',(19.1082694567067,-21.0356533717911,-8.26642743429324));
#85373=CARTESIAN_POINT('Ctrl Pts',(19.1796354137561,-21.0228344939807,-8.26203922536235));
#85374=CARTESIAN_POINT('Ctrl Pts',(19.2504813367645,-21.0063198837036,-8.25765101643146));
#85375=CARTESIAN_POINT('Ctrl Pts',(19.3203952805279,-20.9861655721633,-8.25326280750057));
#85376=CARTESIAN_POINT('Ctrl Pts',(19.3902054604071,-20.9660411729629,-8.24888111139929));
#85377=CARTESIAN_POINT('Ctrl Pts',(19.4590859472334,-20.9422879285591,-8.24449941529801));
#85378=CARTESIAN_POINT('Ctrl Pts',(19.526634079588,-20.9150130452637,-8.24011771919673));
#85379=CARTESIAN_POINT('Ctrl Pts',(19.5941028375112,-20.887770212127,-8.23574117193709));
#85380=CARTESIAN_POINT('Ctrl Pts',(19.6602419060116,-20.8570141403841,-8.23136462467746));
#85381=CARTESIAN_POINT('Ctrl Pts',(19.724664551087,-20.8229015867275,-8.22698807741782));
#85382=CARTESIAN_POINT('Ctrl Pts',(19.7890463402572,-20.7888106667567,-8.22261430570085));
#85383=CARTESIAN_POINT('Ctrl Pts',(19.8517134405357,-20.7513677135307,-8.21824053398388));
#85384=CARTESIAN_POINT('Ctrl Pts',(19.9123011549775,-20.7107766737647,-8.21386676226691));
#85385=CARTESIAN_POINT('Ctrl Pts',(19.9728704323744,-20.6701979859884,-8.20949432150336));
#85386=CARTESIAN_POINT('Ctrl Pts',(20.0313611796541,-20.6264733818696,-8.20512188073982));
#85387=CARTESIAN_POINT('Ctrl Pts',(20.0874367225441,-20.5798507419506,-8.20074943997627));
#85388=CARTESIAN_POINT('Ctrl Pts',(20.1435136992921,-20.5332269098853,-8.19637688740892));
#85389=CARTESIAN_POINT('Ctrl Pts',(20.1971749793955,-20.4837052048255,-8.19200433484156));
#85390=CARTESIAN_POINT('Ctrl Pts',(20.2481174066906,-20.4315734110738,-8.18763178227421));
#85391=CARTESIAN_POINT('Ctrl Pts',(20.2991127039582,-20.3793875129803,-8.18325469170688));
#85392=CARTESIAN_POINT('Ctrl Pts',(20.3473831767919,-20.3245864635399,-8.17887760113956));
#85393=CARTESIAN_POINT('Ctrl Pts',(20.3926635636811,-20.2674938929986,-8.17450051057223));
#85394=CARTESIAN_POINT('Ctrl Pts',(20.4379686798702,-20.2103701420857,-8.17012102951329));
#85395=CARTESIAN_POINT('Ctrl Pts',(20.4802801788311,-20.1509527715819,-8.16574154845435));
#85396=CARTESIAN_POINT('Ctrl Pts',(20.5193756546998,-20.0895951703508,-8.16136206739541));
#85397=CARTESIAN_POINT('Ctrl Pts',(20.558540427037,-20.0281288131833,-8.15697482373569));
#85398=CARTESIAN_POINT('Ctrl Pts',(20.594477554813,-19.9647157776937,-8.15258758007597));
#85399=CARTESIAN_POINT('Ctrl Pts',(20.627010467696,-19.8997343347128,-8.14820033641625));
#85400=CARTESIAN_POINT('Ctrl Pts',(20.6491297135924,-19.8555532150827,-8.14521743348143));
#85401=CARTESIAN_POINT('Ctrl Pts',(20.6696762814795,-19.8106475457985,-8.14223453054661));
#85402=CARTESIAN_POINT('Ctrl Pts',(20.6886076987149,-19.7651406668741,-8.1392516276118));
#85403=CARTESIAN_POINT('Ctrl Pts',(20.7164580900962,-19.6981945754734,-8.1348634186809));
#85404=CARTESIAN_POINT('Ctrl Pts',(20.7409194707722,-19.6296853205151,-8.13047520975));
#85405=CARTESIAN_POINT('Ctrl Pts',(20.7618159759921,-19.5599896113515,-8.1260870008191));
#85406=CARTESIAN_POINT('Ctrl Pts',(20.7826814673335,-19.4903973421759,-8.12170530471784));
#85407=CARTESIAN_POINT('Ctrl Pts',(20.7999924489196,-19.4196225726486,-8.11732360861657));
#85408=CARTESIAN_POINT('Ctrl Pts',(20.813621111304,-19.3480619060435,-8.1129419125153));
#85409=CARTESIAN_POINT('Ctrl Pts',(20.8272337589254,-19.2765853289167,-8.10856536525566));
#85410=CARTESIAN_POINT('Ctrl Pts',(20.8371725931962,-19.204325160743,-8.10418881799602));
#85411=CARTESIAN_POINT('Ctrl Pts',(20.8433600899069,-19.1316914330405,-8.09981227073638));
#85412=CARTESIAN_POINT('Ctrl Pts',(20.849543662597,-19.0591037685925,-8.09543849901941));
#85413=CARTESIAN_POINT('Ctrl Pts',(20.8519805772149,-18.9861434941225,-8.09106472730244));
#85414=CARTESIAN_POINT('Ctrl Pts',(20.8506449171335,-18.9132276545351,-8.08669095558547));
#85415=CARTESIAN_POINT('Ctrl Pts',(20.849309663498,-18.8403340034827,-8.08231851482192));
#85416=CARTESIAN_POINT('Ctrl Pts',(20.8442041231405,-18.7674852424751,-8.07794607405836));
#85417=CARTESIAN_POINT('Ctrl Pts',(20.8353544889708,-18.6950986343318,-8.07357363329482));
#85418=CARTESIAN_POINT('Ctrl Pts',(20.826504628515,-18.6227101752547,-8.06920108072747));
#85419=CARTESIAN_POINT('Ctrl Pts',(20.8139105446927,-18.550784371074,-8.06482852816012));
#85420=CARTESIAN_POINT('Ctrl Pts',(20.7976501258781,-18.4797319003326,-8.06045597559277));
#85421=CARTESIAN_POINT('Ctrl Pts',(20.7813728313875,-18.4086056886572,-8.05607888502545));
#85422=CARTESIAN_POINT('Ctrl Pts',(20.7614217126851,-18.338355091294,-8.05170179445812));
#85423=CARTESIAN_POINT('Ctrl Pts',(20.7379253105678,-18.2693783261091,-8.0473247038908));
#85424=CARTESIAN_POINT('Ctrl Pts',(20.7144160761932,-18.2003638901525,-8.04294522283186));
#85425=CARTESIAN_POINT('Ctrl Pts',(20.6873578824888,-18.1326251197522,-8.03856574177292));
#85426=CARTESIAN_POINT('Ctrl Pts',(20.6569274894877,-18.0665403057323,-8.03418626071398));
#85427=CARTESIAN_POINT('Ctrl Pts',(20.6264431588193,-18.0003383568232,-8.02979901705427));
#85428=CARTESIAN_POINT('Ctrl Pts',(20.5925749169665,-17.9357966461503,-8.02541177339455));
#85429=CARTESIAN_POINT('Ctrl Pts',(20.555545255664,-17.8732683922458,-8.02102452973483));
#85430=CARTESIAN_POINT('Ctrl Pts',(20.5303686541479,-17.8307552047989,-8.01804162680001));
#85431=CARTESIAN_POINT('Ctrl Pts',(20.5037315602569,-17.7891722056905,-8.01505872386519));
#85432=CARTESIAN_POINT('Ctrl Pts',(20.475714693788,-17.7486218693016,-8.01207582093037));
#85433=CARTESIAN_POINT('Ctrl Pts',(20.4344985139989,-17.6889674480277,-8.00768761199947));
#85434=CARTESIAN_POINT('Ctrl Pts',(20.3901335538166,-17.6313165376484,-8.00329940306857));
#85435=CARTESIAN_POINT('Ctrl Pts',(20.342841373937,-17.5760209182155,-7.99891119413767));
#85436=CARTESIAN_POINT('Ctrl Pts',(20.2956193834937,-17.5208073666502,-7.99452949803641));
#85437=CARTESIAN_POINT('Ctrl Pts',(20.2454791086752,-17.4679425302631,-7.99014780193516));
#85438=CARTESIAN_POINT('Ctrl Pts',(20.1926848492421,-17.4177485504026,-7.9857661058339));
#85439=CARTESIAN_POINT('Ctrl Pts',(20.1399526272652,-17.367613552463,-7.98138955857425));
#85440=CARTESIAN_POINT('Ctrl Pts',(20.0845729637365,-17.3201435071859,-7.97701301131462));
#85441=CARTESIAN_POINT('Ctrl Pts',(20.0268486678897,-17.2756255424471,-7.97263646405497));
#85442=CARTESIAN_POINT('Ctrl Pts',(19.9691609799523,-17.2311358103545,-7.968262692338));
#85443=CARTESIAN_POINT('Ctrl Pts',(19.9091319909997,-17.1895947380413,-7.96388892062103));
#85444=CARTESIAN_POINT('Ctrl Pts',(19.8470983416193,-17.1512498557866,-7.95951514890405));
#85445=CARTESIAN_POINT('Ctrl Pts',(19.7850835692867,-17.1129166420084,-7.9551427081405));
#85446=CARTESIAN_POINT('Ctrl Pts',(19.7210657576844,-17.0777779408324,-7.95077026737695));
#85447=CARTESIAN_POINT('Ctrl Pts',(19.6554099365354,-17.0460375846167,-7.9463978266134));
#85448=CARTESIAN_POINT('Ctrl Pts',(19.5897524365599,-17.0142964167966,-7.94202527404605));
#85449=CARTESIAN_POINT('Ctrl Pts',(19.5224572790419,-16.9859539746119,-7.9376527214787));
#85450=CARTESIAN_POINT('Ctrl Pts',(19.4539119391446,-16.9611670587724,-7.93328016891136));
#85451=CARTESIAN_POINT('Ctrl Pts',(19.385295460308,-16.9363544181366,-7.92890307834403));
#85452=CARTESIAN_POINT('Ctrl Pts',(19.3154266631729,-16.9151048356875,-7.9245259877767));
#85453=CARTESIAN_POINT('Ctrl Pts',(19.2447099626404,-16.8975257767351,-7.92014889720936));
#85454=CARTESIAN_POINT('Ctrl Pts',(19.1739546410931,-16.8799371172062,-7.91576941615042));
#85455=CARTESIAN_POINT('Ctrl Pts',(19.1023509680262,-16.8660230644093,-7.91138993509147));
#85456=CARTESIAN_POINT('Ctrl Pts',(19.0303127030105,-16.8558397527778,-7.90701045403253));
#85457=CARTESIAN_POINT('Ctrl Pts',(18.9581467506537,-16.8456383912948,-7.90262321037281));
#85458=CARTESIAN_POINT('Ctrl Pts',(18.8855451489719,-16.8391810190706,-7.89823596671308));
#85459=CARTESIAN_POINT('Ctrl Pts',(18.8129253294089,-16.8364717462587,-7.89384872305336));
#85460=CARTESIAN_POINT('Ctrl Pts',(18.7635508497353,-16.8346297018115,-7.89086582011855));
#85461=CARTESIAN_POINT('Ctrl Pts',(18.7141679744269,-16.834519193629,-7.88788291718374));
#85462=CARTESIAN_POINT('Ctrl Pts',(18.6649065603161,-16.8361278165748,-7.88490001424893));
#85463=CARTESIAN_POINT('Ctrl Pts',(18.5924370961486,-16.8384942943756,-7.88051180531803));
#85464=CARTESIAN_POINT('Ctrl Pts',(18.5199478924754,-16.8445928606293,-7.87612359638714));
#85465=CARTESIAN_POINT('Ctrl Pts',(18.4478546672522,-16.8544276297237,-7.87173538745625));
#85466=CARTESIAN_POINT('Ctrl Pts',(18.3758684403285,-16.8642478023901,-7.86735369135498));
#85467=CARTESIAN_POINT('Ctrl Pts',(18.3042774991949,-16.8777931053665,-7.86297199525372));
#85468=CARTESIAN_POINT('Ctrl Pts',(18.2334957741929,-16.8950156733827,-7.85859029915245));
#85469=CARTESIAN_POINT('Ctrl Pts',(18.1627972233507,-16.9122180035109,-7.85421375189281));
#85470=CARTESIAN_POINT('Ctrl Pts',(18.0929064660606,-16.9330889013489,-7.84983720463317));
#85471=CARTESIAN_POINT('Ctrl Pts',(18.0242288363219,-16.957529169125,-7.84546065737353));
#85472=CARTESIAN_POINT('Ctrl Pts',(17.9555947609379,-16.9819539372385,-7.84108688565657));
#85473=CARTESIAN_POINT('Ctrl Pts',(17.8881727399597,-17.0099434225998,-7.8367131139396));
#85474=CARTESIAN_POINT('Ctrl Pts',(17.8223531243443,-17.0413485471946,-7.83233934222264));
#85475=CARTESIAN_POINT('Ctrl Pts',(17.7565535378591,-17.0727441151046,-7.82796690145909));
#85476=CARTESIAN_POINT('Ctrl Pts',(17.6923558237636,-17.1075530511353,-7.82359446069555));
#85477=CARTESIAN_POINT('Ctrl Pts',(17.6301289564798,-17.1455787536464,-7.819222019932));
#85478=CARTESIAN_POINT('Ctrl Pts',(17.5679004980477,-17.1836054284792,-7.81484946736464));
#85479=CARTESIAN_POINT('Ctrl Pts',(17.5076433970481,-17.2248487798647,-7.81047691479728));
#85480=CARTESIAN_POINT('Ctrl Pts',(17.4496992310201,-17.2690678757604,-7.80610436222991));
#85481=CARTESIAN_POINT('Ctrl Pts',(17.3916949283513,-17.3133328639015,-7.80172727166259));
#85482=CARTESIAN_POINT('Ctrl Pts',(17.3360087376083,-17.3605794693657,-7.79735018109527));
#85483=CARTESIAN_POINT('Ctrl Pts',(17.2829499222259,-17.4105258121552,-7.79297309052795));
#85484=CARTESIAN_POINT('Ctrl Pts',(17.2298621294551,-17.4604994324963,-7.78859360946901));
#85485=CARTESIAN_POINT('Ctrl Pts',(17.1794049028396,-17.5131753771404,-7.78421412841008));
#85486=CARTESIAN_POINT('Ctrl Pts',(17.1318494027623,-17.5682361242716,-7.77983464735114));
#85487=CARTESIAN_POINT('Ctrl Pts',(17.0842096108804,-17.6233944662074,-7.77544740369142));
#85488=CARTESIAN_POINT('Ctrl Pts',(17.0394821127491,-17.6809456706579,-7.7710601600317));
#85489=CARTESIAN_POINT('Ctrl Pts',(16.9978963120804,-17.7405409685871,-7.76667291637198));
#85490=CARTESIAN_POINT('Ctrl Pts',(16.9696219748237,-17.7810600285899,-7.76369001343715));
#85491=CARTESIAN_POINT('Ctrl Pts',(16.9427990411462,-17.8225233957318,-7.76070711050233));
#85492=CARTESIAN_POINT('Ctrl Pts',(16.9174873693318,-17.864815166302,-7.7577242075675));
#85493=CARTESIAN_POINT('Ctrl Pts',(16.8789674908493,-17.9291757456869,-7.75318475796428));
#85494=CARTESIAN_POINT('Ctrl Pts',(16.843807884674,-17.995692576386,-7.74864530836106));
#85495=CARTESIAN_POINT('Ctrl Pts',(16.8122472000427,-18.0639937073104,-7.74410585875784));
#85496=CARTESIAN_POINT('Ctrl Pts',(16.7803526868129,-18.1330172836152,-7.73951839377989));
#85497=CARTESIAN_POINT('Ctrl Pts',(16.7521339850622,-18.2038627902841,-7.73493092880195));
#85498=CARTESIAN_POINT('Ctrl Pts',(16.727791895044,-18.2761168447069,-7.730343463824));
#85499=CARTESIAN_POINT('Ctrl Pts',(16.7037989805433,-18.3473344496374,-7.72582180381417));
#85500=CARTESIAN_POINT('Ctrl Pts',(16.6835723608134,-18.4199200369919,-7.72130014380433));
#85501=CARTESIAN_POINT('Ctrl Pts',(16.6672572513858,-18.493455115555,-7.7167784837945));
#85502=CARTESIAN_POINT('Ctrl Pts',(16.6505859845116,-18.5685954586082,-7.7121581163325));
#85503=CARTESIAN_POINT('Ctrl Pts',(16.6379992287984,-18.6447268210055,-7.7075377488705));
#85504=CARTESIAN_POINT('Ctrl Pts',(16.6295984951253,-18.7213849391715,-7.7029173814085));
#85505=CARTESIAN_POINT('Ctrl Pts',(16.6211977614521,-18.7980430573374,-7.6982970139465));
#85506=CARTESIAN_POINT('Ctrl Pts',(16.6169831628437,-18.8752274520633,-7.6936766464845));
#85507=CARTESIAN_POINT('Ctrl Pts',(16.617000050606,-18.9524628884561,-7.6890562790225));
#85508=CARTESIAN_POINT('Ctrl Pts',(16.6203930087273,-18.9524685809736,-7.68905589348695));
#85509=CARTESIAN_POINT('Ctrl Pts',(16.6199117165189,-19.2000067410856,-7.67422393562464));
#85510=CARTESIAN_POINT('Ctrl Pts',(16.6606020197591,-19.4473941720768,-7.65939197776232));
#85511=CARTESIAN_POINT('Ctrl Pts',(16.7430902533864,-19.6789409674447,-7.64456001990001));
#85512=CARTESIAN_POINT('Origin',(18.734,-18.952,0.));
#85513=CARTESIAN_POINT('',(16.7454194485728,-19.6781104533646,-6.845005987876));
#85514=CARTESIAN_POINT('',(16.7454194581678,-19.6781104796424,-7.06814844662885));
#85515=CARTESIAN_POINT('',(16.7454194499637,-19.6781104571739,0.));
#85516=CARTESIAN_POINT('',(16.6170002518876,-18.9509672890084,-7.10922274860006));
#85517=CARTESIAN_POINT('Ctrl Pts',(16.7454194581678,-19.6781104796424,-7.06814844662885));
#85518=CARTESIAN_POINT('Ctrl Pts',(16.7207165638647,-19.6104572831724,-7.07229326072067));
#85519=CARTESIAN_POINT('Ctrl Pts',(16.6994767838628,-19.5415729101478,-7.07632982305453));
#85520=CARTESIAN_POINT('Ctrl Pts',(16.6386705851604,-19.3014695034662,-7.08999348029963));
#85521=CARTESIAN_POINT('Ctrl Pts',(16.6169146031621,-19.1265423838649,-7.0992095971379));
#85522=CARTESIAN_POINT('Ctrl Pts',(16.6170002518876,-18.9509672890084,-7.10922274860006));
#85523=CARTESIAN_POINT('Ctrl Pts',(16.617000253271,-18.9509644570508,-7.10922291010835));
#85524=CARTESIAN_POINT('Ctrl Pts',(16.6170133611986,-18.9241674230888,-7.11075116213054));
#85525=CARTESIAN_POINT('Ctrl Pts',(16.6175352641052,-18.8973740236385,-7.11229811087022));
#85526=CARTESIAN_POINT('Ctrl Pts',(16.6191227647428,-18.8561184599557,-7.11471892900856));
#85527=CARTESIAN_POINT('Ctrl Pts',(16.6198286092063,-18.8416446884933,-7.11557561664734));
#85528=CARTESIAN_POINT('Ctrl Pts',(16.620960018787,-18.8224889256946,-7.11672055060971));
#85529=CARTESIAN_POINT('Ctrl Pts',(16.6212526901732,-18.8177990892457,-7.11700174460842));
#85530=CARTESIAN_POINT('Ctrl Pts',(16.6217938177868,-18.8095688228847,-7.11749682870153));
#85531=CARTESIAN_POINT('Ctrl Pts',(16.622035569275,-18.8060279501914,-7.11771035080805));
#85532=CARTESIAN_POINT('Ctrl Pts',(16.6225281743189,-18.7990703883075,-7.11813096599797));
#85533=CARTESIAN_POINT('Ctrl Pts',(16.6227784202911,-18.7956536599959,-7.11833802549928));
#85534=CARTESIAN_POINT('Ctrl Pts',(16.6233330675064,-18.7883250307724,-7.11878325544969));
#85535=CARTESIAN_POINT('Ctrl Pts',(16.6236400496722,-18.7844133807662,-7.11902156683151));
#85536=CARTESIAN_POINT('Ctrl Pts',(16.62447652773,-18.7741216540878,-7.11965029844778));
#85537=CARTESIAN_POINT('Ctrl Pts',(16.6250240886659,-18.7677431439984,-7.12004171197717));
#85538=CARTESIAN_POINT('Ctrl Pts',(16.6274167974474,-18.7412797610905,-7.12167258776839));
#85539=CARTESIAN_POINT('Ctrl Pts',(16.6295199350736,-18.7212200268298,-7.1229254821994));
#85540=CARTESIAN_POINT('Ctrl Pts',(16.632414264621,-18.6969616360284,-7.12445836054343));
#85541=CARTESIAN_POINT('Ctrl Pts',(16.6329320498058,-18.6927305680807,-7.12472637581752));
#85542=CARTESIAN_POINT('Ctrl Pts',(16.6366907780554,-18.662767065183,-7.12662891591402));
#85543=CARTESIAN_POINT('Ctrl Pts',(16.6403914554856,-18.6370955500176,-7.12828251233134));
#85544=CARTESIAN_POINT('Ctrl Pts',(16.6729288516913,-18.437433946874,-7.141296005818));
#85545=CARTESIAN_POINT('Ctrl Pts',(16.722934133997,-18.2675918236132,-7.15319938306154));
#85546=CARTESIAN_POINT('Ctrl Pts',(16.8171419203852,-18.0515199209895,-7.16840078661708));
#85547=CARTESIAN_POINT('Ctrl Pts',(16.8431322770721,-17.9981501512624,-7.17216862668756));
#85548=CARTESIAN_POINT('Ctrl Pts',(16.8885290151137,-17.9141005654831,-7.17811565638349));
#85549=CARTESIAN_POINT('Ctrl Pts',(16.9065396945572,-17.882707019612,-7.18034034020732));
#85550=CARTESIAN_POINT('Ctrl Pts',(16.931074012134,-17.8423746993651,-7.18320477377927));
#85551=CARTESIAN_POINT('Ctrl Pts',(16.9368742870969,-17.8330050917248,-7.18387067969934));
#85552=CARTESIAN_POINT('Ctrl Pts',(16.9464487817368,-17.8178051899742,-7.18495183978114));
#85553=CARTESIAN_POINT('Ctrl Pts',(16.9501789443334,-17.8119475151765,-7.18536871101327));
#85554=CARTESIAN_POINT('Ctrl Pts',(16.9574233689125,-17.8006938120197,-7.18617006425167));
#85555=CARTESIAN_POINT('Ctrl Pts',(16.9609335551142,-17.7952952632404,-7.18655469184895));
#85556=CARTESIAN_POINT('Ctrl Pts',(16.9690493356662,-17.7829372145805,-7.18743568328244));
#85557=CARTESIAN_POINT('Ctrl Pts',(16.9736715784317,-17.7759887351528,-7.18793141684298));
#85558=CARTESIAN_POINT('Ctrl Pts',(16.9861098378325,-17.7575283223654,-7.18924961557565));
#85559=CARTESIAN_POINT('Ctrl Pts',(16.9939985475541,-17.7460656871364,-7.1900693325874));
#85560=CARTESIAN_POINT('Ctrl Pts',(17.0581390682346,-17.6548065895051,-7.19660723570976));
#85561=CARTESIAN_POINT('Ctrl Pts',(17.1197399411334,-17.5789054841399,-7.20210985633664));
#85562=CARTESIAN_POINT('Ctrl Pts',(17.2799634000678,-17.4072401993666,-7.21506336376851));
#85563=CARTESIAN_POINT('Ctrl Pts',(17.3830793570561,-17.3162994579983,-7.22236047349061));
#85564=CARTESIAN_POINT('Ctrl Pts',(17.535963248145,-17.2058489698827,-7.23281030874296));
#85565=CARTESIAN_POINT('Ctrl Pts',(17.5787448784982,-17.1772548435322,-7.2357023421666));
#85566=CARTESIAN_POINT('Ctrl Pts',(17.6378691584124,-17.140781808804,-7.23971580381614));
#85567=CARTESIAN_POINT('Ctrl Pts',(17.6533358911243,-17.131511275045,-7.24076721868491));
#85568=CARTESIAN_POINT('Ctrl Pts',(17.6763955712468,-17.1180870459139,-7.2423398754025));
#85569=CARTESIAN_POINT('Ctrl Pts',(17.6838989937448,-17.1137802846113,-7.24285238914577));
#85570=CARTESIAN_POINT('Ctrl Pts',(17.6975309911582,-17.1060665887894,-7.24378531425949));
#85571=CARTESIAN_POINT('Ctrl Pts',(17.7036505379642,-17.1026438558614,-7.24420476686297));
#85572=CARTESIAN_POINT('Ctrl Pts',(17.7133176302825,-17.0972998150672,-7.24486858516731));
#85573=CARTESIAN_POINT('Ctrl Pts',(17.7168539213188,-17.0953581040382,-7.24511166736501));
#85574=CARTESIAN_POINT('Ctrl Pts',(17.7204047838171,-17.0934215814666,-7.24535602607436));
#85575=CARTESIAN_POINT('Ctrl Pts',(17.7204138606574,-17.0934166313454,-7.24535665071454));
#85576=CARTESIAN_POINT('Ctrl Pts',(17.7204320698581,-17.0934067009977,-7.24535790381921));
#85577=CARTESIAN_POINT('Ctrl Pts',(17.7204412018053,-17.0934017209977,-7.2453585322553));
#85578=CARTESIAN_POINT('Ctrl Pts',(17.7204595211243,-17.0933917309476,-7.24535979294531));
#85579=CARTESIAN_POINT('Ctrl Pts',(17.7204687089969,-17.0933867206256,-7.2453604252337));
#85580=CARTESIAN_POINT('Ctrl Pts',(17.7204871404368,-17.0933766697873,-7.24536169364699));
#85581=CARTESIAN_POINT('Ctrl Pts',(17.7204963842381,-17.0933716291446,-7.24536232978799));
#85582=CARTESIAN_POINT('Ctrl Pts',(17.7205149285648,-17.0933615171072,-7.24536360597739));
#85583=CARTESIAN_POINT('Ctrl Pts',(17.7205242285134,-17.0933564460279,-7.24536424598611));
#85584=CARTESIAN_POINT('Ctrl Pts',(17.7205428852673,-17.0933462730484,-7.24536552992014));
#85585=CARTESIAN_POINT('Ctrl Pts',(17.7205522423073,-17.0933411710211,-7.24536617386162));
#85586=CARTESIAN_POINT('Ctrl Pts',(17.7205710139306,-17.0933309357744,-7.24536746570849));
#85587=CARTESIAN_POINT('Ctrl Pts',(17.720580427922,-17.0933258028788,-7.24536811357317));
#85588=CARTESIAN_POINT('Ctrl Pts',(17.7205993135353,-17.0933155058512,-7.2453694132725));
#85589=CARTESIAN_POINT('Ctrl Pts',(17.7206087854619,-17.0933103415542,-7.24537006512815));
#85590=CARTESIAN_POINT('Ctrl Pts',(17.7206277871157,-17.0932999816346,-7.2453713728212));
#85591=CARTESIAN_POINT('Ctrl Pts',(17.7206373170627,-17.0932947858932,-7.24537202867376));
#85592=CARTESIAN_POINT('Ctrl Pts',(17.7206564352576,-17.0932843628154,-7.24537334439513));
#85593=CARTESIAN_POINT('Ctrl Pts',(17.7206660236408,-17.0932791354065,-7.24537400427328));
#85594=CARTESIAN_POINT('Ctrl Pts',(17.7206852592978,-17.0932686486756,-7.2453753280865));
#85595=CARTESIAN_POINT('Ctrl Pts',(17.7206949064925,-17.0932633893979,-7.24537599201615));
#85596=CARTESIAN_POINT('Ctrl Pts',(17.7207142599682,-17.0932528388266,-7.24537732394591));
#85597=CARTESIAN_POINT('Ctrl Pts',(17.7207239666169,-17.0932475473335,-7.24537799197136));
#85598=CARTESIAN_POINT('Ctrl Pts',(17.7207434019682,-17.0932369525225,-7.24537932954415));
#85599=CARTESIAN_POINT('Ctrl Pts',(17.7207531870614,-17.0932316184647,-7.24538000297263));
#85600=CARTESIAN_POINT('Ctrl Pts',(17.7207727992919,-17.0932209276323,-7.24538135272692));
#85601=CARTESIAN_POINT('Ctrl Pts',(17.720782625299,-17.093215571474,-7.24538202897517));
#85602=CARTESIAN_POINT('Ctrl Pts',(17.7208023394488,-17.0932048254899,-7.24538338575223));
#85603=CARTESIAN_POINT('Ctrl Pts',(17.7208122258835,-17.0931994365966,-7.2453840661635));
#85604=CARTESIAN_POINT('Ctrl Pts',(17.7208320614158,-17.0931886248587,-7.245385431303));
#85605=CARTESIAN_POINT('Ctrl Pts',(17.7208420089104,-17.0931832028893,-7.2453861159209));
#85606=CARTESIAN_POINT('Ctrl Pts',(17.7208619996744,-17.0931723069557,-7.2453874917526));
#85607=CARTESIAN_POINT('Ctrl Pts',(17.7208719923007,-17.0931668605965,-7.24538817948079));
#85608=CARTESIAN_POINT('Ctrl Pts',(17.7238842193324,-17.0915251142421,-7.24559549240892));
#85609=CARTESIAN_POINT('Ctrl Pts',(17.7268903493805,-17.0898961248331,-7.24580258652638));
#85610=CARTESIAN_POINT('Ctrl Pts',(17.7339397814265,-17.0860981773077,-7.24628868545938));
#85611=CARTESIAN_POINT('Ctrl Pts',(17.73798618483,-17.0839350836294,-7.24656805799393));
#85612=CARTESIAN_POINT('Ctrl Pts',(17.7504630090659,-17.0773173859405,-7.2474304842157));
#85613=CARTESIAN_POINT('Ctrl Pts',(17.7589163827721,-17.0729066421298,-7.24801619947914));
#85614=CARTESIAN_POINT('Ctrl Pts',(17.8726190897224,-17.0145534441301,-7.25591016519681));
#85615=CARTESIAN_POINT('Ctrl Pts',(17.9821673160887,-16.9694719843812,-7.26368497769928));
#85616=CARTESIAN_POINT('Ctrl Pts',(18.199216489691,-16.9007391822163,-7.27872419300949));
#85617=CARTESIAN_POINT('Ctrl Pts',(18.305955198866,-16.8758387687581,-7.28596054281728));
#85618=CARTESIAN_POINT('Ctrl Pts',(18.4890359883618,-16.8478562113822,-7.29786573935853));
#85619=CARTESIAN_POINT('Ctrl Pts',(18.5644921174166,-16.8404371346402,-7.30263387129201));
#85620=CARTESIAN_POINT('Ctrl Pts',(18.6590783958438,-16.8362417025176,-7.3084345722606));
#85621=CARTESIAN_POINT('Ctrl Pts',(18.6779762187534,-16.8356569766535,-7.30958494753696));
#85622=CARTESIAN_POINT('Ctrl Pts',(18.7054508277715,-16.8351751538426,-7.31124541240657));
#85623=CARTESIAN_POINT('Ctrl Pts',(18.7140227529653,-16.8350769032575,-7.31176177211313));
#85624=CARTESIAN_POINT('Ctrl Pts',(18.7290470400866,-16.8349959621119,-7.31266390696164));
#85625=CARTESIAN_POINT('Ctrl Pts',(18.7354991217446,-16.8349906985774,-7.31305038402281));
#85626=CARTESIAN_POINT('Ctrl Pts',(18.7480234389187,-16.8350377386504,-7.31379879919102));
#85627=CARTESIAN_POINT('Ctrl Pts',(18.7540956170281,-16.8350866715485,-7.31416083903772));
#85628=CARTESIAN_POINT('Ctrl Pts',(18.7686043123388,-16.8352660225221,-7.31502398017245));
#85629=CARTESIAN_POINT('Ctrl Pts',(18.777040467128,-16.8354207524491,-7.31552431696063));
#85630=CARTESIAN_POINT('Ctrl Pts',(18.8074392554409,-16.8361601277919,-7.31732185571079));
#85631=CARTESIAN_POINT('Ctrl Pts',(18.8293938734943,-16.8370362293236,-7.31860994896036));
#85632=CARTESIAN_POINT('Ctrl Pts',(19.0379766845316,-16.848614410365,-7.33076152277251));
#85633=CARTESIAN_POINT('Ctrl Pts',(19.2224218394706,-16.8836473321735,-7.34075359847646));
#85634=CARTESIAN_POINT('Ctrl Pts',(19.4751177952318,-16.96738027662,-7.35526996369034));
#85635=CARTESIAN_POINT('Ctrl Pts',(19.548889158123,-16.9965141948136,-7.35963130817193));
#85636=CARTESIAN_POINT('Ctrl Pts',(19.6533465863166,-17.0447056169168,-7.36621325344225));
#85637=CARTESIAN_POINT('Ctrl Pts',(19.6854582623626,-17.0605199334064,-7.36829547362044));
#85638=CARTESIAN_POINT('Ctrl Pts',(19.7237508746885,-17.080600060355,-7.3708687007561));
#85639=CARTESIAN_POINT('Ctrl Pts',(19.7303318437116,-17.0840954570668,-7.37131421667079));
#85640=CARTESIAN_POINT('Ctrl Pts',(19.7405543034133,-17.0895943761088,-7.37201159214417));
#85641=CARTESIAN_POINT('Ctrl Pts',(19.744208654356,-17.0915740413541,-7.37226196105825));
#85642=CARTESIAN_POINT('Ctrl Pts',(19.7509877783966,-17.0952723472187,-7.37272845052502));
#85643=CARTESIAN_POINT('Ctrl Pts',(19.7541140468696,-17.0969881270511,-7.37294438864439));
#85644=CARTESIAN_POINT('Ctrl Pts',(19.7611884180731,-17.1008940230815,-7.37343486583595));
#85645=CARTESIAN_POINT('Ctrl Pts',(19.7651338393522,-17.1030888640941,-7.37370970392245));
#85646=CARTESIAN_POINT('Ctrl Pts',(19.7753093798818,-17.1087922255504,-7.37442182568733));
#85647=CARTESIAN_POINT('Ctrl Pts',(19.7815287405006,-17.1123196856743,-7.37486028233949));
#85648=CARTESIAN_POINT('Ctrl Pts',(19.8197545465749,-17.1342570572481,-7.37757438090023));
#85649=CARTESIAN_POINT('Ctrl Pts',(19.8512906116546,-17.1534690301272,-7.37989686263477));
#85650=CARTESIAN_POINT('Ctrl Pts',(20.0255444227163,-17.2659773465048,-7.39313679436249));
#85651=CARTESIAN_POINT('Ctrl Pts',(20.1570850951643,-17.3754241632414,-7.40464131185876));
#85652=CARTESIAN_POINT('Ctrl Pts',(20.3393638462973,-17.5686887408063,-7.42190384273487));
#85653=CARTESIAN_POINT('Ctrl Pts',(20.3999164767335,-17.6422406198714,-7.42794872778959));
#85654=CARTESIAN_POINT('Ctrl Pts',(20.4677576804373,-17.7369980560549,-7.43510701715657));
#85655=CARTESIAN_POINT('Ctrl Pts',(20.479930989718,-17.7545567028381,-7.43640920745788));
#85656=CARTESIAN_POINT('Ctrl Pts',(20.4968549085228,-17.7797744825177,-7.43824590489082));
#85657=CARTESIAN_POINT('Ctrl Pts',(20.5018253344634,-17.7872838615844,-7.43878869632849));
#85658=CARTESIAN_POINT('Ctrl Pts',(20.5103146616573,-17.8002891834805,-7.43972170567695));
#85659=CARTESIAN_POINT('Ctrl Pts',(20.5138563151837,-17.8057700575856,-7.44011277287772));
#85660=CARTESIAN_POINT('Ctrl Pts',(20.520587165513,-17.8162927801484,-7.44085954613924));
#85661=CARTESIAN_POINT('Ctrl Pts',(20.5237804979782,-17.8213318968956,-7.441215403657));
#85662=CARTESIAN_POINT('Ctrl Pts',(20.5320248987022,-17.8344641066001,-7.44213827486938));
#85663=CARTESIAN_POINT('Ctrl Pts',(20.5370426746313,-17.8425780210501,-7.4427040549919));
#85664=CARTESIAN_POINT('Ctrl Pts',(20.5539458131906,-17.8703285704087,-7.44462431866771));
#85665=CARTESIAN_POINT('Ctrl Pts',(20.565566857233,-17.8901248883897,-7.4459691489453));
#85666=CARTESIAN_POINT('Ctrl Pts',(20.6634795157496,-18.0633093628527,-7.45753007006511));
#85667=CARTESIAN_POINT('Ctrl Pts',(20.7306536824789,-18.2267117827958,-7.46699016710072));
#85668=CARTESIAN_POINT('Ctrl Pts',(20.7995675841096,-18.4801663971577,-7.48128271780431));
#85669=CARTESIAN_POINT('Ctrl Pts',(20.8171447467062,-18.565086594589,-7.48602724678504));
#85670=CARTESIAN_POINT('Ctrl Pts',(20.8348366408193,-18.6881854330896,-7.49312839260848));
#85671=CARTESIAN_POINT('Ctrl Pts',(20.839204550445,-18.7256681167404,-7.49532030000414));
#85672=CARTESIAN_POINT('Ctrl Pts',(20.8432429871891,-18.770781146182,-7.49801516787105));
#85673=CARTESIAN_POINT('Ctrl Pts',(20.8438772085154,-18.7783209481372,-7.49846746253409));
#85674=CARTESIAN_POINT('Ctrl Pts',(20.8447991098677,-18.790032102848,-7.49917315517864));
#85675=CARTESIAN_POINT('Ctrl Pts',(20.8451148812046,-18.7942012687356,-7.49942500438653));
#85676=CARTESIAN_POINT('Ctrl Pts',(20.8456769241264,-18.801925787125,-7.49989282246133));
#85677=CARTESIAN_POINT('Ctrl Pts',(20.8459265695905,-18.8054808362956,-7.50010859985754));
#85678=CARTESIAN_POINT('Ctrl Pts',(20.8464698839516,-18.8135078558083,-7.50059687333769));
#85679=CARTESIAN_POINT('Ctrl Pts',(20.8467583282351,-18.8179801125796,-7.50086965698074));
#85680=CARTESIAN_POINT('Ctrl Pts',(20.847565721075,-18.8311494646103,-7.50167503304515));
#85681=CARTESIAN_POINT('Ctrl Pts',(20.8480451753326,-18.8398487634193,-7.50220975779561));
#85682=CARTESIAN_POINT('Ctrl Pts',(20.8510717496147,-18.9017109229873,-7.50603039148208));
#85683=CARTESIAN_POINT('Ctrl Pts',(20.8516666585363,-18.9549457950084,-7.50941293015124));
#85684=CARTESIAN_POINT('Ctrl Pts',(20.8497711832953,-19.0263960297577,-7.51403194162836));
#85685=CARTESIAN_POINT('Ctrl Pts',(20.849050744181,-19.0446433585941,-7.51521854577946));
#85686=CARTESIAN_POINT('Ctrl Pts',(20.8455799974383,-19.1108191534427,-7.5195424888418));
#85687=CARTESIAN_POINT('Ctrl Pts',(20.8414357445182,-19.1586590493085,-7.52270729218872));
#85688=CARTESIAN_POINT('Ctrl Pts',(20.822529538245,-19.3149004441581,-7.53310346283865));
#85689=CARTESIAN_POINT('Ctrl Pts',(20.8009934882782,-19.4223123959892,-7.54033585418034));
#85690=CARTESIAN_POINT('Ctrl Pts',(20.7562714471666,-19.580603704721,-7.55090864596328));
#85691=CARTESIAN_POINT('Ctrl Pts',(20.7392270189506,-19.6330211794603,-7.55439742641563));
#85692=CARTESIAN_POINT('Ctrl Pts',(20.7082836935235,-19.7168983166133,-7.55995449481805));
#85693=CARTESIAN_POINT('Ctrl Pts',(20.6956309787732,-19.7487870836441,-7.56206121286768));
#85694=CARTESIAN_POINT('Ctrl Pts',(20.6779792150162,-19.7903022293691,-7.56479758075175));
#85695=CARTESIAN_POINT('Ctrl Pts',(20.6736739501927,-19.8002162400644,-7.56545056847658));
#85696=CARTESIAN_POINT('Ctrl Pts',(20.6664968964457,-19.8164028730471,-7.56651604785952));
#85697=CARTESIAN_POINT('Ctrl Pts',(20.6636700781835,-19.8226951089903,-7.56693006884819));
#85698=CARTESIAN_POINT('Ctrl Pts',(20.6581377968209,-19.8348501733766,-7.56772958179424));
#85699=CARTESIAN_POINT('Ctrl Pts',(20.6554361697854,-19.840714654235,-7.56811520006939));
#85700=CARTESIAN_POINT('Ctrl Pts',(20.6491350499264,-19.8542295849077,-7.56900363049126));
#85701=CARTESIAN_POINT('Ctrl Pts',(20.6455164563949,-19.8618710476955,-7.56950577652471));
#85702=CARTESIAN_POINT('Ctrl Pts',(20.6356588493757,-19.882369191595,-7.57085242448115));
#85703=CARTESIAN_POINT('Ctrl Pts',(20.6293352079079,-19.895184858156,-7.57169398473442));
#85704=CARTESIAN_POINT('Ctrl Pts',(20.5701076035913,-20.0122156999669,-7.57937803238027));
#85705=CARTESIAN_POINT('Ctrl Pts',(20.508785386332,-20.1119528273776,-7.58590361758807));
#85706=CARTESIAN_POINT('Ctrl Pts',(20.3430318087841,-20.3373670978567,-7.60122072336177));
#85707=CARTESIAN_POINT('Ctrl Pts',(20.2317156437972,-20.4570120549477,-7.6098287101515));
#85708=CARTESIAN_POINT('Ctrl Pts',(20.0832086240643,-20.5836770448465,-7.62103837067635));
#85709=CARTESIAN_POINT('Ctrl Pts',(20.0581389034589,-20.6040864980786,-7.62292397217365));
#85710=CARTESIAN_POINT('Ctrl Pts',(20.026905799962,-20.6283459733375,-7.62527875170373));
#85711=CARTESIAN_POINT('Ctrl Pts',(20.0211756452397,-20.6327498578838,-7.62571099476218));
#85712=CARTESIAN_POINT('Ctrl Pts',(20.0121540464092,-20.6396101743367,-7.62639207054822));
#85713=CARTESIAN_POINT('Ctrl Pts',(20.0088777497708,-20.6420865626817,-7.62663952362488));
#85714=CARTESIAN_POINT('Ctrl Pts',(20.0027381899975,-20.6466991375734,-7.62710348726891));
#85715=CARTESIAN_POINT('Ctrl Pts',(19.9998767187544,-20.6488376156566,-7.62731983349712));
#85716=CARTESIAN_POINT('Ctrl Pts',(19.9933296662705,-20.6537046806974,-7.62781506717365));
#85717=CARTESIAN_POINT('Ctrl Pts',(19.9896406359132,-20.6564285321438,-7.62809427792971));
#85718=CARTESIAN_POINT('Ctrl Pts',(19.9782646328368,-20.664771200313,-7.62895571946072));
#85719=CARTESIAN_POINT('Ctrl Pts',(19.9705487028104,-20.6703500688002,-7.62954060318709));
#85720=CARTESIAN_POINT('Ctrl Pts',(19.8652733990393,-20.7453913035297,-7.63752583935986));
#85721=CARTESIAN_POINT('Ctrl Pts',(19.7620392319504,-20.8064973880513,-7.64540431265029));
#85722=CARTESIAN_POINT('Ctrl Pts',(19.5561164994488,-20.9058876651664,-7.66050997952928));
#85723=CARTESIAN_POINT('Ctrl Pts',(19.4545093650631,-20.9455953148074,-7.66770930842107));
#85724=CARTESIAN_POINT('Ctrl Pts',(19.2785781956098,-20.9991303388827,-7.67952435461965));
#85725=CARTESIAN_POINT('Ctrl Pts',(19.205750333317,-21.0171299713888,-7.68424034705386));
#85726=CARTESIAN_POINT('Ctrl Pts',(19.1136512399724,-21.0347643378857,-7.68998480594451));
#85727=CARTESIAN_POINT('Ctrl Pts',(19.0951422709268,-21.0380533663137,-7.69112852502209));
#85728=CARTESIAN_POINT('Ctrl Pts',(19.0681517051492,-21.0424795581679,-7.69278120577576));
#85729=CARTESIAN_POINT('Ctrl Pts',(19.059703537322,-21.0438124567707,-7.69329635533019));
#85730=CARTESIAN_POINT('Ctrl Pts',(19.0448713257135,-21.0460605548708,-7.69419709358531));
#85731=CARTESIAN_POINT('Ctrl Pts',(19.0384907888664,-21.0469978399845,-7.69458337756545));
#85732=CARTESIAN_POINT('Ctrl Pts',(19.0260884675414,-21.0487618535583,-7.69533193958978));
#85733=CARTESIAN_POINT('Ctrl Pts',(19.0200672159361,-21.0495918317346,-7.69569431692425));
#85734=CARTESIAN_POINT('Ctrl Pts',(19.0056573295866,-21.0515149100075,-7.69655909101826));
#85735=CARTESIAN_POINT('Ctrl Pts',(18.9972655118182,-21.0525836892411,-7.69706071659597));
#85736=CARTESIAN_POINT('Ctrl Pts',(18.9669181698148,-21.0562639998756,-7.69886774890163));
#85737=CARTESIAN_POINT('Ctrl Pts',(18.9449279887498,-21.0585818979752,-7.70016391874448));
#85738=CARTESIAN_POINT('Ctrl Pts',(18.7380773542932,-21.0771135936689,-7.71224252135256));
#85739=CARTESIAN_POINT('Ctrl Pts',(18.5518804069917,-21.0693008479196,-7.72216856688949));
#85740=CARTESIAN_POINT('Ctrl Pts',(18.2612635610973,-21.0184434176323,-7.73825201626216));
#85741=CARTESIAN_POINT('Ctrl Pts',(18.155091895123,-20.9912467067075,-7.74428538351675));
#85742=CARTESIAN_POINT('Ctrl Pts',(18.0403466907054,-20.9521683076997,-7.75143993975321));
#85743=CARTESIAN_POINT('Ctrl Pts',(18.0292116778076,-20.9482719201642,-7.75214109640204));
#85744=CARTESIAN_POINT('Ctrl Pts',(18.0134012884487,-20.942590749691,-7.75314724322877));
#85745=CARTESIAN_POINT('Ctrl Pts',(18.0086985461336,-20.940882056758,-7.75344785950515));
#85746=CARTESIAN_POINT('Ctrl Pts',(18.0005943822121,-20.9379049268266,-7.75396829664887));
#85747=CARTESIAN_POINT('Ctrl Pts',(17.9971900495196,-20.9366443699878,-7.75418764843126));
#85748=CARTESIAN_POINT('Ctrl Pts',(17.9905874773202,-20.9341802386042,-7.7546145190964));
#85749=CARTESIAN_POINT('Ctrl Pts',(17.9873889037563,-20.9329776747283,-7.75482197166372));
#85750=CARTESIAN_POINT('Ctrl Pts',(17.9787493745823,-20.929705584748,-7.755384065364));
#85751=CARTESIAN_POINT('Ctrl Pts',(17.9733140678972,-20.9276213701007,-7.75573957307488));
#85752=CARTESIAN_POINT('Ctrl Pts',(17.9530708093983,-20.9197629981159,-7.75707047437662));
#85753=CARTESIAN_POINT('Ctrl Pts',(17.9383198625403,-20.9138447190879,-7.75805398748051));
#85754=CARTESIAN_POINT('Ctrl Pts',(17.8094424093461,-20.8604448132691,-7.76675887775666));
#85755=CARTESIAN_POINT('Ctrl Pts',(17.6996216082782,-20.8032222864274,-7.77493827884515));
#85756=CARTESIAN_POINT('Ctrl Pts',(17.4545040878102,-20.646851667991,-7.79415151237519));
#85757=CARTESIAN_POINT('Ctrl Pts',(17.3246942560686,-20.5405559789002,-7.80506941645519));
#85758=CARTESIAN_POINT('Ctrl Pts',(17.1939623449152,-20.4047307047863,-7.81664815580069));
#85759=CARTESIAN_POINT('Ctrl Pts',(17.1794268214328,-20.3891655312427,-7.81794608731221));
#85760=CARTESIAN_POINT('Ctrl Pts',(17.1590898587272,-20.3667183215896,-7.81977787410395));
#85761=CARTESIAN_POINT('Ctrl Pts',(17.1530939780275,-20.3600149275195,-7.82031995357325));
#85762=CARTESIAN_POINT('Ctrl Pts',(17.1428230022233,-20.3483836565338,-7.82125212340098));
#85763=CARTESIAN_POINT('Ctrl Pts',(17.1385276683435,-20.3434738929946,-7.82164305901465));
#85764=CARTESIAN_POINT('Ctrl Pts',(17.1303462116784,-20.334034422648,-7.82238984245075));
#85765=CARTESIAN_POINT('Ctrl Pts',(17.1264564218029,-20.329507990359,-7.82274584047264));
#85766=CARTESIAN_POINT('Ctrl Pts',(17.116390082127,-20.3176933838864,-7.82366964147331));
#85767=CARTESIAN_POINT('Ctrl Pts',(17.1102435877225,-20.3103796904132,-7.82423620585244));
#85768=CARTESIAN_POINT('Ctrl Pts',(17.0894465473258,-20.285290491069,-7.82616203298827));
#85769=CARTESIAN_POINT('Ctrl Pts',(17.0750363784865,-20.2673172073819,-7.82751156515189));
#85770=CARTESIAN_POINT('Ctrl Pts',(16.9537660341881,-20.1108968052215,-7.83901211840196));
#85771=CARTESIAN_POINT('Ctrl Pts',(16.8641495643365,-19.959938913254,-7.84841817815766));
#85772=CARTESIAN_POINT('Ctrl Pts',(16.7766289145641,-19.7596475759913,-7.86031011867401));
#85773=CARTESIAN_POINT('Ctrl Pts',(16.7603899223379,-19.7191097138761,-7.86269367145722));
#85774=CARTESIAN_POINT('Ctrl Pts',(16.7454194590822,-19.6781104821466,-7.86510586795993));
#85775=CARTESIAN_POINT('',(16.6156461116265,-18.9537405764281,-6.88905704663589));
#85776=CARTESIAN_POINT('Ctrl Pts',(16.7430902533864,-19.6789409674447,-7.64456001990001));
#85777=CARTESIAN_POINT('Ctrl Pts',(16.7690655542301,-19.7518543685999,-7.63988948022869));
#85778=CARTESIAN_POINT('Ctrl Pts',(17.0725682270039,-20.4707351681624,-7.5928270049969));
#85779=CARTESIAN_POINT('Ctrl Pts',(18.4531255376191,-21.4394563861295,-7.50337259420462));
#85780=CARTESIAN_POINT('Ctrl Pts',(20.673525152946,-20.5345839369853,-7.3761967875232));
#85781=CARTESIAN_POINT('Ctrl Pts',(21.1145308209525,-18.1777889518937,-7.24902098084176));
#85782=CARTESIAN_POINT('Ctrl Pts',(19.371547213141,-16.5312845504829,-7.12184517416032));
#85783=CARTESIAN_POINT('Ctrl Pts',(17.1752234457631,-17.0731746333353,-7.00185719609169));
#85784=CARTESIAN_POINT('Ctrl Pts',(16.6208560643663,-18.3695361560074,-6.92426115358356));
#85785=CARTESIAN_POINT('Ctrl Pts',(16.6156461116265,-18.9537405764281,-6.88905704663589));
#85786=CARTESIAN_POINT('Ctrl Pts',(16.6170007608245,-18.9537948065389,-6.88983560106466));
#85787=CARTESIAN_POINT('Ctrl Pts',(16.6170691195685,-19.0344248943613,-6.88542677740563));
#85788=CARTESIAN_POINT('Ctrl Pts',(16.6217438746711,-19.1149800361354,-6.8809632257301));
#85789=CARTESIAN_POINT('Ctrl Pts',(16.6337248070316,-19.2186387330682,-6.8749301875487));
#85790=CARTESIAN_POINT('Ctrl Pts',(16.6368453937014,-19.2421629775274,-6.87354145267081));
#85791=CARTESIAN_POINT('Ctrl Pts',(16.6412432763108,-19.2715211984353,-6.87177821045316));
#85792=CARTESIAN_POINT('Ctrl Pts',(16.6421508389439,-19.2774098743235,-6.8714230179003));
#85793=CARTESIAN_POINT('Ctrl Pts',(16.6437157810073,-19.2872867753239,-6.87082459126562));
#85794=CARTESIAN_POINT('Ctrl Pts',(16.6443597521227,-19.2912771311432,-6.87058208819888));
#85795=CARTESIAN_POINT('Ctrl Pts',(16.6455594684996,-19.2985781525279,-6.87013700514065));
#85796=CARTESIAN_POINT('Ctrl Pts',(16.6461116701162,-19.3018893982353,-6.86993462430001));
#85797=CARTESIAN_POINT('Ctrl Pts',(16.6472681666741,-19.3087240324362,-6.86951579339881));
#85798=CARTESIAN_POINT('Ctrl Pts',(16.6478735059419,-19.3122471785425,-6.86929928258382));
#85799=CARTESIAN_POINT('Ctrl Pts',(16.6492800583166,-19.3203110435557,-6.86880233975892));
#85800=CARTESIAN_POINT('Ctrl Pts',(16.6500871820472,-19.3248506756071,-6.86852157583359));
#85801=CARTESIAN_POINT('Ctrl Pts',(16.6526294580089,-19.3388834421341,-6.86765065397933));
#85802=CARTESIAN_POINT('Ctrl Pts',(16.6544146688601,-19.3483672202379,-6.86705775947629));
#85803=CARTESIAN_POINT('Ctrl Pts',(16.6734315752866,-19.4457264490839,-6.86092926727658));
#85804=CARTESIAN_POINT('Ctrl Pts',(16.6961558852748,-19.532427133864,-6.85512342797589));
#85805=CARTESIAN_POINT('Ctrl Pts',(16.7310304511555,-19.6377557645575,-6.8478320303573));
#85806=CARTESIAN_POINT('Ctrl Pts',(16.7380722943999,-19.6579889858539,-6.8464199563341));
#85807=CARTESIAN_POINT('Ctrl Pts',(16.7454194485728,-19.6781104533646,-6.84500598787601));
#85808=CARTESIAN_POINT('Origin',(18.734,-18.952,0.));
#85809=CARTESIAN_POINT('',(16.745419449956,-19.6781104571528,-6.04247203196383));
#85810=CARTESIAN_POINT('',(16.7454195726558,-19.6781107931876,-6.26710635146282));
#85811=CARTESIAN_POINT('',(16.7454194499637,-19.6781104571739,0.));
#85812=CARTESIAN_POINT('Ctrl Pts',(16.7454195726558,-19.6781107931876,-6.26710635146282));
#85813=CARTESIAN_POINT('Ctrl Pts',(16.7157171117681,-19.5967654490344,-6.27277684093396));
#85814=CARTESIAN_POINT('Ctrl Pts',(16.691004302357,-19.5135927381583,-6.27836338234672));
#85815=CARTESIAN_POINT('Ctrl Pts',(16.6614520768127,-19.3858238017327,-6.28658112014348));
#85816=CARTESIAN_POINT('Ctrl Pts',(16.6528139473508,-19.3422858750625,-6.28932035095603));
#85817=CARTESIAN_POINT('Ctrl Pts',(16.6436144425346,-19.2868388967681,-6.29273464287481));
#85818=CARTESIAN_POINT('Ctrl Pts',(16.6417764795419,-19.2751557132193,-6.29344995119706));
#85819=CARTESIAN_POINT('Ctrl Pts',(16.6389885133478,-19.256411908666,-6.29459111071411));
#85820=CARTESIAN_POINT('Ctrl Pts',(16.6379760965532,-19.2493609548218,-6.29501893121541));
#85821=CARTESIAN_POINT('Ctrl Pts',(16.6361227659771,-19.235973530818,-6.29582850592141));
#85822=CARTESIAN_POINT('Ctrl Pts',(16.6352749264707,-19.2296381140277,-6.29621047502385));
#85823=CARTESIAN_POINT('Ctrl Pts',(16.6334140696412,-19.2152372035021,-6.29707615108004));
#85824=CARTESIAN_POINT('Ctrl Pts',(16.6324187832403,-19.2071694893753,-6.29755929335929));
#85825=CARTESIAN_POINT('Ctrl Pts',(16.6299653953218,-19.1862937224656,-6.29880484378213));
#85826=CARTESIAN_POINT('Ctrl Pts',(16.6285777511622,-19.173477608704,-6.29956503076248));
#85827=CARTESIAN_POINT('Ctrl Pts',(16.6203967172938,-19.0908752883665,-6.30443700703756));
#85828=CARTESIAN_POINT('Ctrl Pts',(16.6169563815645,-19.0207966549477,-6.30844166709839));
#85829=CARTESIAN_POINT('Ctrl Pts',(16.6171212273236,-18.7582834317184,-6.3231406527529));
#85830=CARTESIAN_POINT('Ctrl Pts',(16.6434647838365,-18.5668343991246,-6.33317498122216));
#85831=CARTESIAN_POINT('Ctrl Pts',(16.7087052288393,-18.3336573108351,-6.34683370371062));
#85832=CARTESIAN_POINT('Ctrl Pts',(16.7238020870876,-18.2862146758212,-6.34969720243455));
#85833=CARTESIAN_POINT('Ctrl Pts',(16.743184512298,-18.2319974294047,-6.35311511291673));
#85834=CARTESIAN_POINT('Ctrl Pts',(16.7458544887832,-18.2246572818048,-6.35358098216849));
#85835=CARTESIAN_POINT('Ctrl Pts',(16.7501831753964,-18.2129590338692,-6.35432872963475));
#85836=CARTESIAN_POINT('Ctrl Pts',(16.7518158007495,-18.2085912682182,-6.35460909533752));
#85837=CARTESIAN_POINT('Ctrl Pts',(16.754731033288,-18.2008700189836,-6.35510687067238));
#85838=CARTESIAN_POINT('Ctrl Pts',(16.7560077573588,-18.1975143613936,-6.35532392675766));
#85839=CARTESIAN_POINT('Ctrl Pts',(16.7587298593755,-18.1904141665802,-6.35578474685558));
#85840=CARTESIAN_POINT('Ctrl Pts',(16.7601773291144,-18.1866705458515,-6.35602862985684));
#85841=CARTESIAN_POINT('Ctrl Pts',(16.7641078965034,-18.1765901591777,-6.35668774850972));
#85842=CARTESIAN_POINT('Ctrl Pts',(16.7666108958845,-18.1702612771773,-6.35710415327289));
#85843=CARTESIAN_POINT('Ctrl Pts',(16.7791207435806,-18.1390705163343,-6.35916871338343));
#85844=CARTESIAN_POINT('Ctrl Pts',(16.7895680732758,-18.1143893628866,-6.36084134111789));
#85845=CARTESIAN_POINT('Ctrl Pts',(16.8210382304209,-18.0438068432985,-6.36572420168939));
#85846=CARTESIAN_POINT('Ctrl Pts',(16.8432373491214,-17.998452172392,-6.36898504072832));
#85847=CARTESIAN_POINT('Ctrl Pts',(16.9295816986985,-17.8369373174763,-6.38094757349529));
#85848=CARTESIAN_POINT('Ctrl Pts',(17.0029893224962,-17.7260737688442,-6.38981577853393));
#85849=CARTESIAN_POINT('Ctrl Pts',(17.1511163108997,-17.5424515436706,-6.40514170336334));
#85850=CARTESIAN_POINT('Ctrl Pts',(17.2217357934411,-17.4669376859675,-6.41168264531775));
#85851=CARTESIAN_POINT('Ctrl Pts',(17.3079107814179,-17.3873416524933,-6.41884329591353));
#85852=CARTESIAN_POINT('Ctrl Pts',(17.3183213355733,-17.377916095698,-6.4196961042375));
#85853=CARTESIAN_POINT('Ctrl Pts',(17.3350950525198,-17.3630304533005,-6.42105099683033));
#85854=CARTESIAN_POINT('Ctrl Pts',(17.3413980605459,-17.3575034920675,-6.42155588183445));
#85855=CARTESIAN_POINT('Ctrl Pts',(17.3526049401324,-17.3477935828225,-6.42244618259143));
#85856=CARTESIAN_POINT('Ctrl Pts',(17.3574953665302,-17.3435953445102,-6.422832231047));
#85857=CARTESIAN_POINT('Ctrl Pts',(17.3676822004434,-17.3349308400779,-6.4236313332911));
#85858=CARTESIAN_POINT('Ctrl Pts',(17.3729815188126,-17.3304681030036,-6.42404423919218));
#85859=CARTESIAN_POINT('Ctrl Pts',(17.3867089413886,-17.319022476089,-6.42510671568596));
#85860=CARTESIAN_POINT('Ctrl Pts',(17.3951695289611,-17.3120787315126,-6.42575468847182));
#85861=CARTESIAN_POINT('Ctrl Pts',(17.4313068415752,-17.2828863101937,-6.42849389265831));
#85862=CARTESIAN_POINT('Ctrl Pts',(17.4594881367251,-17.2612694767678,-6.43055978551352));
#85863=CARTESIAN_POINT('Ctrl Pts',(17.5349316974395,-17.2063583422862,-6.43592259260299));
#85864=CARTESIAN_POINT('Ctrl Pts',(17.5830376397931,-17.1742722467271,-6.43917557627524));
#85865=CARTESIAN_POINT('Ctrl Pts',(17.7707935587747,-17.0598617589398,-6.45137509240044));
#85866=CARTESIAN_POINT('Ctrl Pts',(17.9184023092571,-16.9917069730889,-6.45992612549223));
#85867=CARTESIAN_POINT('Ctrl Pts',(18.0929231656286,-16.9342836115624,-6.47018705162299));
#85868=CARTESIAN_POINT('Ctrl Pts',(18.1136173423145,-16.927825047436,-6.47140679620249));
#85869=CARTESIAN_POINT('Ctrl Pts',(18.1746816658197,-16.9097914988215,-6.4750244682675));
#85870=CARTESIAN_POINT('Ctrl Pts',(18.21529888653,-16.8990993237991,-6.47745422207117));
#85871=CARTESIAN_POINT('Ctrl Pts',(18.2634492315649,-16.887944214515,-6.48039067514367));
#85872=CARTESIAN_POINT('Ctrl Pts',(18.2707031673798,-16.8863039060714,-6.48083454203317));
#85873=CARTESIAN_POINT('Ctrl Pts',(18.2824592564999,-16.8837105778642,-6.481556517014));
#85874=CARTESIAN_POINT('Ctrl Pts',(18.2869562101733,-16.8827339403016,-6.4818333072944));
#85875=CARTESIAN_POINT('Ctrl Pts',(18.2949512122112,-16.8810248831129,-6.4823265620341));
#85876=CARTESIAN_POINT('Ctrl Pts',(18.2984479674057,-16.8802866512211,-6.48254269046489));
#85877=CARTESIAN_POINT('Ctrl Pts',(18.3059568251153,-16.878721238935,-6.48300766352775));
#85878=CARTESIAN_POINT('Ctrl Pts',(18.3099694042507,-16.8778968603612,-6.4832566586424));
#85879=CARTESIAN_POINT('Ctrl Pts',(18.321020868464,-16.875659763212,-6.48394383287429));
#85880=CARTESIAN_POINT('Ctrl Pts',(18.3280645101896,-16.8742712119483,-6.48438335376392));
#85881=CARTESIAN_POINT('Ctrl Pts',(18.3661873357337,-16.8669571047216,-6.48677007694406));
#85882=CARTESIAN_POINT('Ctrl Pts',(18.3973875683389,-16.8616933590456,-6.48875161386752));
#85883=CARTESIAN_POINT('Ctrl Pts',(18.5904532894668,-16.8335557954143,-6.501138798924));
#85884=CARTESIAN_POINT('Ctrl Pts',(18.7543959575774,-16.8287959773175,-6.51214903693729));
#85885=CARTESIAN_POINT('Ctrl Pts',(19.033862890239,-16.8530783698959,-6.53047401592194));
#85886=CARTESIAN_POINT('Ctrl Pts',(19.1494470394382,-16.8728652348922,-6.53793076193387));
#85887=CARTESIAN_POINT('Ctrl Pts',(19.2766584581424,-16.9056825582303,-6.54595262162781));
#85888=CARTESIAN_POINT('Ctrl Pts',(19.2904615806804,-16.9093928915137,-6.54682078999123));
#85889=CARTESIAN_POINT('Ctrl Pts',(19.3123692531386,-16.9155203165439,-6.54819534458157));
#85890=CARTESIAN_POINT('Ctrl Pts',(19.3204985382494,-16.9178466227992,-6.5487046605073));
#85891=CARTESIAN_POINT('Ctrl Pts',(19.3348107017058,-16.9220351747256,-6.54960010301336));
#85892=CARTESIAN_POINT('Ctrl Pts',(19.3409993653486,-16.9238771084979,-6.54998688601738));
#85893=CARTESIAN_POINT('Ctrl Pts',(19.3537815728068,-16.9277452284498,-6.55078494255546));
#85894=CARTESIAN_POINT('Ctrl Pts',(19.36037384217,-16.9297753859397,-6.55119608086406));
#85895=CARTESIAN_POINT('Ctrl Pts',(19.3772687660389,-16.9350688942401,-6.55224867059282));
#85896=CARTESIAN_POINT('Ctrl Pts',(19.3875566481281,-16.9383790066186,-6.55288858140185));
#85897=CARTESIAN_POINT('Ctrl Pts',(19.4303800315285,-16.9525201443215,-6.5555482941823));
#85898=CARTESIAN_POINT('Ctrl Pts',(19.4626763810054,-16.9640624331487,-6.55754458891593));
#85899=CARTESIAN_POINT('Ctrl Pts',(19.5460741881547,-16.9961734429723,-6.5626860350182));
#85900=CARTESIAN_POINT('Ctrl Pts',(19.5966794607789,-17.0179610136745,-6.56579185022321));
#85901=CARTESIAN_POINT('Ctrl Pts',(19.7450262601731,-17.0888130303627,-6.5749332184549));
#85902=CARTESIAN_POINT('Ctrl Pts',(19.8398772852943,-17.1434989358135,-6.58082003201506));
#85903=CARTESIAN_POINT('Ctrl Pts',(19.9655506949163,-17.2295540709509,-6.58911246717644));
#85904=CARTESIAN_POINT('Ctrl Pts',(20.0002722973563,-17.2549168048054,-6.59146243015674));
#85905=CARTESIAN_POINT('Ctrl Pts',(20.0938164011725,-17.3277168677431,-6.59802434544196));
#85906=CARTESIAN_POINT('Ctrl Pts',(20.1509032086612,-17.3772685741599,-6.60229309621258));
#85907=CARTESIAN_POINT('Ctrl Pts',(20.2120398064826,-17.4363557617218,-6.60733214526215));
#85908=CARTESIAN_POINT('Ctrl Pts',(20.2188215667602,-17.4429989947439,-6.60789802427315));
#85909=CARTESIAN_POINT('Ctrl Pts',(20.2288085650317,-17.4529145014359,-6.6087420805178));
#85910=CARTESIAN_POINT('Ctrl Pts',(20.2320483415413,-17.4561520319236,-6.60901758768075));
#85911=CARTESIAN_POINT('Ctrl Pts',(20.2377958635765,-17.461932968475,-6.60950943563549));
#85912=CARTESIAN_POINT('Ctrl Pts',(20.2403077037108,-17.4644722324413,-6.60972544767004));
#85913=CARTESIAN_POINT('Ctrl Pts',(20.2456965333109,-17.4699475420651,-6.61019117452609));
#85914=CARTESIAN_POINT('Ctrl Pts',(20.2485713590113,-17.4728855707912,-6.61044104511615));
#85915=CARTESIAN_POINT('Ctrl Pts',(20.2564885156772,-17.4810240688811,-6.61113305068991));
#85916=CARTESIAN_POINT('Ctrl Pts',(20.2615126845736,-17.4862420168139,-6.61157655820772));
#85917=CARTESIAN_POINT('Ctrl Pts',(20.2889780146913,-17.5150612389209,-6.61402464833719));
#85918=CARTESIAN_POINT('Ctrl Pts',(20.3108977326246,-17.5391507864432,-6.61606564154915));
#85919=CARTESIAN_POINT('Ctrl Pts',(20.4389307853874,-17.6865498752673,-6.62847231391311));
#85920=CARTESIAN_POINT('Ctrl Pts',(20.5310957263475,-17.8212480883874,-6.63942740376185));
#85921=CARTESIAN_POINT('Ctrl Pts',(20.6613734837904,-18.0685052257101,-6.65768271117041));
#85922=CARTESIAN_POINT('Ctrl Pts',(20.7071815180421,-18.1761816814899,-6.66512286935745));
#85923=CARTESIAN_POINT('Ctrl Pts',(20.7483642117033,-18.3006705870517,-6.67312929184691));
#85924=CARTESIAN_POINT('Ctrl Pts',(20.7527147041259,-18.3142820838135,-6.67399725963603));
#85925=CARTESIAN_POINT('Ctrl Pts',(20.7594193991405,-18.3360156367872,-6.67537155768294));
#85926=CARTESIAN_POINT('Ctrl Pts',(20.761863274625,-18.3441093677281,-6.67588081593857));
#85927=CARTESIAN_POINT('Ctrl Pts',(20.7660879237178,-18.3584097714617,-6.67677619136306));
#85928=CARTESIAN_POINT('Ctrl Pts',(20.7678888984241,-18.3646103172207,-6.67716296464597));
#85929=CARTESIAN_POINT('Ctrl Pts',(20.7715552243087,-18.3774520983253,-6.67796103397983));
#85930=CARTESIAN_POINT('Ctrl Pts',(20.7734165414381,-18.3840944130696,-6.67837219464344));
#85931=CARTESIAN_POINT('Ctrl Pts',(20.7781109607767,-18.401167712871,-6.67942490960676));
#85932=CARTESIAN_POINT('Ctrl Pts',(20.7808967256453,-18.411611593747,-6.68006492257538));
#85933=CARTESIAN_POINT('Ctrl Pts',(20.792189773325,-18.4552900830122,-6.68272562812138));
#85934=CARTESIAN_POINT('Ctrl Pts',(20.799968855721,-18.4887087649703,-6.68472279105532));
#85935=CARTESIAN_POINT('Ctrl Pts',(20.8181178077119,-18.5762624915677,-6.68986697858525));
#85936=CARTESIAN_POINT('Ctrl Pts',(20.8271923810118,-18.6306403678502,-6.69297461198297));
#85937=CARTESIAN_POINT('Ctrl Pts',(20.8479099951558,-18.7937899655436,-6.70211915236943));
#85938=CARTESIAN_POINT('Ctrl Pts',(20.8532599530273,-18.9031735973118,-6.7080073304072));
#85939=CARTESIAN_POINT('Ctrl Pts',(20.8488261989703,-19.0583049349306,-6.71645678498698));
#85940=CARTESIAN_POINT('Ctrl Pts',(20.8460284135255,-19.1040734431599,-6.7189634204485));
#85941=CARTESIAN_POINT('Ctrl Pts',(20.8396437483876,-19.1721378598308,-6.72275446854813));
#85942=CARTESIAN_POINT('Ctrl Pts',(20.8371826061535,-19.1945265915747,-6.7240117960614));
#85943=CARTESIAN_POINT('Ctrl Pts',(20.8336953902407,-19.2221793715007,-6.72558200638612));
#85944=CARTESIAN_POINT('Ctrl Pts',(20.8330058781557,-19.2274849310746,-6.7258840615606));
#85945=CARTESIAN_POINT('Ctrl Pts',(20.8261524201063,-19.2787000705403,-6.72880793340792));
#85946=CARTESIAN_POINT('Ctrl Pts',(20.8185038207325,-19.3243947000182,-6.73147945934883));
#85947=CARTESIAN_POINT('Ctrl Pts',(20.8078531538595,-19.3773006817515,-6.73468418036458));
#85948=CARTESIAN_POINT('Ctrl Pts',(20.8063020886773,-19.3847951281276,-6.73514078170952));
#85949=CARTESIAN_POINT('Ctrl Pts',(20.8037502742127,-19.3967967144346,-6.73587644755099));
#85950=CARTESIAN_POINT('Ctrl Pts',(20.8027753421833,-19.4013093560399,-6.73615407551326));
#85951=CARTESIAN_POINT('Ctrl Pts',(20.8010173005514,-19.4093197203138,-6.73664875337252));
#85952=CARTESIAN_POINT('Ctrl Pts',(20.8002400606021,-19.4128186835999,-6.73686546489816));
#85953=CARTESIAN_POINT('Ctrl Pts',(20.7985678437899,-19.4202573437952,-6.73732755458454));
#85954=CARTESIAN_POINT('Ctrl Pts',(20.7976704883132,-19.4241963962834,-6.73757306186803));
#85955=CARTESIAN_POINT('Ctrl Pts',(20.7952045667922,-19.434879568505,-6.73824106936624));
#85956=CARTESIAN_POINT('Ctrl Pts',(20.7936141955909,-19.4416185312106,-6.73866479230366));
#85957=CARTESIAN_POINT('Ctrl Pts',(20.7853698201212,-19.4758018039151,-6.74082560372004));
#85958=CARTESIAN_POINT('Ctrl Pts',(20.7782005526269,-19.5031174002884,-6.74258992917926));
#85959=CARTESIAN_POINT('Ctrl Pts',(20.7555787912444,-19.5827828712908,-6.74783025951389));
#85960=CARTESIAN_POINT('Ctrl Pts',(20.7386462105632,-19.6346863091383,-6.751365347766));
#85961=CARTESIAN_POINT('Ctrl Pts',(20.671155970708,-19.8173026057757,-6.76411145275841));
#85962=CARTESIAN_POINT('Ctrl Pts',(20.6096497610116,-19.9435970764842,-6.77347616543825));
#85963=CARTESIAN_POINT('Ctrl Pts',(20.4885706906434,-20.1400150092137,-6.7883760665901));
#85964=CARTESIAN_POINT('Ctrl Pts',(20.4361200889915,-20.2140178041928,-6.79408742514634));
#85965=CARTESIAN_POINT('Ctrl Pts',(20.3704386939896,-20.2951105509674,-6.80045471507318));
#85966=CARTESIAN_POINT('Ctrl Pts',(20.3616923828878,-20.3056968168467,-6.80128835463687));
#85967=CARTESIAN_POINT('Ctrl Pts',(20.3475003789504,-20.3225379522307,-6.80261866491772));
#85968=CARTESIAN_POINT('Ctrl Pts',(20.3421199696312,-20.328847093074,-6.80311797911128));
#85969=CARTESIAN_POINT('Ctrl Pts',(20.3325008427541,-20.3399933051705,-6.804001853058));
#85970=CARTESIAN_POINT('Ctrl Pts',(20.328276914794,-20.3448429487397,-6.8043870158259));
#85971=CARTESIAN_POINT('Ctrl Pts',(20.3194300644443,-20.3549073646952,-6.80518762348243));
#85972=CARTESIAN_POINT('Ctrl Pts',(20.3148033545621,-20.3601187162842,-6.80560290389716));
#85973=CARTESIAN_POINT('Ctrl Pts',(20.3027209612745,-20.3735932645148,-6.80667862059588));
#85974=CARTESIAN_POINT('Ctrl Pts',(20.2952256381819,-20.3818207502664,-6.80733738131728));
#85975=CARTESIAN_POINT('Ctrl Pts',(20.2623925116868,-20.4172950871922,-6.81018673204135));
#85976=CARTESIAN_POINT('Ctrl Pts',(20.2364028401232,-20.4439314049518,-6.81234932037613));
#85977=CARTESIAN_POINT('Ctrl Pts',(20.1654924194756,-20.5128728535719,-6.81802520626901));
#85978=CARTESIAN_POINT('Ctrl Pts',(20.1194009337238,-20.5539237560652,-6.82148754409593));
#85979=CARTESIAN_POINT('Ctrl Pts',(19.9574244261251,-20.6859584487774,-6.83304903405252));
#85980=CARTESIAN_POINT('Ctrl Pts',(19.833878030955,-20.7668400265856,-6.84085978024349));
#85981=CARTESIAN_POINT('Ctrl Pts',(19.6401114313903,-20.8665874515746,-6.85296096597903));
#85982=CARTESIAN_POINT('Ctrl Pts',(19.5757058648517,-20.8957623601569,-6.85696745378742));
#85983=CARTESIAN_POINT('Ctrl Pts',(19.5012534312635,-20.9250937493032,-6.86171120454358));
#85984=CARTESIAN_POINT('Ctrl Pts',(19.4925143219775,-20.9284697790188,-6.86226973542677));
#85985=CARTESIAN_POINT('Ctrl Pts',(19.4794929660384,-20.9334010171762,-6.86310490313351));
#85986=CARTESIAN_POINT('Ctrl Pts',(19.4752275058808,-20.9350006396658,-6.86337895091229));
#85987=CARTESIAN_POINT('Ctrl Pts',(19.4676106768614,-20.9378290753481,-6.86386920826725));
#85988=CARTESIAN_POINT('Ctrl Pts',(19.4642613321553,-20.9390631918023,-6.86408509736251));
#85989=CARTESIAN_POINT('Ctrl Pts',(19.4570325280633,-20.9417060077999,-6.86455172454537));
#85990=CARTESIAN_POINT('Ctrl Pts',(19.4531521212957,-20.9431118150111,-6.86480262458211));
#85991=CARTESIAN_POINT('Ctrl Pts',(19.4423785923912,-20.9469792843731,-6.86550032297558));
#85992=CARTESIAN_POINT('Ctrl Pts',(19.4354768536649,-20.9494165302727,-6.8659485305063));
#85993=CARTESIAN_POINT('Ctrl Pts',(19.3967263510014,-20.9628750832011,-6.86847146220071));
#85994=CARTESIAN_POINT('Ctrl Pts',(19.3646324932815,-20.9731697548409,-6.87058521452178));
#85995=CARTESIAN_POINT('Ctrl Pts',(19.2634050235159,-21.0029946847435,-6.87729822382512));
#85996=CARTESIAN_POINT('Ctrl Pts',(19.193517172832,-21.019774507139,-6.88199781431464));
#85997=CARTESIAN_POINT('Ctrl Pts',(19.0984184415285,-21.0375477351631,-6.88837432458532));
#85998=CARTESIAN_POINT('Ctrl Pts',(19.0738408090841,-21.0416933667544,-6.89002084513981));
#85999=CARTESIAN_POINT('Ctrl Pts',(18.8813730648572,-21.070672500803,-6.90288308672149));
#86000=CARTESIAN_POINT('Ctrl Pts',(18.7110874713322,-21.0756733060515,-6.91400215221685));
#86001=CARTESIAN_POINT('Ctrl Pts',(18.5187396621086,-21.0581571597103,-6.92589487591079));
#86002=CARTESIAN_POINT('Ctrl Pts',(18.4955054126994,-21.0556528694072,-6.92732166519893));
#86003=CARTESIAN_POINT('Ctrl Pts',(18.4627821770708,-21.0515766737402,-6.92931807621384));
#86004=CARTESIAN_POINT('Ctrl Pts',(18.4532557976113,-21.0503240965053,-6.92989770396659));
#86005=CARTESIAN_POINT('Ctrl Pts',(18.4378165229655,-21.0481870349397,-6.93083463906088));
#86006=CARTESIAN_POINT('Ctrl Pts',(18.4318983464809,-21.0473422941367,-6.93119319731217));
#86007=CARTESIAN_POINT('Ctrl Pts',(18.419538173269,-21.0455245887953,-6.93194085185123));
#86008=CARTESIAN_POINT('Ctrl Pts',(18.4130969217915,-21.0445469314263,-6.93232979539597));
#86009=CARTESIAN_POINT('Ctrl Pts',(18.3978212427824,-21.0421561866463,-6.93325062082878));
#86010=CARTESIAN_POINT('Ctrl Pts',(18.3889910124291,-21.0407167935406,-6.93378166330591));
#86011=CARTESIAN_POINT('Ctrl Pts',(18.3594461566719,-21.0357082908153,-6.93555447949112));
#86012=CARTESIAN_POINT('Ctrl Pts',(18.3387751956277,-21.0318865891334,-6.93678823401119));
#86013=CARTESIAN_POINT('Ctrl Pts',(18.2276664622002,-21.0096282047749,-6.94338915930166));
#86014=CARTESIAN_POINT('Ctrl Pts',(18.1384457872673,-20.985599151113,-6.94857382998983));
#86015=CARTESIAN_POINT('Ctrl Pts',(17.9186476997537,-20.910688874738,-6.96136637431337));
#86016=CARTESIAN_POINT('Ctrl Pts',(17.7910330296627,-20.8525450690877,-6.96880102409604));
#86017=CARTESIAN_POINT('Ctrl Pts',(17.6108382003692,-20.7477989591045,-6.98039040851198));
#86018=CARTESIAN_POINT('Ctrl Pts',(17.5532984805687,-20.7105017086431,-6.98428168865104));
#86019=CARTESIAN_POINT('Ctrl Pts',(17.490106209662,-20.6650394551776,-6.98889687856186));
#86020=CARTESIAN_POINT('Ctrl Pts',(17.4825736368637,-20.6595444319488,-6.98945278129145));
#86021=CARTESIAN_POINT('Ctrl Pts',(17.4714223380889,-20.6512961249973,-6.99028476773022));
#86022=CARTESIAN_POINT('Ctrl Pts',(17.4677756695544,-20.6485805659885,-6.99055829108771));
#86023=CARTESIAN_POINT('Ctrl Pts',(17.4614195361621,-20.6438154464929,-6.99103763440959));
#86024=CARTESIAN_POINT('Ctrl Pts',(17.4587062239407,-20.6417710870099,-6.9912430892678));
#86025=CARTESIAN_POINT('Ctrl Pts',(17.452819062595,-20.6373131174907,-6.99169069856052));
#86026=CARTESIAN_POINT('Ctrl Pts',(17.4496471545203,-20.634897105012,-6.9919330186152));
#86027=CARTESIAN_POINT('Ctrl Pts',(17.4411877201961,-20.6284157879533,-6.99258233414978));
#86028=CARTESIAN_POINT('Ctrl Pts',(17.4359125995587,-20.6243344710283,-6.992990434723));
#86029=CARTESIAN_POINT('Ctrl Pts',(17.4241749041285,-20.6151641174227,-6.99390550907587));
#86030=CARTESIAN_POINT('Ctrl Pts',(17.417722560256,-20.6100622304418,-6.99441332646983));
#86031=CARTESIAN_POINT('Ctrl Pts',(17.3981791753551,-20.594423249501,-6.99596566560015));
#86032=CARTESIAN_POINT('Ctrl Pts',(17.3851840346272,-20.5837680166732,-6.99701746916403));
#86033=CARTESIAN_POINT('Ctrl Pts',(17.3368453813657,-20.5431612695802,-7.00099987075799));
#86034=CARTESIAN_POINT('Ctrl Pts',(17.3023630944086,-20.5122084572404,-7.00398343556874));
#86035=CARTESIAN_POINT('Ctrl Pts',(17.2194705806093,-20.4327375201702,-7.01146386641024));
#86036=CARTESIAN_POINT('Ctrl Pts',(17.1723471433782,-20.3829517215942,-7.01599584036224));
#86037=CARTESIAN_POINT('Ctrl Pts',(17.0230827516861,-20.2090827754921,-7.03113752218766));
#86038=CARTESIAN_POINT('Ctrl Pts',(16.9326383657498,-20.0756589440136,-7.04162667761467));
#86039=CARTESIAN_POINT('Ctrl Pts',(16.8471281735806,-19.9121923280529,-7.05299063890773));
#86040=CARTESIAN_POINT('Ctrl Pts',(16.836460239165,-19.8909342493639,-7.05444320153705));
#86041=CARTESIAN_POINT('Ctrl Pts',(16.8219582091015,-19.8607787657603,-7.05646922583326));
#86042=CARTESIAN_POINT('Ctrl Pts',(16.8178237869933,-19.852028544443,-7.05705309541346));
#86043=CARTESIAN_POINT('Ctrl Pts',(16.8112273404217,-19.8378161149772,-7.05799503237767));
#86044=CARTESIAN_POINT('Ctrl Pts',(16.8087282806853,-19.8323713409289,-7.05835437694544));
#86045=CARTESIAN_POINT('Ctrl Pts',(16.8035640625956,-19.8209927520846,-7.05910222649855));
#86046=CARTESIAN_POINT('Ctrl Pts',(16.8009030694787,-19.8150571071859,-7.0594905850705));
#86047=CARTESIAN_POINT('Ctrl Pts',(16.7946705099276,-19.8009812399099,-7.0604074415907));
#86048=CARTESIAN_POINT('Ctrl Pts',(16.7911227548355,-19.7928305600283,-7.06093511992045));
#86049=CARTESIAN_POINT('Ctrl Pts',(16.7794904341133,-19.7656395036212,-7.06268495435289));
#86050=CARTESIAN_POINT('Ctrl Pts',(16.7716334439858,-19.7465026303007,-7.06389937726305));
#86051=CARTESIAN_POINT('Ctrl Pts',(16.7576410919479,-19.7109476353391,-7.066125921824));
#86052=CARTESIAN_POINT('Ctrl Pts',(16.7514278355577,-19.6945654719617,-7.06714032154971));
#86053=CARTESIAN_POINT('Ctrl Pts',(16.7454194581678,-19.6781104796424,-7.06814844662885));
#86054=CARTESIAN_POINT('Ctrl Pts',(16.7454194485728,-19.6781104533646,-6.84500598787601));
#86055=CARTESIAN_POINT('Ctrl Pts',(16.7536780380464,-19.7007280459546,-6.84341661262277));
#86056=CARTESIAN_POINT('Ctrl Pts',(16.7623223866146,-19.7232044385535,-6.841824850225));
#86057=CARTESIAN_POINT('Ctrl Pts',(16.7857100470872,-19.7810495514162,-6.8377020043978));
#86058=CARTESIAN_POINT('Ctrl Pts',(16.8010330336016,-19.8161734120292,-6.83517284233548));
#86059=CARTESIAN_POINT('Ctrl Pts',(16.8576523309627,-19.936906172792,-6.82641396455609));
#86060=CARTESIAN_POINT('Ctrl Pts',(16.9037554382877,-20.0201428847521,-6.82026484169948));
#86061=CARTESIAN_POINT('Ctrl Pts',(16.9803711804393,-20.1388496765648,-6.8113990453225));
#86062=CARTESIAN_POINT('Ctrl Pts',(17.006707645613,-20.1768623756601,-6.8085426759325));
#86063=CARTESIAN_POINT('Ctrl Pts',(17.0414157734736,-20.2236097468993,-6.80500496816375));
#86064=CARTESIAN_POINT('Ctrl Pts',(17.0486437955743,-20.2331741434187,-6.80427976861819));
#86065=CARTESIAN_POINT('Ctrl Pts',(17.0603174042016,-20.2483513486212,-6.80312660074575));
#86066=CARTESIAN_POINT('Ctrl Pts',(17.0647108159088,-20.2540037912338,-6.80269658935759));
#86067=CARTESIAN_POINT('Ctrl Pts',(17.073076928698,-20.2646554471408,-6.80188519529132));
#86068=CARTESIAN_POINT('Ctrl Pts',(17.0770437308944,-20.2696591726785,-6.8015035845218));
#86069=CARTESIAN_POINT('Ctrl Pts',(17.0860738390126,-20.2809444913788,-6.80064184084566));
#86070=CARTESIAN_POINT('Ctrl Pts',(17.0911505562668,-20.2872152639977,-6.80016225264278));
#86071=CARTESIAN_POINT('Ctrl Pts',(17.1062386150198,-20.3056357371196,-6.79875109607873));
#86072=CARTESIAN_POINT('Ctrl Pts',(17.1163499098169,-20.3177031306008,-6.7978235817372));
#86073=CARTESIAN_POINT('Ctrl Pts',(17.2076554603322,-20.4242354574733,-6.78960463271056));
#86074=CARTESIAN_POINT('Ctrl Pts',(17.2969092350462,-20.5114810165515,-6.78267609119741));
#86075=CARTESIAN_POINT('Ctrl Pts',(17.5230065109461,-20.6964942362747,-6.76672052178679));
#86076=CARTESIAN_POINT('Ctrl Pts',(17.6648044211286,-20.786821714059,-6.75786060465836));
#86077=CARTESIAN_POINT('Ctrl Pts',(17.8351458866485,-20.8688239784094,-6.74686255675113));
#86078=CARTESIAN_POINT('Ctrl Pts',(17.8546927905106,-20.8778690587652,-6.74559503727467));
#86079=CARTESIAN_POINT('Ctrl Pts',(17.8801233784215,-20.8891688890996,-6.74393467957359));
#86080=CARTESIAN_POINT('Ctrl Pts',(17.8858846193461,-20.8916981436783,-6.74355778715657));
#86081=CARTESIAN_POINT('Ctrl Pts',(17.894742296601,-20.8955397647392,-6.74297706638763));
#86082=CARTESIAN_POINT('Ctrl Pts',(17.8978307860735,-20.8968705240081,-6.74277434619168));
#86083=CARTESIAN_POINT('Ctrl Pts',(17.9042045628944,-20.8995988495985,-6.74235547880888));
#86084=CARTESIAN_POINT('Ctrl Pts',(17.9074901901533,-20.9009954540692,-6.74213927397251));
#86085=CARTESIAN_POINT('Ctrl Pts',(17.9149829906281,-20.9041580256838,-6.74164558926162));
#86086=CARTESIAN_POINT('Ctrl Pts',(17.9191923337179,-20.9059186996775,-6.74136779393161));
#86087=CARTESIAN_POINT('Ctrl Pts',(17.9301582013881,-20.9104638794813,-6.74064299419499));
#86088=CARTESIAN_POINT('Ctrl Pts',(17.936923444624,-20.9132270051557,-6.74019474783167));
#86089=CARTESIAN_POINT('Ctrl Pts',(17.9802287930293,-20.9306531162098,-6.73731912937884));
#86090=CARTESIAN_POINT('Ctrl Pts',(18.0171551799489,-20.9443283453943,-6.7348385062367));
#86091=CARTESIAN_POINT('Ctrl Pts',(18.2352222370377,-21.0182398469808,-6.72011010559865));
#86092=CARTESIAN_POINT('Ctrl Pts',(18.423466191539,-21.0547853843035,-6.70717970967866));
#86093=CARTESIAN_POINT('Ctrl Pts',(18.6690805391439,-21.068721482032,-6.69136694511972));
#86094=CARTESIAN_POINT('Ctrl Pts',(18.7241904573857,-21.0696942561511,-6.6878781972971));
#86095=CARTESIAN_POINT('Ctrl Pts',(18.8135720992245,-21.0677820782871,-6.68232117486196));
#86096=CARTESIAN_POINT('Ctrl Pts',(18.847843278002,-21.0662150898382,-6.6802144709364));
#86097=CARTESIAN_POINT('Ctrl Pts',(18.8928445504151,-21.063059976504,-6.67747811850878));
#86098=CARTESIAN_POINT('Ctrl Pts',(18.9036204154534,-21.0622214900432,-6.67682513244238));
#86099=CARTESIAN_POINT('Ctrl Pts',(18.921262400303,-21.0607127293788,-6.67575965511964));
#86100=CARTESIAN_POINT('Ctrl Pts',(18.9281324035724,-21.0600913626422,-6.67534563454353));
#86101=CARTESIAN_POINT('Ctrl Pts',(18.9414269063701,-21.0588233832749,-6.67454612194857));
#86102=CARTESIAN_POINT('Ctrl Pts',(18.9478517176283,-21.0581809357444,-6.67416050361428));
#86103=CARTESIAN_POINT('Ctrl Pts',(18.962682446802,-21.0566293787908,-6.6732720724199));
#86104=CARTESIAN_POINT('Ctrl Pts',(18.9710860947131,-21.0556992823124,-6.67276992567742));
#86105=CARTESIAN_POINT('Ctrl Pts',(18.9936779611847,-21.0530617720149,-6.67142327440938));
#86106=CARTESIAN_POINT('Ctrl Pts',(19.0078549910934,-21.0512609823728,-6.67058171157713));
#86107=CARTESIAN_POINT('Ctrl Pts',(19.1378034867022,-21.0334158707581,-6.66289745615126));
#86108=CARTESIAN_POINT('Ctrl Pts',(19.2520854550784,-21.0079528232304,-6.65637168629916));
#86109=CARTESIAN_POINT('Ctrl Pts',(19.5192312097798,-20.924724214512,-6.64105381461462));
#86110=CARTESIAN_POINT('Ctrl Pts',(19.6686357511708,-20.858481829157,-6.63244527751377));
#86111=CARTESIAN_POINT('Ctrl Pts',(19.83678700674,-20.7593720929295,-6.62123557181563));
#86112=CARTESIAN_POINT('Ctrl Pts',(19.8642425563889,-20.7423308552909,-6.61935069636158));
#86113=CARTESIAN_POINT('Ctrl Pts',(19.8973464684706,-20.7207188050917,-6.61699672473154));
#86114=CARTESIAN_POINT('Ctrl Pts',(19.9033769143353,-20.7167376139198,-6.6165645336402));
#86115=CARTESIAN_POINT('Ctrl Pts',(19.9128023656273,-20.7104455772289,-6.61588352173284));
#86116=CARTESIAN_POINT('Ctrl Pts',(19.9162112955816,-20.7081555504069,-6.61563608014102));
#86117=CARTESIAN_POINT('Ctrl Pts',(19.9225730850745,-20.7038549549787,-6.61517212623207));
#86118=CARTESIAN_POINT('Ctrl Pts',(19.9255275261901,-20.7018468263021,-6.61495577818221));
#86119=CARTESIAN_POINT('Ctrl Pts',(19.9322631359734,-20.6972436759095,-6.61446052475571));
#86120=CARTESIAN_POINT('Ctrl Pts',(19.936040951097,-20.6946438483829,-6.61418129597108));
#86121=CARTESIAN_POINT('Ctrl Pts',(19.9476376019537,-20.6866075811814,-6.61331974459068));
#86122=CARTESIAN_POINT('Ctrl Pts',(19.9554280999317,-20.6811307291466,-6.61273476808163));
#86123=CARTESIAN_POINT('Ctrl Pts',(20.059666091297,-20.6067937251717,-6.60482693076226));
#86124=CARTESIAN_POINT('Ctrl Pts',(20.1501920635098,-20.5300134226837,-6.59703559225824));
#86125=CARTESIAN_POINT('Ctrl Pts',(20.3109865785519,-20.3686018886004,-6.5819853909188));
#86126=CARTESIAN_POINT('Ctrl Pts',(20.3820512515836,-20.2852584589575,-6.57475458099747));
#86127=CARTESIAN_POINT('Ctrl Pts',(20.4787413927651,-20.1522495563294,-6.5641851107618));
#86128=CARTESIAN_POINT('Ctrl Pts',(20.5093731491009,-20.1064576762435,-6.56069805937811));
#86129=CARTESIAN_POINT('Ctrl Pts',(20.5561247201943,-20.0302978367596,-6.55514342264989));
#86130=CARTESIAN_POINT('Ctrl Pts',(20.5733512388232,-20.0006429120504,-6.55303744911663));
#86131=CARTESIAN_POINT('Ctrl Pts',(20.5950502021521,-19.9611074926157,-6.55030189220939));
#86132=CARTESIAN_POINT('Ctrl Pts',(20.6001772741398,-19.9515940050091,-6.54964898823839));
#86133=CARTESIAN_POINT('Ctrl Pts',(20.6084571200258,-19.9359446543029,-6.5485836105344));
#86134=CARTESIAN_POINT('Ctrl Pts',(20.6116531038736,-19.9298319900741,-6.54816960803367));
#86135=CARTESIAN_POINT('Ctrl Pts',(20.6177828965845,-19.9179672302272,-6.54737010662314));
#86136=CARTESIAN_POINT('Ctrl Pts',(20.6207203728542,-19.9122171251438,-6.54698448152206));
#86137=CARTESIAN_POINT('Ctrl Pts',(20.6274437087045,-19.8989062349463,-6.54609600083667));
#86138=CARTESIAN_POINT('Ctrl Pts',(20.6312106859756,-19.8913359952631,-6.54559381160812));
#86139=CARTESIAN_POINT('Ctrl Pts',(20.6412228700802,-19.8709092494572,-6.54424697115701));
#86140=CARTESIAN_POINT('Ctrl Pts',(20.6473834685256,-19.8580115905372,-6.54340526293642));
#86141=CARTESIAN_POINT('Ctrl Pts',(20.702798841186,-19.7389088314875,-6.53570959171701));
#86142=CARTESIAN_POINT('Ctrl Pts',(20.7432983510267,-19.6288454834824,-6.5291736803899));
#86143=CARTESIAN_POINT('Ctrl Pts',(20.8180594019977,-19.3583604642705,-6.51381210631146));
#86144=CARTESIAN_POINT('Ctrl Pts',(20.8432101515545,-19.1962391289494,-6.5051718396048));
#86145=CARTESIAN_POINT('Ctrl Pts',(20.8506615694375,-19.001299386526,-6.4939590367058));
#86146=CARTESIAN_POINT('Ctrl Pts',(20.8511614324631,-18.9697160099649,-6.49211550114772));
#86147=CARTESIAN_POINT('Ctrl Pts',(20.8509076035842,-18.930959910016,-6.48980754471176));
#86148=CARTESIAN_POINT('Ctrl Pts',(20.8508241299618,-18.9237849870449,-6.48937834739955));
#86149=CARTESIAN_POINT('Ctrl Pts',(20.8506357189086,-18.912515734333,-6.48870101438323));
#86150=CARTESIAN_POINT('Ctrl Pts',(20.8505553716861,-18.908420971466,-6.48845423338577));
#86151=CARTESIAN_POINT('Ctrl Pts',(20.850382658026,-18.9007533541636,-6.48799083316416));
#86152=CARTESIAN_POINT('Ctrl Pts',(20.8502931259038,-18.8971804917463,-6.4877743740464));
#86153=CARTESIAN_POINT('Ctrl Pts',(20.8500675816192,-18.889006518436,-6.48727795831878));
#86154=CARTESIAN_POINT('Ctrl Pts',(20.8499256103671,-18.8844056276888,-6.4869976724417));
#86155=CARTESIAN_POINT('Ctrl Pts',(20.8495148649811,-18.8723681505808,-6.48626214392911));
#86156=CARTESIAN_POINT('Ctrl Pts',(20.8492218860273,-18.8649325288807,-6.48580559954916));
#86157=CARTESIAN_POINT('Ctrl Pts',(20.8470114327017,-18.8154637210862,-6.48275425591465));
#86158=CARTESIAN_POINT('Ctrl Pts',(20.843880486483,-18.7734971799336,-6.48009862150874));
#86159=CARTESIAN_POINT('Ctrl Pts',(20.8387360564558,-18.7243396469215,-6.4769301205581));
#86160=CARTESIAN_POINT('Ctrl Pts',(20.8379323540438,-18.7170281909219,-6.47645733971364));
#86161=CARTESIAN_POINT('Ctrl Pts',(20.836257315014,-18.7024880906132,-6.47551429942186));
#86162=CARTESIAN_POINT('Ctrl Pts',(20.8353867557889,-18.6952594460115,-6.47504406866501));
#86163=CARTESIAN_POINT('Ctrl Pts',(20.8135700365253,-18.521654434538,-6.46371936701003));
#86164=CARTESIAN_POINT('Ctrl Pts',(20.772967309756,-18.3583428964865,-6.45243220453915));
#86165=CARTESIAN_POINT('Ctrl Pts',(20.6927190443868,-18.1466743416921,-6.4378410200488));
#86166=CARTESIAN_POINT('Ctrl Pts',(20.669653004821,-18.0927106810954,-6.43411766848078));
#86167=CARTESIAN_POINT('Ctrl Pts',(20.6289083289105,-18.0073839390058,-6.42823248200722));
#86168=CARTESIAN_POINT('Ctrl Pts',(20.6126214110876,-17.9753941844382,-6.4260263188917));
#86169=CARTESIAN_POINT('Ctrl Pts',(20.5902959339706,-17.9341713713622,-6.42318193770447));
#86170=CARTESIAN_POINT('Ctrl Pts',(20.5849885013125,-17.9245510782099,-6.42251801616075));
#86171=CARTESIAN_POINT('Ctrl Pts',(20.5762080643467,-17.9089244642064,-6.42143926542278));
#86172=CARTESIAN_POINT('Ctrl Pts',(20.5727800545382,-17.9028932187188,-6.4210228327517));
#86173=CARTESIAN_POINT('Ctrl Pts',(20.5661117969379,-17.8912941686638,-6.42022177229258));
#86174=CARTESIAN_POINT('Ctrl Pts',(20.5628756651789,-17.8857240976922,-6.41983700183805));
#86175=CARTESIAN_POINT('Ctrl Pts',(20.5553807169491,-17.8729582033306,-6.41895491142425));
#86176=CARTESIAN_POINT('Ctrl Pts',(20.5511045742551,-17.8657726369144,-6.41845822704092));
#86177=CARTESIAN_POINT('Ctrl Pts',(20.5395707938467,-17.8466501619912,-6.41713582273701));
#86178=CARTESIAN_POINT('Ctrl Pts',(20.5322373087074,-17.8347593135334,-6.41631287917404));
#86179=CARTESIAN_POINT('Ctrl Pts',(20.4714672711647,-17.7383726474511,-6.40963480348134));
#86180=CARTESIAN_POINT('Ctrl Pts',(20.4122211229211,-17.6576810987769,-6.40400641677406));
#86181=CARTESIAN_POINT('Ctrl Pts',(20.2361676815161,-17.4504181774575,-6.38902092584685));
#86182=CARTESIAN_POINT('Ctrl Pts',(20.1093107176857,-17.333431345525,-6.3799835453606));
#86183=CARTESIAN_POINT('Ctrl Pts',(19.9372894117595,-17.2097660651834,-6.36791346258814));
#86184=CARTESIAN_POINT('Ctrl Pts',(19.9042057592057,-17.1873746832272,-6.36559693712837));
#86185=CARTESIAN_POINT('Ctrl Pts',(19.8640243073331,-17.161806384331,-6.3627640027438));
#86186=CARTESIAN_POINT('Ctrl Pts',(19.8575151603805,-17.1577141261671,-6.36230449109463));
#86187=CARTESIAN_POINT('Ctrl Pts',(19.8474097087719,-17.1514374422352,-6.36158994975569));
#86188=CARTESIAN_POINT('Ctrl Pts',(19.8438288633841,-17.1492280795106,-6.36133653180358));
#86189=CARTESIAN_POINT('Ctrl Pts',(19.8372045956612,-17.1451681574711,-6.36086727512391));
#86190=CARTESIAN_POINT('Ctrl Pts',(19.8341630800822,-17.1433145979101,-6.3606516373507));
#86191=CARTESIAN_POINT('Ctrl Pts',(19.8273127401953,-17.139163538103,-6.36016556006592));
#86192=CARTESIAN_POINT('Ctrl Pts',(19.8235013693966,-17.1368703763357,-6.35989484456079));
#86193=CARTESIAN_POINT('Ctrl Pts',(19.8137318520794,-17.1310342727399,-6.35920029081883));
#86194=CARTESIAN_POINT('Ctrl Pts',(19.8077635324534,-17.1275085844041,-6.35877537223765));
#86195=CARTESIAN_POINT('Ctrl Pts',(19.7728196821254,-17.1070969160525,-6.35628447796757));
#86196=CARTESIAN_POINT('Ctrl Pts',(19.7434652212802,-17.0908730841479,-6.35417989372362));
#86197=CARTESIAN_POINT('Ctrl Pts',(19.6975171370094,-17.0668849815665,-6.35088133063223));
#86198=CARTESIAN_POINT('Ctrl Pts',(19.6811857390117,-17.058626543587,-6.3497080907537));
#86199=CARTESIAN_POINT('Ctrl Pts',(19.6425621221851,-17.0397201767748,-6.34693475346956));
#86200=CARTESIAN_POINT('Ctrl Pts',(19.6201866386643,-17.0292487349793,-6.34532916368714));
#86201=CARTESIAN_POINT('Ctrl Pts',(19.55662327483,-17.0008471136649,-6.34078012479797));
#86202=CARTESIAN_POINT('Ctrl Pts',(19.5150409357475,-16.9838329553595,-6.33781844973897));
#86203=CARTESIAN_POINT('Ctrl Pts',(19.3704829489971,-16.929987468101,-6.32762833700818));
#86204=CARTESIAN_POINT('Ctrl Pts',(19.2652049020342,-16.8998133509897,-6.32039830598454));
#86205=CARTESIAN_POINT('Ctrl Pts',(19.1041214843611,-16.8668788560421,-6.30983047157207));
#86206=CARTESIAN_POINT('Ctrl Pts',(19.0497689852065,-16.8579582465252,-6.30634427169256));
#86207=CARTESIAN_POINT('Ctrl Pts',(18.9611055010472,-16.8469376707463,-6.30079083250703));
#86208=CARTESIAN_POINT('Ctrl Pts',(18.9269852355622,-16.8435358116761,-6.29868522564573));
#86209=CARTESIAN_POINT('Ctrl Pts',(18.8820200893326,-16.8401534560553,-6.29595006811836));
#86210=CARTESIAN_POINT('Ctrl Pts',(18.8712382213373,-16.8394253979084,-6.29529720537102));
#86211=CARTESIAN_POINT('Ctrl Pts',(18.8535659078902,-16.8383679201015,-6.29423187768985));
#86212=CARTESIAN_POINT('Ctrl Pts',(18.8466786886885,-16.8379895718391,-6.2938178842653));
#86213=CARTESIAN_POINT('Ctrl Pts',(18.8333408036588,-16.8373222238749,-6.29301838846832));
#86214=CARTESIAN_POINT('Ctrl Pts',(18.8268904312178,-16.8370290637167,-6.29263275996703));
#86215=CARTESIAN_POINT('Ctrl Pts',(18.8119899302758,-16.8364201568479,-6.29174425441906));
#86216=CARTESIAN_POINT('Ctrl Pts',(18.8035390133308,-16.8361255163017,-6.29124204384785));
#86217=CARTESIAN_POINT('Ctrl Pts',(18.7807983310311,-16.8354690559655,-6.28989510835804));
#86218=CARTESIAN_POINT('Ctrl Pts',(18.7665061357712,-16.8352013116727,-6.28905332709893));
#86219=CARTESIAN_POINT('Ctrl Pts',(18.6350479479026,-16.8340703656135,-6.28135182791991));
#86220=CARTESIAN_POINT('Ctrl Pts',(18.5179952719898,-16.84279050409,-6.27481073902645));
#86221=CARTESIAN_POINT('Ctrl Pts',(18.2404054660157,-16.8868348208592,-6.25942582610652));
#86222=CARTESIAN_POINT('Ctrl Pts',(18.0821083924364,-16.9312160528081,-6.25076841668036));
#86223=CARTESIAN_POINT('Ctrl Pts',(17.9016686564573,-17.0052368164309,-6.23955361745208));
#86224=CARTESIAN_POINT('Ctrl Pts',(17.8730712694035,-17.0177136079514,-6.23773208932225));
#86225=CARTESIAN_POINT('Ctrl Pts',(17.8382749432368,-17.0338194254977,-6.23544864359803));
#86226=CARTESIAN_POINT('Ctrl Pts',(17.8318034802732,-17.0368546973697,-6.23502107085787));
#86227=CARTESIAN_POINT('Ctrl Pts',(17.8216539560528,-17.0416779276029,-6.23434573451489));
#86228=CARTESIAN_POINT('Ctrl Pts',(17.8179654235865,-17.0434439022241,-6.23409931239371));
#86229=CARTESIAN_POINT('Ctrl Pts',(17.8110620452372,-17.0467736847109,-6.23363620989974));
#86230=CARTESIAN_POINT('Ctrl Pts',(17.807846035753,-17.048334952087,-6.23341968736249));
#86231=CARTESIAN_POINT('Ctrl Pts',(17.800489649668,-17.0519292902876,-6.23292262615336));
#86232=CARTESIAN_POINT('Ctrl Pts',(17.7963519651558,-17.0539677458202,-6.23264175497193));
#86233=CARTESIAN_POINT('Ctrl Pts',(17.7855282359894,-17.0593441521694,-6.231903698042));
#86234=CARTESIAN_POINT('Ctrl Pts',(17.7788532137776,-17.0627039780824,-6.23144519626959));
#86235=CARTESIAN_POINT('Ctrl Pts',(17.7341726007515,-17.0854909548363,-6.22835435169245));
#86236=CARTESIAN_POINT('Ctrl Pts',(17.6967469970419,-17.1060269547391,-6.22565941201138));
#86237=CARTESIAN_POINT('Ctrl Pts',(17.6537632245609,-17.1313327056938,-6.2224602927846));
#86238=CARTESIAN_POINT('Ctrl Pts',(17.6475745436013,-17.1350188187123,-6.22199711003756));
#86239=CARTESIAN_POINT('Ctrl Pts',(17.5067332063704,-17.2198837888335,-6.21139884073029));
#86240=CARTESIAN_POINT('Ctrl Pts',(17.3815204018575,-17.3157810046314,-6.20082558747141));
#86241=CARTESIAN_POINT('Ctrl Pts',(17.1996368741147,-17.4903510061928,-6.18444645934869));
#86242=CARTESIAN_POINT('Ctrl Pts',(17.1356824215481,-17.5605715656691,-6.17842083327181));
#86243=CARTESIAN_POINT('Ctrl Pts',(17.0633767518922,-17.6515531917824,-6.17128275493334));
#86244=CARTESIAN_POINT('Ctrl Pts',(17.0503589549969,-17.6684514726908,-6.16998270808881));
#86245=CARTESIAN_POINT('Ctrl Pts',(17.0322147355487,-17.6927554246906,-6.16814848201649));
#86246=CARTESIAN_POINT('Ctrl Pts',(17.0268770668084,-17.7000010856115,-6.16760604876475));
#86247=CARTESIAN_POINT('Ctrl Pts',(17.0177495690953,-17.7125581794175,-6.16667346187058));
#86248=CARTESIAN_POINT('Ctrl Pts',(17.0139378254468,-17.7178534587254,-6.16628246096825));
#86249=CARTESIAN_POINT('Ctrl Pts',(17.0066870510081,-17.7280250901367,-6.16553568292628));
#86250=CARTESIAN_POINT('Ctrl Pts',(17.0032440433173,-17.7328985180634,-6.16517975496167));
#86251=CARTESIAN_POINT('Ctrl Pts',(16.9943461643336,-17.745606751596,-6.16425641712621));
#86252=CARTESIAN_POINT('Ctrl Pts',(16.9889235641388,-17.7534640700907,-6.16369024335043));
#86253=CARTESIAN_POINT('Ctrl Pts',(16.9706219477666,-17.7803705493189,-6.16176718612473));
#86254=CARTESIAN_POINT('Ctrl Pts',(16.9579999313758,-17.7995931525738,-6.16041999474128));
#86255=CARTESIAN_POINT('Ctrl Pts',(16.8517988247959,-17.9672217507519,-6.1488890428652));
#86256=CARTESIAN_POINT('Ctrl Pts',(16.776691026808,-18.1265196858736,-6.13945578184607));
#86257=CARTESIAN_POINT('Ctrl Pts',(16.695013960994,-18.3759801243864,-6.12517347375519));
#86258=CARTESIAN_POINT('Ctrl Pts',(16.6730620305314,-18.460273191983,-6.12040912736751));
#86259=CARTESIAN_POINT('Ctrl Pts',(16.6490998648993,-18.58279614198,-6.11328125960133));
#86260=CARTESIAN_POINT('Ctrl Pts',(16.6428359519368,-18.6201075673872,-6.11108386664042));
#86261=CARTESIAN_POINT('Ctrl Pts',(16.6365221765187,-18.6650625222771,-6.10838291865366));
#86262=CARTESIAN_POINT('Ctrl Pts',(16.6355092976138,-18.6725664583643,-6.10793029583871));
#86263=CARTESIAN_POINT('Ctrl Pts',(16.633999500558,-18.684223237831,-6.10722420073402));
#86264=CARTESIAN_POINT('Ctrl Pts',(16.6334745843573,-18.6883724795121,-6.1069722800572));
#86265=CARTESIAN_POINT('Ctrl Pts',(16.6325251661729,-18.6960601177614,-6.10650439715054));
#86266=CARTESIAN_POINT('Ctrl Pts',(16.6320973021972,-18.6995980409812,-6.1062886268257));
#86267=CARTESIAN_POINT('Ctrl Pts',(16.6311517266855,-18.7075859865194,-6.10580045657992));
#86268=CARTESIAN_POINT('Ctrl Pts',(16.6306392094378,-18.7120365560352,-6.10552776963964));
#86269=CARTESIAN_POINT('Ctrl Pts',(16.6291723816884,-18.7251399554786,-6.10472293755726));
#86270=CARTESIAN_POINT('Ctrl Pts',(16.6282573256534,-18.7337969613771,-6.10418866430249));
#86271=CARTESIAN_POINT('Ctrl Pts',(16.6221408159027,-18.7952888771069,-6.10037676771165));
#86272=CARTESIAN_POINT('Ctrl Pts',(16.6188755558014,-18.8482929513325,-6.0970029929845));
#86273=CARTESIAN_POINT('Ctrl Pts',(16.6172125017547,-18.9177948226885,-6.09251063019151));
#86274=CARTESIAN_POINT('Ctrl Pts',(16.6170107020456,-18.9342348551601,-6.0914429592908));
#86275=CARTESIAN_POINT('Ctrl Pts',(16.6169886659508,-18.969450098497,-6.08914720684106));
#86276=CARTESIAN_POINT('Ctrl Pts',(16.6172266780594,-18.9882239675803,-6.08791797178373));
#86277=CARTESIAN_POINT('Ctrl Pts',(16.6217705576826,-19.1630888292966,-6.07643128871818));
#86278=CARTESIAN_POINT('Ctrl Pts',(16.6430861352163,-19.3182802893092,-6.06600972408595));
#86279=CARTESIAN_POINT('Ctrl Pts',(16.682457428045,-19.4743841569531,-6.05574885775411));
#86280=CARTESIAN_POINT('Ctrl Pts',(16.6836495232712,-19.4790436937119,-6.05544274146085));
#86281=CARTESIAN_POINT('Ctrl Pts',(16.7007617039586,-19.5449932002223,-6.05111238892324));
#86282=CARTESIAN_POINT('Ctrl Pts',(16.7194091640515,-19.6055472396799,-6.04716615599437));
#86283=CARTESIAN_POINT('Ctrl Pts',(16.7422893786803,-19.6694948135655,-6.0430290074528));
#86284=CARTESIAN_POINT('Ctrl Pts',(16.7438474203191,-19.6738051789005,-6.0427502863575));
#86285=CARTESIAN_POINT('Ctrl Pts',(16.745419449956,-19.6781104571528,-6.04247203196383));
#86286=CARTESIAN_POINT('Origin',(18.734,-18.952,0.));
#86287=CARTESIAN_POINT('',(16.7454193808392,-19.6781102678644,-5.2445270093495));
#86288=CARTESIAN_POINT('',(16.7454194499637,-19.6781104571739,-5.46434829365947));
#86289=CARTESIAN_POINT('',(16.7454194499637,-19.6781104571739,0.));
#86290=CARTESIAN_POINT('',(16.6170010064127,-18.9536488955056,-5.51218454189074));
#86291=CARTESIAN_POINT('Ctrl Pts',(16.7454194499637,-19.6781104571738,-5.46434829365948));
#86292=CARTESIAN_POINT('Ctrl Pts',(16.7446943071836,-19.6761245267768,-5.46447551690423));
#86293=CARTESIAN_POINT('Ctrl Pts',(16.7439721428843,-19.6741375198516,-5.46460291538803));
#86294=CARTESIAN_POINT('Ctrl Pts',(16.7420395627859,-19.668795186884,-5.46494573705574));
#86295=CARTESIAN_POINT('Ctrl Pts',(16.740834673765,-19.6654379478235,-5.46516148725336));
#86296=CARTESIAN_POINT('Ctrl Pts',(16.7382466302088,-19.6581690313182,-5.46562930939242));
#86297=CARTESIAN_POINT('Ctrl Pts',(16.7368665075815,-19.6542563823876,-5.46588155128637));
#86298=CARTESIAN_POINT('Ctrl Pts',(16.7330506743712,-19.6433362668555,-5.46658669042906));
#86299=CARTESIAN_POINT('Ctrl Pts',(16.7306403118551,-19.6363200959883,-5.46704104538664));
#86300=CARTESIAN_POINT('Ctrl Pts',(16.7169874844115,-19.5958885730821,-5.46966620983734));
#86301=CARTESIAN_POINT('Ctrl Pts',(16.7065449808684,-19.562211267477,-5.47187977553071));
#86302=CARTESIAN_POINT('Ctrl Pts',(16.6759043949841,-19.4539041773888,-5.47904995503641));
#86303=CARTESIAN_POINT('Ctrl Pts',(16.6589516976596,-19.3784249555281,-5.48412164478996));
#86304=CARTESIAN_POINT('Ctrl Pts',(16.6268475125217,-19.1870216376276,-5.49692887962248));
#86305=CARTESIAN_POINT('Ctrl Pts',(16.6170917570329,-19.0704424925791,-5.50467061913699));
#86306=CARTESIAN_POINT('Ctrl Pts',(16.6170006442156,-18.9536515473445,-5.51218500318624));
#86307=CARTESIAN_POINT('Ctrl Pts',(16.6170006421803,-18.9536489362698,-5.51218517118397));
#86308=CARTESIAN_POINT('Ctrl Pts',(16.6169350227986,-18.8694029946168,-5.51760559206411));
#86309=CARTESIAN_POINT('Ctrl Pts',(16.6218981978728,-18.7852181862553,-5.52290048669229));
#86310=CARTESIAN_POINT('Ctrl Pts',(16.6330988041816,-18.6912100105785,-5.52867287540626));
#86311=CARTESIAN_POINT('Ctrl Pts',(16.6344059040723,-18.6808876771746,-5.52930485326695));
#86312=CARTESIAN_POINT('Ctrl Pts',(16.6367383481429,-18.6634977365485,-5.53036651801471));
#86313=CARTESIAN_POINT('Ctrl Pts',(16.6377234402747,-18.6564250019566,-5.53079746726724));
#86314=CARTESIAN_POINT('Ctrl Pts',(16.6396009366482,-18.6434267198169,-5.53158795047688));
#86315=CARTESIAN_POINT('Ctrl Pts',(16.6404827461591,-18.6374997379464,-5.53194781578317));
#86316=CARTESIAN_POINT('Ctrl Pts',(16.6423536690302,-18.6252811808389,-5.53268851343968));
#86317=CARTESIAN_POINT('Ctrl Pts',(16.6433460334406,-18.618990159104,-5.53306923867726));
#86318=CARTESIAN_POINT('Ctrl Pts',(16.6456303021374,-18.6049219739914,-5.53391923499687));
#86319=CARTESIAN_POINT('Ctrl Pts',(16.6469372946277,-18.5971473298608,-5.53438802202666));
#86320=CARTESIAN_POINT('Ctrl Pts',(16.6503588000011,-18.5774675616511,-5.53557232868738));
#86321=CARTESIAN_POINT('Ctrl Pts',(16.6525319506701,-18.5655728187298,-5.53628598174709));
#86322=CARTESIAN_POINT('Ctrl Pts',(16.6655166090979,-18.4977911985791,-5.54034127620859));
#86323=CARTESIAN_POINT('Ctrl Pts',(16.6784773211522,-18.4423368536831,-5.54361371769315));
#86324=CARTESIAN_POINT('Ctrl Pts',(16.7044778550569,-18.3483651850948,-5.54912153051582));
#86325=CARTESIAN_POINT('Ctrl Pts',(16.7164193773397,-18.3095797473647,-5.55138377997392));
#86326=CARTESIAN_POINT('Ctrl Pts',(16.7772584422577,-18.1304571376729,-5.56183572081334));
#86327=CARTESIAN_POINT('Ctrl Pts',(16.8397261769852,-17.9951860173959,-5.56971124631329));
#86328=CARTESIAN_POINT('Ctrl Pts',(16.9473241089663,-17.8147856574959,-5.58140631501462));
#86329=CARTESIAN_POINT('Ctrl Pts',(16.9810917181612,-17.76339647281,-5.5848954987269));
#86330=CARTESIAN_POINT('Ctrl Pts',(17.0245031309752,-17.7032117611225,-5.58926844938547));
#86331=CARTESIAN_POINT('Ctrl Pts',(17.0320560824401,-17.6929374541602,-5.59002551701624));
#86332=CARTESIAN_POINT('Ctrl Pts',(17.0427968236048,-17.6786000334856,-5.5910978610143));
#86333=CARTESIAN_POINT('Ctrl Pts',(17.0459075357386,-17.6744791628357,-5.59140794107597));
#86334=CARTESIAN_POINT('Ctrl Pts',(17.0512483419108,-17.6674575738203,-5.59193956495328));
#86335=CARTESIAN_POINT('Ctrl Pts',(17.0534709641874,-17.6645511477927,-5.59216058428967));
#86336=CARTESIAN_POINT('Ctrl Pts',(17.057758976812,-17.6589739248193,-5.59258659438384));
#86337=CARTESIAN_POINT('Ctrl Pts',(17.0598232317183,-17.6563022933221,-5.59279150036745));
#86338=CARTESIAN_POINT('Ctrl Pts',(17.0653350907805,-17.6492038133727,-5.59333813627106));
#86339=CARTESIAN_POINT('Ctrl Pts',(17.0687938905799,-17.6447857502881,-5.59368065136171));
#86340=CARTESIAN_POINT('Ctrl Pts',(17.08127082961,-17.6289783317728,-5.59491422656436));
#86341=CARTESIAN_POINT('Ctrl Pts',(17.0903883505925,-17.6176684202998,-5.59581197951903));
#86342=CARTESIAN_POINT('Ctrl Pts',(17.200503309865,-17.4839164000592,-5.60660193792685));
#86343=CARTESIAN_POINT('Ctrl Pts',(17.3148381850228,-17.3731221783315,-5.61724586839603));
#86344=CARTESIAN_POINT('Ctrl Pts',(17.5176005004806,-17.2166167868411,-5.63410078951487));
#86345=CARTESIAN_POINT('Ctrl Pts',(17.5987568061117,-17.1624723268067,-5.64042665492986));
#86346=CARTESIAN_POINT('Ctrl Pts',(17.7122850875287,-17.0975735432327,-5.64865929151614));
#86347=CARTESIAN_POINT('Ctrl Pts',(17.7415946565475,-17.0817244391084,-5.65073406370446));
#86348=CARTESIAN_POINT('Ctrl Pts',(17.7854570821705,-17.0593275041427,-5.65376557909403));
#86349=CARTESIAN_POINT('Ctrl Pts',(17.7997283748285,-17.0522422797378,-5.65474072790219));
#86350=CARTESIAN_POINT('Ctrl Pts',(17.8257475257002,-17.0396887536952,-5.65649867414142));
#86351=CARTESIAN_POINT('Ctrl Pts',(17.8374680790026,-17.0341659649094,-5.65728333088977));
#86352=CARTESIAN_POINT('Ctrl Pts',(17.8559004135295,-17.0256864520797,-5.65850623506506));
#86353=CARTESIAN_POINT('Ctrl Pts',(17.8625779659465,-17.0226564822884,-5.65894700383009));
#86354=CARTESIAN_POINT('Ctrl Pts',(17.8693096748947,-17.0196440174112,-5.65938910762456));
#86355=CARTESIAN_POINT('Ctrl Pts',(17.8693481578123,-17.0196267975417,-5.65939163490994));
#86356=CARTESIAN_POINT('Ctrl Pts',(17.8694264533099,-17.0195917656287,-5.65939677665411));
#86357=CARTESIAN_POINT('Ctrl Pts',(17.8694662658332,-17.0195739537075,-5.65939939110402));
#86358=CARTESIAN_POINT('Ctrl Pts',(17.8695472699262,-17.0195377158909,-5.65940471040463));
#86359=CARTESIAN_POINT('Ctrl Pts',(17.8695884614128,-17.0195192901368,-5.65940741524432));
#86360=CARTESIAN_POINT('Ctrl Pts',(17.8696722746066,-17.0194818020789,-5.65941291866806));
#86361=CARTESIAN_POINT('Ctrl Pts',(17.8697148964165,-17.0194627398408,-5.65941571725291));
#86362=CARTESIAN_POINT('Ctrl Pts',(17.8698016326997,-17.0194239512271,-5.65942141224898));
#86363=CARTESIAN_POINT('Ctrl Pts',(17.8698457336059,-17.0194042310392,-5.6594243077628));
#86364=CARTESIAN_POINT('Ctrl Pts',(17.8699354782875,-17.0193641044377,-5.65943019989428));
#86365=CARTESIAN_POINT('Ctrl Pts',(17.8699811233137,-17.0193436975943,-5.65943319658701));
#86366=CARTESIAN_POINT('Ctrl Pts',(17.8700740092451,-17.0193021743753,-5.65943929453521));
#86367=CARTESIAN_POINT('Ctrl Pts',(17.8701212512532,-17.0192810576444,-5.6594423958558));
#86368=CARTESIAN_POINT('Ctrl Pts',(17.8702173914648,-17.0192380881082,-5.6594487069971));
#86369=CARTESIAN_POINT('Ctrl Pts',(17.8702662906793,-17.0192162349992,-5.65945191687633));
#86370=CARTESIAN_POINT('Ctrl Pts',(17.8703658080825,-17.0191717651008,-5.65945844923198));
#86371=CARTESIAN_POINT('Ctrl Pts',(17.8704164271829,-17.0191491480631,-5.65946177175981));
#86372=CARTESIAN_POINT('Ctrl Pts',(17.8705194496144,-17.0191031216335,-5.65946853367027));
#86373=CARTESIAN_POINT('Ctrl Pts',(17.8705718539176,-17.0190797119783,-5.65947197310764));
#86374=CARTESIAN_POINT('Ctrl Pts',(17.8706785147643,-17.0190320704522,-5.65947897327325));
#86375=CARTESIAN_POINT('Ctrl Pts',(17.8707327721683,-17.0190078383806,-5.65948253404822));
#86376=CARTESIAN_POINT('Ctrl Pts',(17.8708432101602,-17.0189585208956,-5.65948978151524));
#86377=CARTESIAN_POINT('Ctrl Pts',(17.8708993913897,-17.018933435393,-5.65949346823892));
#86378=CARTESIAN_POINT('Ctrl Pts',(17.8710137506744,-17.0188823787639,-5.659500972404));
#86379=CARTESIAN_POINT('Ctrl Pts',(17.8710719295412,-17.0188564074873,-5.65950478988741));
#86380=CARTESIAN_POINT('Ctrl Pts',(17.8711903608708,-17.0188035456843,-5.6595125605751));
#86381=CARTESIAN_POINT('Ctrl Pts',(17.8712506139923,-17.0187766550922,-5.65951651381048));
#86382=CARTESIAN_POINT('Ctrl Pts',(17.8713732738242,-17.0187219196513,-5.65952456121369));
#86383=CARTESIAN_POINT('Ctrl Pts',(17.8714356811169,-17.0186940747881,-5.65952865540668));
#86384=CARTESIAN_POINT('Ctrl Pts',(17.8715627324487,-17.0186373944475,-5.65953699014101));
#86385=CARTESIAN_POINT('Ctrl Pts',(17.871627377147,-17.0186085589401,-5.65954123071157));
#86386=CARTESIAN_POINT('Ctrl Pts',(17.8717589900414,-17.0185498594166,-5.65954986384918));
#86387=CARTESIAN_POINT('Ctrl Pts',(17.8718259586386,-17.0185199955058,-5.65955425642745));
#86388=CARTESIAN_POINT('Ctrl Pts',(17.8719623113204,-17.0184591990169,-5.65956319956844));
#86389=CARTESIAN_POINT('Ctrl Pts',(17.8720316931899,-17.0184282677323,-5.65956774996957));
#86390=CARTESIAN_POINT('Ctrl Pts',(17.8721597313376,-17.0183711950234,-5.65957614689648));
#86391=CARTESIAN_POINT('Ctrl Pts',(17.8722183884455,-17.0183450519521,-5.65957999354451));
#86392=CARTESIAN_POINT('Ctrl Pts',(17.8723455735027,-17.0182883733799,-5.65958833378747));
#86393=CARTESIAN_POINT('Ctrl Pts',(17.8724141029666,-17.018257838371,-5.65959282741978));
#86394=CARTESIAN_POINT('Ctrl Pts',(17.8725627043293,-17.0181916348017,-5.65960257104508));
#86395=CARTESIAN_POINT('Ctrl Pts',(17.8726427776966,-17.018155967181,-5.65960782104974));
#86396=CARTESIAN_POINT('Ctrl Pts',(17.8728164233179,-17.0180786319644,-5.65961920542613));
#86397=CARTESIAN_POINT('Ctrl Pts',(17.8729099970741,-17.0180369658773,-5.65962533978073));
#86398=CARTESIAN_POINT('Ctrl Pts',(17.8731129330203,-17.0179466211511,-5.65963864258498));
#86399=CARTESIAN_POINT('Ctrl Pts',(17.8732222968437,-17.0178979447612,-5.65964581098369));
#86400=CARTESIAN_POINT('Ctrl Pts',(17.8734594918218,-17.01779239652,-5.65966135696751));
#86401=CARTESIAN_POINT('Ctrl Pts',(17.8735873239917,-17.0177355282849,-5.65966973440319));
#86402=CARTESIAN_POINT('Ctrl Pts',(17.8738603533401,-17.0176140991275,-5.65968762556345));
#86403=CARTESIAN_POINT('Ctrl Pts',(17.8740055521962,-17.0175495418603,-5.65969713916434));
#86404=CARTESIAN_POINT('Ctrl Pts',(17.8800513360354,-17.0148623243139,-5.66009322281979));
#86405=CARTESIAN_POINT('Ctrl Pts',(17.8859639318968,-17.0122666358823,-5.66047886515401));
#86406=CARTESIAN_POINT('Ctrl Pts',(17.8996478086091,-17.0063338036385,-5.66136747146807));
#86407=CARTESIAN_POINT('Ctrl Pts',(17.9074274292356,-17.0030160812955,-5.66186976848795));
#86408=CARTESIAN_POINT('Ctrl Pts',(17.928413223001,-16.994214666736,-5.66321708880192));
#86409=CARTESIAN_POINT('Ctrl Pts',(17.9416555621867,-16.988817946999,-5.66405916577417));
#86410=CARTESIAN_POINT('Ctrl Pts',(18.0634385186055,-16.9406200923856,-5.67173194859101));
#86411=CARTESIAN_POINT('Ctrl Pts',(18.1752954471009,-16.906723416681,-5.6782469384445));
#86412=CARTESIAN_POINT('Ctrl Pts',(18.4481258427835,-16.8481167008556,-5.69352434138673));
#86413=CARTESIAN_POINT('Ctrl Pts',(18.6102383492975,-16.8323961832075,-5.70210470895674));
#86414=CARTESIAN_POINT('Ctrl Pts',(18.8054972418901,-16.8359508169542,-5.71331233068431));
#86415=CARTESIAN_POINT('Ctrl Pts',(18.8384409162346,-16.8373208697635,-5.71523458434318));
#86416=CARTESIAN_POINT('Ctrl Pts',(18.8785926222888,-16.8399311470804,-5.71763013311381));
#86417=CARTESIAN_POINT('Ctrl Pts',(18.8858456019452,-16.8404402031728,-5.71806496797585));
#86418=CARTESIAN_POINT('Ctrl Pts',(18.8972006262636,-16.8412959701197,-5.7187492280128));
#86419=CARTESIAN_POINT('Ctrl Pts',(18.9013046059562,-16.8416173061911,-5.71899725215569));
#86420=CARTESIAN_POINT('Ctrl Pts',(18.9089668395643,-16.8422397394575,-5.71946170027918));
#86421=CARTESIAN_POINT('Ctrl Pts',(18.9125252777922,-16.8425378703443,-5.71967795634331));
#86422=CARTESIAN_POINT('Ctrl Pts',(18.9206372324492,-16.8432381737941,-5.72017221190029));
#86423=CARTESIAN_POINT('Ctrl Pts',(18.9251901942608,-16.843646091162,-5.72045052974823));
#86424=CARTESIAN_POINT('Ctrl Pts',(18.93704612942,-16.844747029102,-5.721177576326));
#86425=CARTESIAN_POINT('Ctrl Pts',(18.944346813191,-16.8454632619812,-5.72162755942545));
#86426=CARTESIAN_POINT('Ctrl Pts',(18.9915467508741,-16.8503416192697,-5.7245508748871));
#86427=CARTESIAN_POINT('Ctrl Pts',(19.0313218380476,-16.8555989115244,-5.72707950848353));
#86428=CARTESIAN_POINT('Ctrl Pts',(19.2554634123781,-16.8917315644293,-5.74161077908658));
#86429=CARTESIAN_POINT('Ctrl Pts',(19.4352570585357,-16.9457900248012,-5.75426243444807));
#86430=CARTESIAN_POINT('Ctrl Pts',(19.6769844769193,-17.0550022500074,-5.77133966825835));
#86431=CARTESIAN_POINT('Ctrl Pts',(19.7465040706997,-17.0911781063814,-5.77627398346786));
#86432=CARTESIAN_POINT('Ctrl Pts',(19.8304196120095,-17.140944115937,-5.7822535054873));
#86433=CARTESIAN_POINT('Ctrl Pts',(19.8468386260565,-17.15098650434,-5.7834248383092));
#86434=CARTESIAN_POINT('Ctrl Pts',(19.8704224628136,-17.1658567985635,-5.78510977979849));
#86435=CARTESIAN_POINT('Ctrl Pts',(19.8776979144243,-17.1705066281298,-5.78562992083963));
#86436=CARTESIAN_POINT('Ctrl Pts',(19.89036817752,-17.1787139563357,-5.78653643052581));
#86437=CARTESIAN_POINT('Ctrl Pts',(19.8957754877898,-17.1822518619751,-5.7869235218915));
#86438=CARTESIAN_POINT('Ctrl Pts',(19.9062179450938,-17.1891526586306,-5.78767152365043));
#86439=CARTESIAN_POINT('Ctrl Pts',(19.9112550242194,-17.192512498227,-5.78803254332648));
#86440=CARTESIAN_POINT('Ctrl Pts',(19.9232211596349,-17.2005685574896,-5.78889072630208));
#86441=CARTESIAN_POINT('Ctrl Pts',(19.9301369475409,-17.2052843762867,-5.78938714531626));
#86442=CARTESIAN_POINT('Ctrl Pts',(19.9547609130254,-17.2222900808458,-5.79115640509348));
#86443=CARTESIAN_POINT('Ctrl Pts',(19.9723095139871,-17.234809501203,-5.79242051212765));
#86444=CARTESIAN_POINT('Ctrl Pts',(20.1431267712248,-17.3606535062871,-5.80476723875693));
#86445=CARTESIAN_POINT('Ctrl Pts',(20.2806128910576,-17.4939135859242,-5.81493699732937));
#86446=CARTESIAN_POINT('Ctrl Pts',(20.4459354991579,-17.7042499463965,-5.829537841401));
#86447=CARTESIAN_POINT('Ctrl Pts',(20.490125763983,-17.7672536903842,-5.83377648366255));
#86448=CARTESIAN_POINT('Ctrl Pts',(20.5493717944037,-17.8623443803206,-5.84019112560869));
#86449=CARTESIAN_POINT('Ctrl Pts',(20.5672094732885,-17.8926290435782,-5.84223672412439));
#86450=CARTESIAN_POINT('Ctrl Pts',(20.5878853854289,-17.9298195305303,-5.84476930748475));
#86451=CARTESIAN_POINT('Ctrl Pts',(20.5914526923786,-17.936316276413,-5.84521246473651));
#86452=CARTESIAN_POINT('Ctrl Pts',(20.5969628220267,-17.9464773871417,-5.84590694501551));
#86453=CARTESIAN_POINT('Ctrl Pts',(20.5989291562691,-17.950129028945,-5.84615679739511));
#86454=CARTESIAN_POINT('Ctrl Pts',(20.6025667278976,-17.956932108814,-5.84662283028362));
#86455=CARTESIAN_POINT('Ctrl Pts',(20.6042407351354,-17.9600820010215,-5.84683883153487));
#86456=CARTESIAN_POINT('Ctrl Pts',(20.6080210937815,-17.9672388955982,-5.84733010967557));
#86457=CARTESIAN_POINT('Ctrl Pts',(20.6101225486658,-17.9712484136192,-5.84760568970901));
#86458=CARTESIAN_POINT('Ctrl Pts',(20.616328450418,-17.983182038179,-5.84842687485972));
#86459=CARTESIAN_POINT('Ctrl Pts',(20.6203956094586,-17.9911252752903,-5.84897473663431));
#86460=CARTESIAN_POINT('Ctrl Pts',(20.650873827475,-18.0515891501038,-5.85315327381671));
#86461=CARTESIAN_POINT('Ctrl Pts',(20.6751347407946,-18.1051590765481,-5.85690168862045));
#86462=CARTESIAN_POINT('Ctrl Pts',(20.7573841374128,-18.3089442862489,-5.87115228501349));
#86463=CARTESIAN_POINT('Ctrl Pts',(20.8004134778637,-18.4646133598965,-5.88197243785938));
#86464=CARTESIAN_POINT('Ctrl Pts',(20.83827332445,-18.7057689371455,-5.89773293319788));
#86465=CARTESIAN_POINT('Ctrl Pts',(20.8463182405322,-18.7885665658537,-5.90298236303472));
#86466=CARTESIAN_POINT('Ctrl Pts',(20.8502283583189,-18.891490113137,-5.90929917240716));
#86467=CARTESIAN_POINT('Ctrl Pts',(20.850703145337,-18.911358300341,-5.91050920873632));
#86468=CARTESIAN_POINT('Ctrl Pts',(20.8509839287434,-18.9399770784174,-5.91223922545566));
#86469=CARTESIAN_POINT('Ctrl Pts',(20.8510155351723,-18.948723930948,-5.91276623586004));
#86470=CARTESIAN_POINT('Ctrl Pts',(20.8509761845312,-18.9639510534059,-5.91368073249653));
#86471=CARTESIAN_POINT('Ctrl Pts',(20.8509296835682,-18.9704312187982,-5.91406897946326));
#86472=CARTESIAN_POINT('Ctrl Pts',(20.8507825313564,-18.9829356586667,-5.9148163954341));
#86473=CARTESIAN_POINT('Ctrl Pts',(20.8506859158304,-18.9889599095375,-5.91517568702399));
#86474=CARTESIAN_POINT('Ctrl Pts',(20.8503959608,-19.0032376021382,-5.91602538732019));
#86475=CARTESIAN_POINT('Ctrl Pts',(20.8501800573199,-19.0114905261439,-5.9165150860796));
#86476=CARTESIAN_POINT('Ctrl Pts',(20.8492481751235,-19.0405977626733,-5.91823724521997));
#86477=CARTESIAN_POINT('Ctrl Pts',(20.8482721414848,-19.0614429690031,-5.9194615755354));
#86478=CARTESIAN_POINT('Ctrl Pts',(20.8349195301613,-19.2780217101206,-5.93209802108429));
#86479=CARTESIAN_POINT('Ctrl Pts',(20.7957116125451,-19.471136842044,-5.94253264527725));
#86480=CARTESIAN_POINT('Ctrl Pts',(20.7060363475559,-19.725409376425,-5.95726787856034));
#86481=CARTESIAN_POINT('Ctrl Pts',(20.6780044229229,-19.7933884761063,-5.96132793154709));
#86482=CARTESIAN_POINT('Ctrl Pts',(20.6318415645186,-19.890645122005,-5.96749811587761));
#86483=CARTESIAN_POINT('Ctrl Pts',(20.6164405123277,-19.9211618470911,-5.96948906163561));
#86484=CARTESIAN_POINT('Ctrl Pts',(20.5968388670197,-19.9577705438264,-5.97196095558192));
#86485=CARTESIAN_POINT('Ctrl Pts',(20.5933354846469,-19.9642324748997,-5.97240049907114));
#86486=CARTESIAN_POINT('Ctrl Pts',(20.5878093207955,-19.9742999034154,-5.97309054237961));
#86487=CARTESIAN_POINT('Ctrl Pts',(20.5858094709634,-19.9779180147411,-5.97333960195996));
#86488=CARTESIAN_POINT('Ctrl Pts',(20.5820635311024,-19.9846484981735,-5.97380494150045));
#86489=CARTESIAN_POINT('Ctrl Pts',(20.580320164469,-19.9877623209086,-5.97402104710093));
#86490=CARTESIAN_POINT('Ctrl Pts',(20.5763382018878,-19.994832495569,-5.97451358841931));
#86491=CARTESIAN_POINT('Ctrl Pts',(20.574094740651,-19.9987860375872,-5.97479033376068));
#86492=CARTESIAN_POINT('Ctrl Pts',(20.5682393351684,-20.009027742675,-5.97551062455493));
#86493=CARTESIAN_POINT('Ctrl Pts',(20.5646078179868,-20.0153045663024,-5.97595538722397));
#86494=CARTESIAN_POINT('Ctrl Pts',(20.5414281557698,-20.0548982776846,-5.97878136511788));
#86495=CARTESIAN_POINT('Ctrl Pts',(20.5210047429295,-20.0876913164861,-5.98121385426217));
#86496=CARTESIAN_POINT('Ctrl Pts',(20.4925758994939,-20.1306714727416,-5.98450801605362));
#86497=CARTESIAN_POINT('Ctrl Pts',(20.4853562319744,-20.1413725115899,-5.98533723008799));
#86498=CARTESIAN_POINT('Ctrl Pts',(20.4775930864207,-20.1526551414211,-5.98622064873828));
#86499=CARTESIAN_POINT('Ctrl Pts',(20.4771465239886,-20.1533033819726,-5.98627143756127));
#86500=CARTESIAN_POINT('Ctrl Pts',(20.4637351643345,-20.1727484041632,-5.98779589475466));
#86501=CARTESIAN_POINT('Ctrl Pts',(20.4504677719701,-20.1913339906392,-5.98928001143226));
#86502=CARTESIAN_POINT('Ctrl Pts',(20.4097690239052,-20.2464393109292,-5.99375473987897));
#86503=CARTESIAN_POINT('Ctrl Pts',(20.3814541667607,-20.2822892651614,-5.99676602233453));
#86504=CARTESIAN_POINT('Ctrl Pts',(20.2814846202797,-20.400771285459,-6.00700642808005));
#86505=CARTESIAN_POINT('Ctrl Pts',(20.2045912823814,-20.478765088136,-6.01423700915862));
#86506=CARTESIAN_POINT('Ctrl Pts',(20.0804340602093,-20.5865753048392,-6.02480599869715));
#86507=CARTESIAN_POINT('Ctrl Pts',(20.0374614715426,-20.6210446720852,-6.02829279981356));
#86508=CARTESIAN_POINT('Ctrl Pts',(19.9656280358225,-20.674195396578,-6.03384708465625));
#86509=CARTESIAN_POINT('Ctrl Pts',(19.9375730022023,-20.6939175775582,-6.0359529505016));
#86510=CARTESIAN_POINT('Ctrl Pts',(19.900060847423,-20.7189487492393,-6.03868839018908));
#86511=CARTESIAN_POINT('Ctrl Pts',(19.8910258513193,-20.7248781595169,-6.03934128212492));
#86512=CARTESIAN_POINT('Ctrl Pts',(19.876150233645,-20.734478448887,-6.04040664527257));
#86513=CARTESIAN_POINT('Ctrl Pts',(19.8703364545421,-20.738190370815,-6.04082064517096));
#86514=CARTESIAN_POINT('Ctrl Pts',(19.8590454245858,-20.7453219131538,-6.04162014506751));
#86515=CARTESIAN_POINT('Ctrl Pts',(19.8535704732395,-20.7487450148686,-6.04200577123864));
#86516=CARTESIAN_POINT('Ctrl Pts',(19.840889846732,-20.7565928529328,-6.04289425940899));
#86517=CARTESIAN_POINT('Ctrl Pts',(19.8336731210191,-20.7609995930699,-6.04339645501683));
#86518=CARTESIAN_POINT('Ctrl Pts',(19.8141869501236,-20.7727387095206,-6.04474332372036));
#86519=CARTESIAN_POINT('Ctrl Pts',(19.8018691957539,-20.7799903422187,-6.04558505361947));
#86520=CARTESIAN_POINT('Ctrl Pts',(19.687971721121,-20.8454991751386,-6.05328244033555));
#86521=CARTESIAN_POINT('Ctrl Pts',(19.5817897889601,-20.895362789935,-6.05981987563774));
#86522=CARTESIAN_POINT('Ctrl Pts',(19.3186488225908,-20.9932374225985,-6.07518824952006));
#86523=CARTESIAN_POINT('Ctrl Pts',(19.1592049096371,-21.0323011801609,-6.08383349797618));
#86524=CARTESIAN_POINT('Ctrl Pts',(18.9656474453625,-21.0565234569939,-6.09504685944817));
#86525=CARTESIAN_POINT('Ctrl Pts',(18.9343370969792,-21.0597344066654,-6.09688397808098));
#86526=CARTESIAN_POINT('Ctrl Pts',(18.8958241196297,-21.0628181654,-6.09918478879517));
#86527=CARTESIAN_POINT('Ctrl Pts',(18.888676741851,-21.0633539436256,-6.09961351470817));
#86528=CARTESIAN_POINT('Ctrl Pts',(18.8774430253808,-21.064138692859,-6.1002902684027));
#86529=CARTESIAN_POINT('Ctrl Pts',(18.8733583737348,-21.0644121289226,-6.10053694532106));
#86530=CARTESIAN_POINT('Ctrl Pts',(18.8657059619658,-21.064902107403,-6.10100025901778));
#86531=CARTESIAN_POINT('Ctrl Pts',(18.8621384378512,-21.0651214626611,-6.10121673634778));
#86532=CARTESIAN_POINT('Ctrl Pts',(18.853972511504,-21.0656028033679,-6.10171333840958));
#86533=CARTESIAN_POINT('Ctrl Pts',(18.8493738127962,-21.0658588165524,-6.10199379334528));
#86534=CARTESIAN_POINT('Ctrl Pts',(18.8351628233966,-21.0666034423847,-6.10286282430619));
#86535=CARTESIAN_POINT('Ctrl Pts',(18.8255481651871,-21.0670415033285,-6.10345412012196));
#86536=CARTESIAN_POINT('Ctrl Pts',(18.7294012836835,-21.0707653212148,-6.10939822993797));
#86537=CARTESIAN_POINT('Ctrl Pts',(18.6427568672297,-21.0688039239774,-6.11500403451157));
#86538=CARTESIAN_POINT('Ctrl Pts',(18.4300122787677,-21.0509020042212,-6.12902167268099));
#86539=CARTESIAN_POINT('Ctrl Pts',(18.304740786168,-21.028905934046,-6.13748305759993));
#86540=CARTESIAN_POINT('Ctrl Pts',(18.0889892583227,-20.9706555573753,-6.15194729410804));
#86541=CARTESIAN_POINT('Ctrl Pts',(17.9976065088923,-20.9391432458174,-6.15804197531535));
#86542=CARTESIAN_POINT('Ctrl Pts',(17.8952172254498,-20.8957968701017,-6.16482090748904));
#86543=CARTESIAN_POINT('Ctrl Pts',(17.8818109387683,-20.8899568199136,-6.16570766687662));
#86544=CARTESIAN_POINT('Ctrl Pts',(17.8614116580938,-20.8808178599124,-6.16705593554101));
#86545=CARTESIAN_POINT('Ctrl Pts',(17.8543746394194,-20.8776188560157,-6.16752084917421));
#86546=CARTESIAN_POINT('Ctrl Pts',(17.8415803463361,-20.8717178452156,-6.16836583266904));
#86547=CARTESIAN_POINT('Ctrl Pts',(17.8358174493384,-20.8690283123987,-6.16874632639375));
#86548=CARTESIAN_POINT('Ctrl Pts',(17.8233758156527,-20.8631534069505,-6.16956758342424));
#86549=CARTESIAN_POINT('Ctrl Pts',(17.8167014673545,-20.8599588973965,-6.17000802446731));
#86550=CARTESIAN_POINT('Ctrl Pts',(17.7985847189788,-20.8511707308412,-6.17120329790977));
#86551=CARTESIAN_POINT('Ctrl Pts',(17.7871757127367,-20.8455086460224,-6.17195574260547));
#86552=CARTESIAN_POINT('Ctrl Pts',(17.7311353646994,-20.8170636663194,-6.17565124543442));
#86553=CARTESIAN_POINT('Ctrl Pts',(17.6872694976211,-20.7928030293878,-6.17854193722928));
#86554=CARTESIAN_POINT('Ctrl Pts',(17.4954798087589,-20.6776560301375,-6.19124130415125));
#86555=CARTESIAN_POINT('Ctrl Pts',(17.3582178045451,-20.5703461393829,-6.20043478884896));
#86556=CARTESIAN_POINT('Ctrl Pts',(17.1912971766094,-20.4030992892138,-6.21342103395186));
#86557=CARTESIAN_POINT('Ctrl Pts',(17.1489970438489,-20.3567724473044,-6.21691352420763));
#86558=CARTESIAN_POINT('Ctrl Pts',(17.0889997131088,-20.2848989097309,-6.22229878014459));
#86559=CARTESIAN_POINT('Ctrl Pts',(17.0697048391059,-20.2607271823504,-6.22410480465985));
#86560=CARTESIAN_POINT('Ctrl Pts',(17.046623499201,-20.2304757950802,-6.2263709770117));
#86561=CARTESIAN_POINT('Ctrl Pts',(17.0423282330767,-20.22478688073,-6.22679739217315));
#86562=CARTESIAN_POINT('Ctrl Pts',(17.0356167565575,-20.215803800939,-6.22747130569117));
#86563=CARTESIAN_POINT('Ctrl Pts',(17.0331811648282,-20.2125240886831,-6.22771747195634));
#86564=CARTESIAN_POINT('Ctrl Pts',(17.0286315569084,-20.2063604981061,-6.22818036358819));
#86565=CARTESIAN_POINT('Ctrl Pts',(17.0265153489955,-20.2034783065662,-6.2283969327432));
#86566=CARTESIAN_POINT('Ctrl Pts',(17.021681949478,-20.1968603267421,-6.22889446050305));
#86567=CARTESIAN_POINT('Ctrl Pts',(17.0189696845702,-20.1931210075826,-6.22917575395577));
#86568=CARTESIAN_POINT('Ctrl Pts',(17.0106032965739,-20.1815067251903,-6.23004992143128));
#86569=CARTESIAN_POINT('Ctrl Pts',(17.0049911062667,-20.1736019080929,-6.23064556095518));
#86570=CARTESIAN_POINT('Ctrl Pts',(16.9421416851821,-20.0837772550423,-6.23741893712719));
#86571=CARTESIAN_POINT('Ctrl Pts',(16.8907261923401,-19.9979507172628,-6.24393186162075));
#86572=CARTESIAN_POINT('Ctrl Pts',(16.8076114278052,-19.8339121607158,-6.25604812770089));
#86573=CARTESIAN_POINT('Ctrl Pts',(16.7741769643098,-19.7568679012229,-6.26161628492563));
#86574=CARTESIAN_POINT('Ctrl Pts',(16.7454195726558,-19.6781107931876,-6.26710635146282));
#86575=CARTESIAN_POINT('',(16.617000284924,-18.950901652078,-5.287306223149));
#86576=CARTESIAN_POINT('Ctrl Pts',(16.745419449956,-19.6781104571528,-6.04247203196383));
#86577=CARTESIAN_POINT('Ctrl Pts',(16.7481387492912,-19.6855577342365,-6.04199070707657));
#86578=CARTESIAN_POINT('Ctrl Pts',(16.7508999037001,-19.6929897896995,-6.04151077890519));
#86579=CARTESIAN_POINT('Ctrl Pts',(16.7565355594176,-19.7079018417615,-6.04054860527923));
#86580=CARTESIAN_POINT('Ctrl Pts',(16.7594108953478,-19.7153813455215,-6.04006639995054));
#86581=CARTESIAN_POINT('Ctrl Pts',(16.7646516739141,-19.7287862461309,-6.03920283878544));
#86582=CARTESIAN_POINT('Ctrl Pts',(16.7670015547204,-19.734717585904,-6.03882096602459));
#86583=CARTESIAN_POINT('Ctrl Pts',(16.7720578574421,-19.7473136300662,-6.03801046018694));
#86584=CARTESIAN_POINT('Ctrl Pts',(16.7747715122763,-19.7539753585776,-6.03758207679116));
#86585=CARTESIAN_POINT('Ctrl Pts',(16.7821570623799,-19.771844853206,-6.03643363270401));
#86586=CARTESIAN_POINT('Ctrl Pts',(16.7868915607623,-19.783026576937,-6.0357156995046));
#86587=CARTESIAN_POINT('Ctrl Pts',(16.8108500261443,-19.8382816408423,-6.03217068491787));
#86588=CARTESIAN_POINT('Ctrl Pts',(16.831476300288,-19.881733865292,-6.02939189453329));
#86589=CARTESIAN_POINT('Ctrl Pts',(16.930577056764,-20.0733660666286,-6.01711721964233));
#86590=CARTESIAN_POINT('Ctrl Pts',(17.0250013165618,-20.2126035042643,-6.00819923758914));
#86591=CARTESIAN_POINT('Ctrl Pts',(17.199551880873,-20.4138148562186,-5.99361572160997));
#86592=CARTESIAN_POINT('Ctrl Pts',(17.2693672499324,-20.4837569939524,-5.98812307736492));
#86593=CARTESIAN_POINT('Ctrl Pts',(17.3511068479787,-20.5549315408755,-5.98170194278436));
#86594=CARTESIAN_POINT('Ctrl Pts',(17.3584620216197,-20.5612477300285,-5.98112420455132));
#86595=CARTESIAN_POINT('Ctrl Pts',(17.3693853990106,-20.5704984803597,-5.98026582182577));
#86596=CARTESIAN_POINT('Ctrl Pts',(17.3729203611795,-20.5734723420463,-5.97998798066685));
#86597=CARTESIAN_POINT('Ctrl Pts',(17.3792087466741,-20.5787275265782,-5.97949356826934));
#86598=CARTESIAN_POINT('Ctrl Pts',(17.3819582460412,-20.5810134686855,-5.97927733901209));
#86599=CARTESIAN_POINT('Ctrl Pts',(17.3878614400673,-20.5858961612704,-5.97881295821649));
#86600=CARTESIAN_POINT('Ctrl Pts',(17.3910168158417,-20.5884907133155,-5.97856466042602));
#86601=CARTESIAN_POINT('Ctrl Pts',(17.3996985525994,-20.595587374442,-5.97788132804067));
#86602=CARTESIAN_POINT('Ctrl Pts',(17.4052401142143,-20.600070681905,-5.9774449759169));
#86603=CARTESIAN_POINT('Ctrl Pts',(17.4349421974628,-20.6238534713412,-5.9751057122744));
#86604=CARTESIAN_POINT('Ctrl Pts',(17.4594994153522,-20.6426487602319,-5.97317002821319));
#86605=CARTESIAN_POINT('Ctrl Pts',(17.5350662192519,-20.6979030162766,-5.96723065921933));
#86606=CARTESIAN_POINT('Ctrl Pts',(17.587290050673,-20.7326388590416,-5.96314954411795));
#86607=CARTESIAN_POINT('Ctrl Pts',(17.7561737857018,-20.834455697973,-5.95019052642287));
#86608=CARTESIAN_POINT('Ctrl Pts',(17.8777423218272,-20.8927760163412,-5.9412248743718));
#86609=CARTESIAN_POINT('Ctrl Pts',(18.0423575389777,-20.9532464173255,-5.92993142488277));
#86610=CARTESIAN_POINT('Ctrl Pts',(18.0810894524547,-20.9662156421424,-5.92732947852865));
#86611=CARTESIAN_POINT('Ctrl Pts',(18.1665837467932,-20.9921174813466,-5.92171050148367));
#86612=CARTESIAN_POINT('Ctrl Pts',(18.213465361283,-21.0045800438516,-5.91870888879738));
#86613=CARTESIAN_POINT('Ctrl Pts',(18.2730119749151,-21.0182375578628,-5.91499301897416));
#86614=CARTESIAN_POINT('Ctrl Pts',(18.2853121651644,-21.0209434120858,-5.91423055066757));
#86615=CARTESIAN_POINT('Ctrl Pts',(18.3048443021115,-21.0250578024833,-5.91302768013504));
#86616=CARTESIAN_POINT('Ctrl Pts',(18.3120605690662,-21.0265385955021,-5.91258497251876));
#86617=CARTESIAN_POINT('Ctrl Pts',(18.3255226958963,-21.0292279028188,-5.9117622075774));
#86618=CARTESIAN_POINT('Ctrl Pts',(18.3317665390026,-21.0304459849698,-5.91138184856124));
#86619=CARTESIAN_POINT('Ctrl Pts',(18.3456487633709,-21.0330893039478,-5.91053890314906));
#86620=CARTESIAN_POINT('Ctrl Pts',(18.3532897159894,-21.0345006737356,-5.91007676338969));
#86621=CARTESIAN_POINT('Ctrl Pts',(18.3755207657643,-21.0384805536681,-5.90873738525707));
#86622=CARTESIAN_POINT('Ctrl Pts',(18.3901304551278,-21.0409380591613,-5.9078636782931));
#86623=CARTESIAN_POINT('Ctrl Pts',(18.506761463762,-21.0592998779833,-5.90093807131005));
#86624=CARTESIAN_POINT('Ctrl Pts',(18.6098026865321,-21.067875510353,-5.89512919743182));
#86625=CARTESIAN_POINT('Ctrl Pts',(18.872705181404,-21.0704748771832,-5.88065401722067));
#86626=CARTESIAN_POINT('Ctrl Pts',(19.0319912381937,-21.0539914986133,-5.87222578509501));
#86627=CARTESIAN_POINT('Ctrl Pts',(19.235308715798,-21.0093610985793,-5.86047071994354));
#86628=CARTESIAN_POINT('Ctrl Pts',(19.2823439196685,-20.9973271806295,-5.85767580525113));
#86629=CARTESIAN_POINT('Ctrl Pts',(19.3363657926869,-20.9815084741173,-5.85433393032942));
#86630=CARTESIAN_POINT('Ctrl Pts',(19.3437994923213,-20.9792872933324,-5.85387113548219));
#86631=CARTESIAN_POINT('Ctrl Pts',(19.3556664429391,-20.9756702880281,-5.85312739398144));
#86632=CARTESIAN_POINT('Ctrl Pts',(19.3601076775438,-20.9743006146719,-5.85284793443878));
#86633=CARTESIAN_POINT('Ctrl Pts',(19.3679697913483,-20.9718475635104,-5.85235118750972));
#86634=CARTESIAN_POINT('Ctrl Pts',(19.3713924687732,-20.9707701000234,-5.85213424864671));
#86635=CARTESIAN_POINT('Ctrl Pts',(19.3786459916911,-20.9684663954237,-5.85167302286242));
#86636=CARTESIAN_POINT('Ctrl Pts',(19.3824760267831,-20.9672379563071,-5.85142861365488));
#86637=CARTESIAN_POINT('Ctrl Pts',(19.3928136955816,-20.9638897478543,-5.85076661739924));
#86638=CARTESIAN_POINT('Ctrl Pts',(19.3993145230052,-20.961749343955,-5.85034784399367));
#86639=CARTESIAN_POINT('Ctrl Pts',(19.4316533015979,-20.9509276719108,-5.84825266693107));
#86640=CARTESIAN_POINT('Ctrl Pts',(19.4573309949732,-20.9417799062435,-5.84655092824721));
#86641=CARTESIAN_POINT('Ctrl Pts',(19.5312424694622,-20.9138290236909,-5.84155577834798));
#86642=CARTESIAN_POINT('Ctrl Pts',(19.578970470398,-20.8937499469217,-5.83820916551103));
#86643=CARTESIAN_POINT('Ctrl Pts',(19.7513075146447,-20.813690644089,-5.8257878301129));
#86644=CARTESIAN_POINT('Ctrl Pts',(19.8707060636378,-20.7432872504515,-5.81654188506069));
#86645=CARTESIAN_POINT('Ctrl Pts',(20.0148044229229,-20.63807245764,-5.80498894382203));
#86646=CARTESIAN_POINT('Ctrl Pts',(20.0465448755708,-20.6134832342372,-5.80241428550193));
#86647=CARTESIAN_POINT('Ctrl Pts',(20.1232083782398,-20.5505233744019,-5.79612733501363));
#86648=CARTESIAN_POINT('Ctrl Pts',(20.1672630672117,-20.5111455858879,-5.79245394757114));
#86649=CARTESIAN_POINT('Ctrl Pts',(20.2183862453488,-20.4614489214751,-5.78811263181848));
#86650=CARTESIAN_POINT('Ctrl Pts',(20.227081720279,-20.4528482795876,-5.78737127448224));
#86651=CARTESIAN_POINT('Ctrl Pts',(20.2412892904811,-20.438549973334,-5.78615491197485));
#86652=CARTESIAN_POINT('Ctrl Pts',(20.2468446954101,-20.4328959310682,-5.78567799303401));
#86653=CARTESIAN_POINT('Ctrl Pts',(20.2568085952445,-20.42264053584,-5.7848201996241));
#86654=CARTESIAN_POINT('Ctrl Pts',(20.2612282972139,-20.4180502491288,-5.78443883663041));
#86655=CARTESIAN_POINT('Ctrl Pts',(20.2706324608343,-20.4081944405868,-5.78362547086898));
#86656=CARTESIAN_POINT('Ctrl Pts',(20.2756107432682,-20.4029231153759,-5.78319373834905));
#86657=CARTESIAN_POINT('Ctrl Pts',(20.28903055778,-20.3885663108431,-5.7820266843052));
#86658=CARTESIAN_POINT('Ctrl Pts',(20.2974195777854,-20.3794319720167,-5.78129361294003));
#86659=CARTESIAN_POINT('Ctrl Pts',(20.3401523099804,-20.3320739967788,-5.77754027536949));
#86660=CARTESIAN_POINT('Ctrl Pts',(20.3731779965723,-20.2926810217713,-5.7745755781199));
#86661=CARTESIAN_POINT('Ctrl Pts',(20.5101613572313,-20.1166487804733,-5.76191625201652));
#86662=CARTESIAN_POINT('Ctrl Pts',(20.5987105623636,-19.968863126292,-5.75281706380873));
#86663=CARTESIAN_POINT('Ctrl Pts',(20.7054048832317,-19.7288713900421,-5.7383926325167));
#86664=CARTESIAN_POINT('Ctrl Pts',(20.7369623533648,-19.6434506633284,-5.73330447001261));
#86665=CARTESIAN_POINT('Ctrl Pts',(20.7656829766929,-19.5470181719367,-5.72734303716419));
#86666=CARTESIAN_POINT('Ctrl Pts',(20.7683772552651,-19.5377401454468,-5.72676728004617));
#86667=CARTESIAN_POINT('Ctrl Pts',(20.7722639615859,-19.5240055092786,-5.72591128899053));
#86668=CARTESIAN_POINT('Ctrl Pts',(20.7735055232919,-19.5195627712275,-5.72563383591011));
#86669=CARTESIAN_POINT('Ctrl Pts',(20.7756834930981,-19.5116698088704,-5.72513985160232));
#86670=CARTESIAN_POINT('Ctrl Pts',(20.7766256925935,-19.5082212335887,-5.72492366015826));
#86671=CARTESIAN_POINT('Ctrl Pts',(20.7786269157219,-19.5008228290067,-5.72445906327036));
#86672=CARTESIAN_POINT('Ctrl Pts',(20.7796832157756,-19.4968723723711,-5.72421051002225));
#86673=CARTESIAN_POINT('Ctrl Pts',(20.7825541577406,-19.4860093072181,-5.72352577079516));
#86674=CARTESIAN_POINT('Ctrl Pts',(20.7843452312957,-19.4790906056236,-5.72308825843168));
#86675=CARTESIAN_POINT('Ctrl Pts',(20.7937630546606,-19.4419362450744,-5.72073174931013));
#86676=CARTESIAN_POINT('Ctrl Pts',(20.8007556579683,-19.4115456201891,-5.71877941676331));
#86677=CARTESIAN_POINT('Ctrl Pts',(20.840282190576,-19.2205460098615,-5.70640137008781));
#86678=CARTESIAN_POINT('Ctrl Pts',(20.8547462255173,-19.0567703334592,-5.69536346719755));
#86679=CARTESIAN_POINT('Ctrl Pts',(20.8469095587802,-18.7758460519865,-5.67700415240263));
#86680=CARTESIAN_POINT('Ctrl Pts',(20.8339246690935,-18.6591838884141,-5.66953964958673));
#86681=CARTESIAN_POINT('Ctrl Pts',(20.8085934934435,-18.5301526884317,-5.6615105742519));
#86682=CARTESIAN_POINT('Ctrl Pts',(20.805697852025,-18.5161544505642,-5.66064231408016));
#86683=CARTESIAN_POINT('Ctrl Pts',(20.8008639251029,-18.4939235691392,-5.65926764211037));
#86684=CARTESIAN_POINT('Ctrl Pts',(20.799017742708,-18.4856715460704,-5.65875829983431));
#86685=CARTESIAN_POINT('Ctrl Pts',(20.7956746903455,-18.4711381037897,-5.65786282672941));
#86686=CARTESIAN_POINT('Ctrl Pts',(20.7941984407228,-18.4648520981111,-5.65747603933531));
#86687=CARTESIAN_POINT('Ctrl Pts',(20.7910857799759,-18.4518653486167,-5.65667798879759));
#86688=CARTESIAN_POINT('Ctrl Pts',(20.7894453320078,-18.4451656438717,-5.65626686080514));
#86689=CARTESIAN_POINT('Ctrl Pts',(20.7851508737915,-18.4279905856371,-5.65521432865093));
#86690=CARTESIAN_POINT('Ctrl Pts',(20.7824493271382,-18.4175272372723,-5.65457446476992));
#86691=CARTESIAN_POINT('Ctrl Pts',(20.770843162559,-18.3739564942231,-5.65191520729823));
#86692=CARTESIAN_POINT('Ctrl Pts',(20.7612148074383,-18.341046086698,-5.64991931067721));
#86693=CARTESIAN_POINT('Ctrl Pts',(20.7340522132623,-18.2559314289023,-5.6447791213387));
#86694=CARTESIAN_POINT('Ctrl Pts',(20.7152729622998,-18.2041508144812,-5.64167413957681));
#86695=CARTESIAN_POINT('Ctrl Pts',(20.6532485698303,-18.0519322729142,-5.63253422564439));
#86696=CARTESIAN_POINT('Ctrl Pts',(20.6042229019265,-17.9540500155665,-5.62664803774175));
#86697=CARTESIAN_POINT('Ctrl Pts',(20.5264211001456,-17.8247715683042,-5.61843346120246));
#86698=CARTESIAN_POINT('Ctrl Pts',(20.5039401887055,-17.7897913711027,-5.61616121667305));
#86699=CARTESIAN_POINT('Ctrl Pts',(20.436937111708,-17.6919920922932,-5.60960384701895));
#86700=CARTESIAN_POINT('Ctrl Pts',(20.3900029976483,-17.6309148007828,-5.60525832414802));
#86701=CARTESIAN_POINT('Ctrl Pts',(20.3336587858995,-17.5653236990881,-5.6001337453355));
#86702=CARTESIAN_POINT('Ctrl Pts',(20.3274151160633,-17.5581536472439,-5.59956703565788));
#86703=CARTESIAN_POINT('Ctrl Pts',(20.3180906160939,-17.5475901867729,-5.59872197520079));
#86704=CARTESIAN_POINT('Ctrl Pts',(20.3150466220836,-17.5441642207356,-5.59844630372645));
#86705=CARTESIAN_POINT('Ctrl Pts',(20.3096103236611,-17.5380856222539,-5.59795427608276));
#86706=CARTESIAN_POINT('Ctrl Pts',(20.3072224064655,-17.5354291337211,-5.59773824960221));
#86707=CARTESIAN_POINT('Ctrl Pts',(20.3020732722935,-17.5297299502232,-5.59727262132433));
#86708=CARTESIAN_POINT('Ctrl Pts',(20.2993099578999,-17.5266892911335,-5.59702286444327));
#86709=CARTESIAN_POINT('Ctrl Pts',(20.2916561865217,-17.5183164387628,-5.5963314867647));
#86710=CARTESIAN_POINT('Ctrl Pts',(20.286747272054,-17.5130013013145,-5.59588849744779));
#86711=CARTESIAN_POINT('Ctrl Pts',(20.2596762709581,-17.4839899218357,-5.59344849065966));
#86712=CARTESIAN_POINT('Ctrl Pts',(20.2370002093771,-17.4607817809088,-5.59141533965383));
#86713=CARTESIAN_POINT('Ctrl Pts',(20.0973946205978,-17.3243201436816,-5.57901130615425));
#86714=CARTESIAN_POINT('Ctrl Pts',(19.9682564581952,-17.224343344445,-5.56804903287148));
#86715=CARTESIAN_POINT('Ctrl Pts',(19.7289491046462,-17.0797247201609,-5.54978483409524));
#86716=CARTESIAN_POINT('Ctrl Pts',(19.6241159203917,-17.0276715710751,-5.5423426912471));
#86717=CARTESIAN_POINT('Ctrl Pts',(19.5022235771501,-16.979254248858,-5.53433426529295));
#86718=CARTESIAN_POINT('Ctrl Pts',(19.4888876693982,-16.9741127723112,-5.53346612179614));
#86719=CARTESIAN_POINT('Ctrl Pts',(19.4675807762464,-16.9661450866604,-5.53209159905664));
#86720=CARTESIAN_POINT('Ctrl Pts',(19.4596433378722,-16.9632309733015,-5.53158229032558));
#86721=CARTESIAN_POINT('Ctrl Pts',(19.445614076855,-16.9581755101072,-5.53068685624182));
#86722=CARTESIAN_POINT('Ctrl Pts',(19.4395295571149,-16.9560143446546,-5.53030007450372));
#86723=CARTESIAN_POINT('Ctrl Pts',(19.4269248010237,-16.9516020898591,-5.52950201653108));
#86724=CARTESIAN_POINT('Ctrl Pts',(19.4204032523089,-16.9493549601288,-5.52909087554189));
#86725=CARTESIAN_POINT('Ctrl Pts',(19.403636055677,-16.9436690142584,-5.52803827057667));
#86726=CARTESIAN_POINT('Ctrl Pts',(19.3933747674154,-16.9402766795595,-5.52739834729997));
#86727=CARTESIAN_POINT('Ctrl Pts',(19.3504470503807,-16.9264487161243,-5.52473851277569));
#86728=CARTESIAN_POINT('Ctrl Pts',(19.3175543898468,-16.9167286569075,-5.52274211151668));
#86729=CARTESIAN_POINT('Ctrl Pts',(19.2312560780637,-16.8934911086931,-5.51760032892731));
#86730=CARTESIAN_POINT('Ctrl Pts',(19.1775324962696,-16.8812508524518,-5.51449429051936));
#86731=CARTESIAN_POINT('Ctrl Pts',(19.0159317184782,-16.8510109383415,-5.50535253296559));
#86732=CARTESIAN_POINT('Ctrl Pts',(18.9070747335003,-16.8392561551318,-5.49946555200795));
#86733=CARTESIAN_POINT('Ctrl Pts',(18.7544605181739,-16.8346549291794,-5.49115293314775));
#86734=CARTESIAN_POINT('Ctrl Pts',(18.7110949416286,-16.8346800090703,-5.48878282590522));
#86735=CARTESIAN_POINT('Ctrl Pts',(18.6387105333112,-16.8369459271424,-5.48477287328617));
#86736=CARTESIAN_POINT('Ctrl Pts',(18.609681810146,-16.8384535272548,-5.48315018718292));
#86737=CARTESIAN_POINT('Ctrl Pts',(18.5332498328724,-16.8440030323251,-5.47881882376279));
#86738=CARTESIAN_POINT('Ctrl Pts',(18.4859387752249,-16.8490457142325,-5.47607786768121));
#86739=CARTESIAN_POINT('Ctrl Pts',(18.4311994456352,-16.8567529054084,-5.47279571767541));
#86740=CARTESIAN_POINT('Ctrl Pts',(18.4235631836976,-16.8578706959467,-5.47233532576442));
#86741=CARTESIAN_POINT('Ctrl Pts',(18.4113502443046,-16.8597266849239,-5.47159471656187));
#86742=CARTESIAN_POINT('Ctrl Pts',(18.4067695021204,-16.8604382174673,-5.47131596666438));
#86743=CARTESIAN_POINT('Ctrl Pts',(18.3986487575679,-16.8617269534771,-5.47082002294523));
#86744=CARTESIAN_POINT('Ctrl Pts',(18.3951078424171,-16.8622981145192,-5.47060317371342));
#86745=CARTESIAN_POINT('Ctrl Pts',(18.3875923628475,-16.8635299901456,-5.47014162029549));
#86746=CARTESIAN_POINT('Ctrl Pts',(18.3836182901994,-16.8641930429397,-5.46989679120201));
#86747=CARTESIAN_POINT('Ctrl Pts',(18.3728684132865,-16.866018159407,-5.46923249741576));
#86748=CARTESIAN_POINT('Ctrl Pts',(18.3660964059549,-16.8672018791504,-5.46881183252056));
#86749=CARTESIAN_POINT('Ctrl Pts',(18.3321381477671,-16.8733082529736,-5.46669184182298));
#86750=CARTESIAN_POINT('Ctrl Pts',(18.305045705954,-16.8787295469509,-5.46496647039749));
#86751=CARTESIAN_POINT('Ctrl Pts',(18.2264894029349,-16.8960545205585,-5.45987935058538));
#86752=CARTESIAN_POINT('Ctrl Pts',(18.1753572570648,-16.9093555495304,-5.45646222863149));
#86753=CARTESIAN_POINT('Ctrl Pts',(17.9780377817643,-16.9686473861364,-5.44298624312623));
#86754=CARTESIAN_POINT('Ctrl Pts',(17.8364985171484,-17.0285486237564,-5.4327301261204));
#86755=CARTESIAN_POINT('Ctrl Pts',(17.6322178904866,-17.1425049328573,-5.41770539632465));
#86756=CARTESIAN_POINT('Ctrl Pts',(17.564067935396,-17.1858012940929,-5.41264115752182));
#86757=CARTESIAN_POINT('Ctrl Pts',(17.4877006222605,-17.2406831648322,-5.40690597723646));
#86758=CARTESIAN_POINT('Ctrl Pts',(17.4769266843766,-17.2485816305824,-5.40609527355976));
#86759=CARTESIAN_POINT('Ctrl Pts',(17.4596757886423,-17.261481221151,-5.40479444163929));
#86760=CARTESIAN_POINT('Ctrl Pts',(17.4531519315467,-17.2664187454273,-5.40430185271708));
#86761=CARTESIAN_POINT('Ctrl Pts',(17.4417172321457,-17.2751777185676,-5.40343726363277));
#86762=CARTESIAN_POINT('Ctrl Pts',(17.4367943395821,-17.2789832064612,-5.40306464167132));
#86763=CARTESIAN_POINT('Ctrl Pts',(17.4265674645179,-17.286961050281,-5.40228968678376));
#86764=CARTESIAN_POINT('Ctrl Pts',(17.4212665039761,-17.2911371793684,-5.40188750945744));
#86765=CARTESIAN_POINT('Ctrl Pts',(17.4076756771347,-17.3019498332582,-5.40085506336682));
#86766=CARTESIAN_POINT('Ctrl Pts',(17.3994155483161,-17.3086235642033,-5.40022629044215));
#86767=CARTESIAN_POINT('Ctrl Pts',(17.3815453160414,-17.3232853298586,-5.39886295215658));
#86768=CARTESIAN_POINT('Ctrl Pts',(17.3719549823574,-17.3312969029837,-5.39812935681644));
#86769=CARTESIAN_POINT('Ctrl Pts',(17.3443462413243,-17.3547788528114,-5.39601124820017));
#86770=CARTESIAN_POINT('Ctrl Pts',(17.326516177287,-17.3704683643157,-5.39463555590603));
#86771=CARTESIAN_POINT('Ctrl Pts',(17.2657069690694,-17.4258203083558,-5.38991087557279));
#86772=CARTESIAN_POINT('Ctrl Pts',(17.2241082658136,-17.4669624325992,-5.38662114313595));
#86773=CARTESIAN_POINT('Ctrl Pts',(17.0705437080051,-17.6319746888536,-5.37412048580666));
#86774=CARTESIAN_POINT('Ctrl Pts',(16.9716851432441,-17.7671822761984,-5.36533072763668));
#86775=CARTESIAN_POINT('Ctrl Pts',(16.861928867705,-17.9619260508484,-5.35279259969752));
#86776=CARTESIAN_POINT('Ctrl Pts',(16.8361147496659,-18.0123579789408,-5.34955027416261));
#86777=CARTESIAN_POINT('Ctrl Pts',(16.8086439393009,-18.0717890596408,-5.34566589901993));
#86778=CARTESIAN_POINT('Ctrl Pts',(16.8049826228568,-18.0798422089399,-5.34513823146));
#86779=CARTESIAN_POINT('Ctrl Pts',(16.7995310102159,-18.0920354248045,-5.34433696023719));
#86780=CARTESIAN_POINT('Ctrl Pts',(16.7977032434327,-18.096158769006,-5.34406559602872));
#86781=CARTESIAN_POINT('Ctrl Pts',(16.7944540629059,-18.1035524333439,-5.34357823553818));
#86782=CARTESIAN_POINT('Ctrl Pts',(16.7930277230357,-18.1068205307497,-5.34336254449328));
#86783=CARTESIAN_POINT('Ctrl Pts',(16.7899554460828,-18.1139086722036,-5.34289413450356));
#86784=CARTESIAN_POINT('Ctrl Pts',(16.7883125308254,-18.1177299160629,-5.34264124174425));
#86785=CARTESIAN_POINT('Ctrl Pts',(16.7837517930946,-18.1284244493725,-5.34193248465295));
#86786=CARTESIAN_POINT('Ctrl Pts',(16.7808590919814,-18.135308292111,-5.34147513874715));
#86787=CARTESIAN_POINT('Ctrl Pts',(16.7642159201089,-18.1755086922632,-5.33879834044752));
#86788=CARTESIAN_POINT('Ctrl Pts',(16.7512825491522,-18.2091546432478,-5.33653418196317));
#86789=CARTESIAN_POINT('Ctrl Pts',(16.7123640076299,-18.3186699693303,-5.32912522136634));
#86790=CARTESIAN_POINT('Ctrl Pts',(16.6898292561938,-18.3956877983485,-5.32385730482946));
#86791=CARTESIAN_POINT('Ctrl Pts',(16.6354452693788,-18.6302199152264,-5.30796210733017));
#86792=CARTESIAN_POINT('Ctrl Pts',(16.6170836152047,-18.7902875361735,-5.29735395519403));
#86793=CARTESIAN_POINT('Ctrl Pts',(16.617000284924,-18.950901652078,-5.287306223149));
#86794=CARTESIAN_POINT('Ctrl Pts',(16.6170002837517,-18.9509039138869,-5.28730608165431));
#86795=CARTESIAN_POINT('Ctrl Pts',(16.6169868618986,-18.9768271136034,-5.28568437341906));
#86796=CARTESIAN_POINT('Ctrl Pts',(16.6174495936726,-19.0027494402333,-5.28407668181815));
#86797=CARTESIAN_POINT('Ctrl Pts',(16.6190263323593,-19.0462644316672,-5.28140090717751));
#86798=CARTESIAN_POINT('Ctrl Pts',(16.6198840725923,-19.0638627409736,-5.2803250904963));
#86799=CARTESIAN_POINT('Ctrl Pts',(16.6214584306178,-19.0895615601323,-5.27876299448743));
#86800=CARTESIAN_POINT('Ctrl Pts',(16.622002162565,-19.0976715578003,-5.27827132879577));
#86801=CARTESIAN_POINT('Ctrl Pts',(16.6230473372594,-19.1120220182355,-5.27740358485186));
#86802=CARTESIAN_POINT('Ctrl Pts',(16.6235297763737,-19.1182637277103,-5.27702691438678));
#86803=CARTESIAN_POINT('Ctrl Pts',(16.6245388687493,-19.1306063621236,-5.27628352984855));
#86804=CARTESIAN_POINT('Ctrl Pts',(16.6250643197426,-19.1367073214785,-5.27591678175321));
#86805=CARTESIAN_POINT('Ctrl Pts',(16.6261638694004,-19.1488572175267,-5.27518778927124));
#86806=CARTESIAN_POINT('Ctrl Pts',(16.6267375530475,-19.1549061319947,-5.27482553551552));
#86807=CARTESIAN_POINT('Ctrl Pts',(16.628171445051,-19.1693626531271,-5.27396135880791));
#86808=CARTESIAN_POINT('Ctrl Pts',(16.6290559778645,-19.1777677847624,-5.27346020459241));
#86809=CARTESIAN_POINT('Ctrl Pts',(16.6319011557525,-19.2033318817324,-5.27193970815204));
#86810=CARTESIAN_POINT('Ctrl Pts',(16.6340214891345,-19.2204726163725,-5.27092537975229));
#86811=CARTESIAN_POINT('Ctrl Pts',(16.6419662055849,-19.2788271263581,-5.2674880714534));
#86812=CARTESIAN_POINT('Ctrl Pts',(16.6487962825489,-19.3198955704463,-5.26509633678038));
#86813=CARTESIAN_POINT('Ctrl Pts',(16.6780901110545,-19.4687639697274,-5.2564924142788));
#86814=CARTESIAN_POINT('Ctrl Pts',(16.7077221576998,-19.5748697951031,-5.25049678246115));
#86815=CARTESIAN_POINT('Ctrl Pts',(16.7454193808392,-19.6781102678644,-5.2445270093495));
#86816=CARTESIAN_POINT('Origin',(18.734,-18.952,0.));
#86817=CARTESIAN_POINT('',(16.7454194481082,-19.6781104520924,-4.44630497675564));
#86818=CARTESIAN_POINT('',(16.7454194642264,-19.6781104962347,-4.66702132639115));
#86819=CARTESIAN_POINT('',(16.7454194499637,-19.6781104571739,0.));
#86820=CARTESIAN_POINT('Ctrl Pts',(16.7454194642264,-19.6781104962347,-4.66702132639115));
#86821=CARTESIAN_POINT('Ctrl Pts',(16.6988234569433,-19.5504991841709,-4.67446196791304));
#86822=CARTESIAN_POINT('Ctrl Pts',(16.6646102515307,-19.4186749085756,-4.68169548970326));
#86823=CARTESIAN_POINT('Ctrl Pts',(16.6370543933824,-19.2453826839987,-4.69152883179162));
#86824=CARTESIAN_POINT('Ctrl Pts',(16.6319381922759,-19.2061457568985,-4.69377780195413));
#86825=CARTESIAN_POINT('Ctrl Pts',(16.626393980434,-19.1517834673221,-4.69695245069132));
#86826=CARTESIAN_POINT('Ctrl Pts',(16.6250239200878,-19.1367604804233,-4.69783593480563));
#86827=CARTESIAN_POINT('Ctrl Pts',(16.6229323255952,-19.1107556897743,-4.69937787446987));
#86828=CARTESIAN_POINT('Ctrl Pts',(16.6221356455221,-19.0997803490558,-4.70003253407433));
#86829=CARTESIAN_POINT('Ctrl Pts',(16.6211102620138,-19.083945503156,-4.70098328869644));
#86830=CARTESIAN_POINT('Ctrl Pts',(16.6208126722558,-19.0790904303007,-4.70127564097596));
#86831=CARTESIAN_POINT('Ctrl Pts',(16.6203235174173,-19.0706328035693,-4.70178646094323));
#86832=CARTESIAN_POINT('Ctrl Pts',(16.6201244222697,-19.0670306778377,-4.70200450695554));
#86833=CARTESIAN_POINT('Ctrl Pts',(16.6197264096993,-19.0594793959756,-4.70246265010531));
#86834=CARTESIAN_POINT('Ctrl Pts',(16.6195293494743,-19.0555302017514,-4.70270284534969));
#86835=CARTESIAN_POINT('Ctrl Pts',(16.6190357978485,-19.045049313883,-4.70334184113573));
#86836=CARTESIAN_POINT('Ctrl Pts',(16.6187585035133,-19.0385168200452,-4.7037416930887));
#86837=CARTESIAN_POINT('Ctrl Pts',(16.6177066685289,-19.0106966833973,-4.70545098301501));
#86838=CARTESIAN_POINT('Ctrl Pts',(16.6172232246242,-18.9894001117826,-4.7067754745818));
#86839=CARTESIAN_POINT('Ctrl Pts',(16.6170218767854,-18.9629268972801,-4.70843883518829));
#86840=CARTESIAN_POINT('Ctrl Pts',(16.617001493557,-18.9577528772316,-4.70876473205849));
#86841=CARTESIAN_POINT('Ctrl Pts',(16.6169868171325,-18.9040721310964,-4.71215391963486));
#86842=CARTESIAN_POINT('Ctrl Pts',(16.6186407108799,-18.8555823846155,-4.71528276307785));
#86843=CARTESIAN_POINT('Ctrl Pts',(16.6353861336127,-18.6113422023217,-4.73125347287945));
#86844=CARTESIAN_POINT('Ctrl Pts',(16.6759975092691,-18.4182600520973,-4.74444611234127));
#86845=CARTESIAN_POINT('Ctrl Pts',(16.7587957195953,-18.188768490955,-4.75978160671345));
#86846=CARTESIAN_POINT('Ctrl Pts',(16.7764544949314,-18.1445531266853,-4.7627263938696));
#86847=CARTESIAN_POINT('Ctrl Pts',(16.8006203664839,-18.08951013166,-4.76638234636621));
#86848=CARTESIAN_POINT('Ctrl Pts',(16.8057522333939,-18.078097178512,-4.76713987196758));
#86849=CARTESIAN_POINT('Ctrl Pts',(16.8140577650559,-18.0600556036716,-4.76833670074756));
#86850=CARTESIAN_POINT('Ctrl Pts',(16.8171652099536,-18.0533969833946,-4.76877827062177));
#86851=CARTESIAN_POINT('Ctrl Pts',(16.8230280562325,-18.0410029007359,-4.76959996751399));
#86852=CARTESIAN_POINT('Ctrl Pts',(16.8257747611383,-18.0352634381284,-4.76998038978466));
#86853=CARTESIAN_POINT('Ctrl Pts',(16.8319433130545,-18.0225215979931,-4.7708247836726));
#86854=CARTESIAN_POINT('Ctrl Pts',(16.8353780473832,-18.0155255349562,-4.77128830088787));
#86855=CARTESIAN_POINT('Ctrl Pts',(16.8455036892124,-17.9951857541092,-4.77263568882129));
#86856=CARTESIAN_POINT('Ctrl Pts',(16.8522972741185,-17.9818934669447,-4.77351596196072));
#86857=CARTESIAN_POINT('Ctrl Pts',(16.9092402191692,-17.873328397997,-4.78070598899491));
#86858=CARTESIAN_POINT('Ctrl Pts',(16.9664529930495,-17.7819304747911,-4.78674994189988));
#86859=CARTESIAN_POINT('Ctrl Pts',(17.109755897751,-17.5876688993976,-4.80001598495269));
#86860=CARTESIAN_POINT('Ctrl Pts',(17.199144359828,-17.4878335212404,-4.80713503285765));
#86861=CARTESIAN_POINT('Ctrl Pts',(17.3093993042227,-17.385963236324,-4.81548117151138));
#86862=CARTESIAN_POINT('Ctrl Pts',(17.3215810198652,-17.3749676945156,-4.81639828677522));
#86863=CARTESIAN_POINT('Ctrl Pts',(17.3736914804033,-17.3290195133269,-4.82030637030103));
#86864=CARTESIAN_POINT('Ctrl Pts',(17.4147958908763,-17.2954359528519,-4.82335194662809));
#86865=CARTESIAN_POINT('Ctrl Pts',(17.4640568970095,-17.2581849938948,-4.82701707861956));
#86866=CARTESIAN_POINT('Ctrl Pts',(17.4710315783227,-17.2529780696824,-4.82753635589282));
#86867=CARTESIAN_POINT('Ctrl Pts',(17.4816442233066,-17.2451566924231,-4.82832733821555));
#86868=CARTESIAN_POINT('Ctrl Pts',(17.4852588009897,-17.2425104606685,-4.82859688852883));
#86869=CARTESIAN_POINT('Ctrl Pts',(17.4917638953347,-17.2377797222716,-4.82908231315701));
#86870=CARTESIAN_POINT('Ctrl Pts',(17.4946512981478,-17.2356910257103,-4.82929789256426));
#86871=CARTESIAN_POINT('Ctrl Pts',(17.5009390259754,-17.2311667343445,-4.82976760828476));
#86872=CARTESIAN_POINT('Ctrl Pts',(17.5043412547042,-17.2287339545885,-4.8300219268285));
#86873=CARTESIAN_POINT('Ctrl Pts',(17.5139238827321,-17.2219246780926,-4.83073862991125));
#86874=CARTESIAN_POINT('Ctrl Pts',(17.5201205163407,-17.2175712910091,-4.83120254904962));
#86875=CARTESIAN_POINT('Ctrl Pts',(17.5574250787705,-17.1916611531595,-4.83399750136794));
#86876=CARTESIAN_POINT('Ctrl Pts',(17.5890811189297,-17.170909955644,-4.83637787189424));
#86877=CARTESIAN_POINT('Ctrl Pts',(17.6953691754556,-17.1052404387069,-4.84435477389429));
#86878=CARTESIAN_POINT('Ctrl Pts',(17.7722144513456,-17.0640801112438,-4.85009442603247));
#86879=CARTESIAN_POINT('Ctrl Pts',(18.0107217372933,-16.9546785314189,-4.86743165257851));
#86880=CARTESIAN_POINT('Ctrl Pts',(18.1785690169876,-16.9016477585081,-4.87894119187821));
#86881=CARTESIAN_POINT('Ctrl Pts',(18.3736798159472,-16.8657623757734,-4.89115217917399));
#86882=CARTESIAN_POINT('Ctrl Pts',(18.3963686451636,-16.8619705280759,-4.89255633845765));
#86883=CARTESIAN_POINT('Ctrl Pts',(18.4285570947284,-16.8571289318122,-4.89452678066019));
#86884=CARTESIAN_POINT('Ctrl Pts',(18.4380083163656,-16.8557726534075,-4.89510272231644));
#86885=CARTESIAN_POINT('Ctrl Pts',(18.4533807096104,-16.8536727089882,-4.89603531575576));
#86886=CARTESIAN_POINT('Ctrl Pts',(18.4592963408922,-16.8528900678741,-4.8963931957589));
#86887=CARTESIAN_POINT('Ctrl Pts',(18.4716866918103,-16.8513040929079,-4.89714071219739));
#86888=CARTESIAN_POINT('Ctrl Pts',(18.4781619836584,-16.8505056563029,-4.89753019028512));
#86889=CARTESIAN_POINT('Ctrl Pts',(18.4935765002678,-16.848677269474,-4.89845459190866));
#86890=CARTESIAN_POINT('Ctrl Pts',(18.5025188505678,-16.847674348102,-4.89898865816394));
#86891=CARTESIAN_POINT('Ctrl Pts',(18.5326724272337,-16.8444870381601,-4.90078231527588));
#86892=CARTESIAN_POINT('Ctrl Pts',(18.5539106200222,-16.8425660617114,-4.9020336227825));
#86893=CARTESIAN_POINT('Ctrl Pts',(18.6697220741529,-16.8338529005574,-4.90879683995305));
#86894=CARTESIAN_POINT('Ctrl Pts',(18.7646461587201,-16.833098720746,-4.91411557334995));
#86895=CARTESIAN_POINT('Ctrl Pts',(19.0284689899736,-16.8487424624775,-4.92865727462931));
#86896=CARTESIAN_POINT('Ctrl Pts',(19.1957911698045,-16.8790451841467,-4.93757429016926));
#86897=CARTESIAN_POINT('Ctrl Pts',(19.3942326978688,-16.9402237222502,-4.94941731566111));
#86898=CARTESIAN_POINT('Ctrl Pts',(19.4304574451852,-16.9524756501796,-4.95163587933073));
#86899=CARTESIAN_POINT('Ctrl Pts',(19.4731106509165,-16.9682014457571,-4.95433801193991));
#86900=CARTESIAN_POINT('Ctrl Pts',(19.4798803577023,-16.9707368305246,-4.95476961075706));
#86901=CARTESIAN_POINT('Ctrl Pts',(19.4908791616161,-16.9749204528084,-4.95547548944941));
#86902=CARTESIAN_POINT('Ctrl Pts',(19.4951162413002,-16.9765477308828,-4.95574854562345));
#86903=CARTESIAN_POINT('Ctrl Pts',(19.5026747936992,-16.9794785696899,-4.956237728215));
#86904=CARTESIAN_POINT('Ctrl Pts',(19.5059982336508,-16.9807769130603,-4.95645353977999));
#86905=CARTESIAN_POINT('Ctrl Pts',(19.513169763893,-16.9835994793816,-4.95692080598098));
#86906=CARTESIAN_POINT('Ctrl Pts',(19.5170166171156,-16.9851265655413,-4.95717242687282));
#86907=CARTESIAN_POINT('Ctrl Pts',(19.5277035002433,-16.9894052605318,-4.95787411954539));
#86908=CARTESIAN_POINT('Ctrl Pts',(19.5345335938311,-16.9921813045193,-4.95832562646303));
#86909=CARTESIAN_POINT('Ctrl Pts',(19.5732653755652,-17.0081598172767,-4.96090279374959));
#86910=CARTESIAN_POINT('Ctrl Pts',(19.6048528720404,-17.0221046702017,-4.96306943810205));
#86911=CARTESIAN_POINT('Ctrl Pts',(19.7036616063405,-17.0686451715156,-4.97002246954352));
#86912=CARTESIAN_POINT('Ctrl Pts',(19.7695035696544,-17.1040281752955,-4.97491682217222));
#86913=CARTESIAN_POINT('Ctrl Pts',(19.9992014125371,-17.2436016448319,-4.99264425422368));
#86914=CARTESIAN_POINT('Ctrl Pts',(20.1504628739279,-17.3667479439259,-5.00547037846406));
#86915=CARTESIAN_POINT('Ctrl Pts',(20.2972373612967,-17.5242659670621,-5.01869782342656));
#86916=CARTESIAN_POINT('Ctrl Pts',(20.3114107851474,-17.5399409423562,-5.01998620073653));
#86917=CARTESIAN_POINT('Ctrl Pts',(20.330821585278,-17.5620652108692,-5.02176686976182));
#86918=CARTESIAN_POINT('Ctrl Pts',(20.33625893219,-17.5683366700919,-5.02226749857302));
#86919=CARTESIAN_POINT('Ctrl Pts',(20.3455867507635,-17.5792241320495,-5.02312956967299));
#86920=CARTESIAN_POINT('Ctrl Pts',(20.3494945922022,-17.5838250614038,-5.02349172823265));
#86921=CARTESIAN_POINT('Ctrl Pts',(20.3575518636169,-17.5933940072849,-5.02424054430023));
#86922=CARTESIAN_POINT('Ctrl Pts',(20.3616982994939,-17.5983644713011,-5.02462707676828));
#86923=CARTESIAN_POINT('Ctrl Pts',(20.3713655994835,-17.6100616186339,-5.02553108681136));
#86924=CARTESIAN_POINT('Ctrl Pts',(20.3768679401055,-17.6168035123711,-5.02604780861657));
#86925=CARTESIAN_POINT('Ctrl Pts',(20.3946413288914,-17.6388570557911,-5.02772424372196));
#86926=CARTESIAN_POINT('Ctrl Pts',(20.4067413295677,-17.6543056994098,-5.02887710028773));
#86927=CARTESIAN_POINT('Ctrl Pts',(20.4677836211424,-17.7345139826193,-5.03475724037706));
#86928=CARTESIAN_POINT('Ctrl Pts',(20.5131895213832,-17.8018849723305,-5.0393452707916));
#86929=CARTESIAN_POINT('Ctrl Pts',(20.6406534510727,-18.0166992390387,-5.0531884414534));
#86930=CARTESIAN_POINT('Ctrl Pts',(20.7090523841095,-18.1714391576291,-5.0620596615006));
#86931=CARTESIAN_POINT('Ctrl Pts',(20.7741179477669,-18.3841053186586,-5.07456202087068));
#86932=CARTESIAN_POINT('Ctrl Pts',(20.7878941317968,-18.4361478299142,-5.07764924545969));
#86933=CARTESIAN_POINT('Ctrl Pts',(20.8015839524154,-18.4971792190701,-5.08136089540101));
#86934=CARTESIAN_POINT('Ctrl Pts',(20.803443475616,-18.5057164149007,-5.08188214256367));
#86935=CARTESIAN_POINT('Ctrl Pts',(20.8061778320212,-18.5186546814733,-5.08267554156417));
#86936=CARTESIAN_POINT('Ctrl Pts',(20.8070916340495,-18.5230475450693,-5.08294551891231));
#86937=CARTESIAN_POINT('Ctrl Pts',(20.8087062463014,-18.5309350462942,-5.08343139760595));
#86938=CARTESIAN_POINT('Ctrl Pts',(20.8094122021839,-18.5344285756738,-5.08364700160978));
#86939=CARTESIAN_POINT('Ctrl Pts',(20.8109263507429,-18.5420202673165,-5.08411640228897));
#86940=CARTESIAN_POINT('Ctrl Pts',(20.8117312271716,-18.5461189896515,-5.08437037918332));
#86941=CARTESIAN_POINT('Ctrl Pts',(20.813956401713,-18.5576304608555,-5.08508517552231));
#86942=CARTESIAN_POINT('Ctrl Pts',(20.8153491785127,-18.5650483756389,-5.08554751676513));
#86943=CARTESIAN_POINT('Ctrl Pts',(20.823407876091,-18.6092715464762,-5.08831349690364));
#86944=CARTESIAN_POINT('Ctrl Pts',(20.8291366281751,-18.6462383650756,-5.09066531570909));
#86945=CARTESIAN_POINT('Ctrl Pts',(20.8447157358734,-18.7680043940224,-5.09850005886564));
#86946=CARTESIAN_POINT('Ctrl Pts',(20.8504170577727,-18.8532464401609,-5.10412098239));
#86947=CARTESIAN_POINT('Ctrl Pts',(20.8520835937592,-19.1164030776585,-5.12150613993781));
#86948=CARTESIAN_POINT('Ctrl Pts',(20.8308029983747,-19.293684130979,-5.13319015950719));
#86949=CARTESIAN_POINT('Ctrl Pts',(20.7820535464246,-19.4883635979075,-5.14554080955071));
#86950=CARTESIAN_POINT('Ctrl Pts',(20.77615573115,-19.5103988465163,-5.14693304107251));
#86951=CARTESIAN_POINT('Ctrl Pts',(20.7672940952352,-19.5414867933826,-5.14888980255299));
#86952=CARTESIAN_POINT('Ctrl Pts',(20.7646237123329,-19.5506208322699,-5.14946381034992));
#86953=CARTESIAN_POINT('Ctrl Pts',(20.7601804364233,-19.5654471265633,-5.15039412793865));
#86954=CARTESIAN_POINT('Ctrl Pts',(20.7584449504504,-19.5711503708782,-5.15075165409909));
#86955=CARTESIAN_POINT('Ctrl Pts',(20.7547582186108,-19.5830846644017,-5.15149911026087));
#86956=CARTESIAN_POINT('Ctrl Pts',(20.7528021871447,-19.5893141787053,-5.15188887893397));
#86957=CARTESIAN_POINT('Ctrl Pts',(20.7480735952767,-19.6041334380661,-5.15281520608287));
#86958=CARTESIAN_POINT('Ctrl Pts',(20.7452748449081,-19.6127147420156,-5.15335089764109));
#86959=CARTESIAN_POINT('Ctrl Pts',(20.735628094291,-19.6416634590871,-5.15515583012444));
#86960=CARTESIAN_POINT('Ctrl Pts',(20.728524774723,-19.6619448483473,-5.15641664286948));
#86961=CARTESIAN_POINT('Ctrl Pts',(20.6593009910564,-19.8503473638225,-5.16810322495215));
#86962=CARTESIAN_POINT('Ctrl Pts',(20.5763775377804,-20.0100472139787,-5.1777344611722));
#86963=CARTESIAN_POINT('Ctrl Pts',(20.4055670582364,-20.2566572969864,-5.19406000301463));
#86964=CARTESIAN_POINT('Ctrl Pts',(20.328463064136,-20.3498362250276,-5.20068308558403));
#86965=CARTESIAN_POINT('Ctrl Pts',(20.2372032464848,-20.4426907926725,-5.20839927507256));
#86966=CARTESIAN_POINT('Ctrl Pts',(20.2305066482437,-20.4494133977567,-5.20896488448912));
#86967=CARTESIAN_POINT('Ctrl Pts',(20.2205117239458,-20.4593131275309,-5.20980861478114));
#86968=CARTESIAN_POINT('Ctrl Pts',(20.2172478112813,-20.4625250409313,-5.21008406857941));
#86969=CARTESIAN_POINT('Ctrl Pts',(20.2114196428091,-20.4682232540697,-5.21057585819148));
#86970=CARTESIAN_POINT('Ctrl Pts',(20.2088594909027,-20.4707136790727,-5.21079186555056));
#86971=CARTESIAN_POINT('Ctrl Pts',(20.2033388703169,-20.4760568184924,-5.21125762451018));
#86972=CARTESIAN_POINT('Ctrl Pts',(20.2003764340119,-20.4789073498178,-5.21150753210191));
#86973=CARTESIAN_POINT('Ctrl Pts',(20.1921695041917,-20.486758354533,-5.21219974206957));
#86974=CARTESIAN_POINT('Ctrl Pts',(20.1869076680303,-20.4917405023072,-5.21264341828775));
#86975=CARTESIAN_POINT('Ctrl Pts',(20.157828151169,-20.518992542863,-5.21509414724068));
#86976=CARTESIAN_POINT('Ctrl Pts',(20.1335253562638,-20.5407355789536,-5.21713770126414));
#86977=CARTESIAN_POINT('Ctrl Pts',(19.9850465325458,-20.6675245929747,-5.22954523903706));
#86978=CARTESIAN_POINT('Ctrl Pts',(19.8496058956549,-20.758534107256,-5.24049798826835));
#86979=CARTESIAN_POINT('Ctrl Pts',(19.6012651554108,-20.886732643794,-5.25875317507815));
#86980=CARTESIAN_POINT('Ctrl Pts',(19.4931765863139,-20.9316459216739,-5.26619530806575));
#86981=CARTESIAN_POINT('Ctrl Pts',(19.3683368794992,-20.9717794926344,-5.27420197547602));
#86982=CARTESIAN_POINT('Ctrl Pts',(19.3547128580724,-20.9760079147617,-5.27506842114454));
#86983=CARTESIAN_POINT('Ctrl Pts',(19.3329543038577,-20.9825206472383,-5.27644077215336));
#86984=CARTESIAN_POINT('Ctrl Pts',(19.3248472203679,-20.9848944690724,-5.27694959259776));
#86985=CARTESIAN_POINT('Ctrl Pts',(19.3105198928001,-20.9889966831563,-5.27784445889519));
#86986=CARTESIAN_POINT('Ctrl Pts',(19.3043055850123,-20.9907452550821,-5.27823115851425));
#86987=CARTESIAN_POINT('Ctrl Pts',(19.2914318144341,-20.9943041879194,-5.27902932567515));
#86988=CARTESIAN_POINT('Ctrl Pts',(19.284771295619,-20.9961104680013,-5.27944065659752));
#86989=CARTESIAN_POINT('Ctrl Pts',(19.2676435156226,-21.0006655936315,-5.28049432519043));
#86990=CARTESIAN_POINT('Ctrl Pts',(19.2571637116441,-21.0033668257279,-5.28113511604412));
#86991=CARTESIAN_POINT('Ctrl Pts',(19.2132663224012,-21.0143233618144,-5.28380339296977));
#86992=CARTESIAN_POINT('Ctrl Pts',(19.1796695204334,-21.0218436495487,-5.28580717813392));
#86993=CARTESIAN_POINT('Ctrl Pts',(19.091597778484,-21.0393135599577,-5.29097229240118));
#86994=CARTESIAN_POINT('Ctrl Pts',(19.0368886497974,-21.0479516186433,-5.294093808669));
#86995=CARTESIAN_POINT('Ctrl Pts',(18.8730940357218,-21.0672648340811,-5.3032625605962));
#86996=CARTESIAN_POINT('Ctrl Pts',(18.7634527245879,-21.0716287091711,-5.30916115023632));
#86997=CARTESIAN_POINT('Ctrl Pts',(18.593661112367,-21.0652051429016,-5.31841310948858));
#86998=CARTESIAN_POINT('Ctrl Pts',(18.5334831769926,-21.0603461124867,-5.32171765286354));
#86999=CARTESIAN_POINT('Ctrl Pts',(18.4157969663717,-21.0457593265224,-5.32836057403453));
#87000=CARTESIAN_POINT('Ctrl Pts',(18.3583215465393,-21.0362134478195,-5.33169108892318));
#87001=CARTESIAN_POINT('Ctrl Pts',(18.2926015762768,-21.0224916636395,-5.33567374155975));
#87002=CARTESIAN_POINT('Ctrl Pts',(18.2838963721323,-21.0206166913074,-5.33620485123954));
#87003=CARTESIAN_POINT('Ctrl Pts',(18.2707881091677,-21.0177067071606,-5.33701034022951));
#87004=CARTESIAN_POINT('Ctrl Pts',(18.2663759881435,-21.0167123863822,-5.33728244488949));
#87005=CARTESIAN_POINT('Ctrl Pts',(18.2584901017543,-21.0149086404725,-5.33777060092777));
#87006=CARTESIAN_POINT('Ctrl Pts',(18.2550151659508,-21.0141045683352,-5.33798634285901));
#87007=CARTESIAN_POINT('Ctrl Pts',(18.2475010769315,-21.0123458504461,-5.33845424385345));
#87008=CARTESIAN_POINT('Ctrl Pts',(18.2434627499495,-21.01138812059,-5.33870657338992));
#87009=CARTESIAN_POINT('Ctrl Pts',(18.2322075486001,-21.0086838526422,-5.339412199354));
#87010=CARTESIAN_POINT('Ctrl Pts',(18.2249970902658,-21.0069112312037,-5.33986695669133));
#87011=CARTESIAN_POINT('Ctrl Pts',(18.1835029577228,-20.9964785100172,-5.34249899316209));
#87012=CARTESIAN_POINT('Ctrl Pts',(18.1494333585219,-20.9869989860733,-5.34471928541359));
#87013=CARTESIAN_POINT('Ctrl Pts',(18.0413221830518,-20.9539793880848,-5.3519209300234));
#87014=CARTESIAN_POINT('Ctrl Pts',(17.9683350467338,-20.9272163355083,-5.35701840454586));
#87015=CARTESIAN_POINT('Ctrl Pts',(17.7269462436826,-20.8233107164373,-5.37436203939018));
#87016=CARTESIAN_POINT('Ctrl Pts',(17.5672000795249,-20.728109757915,-5.38658232570517));
#87017=CARTESIAN_POINT('Ctrl Pts',(17.4024685262322,-20.5980023674751,-5.39952483469995));
#87018=CARTESIAN_POINT('Ctrl Pts',(17.383342064452,-20.5823444672028,-5.4010353085623));
#87019=CARTESIAN_POINT('Ctrl Pts',(17.3569924000674,-20.5599912406533,-5.40312803996645));
#87020=CARTESIAN_POINT('Ctrl Pts',(17.3495356163368,-20.5535755167236,-5.40372163285419));
#87021=CARTESIAN_POINT('Ctrl Pts',(17.3375875035354,-20.5431497053441,-5.40467505580946));
#87022=CARTESIAN_POINT('Ctrl Pts',(17.3330681556735,-20.5391720807194,-5.40503622395731));
#87023=CARTESIAN_POINT('Ctrl Pts',(17.3240140414579,-20.5311344600123,-5.40576090779376));
#87024=CARTESIAN_POINT('Ctrl Pts',(17.3194796934778,-20.5270740775325,-5.40612440227856));
#87025=CARTESIAN_POINT('Ctrl Pts',(17.3087651588247,-20.5173959242197,-5.40698472385317));
#87026=CARTESIAN_POINT('Ctrl Pts',(17.302600550861,-20.5117609983964,-5.40748082081452));
#87027=CARTESIAN_POINT('Ctrl Pts',(17.2834008785157,-20.4940013303064,-5.409029561869));
#87028=CARTESIAN_POINT('Ctrl Pts',(17.2704850889812,-20.4817483609572,-5.41007672649453));
#87029=CARTESIAN_POINT('Ctrl Pts',(17.240760746323,-20.4528283529638,-5.41250045665302));
#87030=CARTESIAN_POINT('Ctrl Pts',(17.2240739439454,-20.4360392792182,-5.41387168165147));
#87031=CARTESIAN_POINT('Ctrl Pts',(17.1673425623045,-20.377012502134,-5.41857620144597));
#87032=CARTESIAN_POINT('Ctrl Pts',(17.12875902556,-20.3334044712007,-5.42185082491593));
#87033=CARTESIAN_POINT('Ctrl Pts',(16.9876329321103,-20.1599902756054,-5.43425259867397));
#87034=CARTESIAN_POINT('Ctrl Pts',(16.8986446806635,-20.0199432858701,-5.44296640652934));
#87035=CARTESIAN_POINT('Ctrl Pts',(16.8014676033383,-19.8182737938716,-5.45550400786095));
#87036=CARTESIAN_POINT('Ctrl Pts',(16.7782692661977,-19.7645439925457,-5.45884882988038));
#87037=CARTESIAN_POINT('Ctrl Pts',(16.7541361330696,-19.7016049160798,-5.46284742918434));
#87038=CARTESIAN_POINT('Ctrl Pts',(16.7509973612087,-19.6932617554037,-5.46337908118137));
#87039=CARTESIAN_POINT('Ctrl Pts',(16.7470769047147,-19.6826376833051,-5.46405840735278));
#87040=CARTESIAN_POINT('Ctrl Pts',(16.7462462413202,-19.6803747699851,-5.46420323660037));
#87041=CARTESIAN_POINT('Ctrl Pts',(16.7454194499637,-19.6781104571738,-5.46434829365948));
#87042=CARTESIAN_POINT('Ctrl Pts',(16.7454193808392,-19.6781102678644,-5.2445270093495));
#87043=CARTESIAN_POINT('Ctrl Pts',(16.766587520815,-19.7360829405597,-5.24117479976143));
#87044=CARTESIAN_POINT('Ctrl Pts',(16.7902987735039,-19.7931519605987,-5.23782816634432));
#87045=CARTESIAN_POINT('Ctrl Pts',(16.8430672133903,-19.905935431496,-5.23098482781489));
#87046=CARTESIAN_POINT('Ctrl Pts',(16.8721437371547,-19.9615096429608,-5.22749298686203));
#87047=CARTESIAN_POINT('Ctrl Pts',(16.9191780065077,-20.0424431844216,-5.22210863640132));
#87048=CARTESIAN_POINT('Ctrl Pts',(16.9352983718101,-20.0688336636703,-5.2203028337863));
#87049=CARTESIAN_POINT('Ctrl Pts',(16.9558380198731,-20.1008602101464,-5.21803690875092));
#87050=CARTESIAN_POINT('Ctrl Pts',(16.9597163425328,-20.1068408156888,-5.21761051028791));
#87051=CARTESIAN_POINT('Ctrl Pts',(16.9658647109005,-20.1162178867387,-5.21693661732211));
#87052=CARTESIAN_POINT('Ctrl Pts',(16.9681145521302,-20.1196276258782,-5.21669045477579));
#87053=CARTESIAN_POINT('Ctrl Pts',(16.972352171989,-20.1260096745917,-5.21622756624743));
#87054=CARTESIAN_POINT('Ctrl Pts',(16.9743376167184,-20.1289834672395,-5.21601099645364));
#87055=CARTESIAN_POINT('Ctrl Pts',(16.9789053705132,-20.135787642143,-5.21551346204761));
#87056=CARTESIAN_POINT('Ctrl Pts',(16.9814926820624,-20.1396146006955,-5.21523216255377));
#87057=CARTESIAN_POINT('Ctrl Pts',(16.9895487918989,-20.1514469463241,-5.21435795785947));
#87058=CARTESIAN_POINT('Ctrl Pts',(16.9950599823428,-20.1594231243758,-5.21376228682459));
#87059=CARTESIAN_POINT('Ctrl Pts',(17.057328512786,-20.2482318608905,-5.20706090588122));
#87060=CARTESIAN_POINT('Ctrl Pts',(17.1196150892808,-20.3250262359966,-5.20062764184388));
#87061=CARTESIAN_POINT('Ctrl Pts',(17.3015407196668,-20.5197658748576,-5.18307319119865));
#87062=CARTESIAN_POINT('Ctrl Pts',(17.4302426709673,-20.6283241836233,-5.17192748815693));
#87063=CARTESIAN_POINT('Ctrl Pts',(17.5967906935513,-20.7379003696934,-5.15940133548108));
#87064=CARTESIAN_POINT('Ctrl Pts',(17.6235431142517,-20.7546565971322,-5.15743871609121));
#87065=CARTESIAN_POINT('Ctrl Pts',(17.663828306338,-20.7786516966939,-5.15455519329351));
#87066=CARTESIAN_POINT('Ctrl Pts',(17.6770802753552,-20.7863512722429,-5.15361788548105));
#87067=CARTESIAN_POINT('Ctrl Pts',(17.7013526902698,-20.8001035066598,-5.15192118619002));
#87068=CARTESIAN_POINT('Ctrl Pts',(17.7123455763817,-20.8062031407082,-5.1511601327394));
#87069=CARTESIAN_POINT('Ctrl Pts',(17.7297375582689,-20.815651816551,-5.14996744860832));
#87070=CARTESIAN_POINT('Ctrl Pts',(17.7361004400565,-20.8190665803556,-5.14953347771465));
#87071=CARTESIAN_POINT('Ctrl Pts',(17.7425268617856,-20.8224732072189,-5.14909753375409));
#87072=CARTESIAN_POINT('Ctrl Pts',(17.7425729938427,-20.8224976594978,-5.14909440445328));
#87073=CARTESIAN_POINT('Ctrl Pts',(17.7426668840093,-20.8225474214947,-5.14908803579943));
#87074=CARTESIAN_POINT('Ctrl Pts',(17.7427146432438,-20.8225727316523,-5.14908479637879));
#87075=CARTESIAN_POINT('Ctrl Pts',(17.7428118470268,-20.8226242403368,-5.14907820349224));
#87076=CARTESIAN_POINT('Ctrl Pts',(17.7428612926443,-20.8226504392621,-5.14907484996318));
#87077=CARTESIAN_POINT('Ctrl Pts',(17.7429619308434,-20.8227037576371,-5.14906802470699));
#87078=CARTESIAN_POINT('Ctrl Pts',(17.743013124214,-20.8227308773245,-5.1490645529364));
#87079=CARTESIAN_POINT('Ctrl Pts',(17.743117321722,-20.8227860704755,-5.14905748690083));
#87080=CARTESIAN_POINT('Ctrl Pts',(17.7431703266561,-20.8228141441677,-5.14905389259261));
#87081=CARTESIAN_POINT('Ctrl Pts',(17.7432782133937,-20.8228712797516,-5.14904657703208));
#87082=CARTESIAN_POINT('Ctrl Pts',(17.7433330959254,-20.8229003418214,-5.14904285574198));
#87083=CARTESIAN_POINT('Ctrl Pts',(17.7434448063247,-20.822959489785,-5.14903528161055));
#87084=CARTESIAN_POINT('Ctrl Pts',(17.743501634972,-20.8229895758691,-5.14903142872876));
#87085=CARTESIAN_POINT('Ctrl Pts',(17.7436173086067,-20.8230508087759,-5.14902358663774));
#87086=CARTESIAN_POINT('Ctrl Pts',(17.743676154301,-20.8230819557338,-5.14901959739391));
#87087=CARTESIAN_POINT('Ctrl Pts',(17.7437959355681,-20.823145348586,-5.14901147763401));
#87088=CARTESIAN_POINT('Ctrl Pts',(17.743856871888,-20.8231775946193,-5.1490073470816));
#87089=CARTESIAN_POINT('Ctrl Pts',(17.7439809106413,-20.8232432251852,-5.14899893958042));
#87090=CARTESIAN_POINT('Ctrl Pts',(17.7440440137244,-20.8232766097863,-5.14899466260297));
#87091=CARTESIAN_POINT('Ctrl Pts',(17.7441724650629,-20.8233445584779,-5.14898595693991));
#87092=CARTESIAN_POINT('Ctrl Pts',(17.7442378137746,-20.8233791225145,-5.14898152823984));
#87093=CARTESIAN_POINT('Ctrl Pts',(17.7443708402382,-20.8234494735391,-5.14897251349784));
#87094=CARTESIAN_POINT('Ctrl Pts',(17.7444385152684,-20.8234852587705,-5.1489679276581));
#87095=CARTESIAN_POINT('Ctrl Pts',(17.7445651243489,-20.8235521983873,-5.14895934878097));
#87096=CARTESIAN_POINT('Ctrl Pts',(17.7446240593062,-20.8235833543873,-5.14895535561881));
#87097=CARTESIAN_POINT('Ctrl Pts',(17.7447516802526,-20.8236508135633,-5.14894670903985));
#87098=CARTESIAN_POINT('Ctrl Pts',(17.7448203678529,-20.8236871163154,-5.14894205558503));
#87099=CARTESIAN_POINT('Ctrl Pts',(17.7449690906242,-20.8237657087608,-5.14893198048351));
#87100=CARTESIAN_POINT('Ctrl Pts',(17.7450491272721,-20.8238079975053,-5.14892655883323));
#87101=CARTESIAN_POINT('Ctrl Pts',(17.7452223979139,-20.823899533824,-5.14891482234299));
#87102=CARTESIAN_POINT('Ctrl Pts',(17.7453156337355,-20.8239487800211,-5.14890850750991));
#87103=CARTESIAN_POINT('Ctrl Pts',(17.7455174428088,-20.8240553542039,-5.14889484012024));
#87104=CARTESIAN_POINT('Ctrl Pts',(17.7456260178439,-20.8241126799613,-5.14888748761968));
#87105=CARTESIAN_POINT('Ctrl Pts',(17.7458609760584,-20.8242367077338,-5.14887157814187));
#87106=CARTESIAN_POINT('Ctrl Pts',(17.7459873606819,-20.824303406227,-5.14886302130579));
#87107=CARTESIAN_POINT('Ctrl Pts',(17.7462732878129,-20.8244542650139,-5.1488436647522));
#87108=CARTESIAN_POINT('Ctrl Pts',(17.7464328343613,-20.8245384177338,-5.14883286530239));
#87109=CARTESIAN_POINT('Ctrl Pts',(17.7523042955182,-20.8276343568583,-5.14843548898989));
#87110=CARTESIAN_POINT('Ctrl Pts',(17.7580299975305,-20.8306200394255,-5.14804983972057));
#87111=CARTESIAN_POINT('Ctrl Pts',(17.7712868466837,-20.8374558928897,-5.14716118240317));
#87112=CARTESIAN_POINT('Ctrl Pts',(17.7788276184615,-20.8412872371119,-5.14665884156104));
#87113=CARTESIAN_POINT('Ctrl Pts',(17.7991802191402,-20.8514750637132,-5.14531132592591));
#87114=CARTESIAN_POINT('Ctrl Pts',(17.8120339736784,-20.8577471504928,-5.14446909880766));
#87115=CARTESIAN_POINT('Ctrl Pts',(17.9304952245364,-20.9140721555885,-5.13678484369134));
#87116=CARTESIAN_POINT('Ctrl Pts',(18.0400204122868,-20.9554332195214,-5.1302596633236));
#87117=CARTESIAN_POINT('Ctrl Pts',(18.3090878571133,-21.0323099481725,-5.11494052932477));
#87118=CARTESIAN_POINT('Ctrl Pts',(18.4703872106178,-21.0588308344687,-5.1063302845368));
#87119=CARTESIAN_POINT('Ctrl Pts',(18.6653454802484,-21.0681325740938,-5.09512043216081));
#87120=CARTESIAN_POINT('Ctrl Pts',(18.6976103034938,-21.0689331704703,-5.09323780193555));
#87121=CARTESIAN_POINT('Ctrl Pts',(18.7371021885638,-21.069010050594,-5.09088632858741));
#87122=CARTESIAN_POINT('Ctrl Pts',(18.7443255076406,-21.0689871417563,-5.09045429818655));
#87123=CARTESIAN_POINT('Ctrl Pts',(18.755654446319,-21.0688932295526,-5.08977348372276));
#87124=CARTESIAN_POINT('Ctrl Pts',(18.7597602956431,-21.0688472469408,-5.08952607756281));
#87125=CARTESIAN_POINT('Ctrl Pts',(18.7674380497953,-21.0687389209107,-5.08906215353391));
#87126=CARTESIAN_POINT('Ctrl Pts',(18.7710099394135,-21.0686794812152,-5.08884579970967));
#87127=CARTESIAN_POINT('Ctrl Pts',(18.7791677093746,-21.0685230727996,-5.0883504847758));
#87128=CARTESIAN_POINT('Ctrl Pts',(18.7837534202208,-21.0684202408607,-5.08807119994708));
#87129=CARTESIAN_POINT('Ctrl Pts',(18.7978633104379,-21.0680579518034,-5.08720930749281));
#87130=CARTESIAN_POINT('Ctrl Pts',(18.8073859477431,-21.0677491043806,-5.08662404296766));
#87131=CARTESIAN_POINT('Ctrl Pts',(18.9364094484131,-21.0626924060164,-5.0786486255935));
#87132=CARTESIAN_POINT('Ctrl Pts',(19.0552876961205,-21.0478911239382,-5.07078168182625));
#87133=CARTESIAN_POINT('Ctrl Pts',(19.2788786405678,-21.0005779722052,-5.05568356514402));
#87134=CARTESIAN_POINT('Ctrl Pts',(19.3835995988073,-20.969817702043,-5.04848028866793));
#87135=CARTESIAN_POINT('Ctrl Pts',(19.555649795197,-20.9044887718609,-5.0366556435896));
#87136=CARTESIAN_POINT('Ctrl Pts',(19.6243473337719,-20.8741354173499,-5.03193410381107));
#87137=CARTESIAN_POINT('Ctrl Pts',(19.7080706811158,-20.8316885625777,-5.02618365802385));
#87138=CARTESIAN_POINT('Ctrl Pts',(19.724733240119,-20.8229597715777,-5.02503922898156));
#87139=CARTESIAN_POINT('Ctrl Pts',(19.7488019061056,-20.8099395234349,-5.02338571777478));
#87140=CARTESIAN_POINT('Ctrl Pts',(19.7563014684108,-20.8058235871889,-5.02287043898416));
#87141=CARTESIAN_POINT('Ctrl Pts',(19.7694107919308,-20.798525137866,-5.02196955171942));
#87142=CARTESIAN_POINT('Ctrl Pts',(19.7750313038117,-20.7953622592235,-5.02158324725687));
#87143=CARTESIAN_POINT('Ctrl Pts',(19.7859200928922,-20.7891690324963,-5.0208347014047));
#87144=CARTESIAN_POINT('Ctrl Pts',(19.7911899411518,-20.7861415881294,-5.02047236046221));
#87145=CARTESIAN_POINT('Ctrl Pts',(19.8037616307306,-20.7788471680432,-5.01960776213131));
#87146=CARTESIAN_POINT('Ctrl Pts',(19.8110511200237,-20.7745590278453,-5.01910627520533));
#87147=CARTESIAN_POINT('Ctrl Pts',(19.8372914704912,-20.7589103788829,-5.01730026903631));
#87148=CARTESIAN_POINT('Ctrl Pts',(19.8560903088074,-20.7472967941979,-5.01600497276923));
#87149=CARTESIAN_POINT('Ctrl Pts',(20.0311434415229,-20.6353281251975,-5.0039191883543));
#87150=CARTESIAN_POINT('Ctrl Pts',(20.1737332115338,-20.51512154638,-4.99398657516972));
#87151=CARTESIAN_POINT('Ctrl Pts',(20.3527449112073,-20.3186617741078,-4.97949715573226));
#87152=CARTESIAN_POINT('Ctrl Pts',(20.4032658492327,-20.2564726959617,-4.97509385549669));
#87153=CARTESIAN_POINT('Ctrl Pts',(20.4712245579586,-20.1623869300008,-4.96845482327554));
#87154=CARTESIAN_POINT('Ctrl Pts',(20.4915597685408,-20.1326646420797,-4.96636025103566));
#87155=CARTESIAN_POINT('Ctrl Pts',(20.5151824756617,-20.0961738130957,-4.96377331908926));
#87156=CARTESIAN_POINT('Ctrl Pts',(20.5192059329232,-20.0898859782372,-4.96332701873268));
#87157=CARTESIAN_POINT('Ctrl Pts',(20.5254190746871,-20.0800620535029,-4.96262868054329));
#87158=CARTESIAN_POINT('Ctrl Pts',(20.5276317819882,-20.0765404962315,-4.96237814003187));
#87159=CARTESIAN_POINT('Ctrl Pts',(20.5317223407796,-20.0699875228954,-4.96191149810616));
#87160=CARTESIAN_POINT('Ctrl Pts',(20.5336029155269,-20.0669578744101,-4.96169558017775));
#87161=CARTESIAN_POINT('Ctrl Pts',(20.5378451202764,-20.0600848931543,-4.96120536547796));
#87162=CARTESIAN_POINT('Ctrl Pts',(20.5402021141446,-20.0562387741653,-4.96093077104908));
#87163=CARTESIAN_POINT('Ctrl Pts',(20.5462565768015,-20.0462879142601,-4.96021969089374));
#87164=CARTESIAN_POINT('Ctrl Pts',(20.5499354633916,-20.0401720125702,-4.95978203778065));
#87165=CARTESIAN_POINT('Ctrl Pts',(20.5723483959082,-20.0024818317104,-4.95708172441507));
#87166=CARTESIAN_POINT('Ctrl Pts',(20.5902881748598,-19.9704452565031,-4.9547727560753));
#87167=CARTESIAN_POINT('Ctrl Pts',(20.6867179231991,-19.7872229537487,-4.94155886630472));
#87168=CARTESIAN_POINT('Ctrl Pts',(20.7475683369636,-19.627463017674,-4.93006552004989));
#87169=CARTESIAN_POINT('Ctrl Pts',(20.8116276936537,-19.3694572989089,-4.91278865567016));
#87170=CARTESIAN_POINT('Ctrl Pts',(20.8283436721875,-19.2753207036624,-4.90672137455992));
#87171=CARTESIAN_POINT('Ctrl Pts',(20.8409557520772,-19.1590859664567,-4.899539592127));
#87172=CARTESIAN_POINT('Ctrl Pts',(20.8429418766939,-19.1377723129207,-4.89823491464743));
#87173=CARTESIAN_POINT('Ctrl Pts',(20.8453044509209,-19.1074468728523,-4.89639535026117));
#87174=CARTESIAN_POINT('Ctrl Pts',(20.8459470550914,-19.098457690731,-4.89585214384242));
#87175=CARTESIAN_POINT('Ctrl Pts',(20.846956051088,-19.0829516109355,-4.89491864504823));
#87176=CARTESIAN_POINT('Ctrl Pts',(20.8473497378375,-19.0764366718422,-4.8945275010291));
#87177=CARTESIAN_POINT('Ctrl Pts',(20.8480455105541,-19.0639649575464,-4.89378073307569));
#87178=CARTESIAN_POINT('Ctrl Pts',(20.848352563931,-19.0580085323544,-4.89342495695304));
#87179=CARTESIAN_POINT('Ctrl Pts',(20.8490849375401,-19.0425293776329,-4.89250262481711));
#87180=CARTESIAN_POINT('Ctrl Pts',(20.8494711243088,-19.0330048637839,-4.89193729946376));
#87181=CARTESIAN_POINT('Ctrl Pts',(20.8505663600304,-19.0005851852725,-4.89002026297689));
#87182=CARTESIAN_POINT('Ctrl Pts',(20.8509681706519,-18.9776807583392,-4.88867816039968));
#87183=CARTESIAN_POINT('Ctrl Pts',(20.851229575852,-18.7781617034181,-4.87708341780581));
#87184=CARTESIAN_POINT('Ctrl Pts',(20.829361441651,-18.602217347693,-4.8675930135609));
#87185=CARTESIAN_POINT('Ctrl Pts',(20.7646769364804,-18.3474564016516,-4.85328877317991));
#87186=CARTESIAN_POINT('Ctrl Pts',(20.7383771435592,-18.2652746547204,-4.84856656756729));
#87187=CARTESIAN_POINT('Ctrl Pts',(20.6935117335157,-18.1498664672737,-4.84149553779059));
#87188=CARTESIAN_POINT('Ctrl Pts',(20.6789483711616,-18.1151727309016,-4.83930983139501));
#87189=CARTESIAN_POINT('Ctrl Pts',(20.6603586326572,-18.0739973946479,-4.83662183706322));
#87190=CARTESIAN_POINT('Ctrl Pts',(20.6572108943854,-18.0671237327015,-4.83616991467182));
#87191=CARTESIAN_POINT('Ctrl Pts',(20.6522658375635,-18.0564763281121,-4.83546467867024));
#87192=CARTESIAN_POINT('Ctrl Pts',(20.6504940094967,-18.0526907198608,-4.83521291061632));
#87193=CARTESIAN_POINT('Ctrl Pts',(20.6471906361685,-18.0456869791504,-4.83474516617037));
#87194=CARTESIAN_POINT('Ctrl Pts',(20.645662170996,-18.0424674577108,-4.83452938075615));
#87195=CARTESIAN_POINT('Ctrl Pts',(20.6421925719484,-18.0352065614768,-4.83404099001893));
#87196=CARTESIAN_POINT('Ctrl Pts',(20.6402467364802,-18.0311675074361,-4.83376809652335));
#87197=CARTESIAN_POINT('Ctrl Pts',(20.6344781796465,-18.0192901083543,-4.83296210202507));
#87198=CARTESIAN_POINT('Ctrl Pts',(20.6306198911076,-18.0114692796454,-4.83242686389385));
#87199=CARTESIAN_POINT('Ctrl Pts',(20.602809084369,-17.9559632462738,-4.82859708094487));
#87200=CARTESIAN_POINT('Ctrl Pts',(20.5771114118441,-17.9091788767439,-4.82520540835786));
#87201=CARTESIAN_POINT('Ctrl Pts',(20.5406308361121,-17.8483318014866,-4.82062024229572));
#87202=CARTESIAN_POINT('Ctrl Pts',(20.5313974494874,-17.8333575840296,-4.81947726885003));
#87203=CARTESIAN_POINT('Ctrl Pts',(20.4960067582514,-17.7775324149195,-4.81516533873204));
#87204=CARTESIAN_POINT('Ctrl Pts',(20.4686350687213,-17.7374701054467,-4.81196761509608));
#87205=CARTESIAN_POINT('Ctrl Pts',(20.3751395338638,-17.6102419595451,-4.80153801718461));
#87206=CARTESIAN_POINT('Ctrl Pts',(20.3036277226784,-17.5272453240315,-4.79430521460465));
#87207=CARTESIAN_POINT('Ctrl Pts',(20.1869268550375,-17.4113090083487,-4.78373155890178));
#87208=CARTESIAN_POINT('Ctrl Pts',(20.1463327209863,-17.3740132180049,-4.78024232864403));
#87209=CARTESIAN_POINT('Ctrl Pts',(20.0781788869175,-17.3161366592632,-4.77468462779284));
#87210=CARTESIAN_POINT('Ctrl Pts',(20.0514942741945,-17.2945698194499,-4.77257771618738));
#87211=CARTESIAN_POINT('Ctrl Pts',(20.0157271243577,-17.267072285667,-4.7698411375673));
#87212=CARTESIAN_POINT('Ctrl Pts',(20.0071077824445,-17.2605502062117,-4.76918812816274));
#87213=CARTESIAN_POINT('Ctrl Pts',(19.9929062908602,-17.2499742852708,-4.76812262252011));
#87214=CARTESIAN_POINT('Ctrl Pts',(19.9873536860634,-17.2458812696209,-4.76770859680545));
#87215=CARTESIAN_POINT('Ctrl Pts',(19.9765651572319,-17.2380097668315,-4.76690908102986));
#87216=CARTESIAN_POINT('Ctrl Pts',(19.9713317639453,-17.2342279555421,-4.76652346461807));
#87217=CARTESIAN_POINT('Ctrl Pts',(19.9592058925206,-17.2255495949808,-4.76563504748775));
#87218=CARTESIAN_POINT('Ctrl Pts',(19.9523011902965,-17.2206702529721,-4.76513291281909));
#87219=CARTESIAN_POINT('Ctrl Pts',(19.9336483469028,-17.2076557000433,-4.76378631531194));
#87220=CARTESIAN_POINT('Ctrl Pts',(19.9218466341522,-17.1995977683016,-4.76294479379496));
#87221=CARTESIAN_POINT('Ctrl Pts',(19.8128225415864,-17.1267661589018,-4.75526373942634));
#87222=CARTESIAN_POINT('Ctrl Pts',(19.7104705291067,-17.0700203989717,-4.74874081322979));
#87223=CARTESIAN_POINT('Ctrl Pts',(19.4555786734846,-16.9551277701251,-4.73343476879697));
#87224=CARTESIAN_POINT('Ctrl Pts',(19.3000127977038,-16.9055904261853,-4.72483473639969));
#87225=CARTESIAN_POINT('Ctrl Pts',(19.1084259258384,-16.8681211455224,-4.71362572691807));
#87226=CARTESIAN_POINT('Ctrl Pts',(19.0763835274958,-16.8626175283382,-4.71172963484275));
#87227=CARTESIAN_POINT('Ctrl Pts',(19.0370676437198,-16.8567932282768,-4.70936318384116));
#87228=CARTESIAN_POINT('Ctrl Pts',(19.0299008439791,-16.8557690728276,-4.70893019320783));
#87229=CARTESIAN_POINT('Ctrl Pts',(19.0186577398976,-16.8542212078362,-4.70824819892432));
#87230=CARTESIAN_POINT('Ctrl Pts',(19.0145848458527,-16.8536725628841,-4.70800058107788));
#87231=CARTESIAN_POINT('Ctrl Pts',(19.006969077476,-16.8526692396113,-4.70753647822845));
#87232=CARTESIAN_POINT('Ctrl Pts',(19.0034266412007,-16.8522116670656,-4.7073201585988));
#87233=CARTESIAN_POINT('Ctrl Pts',(18.9953378568608,-16.8511876536293,-4.70682520975616));
#87234=CARTESIAN_POINT('Ctrl Pts',(18.9907908333071,-16.8506270066669,-4.70654625867494));
#87235=CARTESIAN_POINT('Ctrl Pts',(18.9768095792498,-16.8489491776177,-4.70568639621303));
#87236=CARTESIAN_POINT('Ctrl Pts',(18.9673697710596,-16.8478807553937,-4.70510284568251));
#87237=CARTESIAN_POINT('Ctrl Pts',(18.8825212210361,-16.8388553648033,-4.69983276152158));
#87238=CARTESIAN_POINT('Ctrl Pts',(18.8067505566895,-16.8348926292283,-4.69495155210683));
#87239=CARTESIAN_POINT('Ctrl Pts',(18.5460078963864,-16.8352695263499,-4.67789874624842));
#87240=CARTESIAN_POINT('Ctrl Pts',(18.361868355271,-16.8597698922016,-4.66550126466966));
#87241=CARTESIAN_POINT('Ctrl Pts',(18.1318242036018,-16.9217512133695,-4.65047365238472));
#87242=CARTESIAN_POINT('Ctrl Pts',(18.0809343291922,-16.9375442785673,-4.64717204959153));
#87243=CARTESIAN_POINT('Ctrl Pts',(18.0188622064967,-16.9594076673491,-4.64317035359587));
#87244=CARTESIAN_POINT('Ctrl Pts',(18.0070709027976,-16.9636790082869,-4.64241129965314));
#87245=CARTESIAN_POINT('Ctrl Pts',(17.9884946156015,-16.9705955144042,-4.64121706777149));
#87246=CARTESIAN_POINT('Ctrl Pts',(17.9816842705339,-16.9731712911504,-4.6407795860556));
#87247=CARTESIAN_POINT('Ctrl Pts',(17.968942136332,-16.9780658508525,-4.63996165395531));
#87248=CARTESIAN_POINT('Ctrl Pts',(17.9630072758027,-16.9803763593079,-4.63958093167464));
#87249=CARTESIAN_POINT('Ctrl Pts',(17.9497500584347,-16.9856065580718,-4.63873098233023));
#87250=CARTESIAN_POINT('Ctrl Pts',(17.9424333762112,-16.9885404455456,-4.63826223907311));
#87251=CARTESIAN_POINT('Ctrl Pts',(17.9239381222289,-16.9960769714797,-4.63707811788252));
#87252=CARTESIAN_POINT('Ctrl Pts',(17.9127821794531,-17.0007346567875,-4.63636460548998));
#87253=CARTESIAN_POINT('Ctrl Pts',(17.8493619227521,-17.0278533142955,-4.6323115959134));
#87254=CARTESIAN_POINT('Ctrl Pts',(17.7979771221796,-17.05231923767,-4.62904120507475));
#87255=CARTESIAN_POINT('Ctrl Pts',(17.7238770941782,-17.0913383529907,-4.62431038061396));
#87256=CARTESIAN_POINT('Ctrl Pts',(17.7003571218875,-17.104300749741,-4.62280633893005));
#87257=CARTESIAN_POINT('Ctrl Pts',(17.5767140127845,-17.1755433072049,-4.61486879543645));
#87258=CARTESIAN_POINT('Ctrl Pts',(17.4812554902167,-17.2415201802596,-4.60864385438076));
#87259=CARTESIAN_POINT('Ctrl Pts',(17.3297826760241,-17.3657249882551,-4.59796497741273));
#87260=CARTESIAN_POINT('Ctrl Pts',(17.2708254324822,-17.4199383530675,-4.59356323234316));
#87261=CARTESIAN_POINT('Ctrl Pts',(17.1900057647959,-17.5031843092151,-4.58692631508331));
#87262=CARTESIAN_POINT('Ctrl Pts',(17.1655927582505,-17.529648608672,-4.58483219916652));
#87263=CARTESIAN_POINT('Ctrl Pts',(17.1369482556436,-17.5623344126283,-4.5822457734869));
#87264=CARTESIAN_POINT('Ctrl Pts',(17.1320583318607,-17.567974130664,-4.58179950201406));
#87265=CARTESIAN_POINT('Ctrl Pts',(17.1244905661914,-17.5767961317317,-4.58110119927231));
#87266=CARTESIAN_POINT('Ctrl Pts',(17.1217920478787,-17.5799607092899,-4.58085066507877));
#87267=CARTESIAN_POINT('Ctrl Pts',(17.1167971340474,-17.5858533730527,-4.58038402877505));
#87268=CARTESIAN_POINT('Ctrl Pts',(17.1144982999495,-17.5885793169779,-4.58016811011205));
#87269=CARTESIAN_POINT('Ctrl Pts',(17.1093069064879,-17.5947668948988,-4.57967788578656));
#87270=CARTESIAN_POINT('Ctrl Pts',(17.1064185323918,-17.5982319566796,-4.57940328241668));
#87271=CARTESIAN_POINT('Ctrl Pts',(17.0978965089804,-17.608522166995,-4.57858763518222));
#87272=CARTESIAN_POINT('Ctrl Pts',(17.0922946398145,-17.6153733411435,-4.57804437860432));
#87273=CARTESIAN_POINT('Ctrl Pts',(17.0511025652341,-17.6664015011843,-4.5739979557316));
#87274=CARTESIAN_POINT('Ctrl Pts',(17.0172610927965,-17.7119542016744,-4.57038509107753));
#87275=CARTESIAN_POINT('Ctrl Pts',(16.9504035834435,-17.8099384376311,-4.56270239707196));
#87276=CARTESIAN_POINT('Ctrl Pts',(16.9177751688064,-17.8625746658577,-4.55862477889792));
#87277=CARTESIAN_POINT('Ctrl Pts',(16.8338945754426,-18.0121591752151,-4.54729667055912));
#87278=CARTESIAN_POINT('Ctrl Pts',(16.7877886608281,-18.1117820025346,-4.54004809148312));
#87279=CARTESIAN_POINT('Ctrl Pts',(16.730316654,-18.2664292459557,-4.52944127177649));
#87280=CARTESIAN_POINT('Ctrl Pts',(16.7130722623162,-18.3190654686249,-4.5259347676104));
#87281=CARTESIAN_POINT('Ctrl Pts',(16.6884846752926,-18.4054279846415,-4.52035278549321));
#87282=CARTESIAN_POINT('Ctrl Pts',(16.6798675390215,-18.4387613002577,-4.51823844646771));
#87283=CARTESIAN_POINT('Ctrl Pts',(16.6696144564368,-18.4828321771183,-4.51549378007866));
#87284=CARTESIAN_POINT('Ctrl Pts',(16.6672430078921,-18.4933916039965,-4.51483993742794));
#87285=CARTESIAN_POINT('Ctrl Pts',(16.6634921046792,-18.5107136083516,-4.513773420653));
#87286=CARTESIAN_POINT('Ctrl Pts',(16.662064583693,-18.5174654715133,-4.51335921144638));
#87287=CARTESIAN_POINT('Ctrl Pts',(16.6593656414592,-18.5305466191723,-4.51255958175244));
#87288=CARTESIAN_POINT('Ctrl Pts',(16.6580901071835,-18.5368749680149,-4.51217403365391));
#87289=CARTESIAN_POINT('Ctrl Pts',(16.6552123725028,-18.5514973710976,-4.51128611711599));
#87290=CARTESIAN_POINT('Ctrl Pts',(16.6536308208215,-18.5597954137541,-4.51078441231691));
#87291=CARTESIAN_POINT('Ctrl Pts',(16.6495122711773,-18.5821305926305,-4.50943972839927));
#87292=CARTESIAN_POINT('Ctrl Pts',(16.6470673798474,-18.5961844243212,-4.50859967738244));
#87293=CARTESIAN_POINT('Ctrl Pts',(16.6261906884283,-18.7238153608063,-4.50102301408465));
#87294=CARTESIAN_POINT('Ctrl Pts',(16.6169037095493,-18.8387007765424,-4.49459281209416));
#87295=CARTESIAN_POINT('Ctrl Pts',(16.6171578058381,-19.1400360565124,-4.47808638902454));
#87296=CARTESIAN_POINT('Ctrl Pts',(16.641892451733,-19.3254189864425,-4.46831880430488));
#87297=CARTESIAN_POINT('Ctrl Pts',(16.6942562459763,-19.5188655759305,-4.45654184705318));
#87298=CARTESIAN_POINT('Ctrl Pts',(16.6981093691169,-19.5325518735356,-4.45569945744374));
#87299=CARTESIAN_POINT('Ctrl Pts',(16.7036607300232,-19.5515351289403,-4.454516918222));
#87300=CARTESIAN_POINT('Ctrl Pts',(16.7052425224844,-19.556866115661,-4.45418327316907));
#87301=CARTESIAN_POINT('Ctrl Pts',(16.707815642707,-19.5654144473005,-4.45364567221952));
#87302=CARTESIAN_POINT('Ctrl Pts',(16.7087936865895,-19.568635809576,-4.45344248887362));
#87303=CARTESIAN_POINT('Ctrl Pts',(16.7108530770338,-19.575361030647,-4.45301703730184));
#87304=CARTESIAN_POINT('Ctrl Pts',(16.7119358439041,-19.5788644146348,-4.4527946835878));
#87305=CARTESIAN_POINT('Ctrl Pts',(16.7145777265088,-19.5873343839741,-4.45225538864194));
#87306=CARTESIAN_POINT('Ctrl Pts',(16.7161460644909,-19.5922980491595,-4.45193791126062));
#87307=CARTESIAN_POINT('Ctrl Pts',(16.7216994278518,-19.6096509575292,-4.45082311577179));
#87308=CARTESIAN_POINT('Ctrl Pts',(16.7257802847427,-19.6220089032853,-4.45002045156157));
#87309=CARTESIAN_POINT('Ctrl Pts',(16.7349633439441,-19.6489799213563,-4.44825062879185));
#87310=CARTESIAN_POINT('Ctrl Pts',(16.7401119394289,-19.6635749106904,-4.44728123477407));
#87311=CARTESIAN_POINT('Ctrl Pts',(16.7454194481082,-19.6781104520924,-4.44630497675564));
#87312=CARTESIAN_POINT('Origin',(18.734,-18.952,0.));
#87313=CARTESIAN_POINT('',(16.7454194499637,-19.6781104571739,-3.64442446316901));
#87314=CARTESIAN_POINT('',(16.7454195176904,-19.6781106426554,-3.86819360277559));
#87315=CARTESIAN_POINT('',(16.7454194499637,-19.6781104571739,0.));
#87316=CARTESIAN_POINT('',(16.6170009086013,-18.9500541448918,-3.91098515934228));
#87317=CARTESIAN_POINT('Ctrl Pts',(16.7454195176904,-19.6781106426554,-3.8681936027756));
#87318=CARTESIAN_POINT('Ctrl Pts',(16.734008174336,-19.6468586910403,-3.870273038502));
#87319=CARTESIAN_POINT('Ctrl Pts',(16.7233298307746,-19.615327548151,-3.87233004139765));
#87320=CARTESIAN_POINT('Ctrl Pts',(16.7086937631107,-19.5684998312811,-3.87532604665878));
#87321=CARTESIAN_POINT('Ctrl Pts',(16.7041601155389,-19.5534045723869,-3.87628296738397));
#87322=CARTESIAN_POINT('Ctrl Pts',(16.6975600376633,-19.5305036165196,-3.87772163856799));
#87323=CARTESIAN_POINT('Ctrl Pts',(16.6953690625293,-19.5227346652623,-3.87820743698151));
#87324=CARTESIAN_POINT('Ctrl Pts',(16.6915244726395,-19.5087975367014,-3.87907495627617));
#87325=CARTESIAN_POINT('Ctrl Pts',(16.6898542406799,-19.5026340824737,-3.87945721338924));
#87326=CARTESIAN_POINT('Ctrl Pts',(16.6863713150496,-19.48954719446,-3.88026595964412));
#87327=CARTESIAN_POINT('Ctrl Pts',(16.6845657868444,-19.4826219233898,-3.88069221239667));
#87328=CARTESIAN_POINT('Ctrl Pts',(16.6809624123329,-19.468508053008,-3.88155749452863));
#87329=CARTESIAN_POINT('Ctrl Pts',(16.6791671198924,-19.4613189002392,-3.88199643667253));
#87330=CARTESIAN_POINT('Ctrl Pts',(16.6747876940001,-19.4433815981793,-3.88308721527926));
#87331=CARTESIAN_POINT('Ctrl Pts',(16.6722499111464,-19.4326222780991,-3.88373756698111));
#87332=CARTESIAN_POINT('Ctrl Pts',(16.6345655722156,-19.2670604299227,-3.89368677446346));
#87333=CARTESIAN_POINT('Ctrl Pts',(16.6168549648591,-19.1088091393682,-3.90236291901907));
#87334=CARTESIAN_POINT('Ctrl Pts',(16.6170008943788,-18.9500540301098,-3.91098518891322));
#87335=CARTESIAN_POINT('Ctrl Pts',(16.6170008942721,-18.9500541461424,-3.91098518261129));
#87336=CARTESIAN_POINT('Ctrl Pts',(16.6171322450268,-18.807150592994,-3.91874652655734));
#87337=CARTESIAN_POINT('Ctrl Pts',(16.6317328278981,-18.6646421589114,-3.92644236870034));
#87338=CARTESIAN_POINT('Ctrl Pts',(16.6625397877042,-18.5151512563269,-3.93541346054193));
#87339=CARTESIAN_POINT('Ctrl Pts',(16.664575528335,-18.5056071413232,-3.93599028140181));
#87340=CARTESIAN_POINT('Ctrl Pts',(16.6678824993184,-18.4906120954945,-3.93690343976338));
#87341=CARTESIAN_POINT('Ctrl Pts',(16.6691095116038,-18.485151422396,-3.93723742441503));
#87342=CARTESIAN_POINT('Ctrl Pts',(16.6714748371374,-18.474816591108,-3.9378723699048));
#87343=CARTESIAN_POINT('Ctrl Pts',(16.6726088136726,-18.4699414673269,-3.93817308878256));
#87344=CARTESIAN_POINT('Ctrl Pts',(16.674595110385,-18.4615372783009,-3.93869364629781));
#87345=CARTESIAN_POINT('Ctrl Pts',(16.6754392482024,-18.458006263442,-3.93891301525651));
#87346=CARTESIAN_POINT('Ctrl Pts',(16.6770954348792,-18.451156427771,-3.93933987301878));
#87347=CARTESIAN_POINT('Ctrl Pts',(16.6779064366034,-18.4478373952451,-3.93954729529748));
#87348=CARTESIAN_POINT('Ctrl Pts',(16.6801203214834,-18.4388712398872,-3.94010920647488));
#87349=CARTESIAN_POINT('Ctrl Pts',(16.6815384461344,-18.4332279630271,-3.94046456097539));
#87350=CARTESIAN_POINT('Ctrl Pts',(16.6869129222515,-18.4122078196071,-3.9417943072034));
#87351=CARTESIAN_POINT('Ctrl Pts',(16.6910188485155,-18.396870211435,-3.94277680076158));
#87352=CARTESIAN_POINT('Ctrl Pts',(16.7288591366647,-18.2616273684232,-3.95153979924237));
#87353=CARTESIAN_POINT('Ctrl Pts',(16.7729395884032,-18.1448813410546,-3.9597852839377));
#87354=CARTESIAN_POINT('Ctrl Pts',(16.8579487258966,-17.9685399638464,-3.97272134811439));
#87355=CARTESIAN_POINT('Ctrl Pts',(16.8920974708809,-17.9059799623512,-3.97741803945359));
#87356=CARTESIAN_POINT('Ctrl Pts',(16.9785938462516,-17.7649381327066,-3.9881673007431));
#87357=CARTESIAN_POINT('Ctrl Pts',(17.0331635959518,-17.6879880280514,-3.99415312531795));
#87358=CARTESIAN_POINT('Ctrl Pts',(17.1062835262746,-17.5982306195257,-4.0012670795449));
#87359=CARTESIAN_POINT('Ctrl Pts',(17.1201345938356,-17.5817478484369,-4.00257972924413));
#87360=CARTESIAN_POINT('Ctrl Pts',(17.1388624500493,-17.5601396928721,-4.00430954043226));
#87361=CARTESIAN_POINT('Ctrl Pts',(17.1435165540233,-17.5548238021679,-4.00473583704547));
#87362=CARTESIAN_POINT('Ctrl Pts',(17.1527803127122,-17.5443490630269,-4.00557734893524));
#87363=CARTESIAN_POINT('Ctrl Pts',(17.1573888137821,-17.5391893159067,-4.00599260474899));
#87364=CARTESIAN_POINT('Ctrl Pts',(17.1663419748287,-17.5292635858118,-4.00679289665995));
#87365=CARTESIAN_POINT('Ctrl Pts',(17.1706832766093,-17.524494689352,-4.00717806750306));
#87366=CARTESIAN_POINT('Ctrl Pts',(17.1807335285554,-17.5135553773427,-4.00806318794605));
#87367=CARTESIAN_POINT('Ctrl Pts',(17.1864575991969,-17.5073989531388,-4.00856248736963));
#87368=CARTESIAN_POINT('Ctrl Pts',(17.2018963169743,-17.4909911835884,-4.00989648076564));
#87369=CARTESIAN_POINT('Ctrl Pts',(17.2116772341861,-17.4808025733234,-4.01072831994755));
#87370=CARTESIAN_POINT('Ctrl Pts',(17.2965477374868,-17.3941471641969,-4.01783566812774));
#87371=CARTESIAN_POINT('Ctrl Pts',(17.3772462405688,-17.3233815535954,-4.02384812440951));
#87372=CARTESIAN_POINT('Ctrl Pts',(17.5573816024749,-17.1881415195211,-4.03622324500037));
#87373=CARTESIAN_POINT('Ctrl Pts',(17.6575569873246,-17.125282499965,-4.0425373436808));
#87374=CARTESIAN_POINT('Ctrl Pts',(17.813994760785,-17.0444766133498,-4.05224394602577));
#87375=CARTESIAN_POINT('Ctrl Pts',(17.8666116221682,-17.0199825161489,-4.05548746685995));
#87376=CARTESIAN_POINT('Ctrl Pts',(17.9472478314773,-16.9864032006027,-4.06052050006638));
#87377=CARTESIAN_POINT('Ctrl Pts',(17.9745618845269,-16.9756894713332,-4.06223582584919));
#87378=CARTESIAN_POINT('Ctrl Pts',(18.008642825369,-16.9631322905427,-4.06439932129622));
#87379=CARTESIAN_POINT('Ctrl Pts',(18.0152093184098,-16.9607497019533,-4.06481722455301));
#87380=CARTESIAN_POINT('Ctrl Pts',(18.0256345172692,-16.9570253053494,-4.06548255138208));
#87381=CARTESIAN_POINT('Ctrl Pts',(18.0294855890195,-16.9556620693148,-4.06572872160866));
#87382=CARTESIAN_POINT('Ctrl Pts',(18.0367147507666,-16.9531265505232,-4.06619161649731));
#87383=CARTESIAN_POINT('Ctrl Pts',(18.0400918730844,-16.9519516764481,-4.06640818492256));
#87384=CARTESIAN_POINT('Ctrl Pts',(18.0478386314845,-16.94927862282,-4.06690570542153));
#87385=CARTESIAN_POINT('Ctrl Pts',(18.0522101929812,-16.9477861899567,-4.06718699230683));
#87386=CARTESIAN_POINT('Ctrl Pts',(18.0657708824511,-16.9432061279213,-4.06806111948406));
#87387=CARTESIAN_POINT('Ctrl Pts',(18.0749762081527,-16.940167350991,-4.06865672491701));
#87388=CARTESIAN_POINT('Ctrl Pts',(18.1796792826009,-16.9063994384453,-4.07545386053984));
#87389=CARTESIAN_POINT('Ctrl Pts',(18.2772139628935,-16.8824360721901,-4.08199312037277));
#87390=CARTESIAN_POINT('Ctrl Pts',(18.5450619534881,-16.836487907142,-4.09990016848115));
#87391=CARTESIAN_POINT('Ctrl Pts',(18.7169864911213,-16.8281313771881,-4.11128276028443));
#87392=CARTESIAN_POINT('Ctrl Pts',(18.9166113850612,-16.8426962769045,-4.12381584691051));
#87393=CARTESIAN_POINT('Ctrl Pts',(18.945128888553,-16.8453595867472,-4.12559196290256));
#87394=CARTESIAN_POINT('Ctrl Pts',(18.9941479474101,-16.8509430329236,-4.12862088491591));
#87395=CARTESIAN_POINT('Ctrl Pts',(19.0146762946979,-16.8535867426123,-4.12988205114767));
#87396=CARTESIAN_POINT('Ctrl Pts',(19.044069221094,-16.8578111273345,-4.13167787983704));
#87397=CARTESIAN_POINT('Ctrl Pts',(19.0529671349999,-16.8591478965386,-4.13222020963701));
#87398=CARTESIAN_POINT('Ctrl Pts',(19.0683017755664,-16.8615517497336,-4.13315267460102));
#87399=CARTESIAN_POINT('Ctrl Pts',(19.074742536386,-16.8625919284245,-4.13354365643846));
#87400=CARTESIAN_POINT('Ctrl Pts',(19.0870648929699,-16.8646404743521,-4.13429043610972));
#87401=CARTESIAN_POINT('Ctrl Pts',(19.0929472255147,-16.8656439665343,-4.13464638458562));
#87402=CARTESIAN_POINT('Ctrl Pts',(19.1082309880289,-16.8683178403119,-4.13556985788703));
#87403=CARTESIAN_POINT('Ctrl Pts',(19.1176255667072,-16.870026992463,-4.13613614588535));
#87404=CARTESIAN_POINT('Ctrl Pts',(19.1496143481711,-16.8760705734365,-4.13806001300611));
#87405=CARTESIAN_POINT('Ctrl Pts',(19.1721498128972,-16.8807098047414,-4.13940788880554));
#87406=CARTESIAN_POINT('Ctrl Pts',(19.3656821144205,-16.9238510634833,-4.15092960843955));
#87407=CARTESIAN_POINT('Ctrl Pts',(19.5313586195494,-16.9830824437085,-4.16035463219325));
#87408=CARTESIAN_POINT('Ctrl Pts',(19.7656511569744,-17.1013299881168,-4.17463384428289));
#87409=CARTESIAN_POINT('Ctrl Pts',(19.8409462725443,-17.1453591533735,-4.17940431541763));
#87410=CARTESIAN_POINT('Ctrl Pts',(19.9447486876472,-17.2149882134013,-4.18654043939971));
#87411=CARTESIAN_POINT('Ctrl Pts',(19.9756161257974,-17.2369165246796,-4.18873952418397));
#87412=CARTESIAN_POINT('Ctrl Pts',(20.0119313908688,-17.2642092184526,-4.19144234737294));
#87413=CARTESIAN_POINT('Ctrl Pts',(20.0179613398528,-17.2687918619851,-4.19189507126423));
#87414=CARTESIAN_POINT('Ctrl Pts',(20.0272829893438,-17.2759553691502,-4.19260129036553));
#87415=CARTESIAN_POINT('Ctrl Pts',(20.0305919199036,-17.2785138519628,-4.19285323308809));
#87416=CARTESIAN_POINT('Ctrl Pts',(20.0367060305067,-17.2832703339385,-4.19332113606196));
#87417=CARTESIAN_POINT('Ctrl Pts',(20.0395132508583,-17.285465616447,-4.19353690427466));
#87418=CARTESIAN_POINT('Ctrl Pts',(20.0458366172362,-17.2904363521236,-4.19402504293687));
#87419=CARTESIAN_POINT('Ctrl Pts',(20.0493494845876,-17.2932158673269,-4.1942977002401));
#87420=CARTESIAN_POINT('Ctrl Pts',(20.0596613368682,-17.3014283524415,-4.19510236547206));
#87421=CARTESIAN_POINT('Ctrl Pts',(20.0664355750082,-17.3068920472293,-4.19563650022051));
#87422=CARTESIAN_POINT('Ctrl Pts',(20.1142609018017,-17.3459542652007,-4.19944561028889));
#87423=CARTESIAN_POINT('Ctrl Pts',(20.1540666107663,-17.3810407836746,-4.20281658411742));
#87424=CARTESIAN_POINT('Ctrl Pts',(20.2031407328953,-17.4276871496822,-4.20719151568062));
#87425=CARTESIAN_POINT('Ctrl Pts',(20.2136669332617,-17.4379029387482,-4.20814353803682));
#87426=CARTESIAN_POINT('Ctrl Pts',(20.3360684427876,-17.559190381806,-4.21936749038897));
#87427=CARTESIAN_POINT('Ctrl Pts',(20.4353191157243,-17.6823298164806,-4.22994489757944));
#87428=CARTESIAN_POINT('Ctrl Pts',(20.5622276355565,-17.8817357765132,-4.24516587916816));
#87429=CARTESIAN_POINT('Ctrl Pts',(20.6007489992924,-17.950435009645,-4.25012587390771));
#87430=CARTESIAN_POINT('Ctrl Pts',(20.64384402799,-18.0384589932508,-4.25613296943187));
#87431=CARTESIAN_POINT('Ctrl Pts',(20.6520921023564,-18.0559061947288,-4.25730750637208));
#87432=CARTESIAN_POINT('Ctrl Pts',(20.6636877172089,-18.0813284048728,-4.25899618570591));
#87433=CARTESIAN_POINT('Ctrl Pts',(20.6672265924911,-18.0892145932762,-4.25951690101564));
#87434=CARTESIAN_POINT('Ctrl Pts',(20.6733270889082,-18.1030352089832,-4.26042407650483));
#87435=CARTESIAN_POINT('Ctrl Pts',(20.6759099976907,-18.1089600623545,-4.26081126257151));
#87436=CARTESIAN_POINT('Ctrl Pts',(20.6808588888161,-18.1204555962414,-4.26155920738928));
#87437=CARTESIAN_POINT('Ctrl Pts',(20.6832281931125,-18.1260247699052,-4.26192007655446));
#87438=CARTESIAN_POINT('Ctrl Pts',(20.6888135317041,-18.1393112807005,-4.26277752508377));
#87439=CARTESIAN_POINT('Ctrl Pts',(20.6920078119325,-18.14703769674,-4.26327336314781));
#87440=CARTESIAN_POINT('Ctrl Pts',(20.7032505681011,-18.1746949086611,-4.26503849117533));
#87441=CARTESIAN_POINT('Ctrl Pts',(20.7110413474744,-18.1947295295945,-4.26629910137887));
#87442=CARTESIAN_POINT('Ctrl Pts',(20.7851008758058,-18.394117725974,-4.27867745431361));
#87443=CARTESIAN_POINT('Ctrl Pts',(20.8270869071199,-18.5815407342442,-4.28887559396418));
#87444=CARTESIAN_POINT('Ctrl Pts',(20.8448918862198,-18.7902653813083,-4.3003100274299));
#87445=CARTESIAN_POINT('Ctrl Pts',(20.8462087670023,-18.8084843100314,-4.30130965431589));
#87446=CARTESIAN_POINT('Ctrl Pts',(20.8510070428199,-18.8894227599961,-4.3057654180126));
#87447=CARTESIAN_POINT('Ctrl Pts',(20.8519314225192,-18.9522576988149,-4.30926363796277));
#87448=CARTESIAN_POINT('Ctrl Pts',(20.849139428657,-19.0459828194259,-4.31465688290954));
#87449=CARTESIAN_POINT('Ctrl Pts',(20.847538809199,-19.0769041523292,-4.3164648639232));
#87450=CARTESIAN_POINT('Ctrl Pts',(20.8447361385059,-19.1148889285882,-4.31873321641045));
#87451=CARTESIAN_POINT('Ctrl Pts',(20.8441754997984,-19.1219976653006,-4.31915977826667));
#87452=CARTESIAN_POINT('Ctrl Pts',(20.8432371618529,-19.1331747455037,-4.31983387210236));
#87453=CARTESIAN_POINT('Ctrl Pts',(20.8428835749369,-19.1372451350554,-4.32008007080195));
#87454=CARTESIAN_POINT('Ctrl Pts',(20.8421984554848,-19.1448757567485,-4.32054298910724));
#87455=CARTESIAN_POINT('Ctrl Pts',(20.8418696855567,-19.148436181193,-4.32075955229524));
#87456=CARTESIAN_POINT('Ctrl Pts',(20.8410955761397,-19.1565936563274,-4.32125702064421));
#87457=CARTESIAN_POINT('Ctrl Pts',(20.8406442130522,-19.1611900807342,-4.32153826035543));
#87458=CARTESIAN_POINT('Ctrl Pts',(20.8391992657662,-19.1754254890373,-4.32241209810004));
#87459=CARTESIAN_POINT('Ctrl Pts',(20.8381545555891,-19.1850589962553,-4.32300745868872));
#87460=CARTESIAN_POINT('Ctrl Pts',(20.8252845760865,-19.2965869227376,-4.32994383226708));
#87461=CARTESIAN_POINT('Ctrl Pts',(20.8061357762546,-19.397488101707,-4.33663765486278));
#87462=CARTESIAN_POINT('Ctrl Pts',(20.750556775186,-19.6062705190626,-4.35088033031));
#87463=CARTESIAN_POINT('Ctrl Pts',(20.7125840652424,-19.7134323845532,-4.35841699205622));
#87464=CARTESIAN_POINT('Ctrl Pts',(20.6406403324251,-19.8741305395517,-4.36979857556154));
#87465=CARTESIAN_POINT('Ctrl Pts',(20.6125598904463,-19.9300674802251,-4.37377946027903));
#87466=CARTESIAN_POINT('Ctrl Pts',(20.5637103667782,-20.0174862935634,-4.38002097853965));
#87467=CARTESIAN_POINT('Ctrl Pts',(20.5445088835228,-20.0497973103322,-4.38233289887023));
#87468=CARTESIAN_POINT('Ctrl Pts',(20.5184970648319,-20.0910276398573,-4.38529152193148));
#87469=CARTESIAN_POINT('Ctrl Pts',(20.5124629895278,-20.1004263760125,-4.38596656429279));
#87470=CARTESIAN_POINT('Ctrl Pts',(20.5025388203374,-20.1156185479077,-4.38705881912149));
#87471=CARTESIAN_POINT('Ctrl Pts',(20.4986940244358,-20.1214411853572,-4.38747771179553));
#87472=CARTESIAN_POINT('Ctrl Pts',(20.491251790785,-20.1325915753133,-4.38828045549983));
#87473=CARTESIAN_POINT('Ctrl Pts',(20.4876587406391,-20.1379221503561,-4.38866446542979));
#87474=CARTESIAN_POINT('Ctrl Pts',(20.4793861792415,-20.1500753435945,-4.3895405862509));
#87475=CARTESIAN_POINT('Ctrl Pts',(20.4746908245431,-20.1568870901183,-4.3900320903874));
#87476=CARTESIAN_POINT('Ctrl Pts',(20.4621325456825,-20.1748792767801,-4.39133163607962));
#87477=CARTESIAN_POINT('Ctrl Pts',(20.4542009880882,-20.1860115050842,-4.39213705283293));
#87478=CARTESIAN_POINT('Ctrl Pts',(20.3943245239867,-20.2683510604055,-4.39810626087974));
#87479=CARTESIAN_POINT('Ctrl Pts',(20.3380825057733,-20.3363336483364,-4.40309658136059));
#87480=CARTESIAN_POINT('Ctrl Pts',(20.1816587004008,-20.5030309732924,-4.41576490590478));
#87481=CARTESIAN_POINT('Ctrl Pts',(20.0756097215768,-20.5956223510044,-4.42323448884659));
#87482=CARTESIAN_POINT('Ctrl Pts',(19.9153729328119,-20.709613924748,-4.43408921663631));
#87483=CARTESIAN_POINT('Ctrl Pts',(19.8682928023491,-20.7403589316955,-4.43723642182673));
#87484=CARTESIAN_POINT('Ctrl Pts',(19.7953303218629,-20.7839651186258,-4.44213758532606));
#87485=CARTESIAN_POINT('Ctrl Pts',(19.7703143354167,-20.7982314753511,-4.44382210296991));
#87486=CARTESIAN_POINT('Ctrl Pts',(19.7388943896497,-20.8153101785417,-4.44595269780006));
#87487=CARTESIAN_POINT('Ctrl Pts',(19.7327558788901,-20.8186076843058,-4.44636964464494));
#87488=CARTESIAN_POINT('Ctrl Pts',(19.72302427072,-20.8237735954388,-4.44703191632725));
#87489=CARTESIAN_POINT('Ctrl Pts',(19.7194418366185,-20.8256621324733,-4.44727598481943));
#87490=CARTESIAN_POINT('Ctrl Pts',(19.7126803309807,-20.8292018119008,-4.44773719199818));
#87491=CARTESIAN_POINT('Ctrl Pts',(19.7095024796353,-20.8308551685444,-4.44795418794132));
#87492=CARTESIAN_POINT('Ctrl Pts',(19.7022340422686,-20.8346133438917,-4.44845102228282));
#87493=CARTESIAN_POINT('Ctrl Pts',(19.698140787309,-20.8367128971099,-4.44873118703654));
#87494=CARTESIAN_POINT('Ctrl Pts',(19.6872693707117,-20.8422444893672,-4.44947620041015));
#87495=CARTESIAN_POINT('Ctrl Pts',(19.6804795925781,-20.8456533736611,-4.44994243968108));
#87496=CARTESIAN_POINT('Ctrl Pts',(19.6331949195803,-20.8690753406769,-4.45319511001396));
#87497=CARTESIAN_POINT('Ctrl Pts',(19.5920899380711,-20.8878229155986,-4.45605162024559));
#87498=CARTESIAN_POINT('Ctrl Pts',(19.5448560577405,-20.9075658581413,-4.45934132248214));
#87499=CARTESIAN_POINT('Ctrl Pts',(19.5392817973918,-20.9098678702855,-4.45972966979974));
#87500=CARTESIAN_POINT('Ctrl Pts',(19.387857283215,-20.9716458467912,-4.47028091976166));
#87501=CARTESIAN_POINT('Ctrl Pts',(19.2358317032477,-21.0146844976715,-4.48087241961921));
#87502=CARTESIAN_POINT('Ctrl Pts',(18.9788228692162,-21.0573169277316,-4.49778522002511));
#87503=CARTESIAN_POINT('Ctrl Pts',(18.8761075578689,-21.0667360381832,-4.50430455008965));
#87504=CARTESIAN_POINT('Ctrl Pts',(18.7582955273138,-21.0689123718683,-4.51149026778077));
#87505=CARTESIAN_POINT('Ctrl Pts',(18.743487780466,-21.0690305293784,-4.51238839611533));
#87506=CARTESIAN_POINT('Ctrl Pts',(18.7209110693839,-21.0689737910691,-4.51375029557122));
#87507=CARTESIAN_POINT('Ctrl Pts',(18.7131425145082,-21.0689115049965,-4.51421757808872));
#87508=CARTESIAN_POINT('Ctrl Pts',(18.6990135877202,-21.0687204393229,-4.51506505369275));
#87509=CARTESIAN_POINT('Ctrl Pts',(18.6926531456789,-21.0686057512671,-4.51544568343714));
#87510=CARTESIAN_POINT('Ctrl Pts',(18.678927497251,-21.0682963642911,-4.51626521193568));
#87511=CARTESIAN_POINT('Ctrl Pts',(18.6715625782903,-21.0680918818769,-4.51670379935123));
#87512=CARTESIAN_POINT('Ctrl Pts',(18.6516069289948,-21.0674335512477,-4.51788912828049));
#87513=CARTESIAN_POINT('Ctrl Pts',(18.6390188136284,-21.0669057455247,-4.51863354890142));
#87514=CARTESIAN_POINT('Ctrl Pts',(18.5779506916085,-21.0637988820969,-4.52222981640151));
#87515=CARTESIAN_POINT('Ctrl Pts',(18.5295622256888,-21.0596649717319,-4.52503268904232));
#87516=CARTESIAN_POINT('Ctrl Pts',(18.4408419156624,-21.0490008166845,-4.53011153237708));
#87517=CARTESIAN_POINT('Ctrl Pts',(18.4004759823562,-21.0429605598862,-4.53239921614737));
#87518=CARTESIAN_POINT('Ctrl Pts',(18.2279684054836,-21.0120238199983,-4.54212598747358));
#87519=CARTESIAN_POINT('Ctrl Pts',(18.0981946245966,-20.9757383575991,-4.5492958221996));
#87520=CARTESIAN_POINT('Ctrl Pts',(17.9142085627967,-20.9048352846544,-4.56013213438817));
#87521=CARTESIAN_POINT('Ctrl Pts',(17.8567131831197,-20.8796904162313,-4.56362568054111));
#87522=CARTESIAN_POINT('Ctrl Pts',(17.7726608082376,-20.8383914751444,-4.56901240883797));
#87523=CARTESIAN_POINT('Ctrl Pts',(17.7452021849488,-20.8241443568537,-4.57081879404963));
#87524=CARTESIAN_POINT('Ctrl Pts',(17.7118128666005,-20.8058806015747,-4.57308536833362));
#87525=CARTESIAN_POINT('Ctrl Pts',(17.7055759492039,-20.8024280015811,-4.57351181055268));
#87526=CARTESIAN_POINT('Ctrl Pts',(17.6957925308526,-20.7969474086559,-4.57418575733014));
#87527=CARTESIAN_POINT('Ctrl Pts',(17.6922341929193,-20.7949405015486,-4.57443192957794));
#87528=CARTESIAN_POINT('Ctrl Pts',(17.6855723074812,-20.7911577309575,-4.57489482612849));
#87529=CARTESIAN_POINT('Ctrl Pts',(17.6824674425733,-20.7893842999692,-4.57511139418157));
#87530=CARTESIAN_POINT('Ctrl Pts',(17.6753618234,-20.7853018160686,-4.57560891097636));
#87531=CARTESIAN_POINT('Ctrl Pts',(17.6713641352488,-20.7829875356665,-4.57589019451129));
#87532=CARTESIAN_POINT('Ctrl Pts',(17.6590006636788,-20.7757761363526,-4.57676430113089));
#87533=CARTESIAN_POINT('Ctrl Pts',(17.6506610564777,-20.7708347076815,-4.57735988917283));
#87534=CARTESIAN_POINT('Ctrl Pts',(17.5601865997406,-20.7163833160125,-4.58388409806534));
#87535=CARTESIAN_POINT('Ctrl Pts',(17.4814819645658,-20.6614094318154,-4.59012186014501));
#87536=CARTESIAN_POINT('Ctrl Pts',(17.3080639734281,-20.5218573464661,-4.60477487783295));
#87537=CARTESIAN_POINT('Ctrl Pts',(17.2166671805567,-20.4337055043317,-4.61320498130753));
#87538=CARTESIAN_POINT('Ctrl Pts',(17.095548957908,-20.2938507932039,-4.62512680015848));
#87539=CARTESIAN_POINT('Ctrl Pts',(17.0592296961152,-20.2482371535256,-4.62882514592249));
#87540=CARTESIAN_POINT('Ctrl Pts',(17.003757511288,-20.1723384975902,-4.63467551855821));
#87541=CARTESIAN_POINT('Ctrl Pts',(16.9834109851594,-20.1429674486201,-4.63687122488612));
#87542=CARTESIAN_POINT('Ctrl Pts',(16.9578007277931,-20.1039225028554,-4.63970427586288));
#87543=CARTESIAN_POINT('Ctrl Pts',(16.9518562258008,-20.0947041972219,-4.6403670700672));
#87544=CARTESIAN_POINT('Ctrl Pts',(16.942271512775,-20.0795841864198,-4.64144445219298));
#87545=CARTESIAN_POINT('Ctrl Pts',(16.938588233542,-20.073710149745,-4.64186063588693));
#87546=CARTESIAN_POINT('Ctrl Pts',(16.9315377479591,-20.0623424453259,-4.64266153176346));
#87547=CARTESIAN_POINT('Ctrl Pts',(16.9281666400029,-20.0568512991635,-4.64304638494522));
#87548=CARTESIAN_POINT('Ctrl Pts',(16.9204737008798,-20.0441911157656,-4.64392910686645));
#87549=CARTESIAN_POINT('Ctrl Pts',(16.9161691975441,-20.0370116348093,-4.64442633698628));
#87550=CARTESIAN_POINT('Ctrl Pts',(16.9047787872845,-20.0177555081973,-4.64575115690543));
#87551=CARTESIAN_POINT('Ctrl Pts',(16.8977698422501,-20.005633650806,-4.64657595408827));
#87552=CARTESIAN_POINT('Ctrl Pts',(16.8410108978301,-19.9051831555845,-4.65333769699532));
#87553=CARTESIAN_POINT('Ctrl Pts',(16.7975407853625,-19.8134495866659,-4.65904106758851));
#87554=CARTESIAN_POINT('Ctrl Pts',(16.7555370085584,-19.7053822958017,-4.66542624492597));
#87555=CARTESIAN_POINT('Ctrl Pts',(16.7504072892657,-19.6917705270986,-4.66622485003499));
#87556=CARTESIAN_POINT('Ctrl Pts',(16.7454194642264,-19.6781104962347,-4.66702132639115));
#87557=CARTESIAN_POINT('',(16.6170000029932,-18.9521080403316,-3.68920542528284));
#87558=CARTESIAN_POINT('Ctrl Pts',(16.7454194481082,-19.6781104520924,-4.44630497675564));
#87559=CARTESIAN_POINT('Ctrl Pts',(16.7620249650105,-19.7235875663122,-4.44325057402068));
#87560=CARTESIAN_POINT('Ctrl Pts',(16.7801860421437,-19.7684827781901,-4.44012924995249));
#87561=CARTESIAN_POINT('Ctrl Pts',(16.8760920334208,-19.9839946047985,-4.42474708274802));
#87562=CARTESIAN_POINT('Ctrl Pts',(16.9747456752738,-20.1444254883296,-4.41214842939464));
#87563=CARTESIAN_POINT('Ctrl Pts',(17.128653912656,-20.3331925216919,-4.39674509008298));
#87564=CARTESIAN_POINT('Ctrl Pts',(17.1657754045437,-20.375201105423,-4.39326452551378));
#87565=CARTESIAN_POINT('Ctrl Pts',(17.21284242246,-20.4243835799468,-4.38912058938185));
#87566=CARTESIAN_POINT('Ctrl Pts',(17.2212358015587,-20.4330058310142,-4.38839135267341));
#87567=CARTESIAN_POINT('Ctrl Pts',(17.235236630318,-20.4471452193277,-4.38719075166915));
#87568=CARTESIAN_POINT('Ctrl Pts',(17.2408020475568,-20.4527034159365,-4.38671755806291));
#87569=CARTESIAN_POINT('Ctrl Pts',(17.2509287309101,-20.4627048535588,-4.3858637855344));
#87570=CARTESIAN_POINT('Ctrl Pts',(17.2554792912079,-20.4671587569661,-4.38548273811394));
#87571=CARTESIAN_POINT('Ctrl Pts',(17.2652853251112,-20.4766702597563,-4.38466714512043));
#87572=CARTESIAN_POINT('Ctrl Pts',(17.2705469922286,-20.4817213776718,-4.38423288508739));
#87573=CARTESIAN_POINT('Ctrl Pts',(17.2849676767021,-20.4954225059504,-4.38305175830486));
#87574=CARTESIAN_POINT('Ctrl Pts',(17.2941780608875,-20.5040182021533,-4.38230723643732));
#87575=CARTESIAN_POINT('Ctrl Pts',(17.3433130876007,-20.5490601604775,-4.37838616728606));
#87576=CARTESIAN_POINT('Ctrl Pts',(17.3845480436711,-20.5840512815691,-4.37527146400633));
#87577=CARTESIAN_POINT('Ctrl Pts',(17.5775416422962,-20.7355001608935,-4.36137520466466));
#87578=CARTESIAN_POINT('Ctrl Pts',(17.7432941334274,-20.832628873766,-4.35135116592928));
#87579=CARTESIAN_POINT('Ctrl Pts',(17.9351027651706,-20.9125422710085,-4.33980018923013));
#87580=CARTESIAN_POINT('Ctrl Pts',(17.9504505020504,-20.918726455928,-4.33887558096187));
#87581=CARTESIAN_POINT('Ctrl Pts',(18.0154338884566,-20.9440293422559,-4.33495322844088));
#87582=CARTESIAN_POINT('Ctrl Pts',(18.0657043284998,-20.9614521744423,-4.33190078574014));
#87583=CARTESIAN_POINT('Ctrl Pts',(18.1249045864624,-20.9795028121471,-4.32822792058208));
#87584=CARTESIAN_POINT('Ctrl Pts',(18.1332520097391,-20.9819918035192,-4.32770824988559));
#87585=CARTESIAN_POINT('Ctrl Pts',(18.145916551802,-20.985683096966,-4.32691678488499));
#87586=CARTESIAN_POINT('Ctrl Pts',(18.150222636011,-20.9869233571255,-4.32664714925575));
#87587=CARTESIAN_POINT('Ctrl Pts',(18.1579603156129,-20.9891254215144,-4.32616163403157));
#87588=CARTESIAN_POINT('Ctrl Pts',(18.1613904278957,-20.9900922399649,-4.3259460498309));
#87589=CARTESIAN_POINT('Ctrl Pts',(18.1688504954415,-20.9921746302837,-4.32547639755785));
#87590=CARTESIAN_POINT('Ctrl Pts',(18.1728812667483,-20.993286910518,-4.32522214765856));
#87591=CARTESIAN_POINT('Ctrl Pts',(18.1842164922373,-20.9963787243408,-4.32450582769488));
#87592=CARTESIAN_POINT('Ctrl Pts',(18.1915282185601,-20.9983310182653,-4.32404222560675));
#87593=CARTESIAN_POINT('Ctrl Pts',(18.2353814012106,-21.0097886496481,-4.32125312558855));
#87594=CARTESIAN_POINT('Ctrl Pts',(18.2721589538434,-21.0183535694137,-4.31887852524716));
#87595=CARTESIAN_POINT('Ctrl Pts',(18.3941219554129,-21.0433384188235,-4.31093049535583));
#87596=CARTESIAN_POINT('Ctrl Pts',(18.480085226604,-21.055506321663,-4.30521499128242));
#87597=CARTESIAN_POINT('Ctrl Pts',(18.7418155003558,-21.0762741531225,-4.28786816794678));
#87598=CARTESIAN_POINT('Ctrl Pts',(18.9181715414562,-21.0682953942103,-4.27632337986769));
#87599=CARTESIAN_POINT('Ctrl Pts',(19.1141662730203,-21.0347121598167,-4.26408405468157));
#87600=CARTESIAN_POINT('Ctrl Pts',(19.1367362652717,-21.0304657566607,-4.26268221875535));
#87601=CARTESIAN_POINT('Ctrl Pts',(19.1685805919242,-21.0239362326402,-4.26071444128344));
#87602=CARTESIAN_POINT('Ctrl Pts',(19.1779148194114,-21.0219564441732,-4.26013887635612));
#87603=CARTESIAN_POINT('Ctrl Pts',(19.1930631187195,-21.0186363119889,-4.25920672641979));
#87604=CARTESIAN_POINT('Ctrl Pts',(19.1988853939554,-21.0173343953508,-4.25884891550203));
#87605=CARTESIAN_POINT('Ctrl Pts',(19.2110640127712,-21.014557031007,-4.25810141160334));
#87606=CARTESIAN_POINT('Ctrl Pts',(19.2174192032255,-21.0130767704918,-4.25771187754814));
#87607=CARTESIAN_POINT('Ctrl Pts',(19.2325268295404,-21.0094841590691,-4.25678710379233));
#87608=CARTESIAN_POINT('Ctrl Pts',(19.2412728790618,-21.0073452981371,-4.25625272323438));
#87609=CARTESIAN_POINT('Ctrl Pts',(19.2707159145857,-20.999945569871,-4.25445688936834));
#87610=CARTESIAN_POINT('Ctrl Pts',(19.2913472933398,-20.9944272505649,-4.2532037472672));
#87611=CARTESIAN_POINT('Ctrl Pts',(19.4033611442526,-20.9626428990166,-4.24642344098933));
#87612=CARTESIAN_POINT('Ctrl Pts',(19.4929832452532,-20.9305541927143,-4.24109059784727));
#87613=CARTESIAN_POINT('Ctrl Pts',(19.7363294033509,-20.8244458185074,-4.22648539037809));
#87614=CARTESIAN_POINT('Ctrl Pts',(19.8836950237315,-20.7377511031314,-4.21752245334345));
#87615=CARTESIAN_POINT('Ctrl Pts',(20.0485720538876,-20.6118096533522,-4.20567638964912));
#87616=CARTESIAN_POINT('Ctrl Pts',(20.0774800446018,-20.5884989347384,-4.20352008597582));
#87617=CARTESIAN_POINT('Ctrl Pts',(20.1112138538258,-20.559800456601,-4.20088710488825));
#87618=CARTESIAN_POINT('Ctrl Pts',(20.1166459097343,-20.5551314956709,-4.20045940006467));
#87619=CARTESIAN_POINT('Ctrl Pts',(20.1254659567804,-20.5474723157477,-4.19975863629244));
#87620=CARTESIAN_POINT('Ctrl Pts',(20.1288683033351,-20.5444986137129,-4.19948677182063));
#87621=CARTESIAN_POINT('Ctrl Pts',(20.1349389239234,-20.5391584204026,-4.1989988741905));
#87622=CARTESIAN_POINT('Ctrl Pts',(20.1376107612441,-20.5367960596454,-4.19878314911413));
#87623=CARTESIAN_POINT('Ctrl Pts',(20.1433811896968,-20.5316679752768,-4.19831508456265));
#87624=CARTESIAN_POINT('Ctrl Pts',(20.1464775726212,-20.5288999195079,-4.19806257353658));
#87625=CARTESIAN_POINT('Ctrl Pts',(20.1550968878815,-20.5211488040496,-4.19735593901223));
#87626=CARTESIAN_POINT('Ctrl Pts',(20.1606016680782,-20.5161457767283,-4.1969003479617));
#87627=CARTESIAN_POINT('Ctrl Pts',(20.1922825458036,-20.487046205167,-4.19425399916898));
#87628=CARTESIAN_POINT('Ctrl Pts',(20.2178725897038,-20.4623233518713,-4.19201969066369));
#87629=CARTESIAN_POINT('Ctrl Pts',(20.2978747302283,-20.3810359527808,-4.18475220594539));
#87630=CARTESIAN_POINT('Ctrl Pts',(20.3497672864184,-20.322088442459,-4.17960070547353));
#87631=CARTESIAN_POINT('Ctrl Pts',(20.5145165245978,-20.1125302008044,-4.16200627179355));
#87632=CARTESIAN_POINT('Ctrl Pts',(20.6105698709585,-19.9497894169119,-4.14960150739656));
#87633=CARTESIAN_POINT('Ctrl Pts',(20.6923612119241,-19.7563553017386,-4.13668939720248));
#87634=CARTESIAN_POINT('Ctrl Pts',(20.7005561660786,-19.7361064912185,-4.13535699814116));
#87635=CARTESIAN_POINT('Ctrl Pts',(20.7114730724325,-19.7078836512959,-4.13352579551715));
#87636=CARTESIAN_POINT('Ctrl Pts',(20.7144628107774,-19.7000153105525,-4.13301802458144));
#87637=CARTESIAN_POINT('Ctrl Pts',(20.7195266532424,-19.6864451763178,-4.1321469695101));
#87638=CARTESIAN_POINT('Ctrl Pts',(20.7216233026992,-19.6807519574665,-4.13178293402681));
#87639=CARTESIAN_POINT('Ctrl Pts',(20.7259001015553,-19.6689830201237,-4.13103327451251));
#87640=CARTESIAN_POINT('Ctrl Pts',(20.7280769970745,-19.6629061800859,-4.1306477621981));
#87641=CARTESIAN_POINT('Ctrl Pts',(20.7330862708609,-19.6487186554223,-4.12975132131604));
#87642=CARTESIAN_POINT('Ctrl Pts',(20.7358971533161,-19.6406004603696,-4.12924111098228));
#87643=CARTESIAN_POINT('Ctrl Pts',(20.7447679816001,-19.6144668980911,-4.1276072886998));
#87644=CARTESIAN_POINT('Ctrl Pts',(20.7506348627138,-19.5963866325681,-4.12649005023018));
#87645=CARTESIAN_POINT('Ctrl Pts',(20.7788916609616,-19.5051380761807,-4.12091372228174));
#87646=CARTESIAN_POINT('Ctrl Pts',(20.7975478867688,-19.4308690300516,-4.1165776338642));
#87647=CARTESIAN_POINT('Ctrl Pts',(20.8330979413149,-19.2478875854949,-4.10621827960241));
#87648=CARTESIAN_POINT('Ctrl Pts',(20.8456243471935,-19.1385611644657,-4.10030441919368));
#87649=CARTESIAN_POINT('Ctrl Pts',(20.8521447173799,-18.9588373472105,-4.09050992506386));
#87650=CARTESIAN_POINT('Ctrl Pts',(20.851213659677,-18.8888416956147,-4.08667438613998));
#87651=CARTESIAN_POINT('Ctrl Pts',(20.8437800173909,-18.7707295118865,-4.079990300364));
#87652=CARTESIAN_POINT('Ctrl Pts',(20.8390856216013,-18.7225562039939,-4.0772036432575));
#87653=CARTESIAN_POINT('Ctrl Pts',(20.8317297155465,-18.6669050425509,-4.07387092628283));
#87654=CARTESIAN_POINT('Ctrl Pts',(20.8306717068757,-18.6592256095969,-4.07340851279436));
#87655=CARTESIAN_POINT('Ctrl Pts',(20.8289122270146,-18.6469535373236,-4.07266526833124));
#87656=CARTESIAN_POINT('Ctrl Pts',(20.8282377618997,-18.6423570136777,-4.07238592133023));
#87657=CARTESIAN_POINT('Ctrl Pts',(20.8270155818869,-18.6342144617413,-4.07188930190836));
#87658=CARTESIAN_POINT('Ctrl Pts',(20.8264739755968,-18.6306675621209,-4.07167237738703));
#87659=CARTESIAN_POINT('Ctrl Pts',(20.8253059220791,-18.6231463435563,-4.07121110022692));
#87660=CARTESIAN_POINT('Ctrl Pts',(20.8246771715133,-18.6191724906672,-4.07096662488864));
#87661=CARTESIAN_POINT('Ctrl Pts',(20.8229474752499,-18.6084387179358,-4.07030426686697));
#87662=CARTESIAN_POINT('Ctrl Pts',(20.8218250570873,-18.6016823770901,-4.06988519565038));
#87663=CARTESIAN_POINT('Ctrl Pts',(20.8160626691347,-18.5680075822169,-4.06778613343214));
#87664=CARTESIAN_POINT('Ctrl Pts',(20.8109350256201,-18.5411765947512,-4.06608069682155));
#87665=CARTESIAN_POINT('Ctrl Pts',(20.7945570946609,-18.4636454696931,-4.06107120426277));
#87666=CARTESIAN_POINT('Ctrl Pts',(20.7819589992993,-18.4132524724586,-4.05771361070909));
#87667=CARTESIAN_POINT('Ctrl Pts',(20.7289403618539,-18.2300883454846,-4.04524807277243));
#87668=CARTESIAN_POINT('Ctrl Pts',(20.6773432552504,-18.1009038521253,-4.03596899587365));
#87669=CARTESIAN_POINT('Ctrl Pts',(20.569549357182,-17.8929641326548,-4.02080822720532));
#87670=CARTESIAN_POINT('Ctrl Pts',(20.519939416656,-17.8112882985431,-4.01478011230963));
#87671=CARTESIAN_POINT('Ctrl Pts',(20.4570007153589,-17.7218985473351,-4.00810853364584));
#87672=CARTESIAN_POINT('Ctrl Pts',(20.448911262178,-17.7106457289853,-4.00726709431055));
#87673=CARTESIAN_POINT('Ctrl Pts',(20.4357839605596,-17.6927582752486,-4.00592677553272));
#87674=CARTESIAN_POINT('Ctrl Pts',(20.4308165426145,-17.686072674448,-4.00542518911778));
#87675=CARTESIAN_POINT('Ctrl Pts',(20.4219404330924,-17.6742725148358,-4.00453869918699));
#87676=CARTESIAN_POINT('Ctrl Pts',(20.4180476507871,-17.6691461722745,-4.00415318056397));
#87677=CARTESIAN_POINT('Ctrl Pts',(20.4099021345018,-17.6585204437411,-4.00335321393102));
#87678=CARTESIAN_POINT('Ctrl Pts',(20.4056455660315,-17.6530240840469,-4.00293892353501));
#87679=CARTESIAN_POINT('Ctrl Pts',(20.394551602368,-17.6388436745648,-4.00186872197426));
#87680=CARTESIAN_POINT('Ctrl Pts',(20.3876730806668,-17.630191954767,-4.00121445382104));
#87681=CARTESIAN_POINT('Ctrl Pts',(20.3577945671135,-17.5932094325945,-3.99841151329896));
#87682=CARTESIAN_POINT('Ctrl Pts',(20.3341311157104,-17.5654210264271,-3.9962897026237));
#87683=CARTESIAN_POINT('Ctrl Pts',(20.2696696035534,-17.4935721330939,-3.99074664840355));
#87684=CARTESIAN_POINT('Ctrl Pts',(20.2276947671477,-17.4506107377091,-3.98737330512819));
#87685=CARTESIAN_POINT('Ctrl Pts',(20.0623019353966,-17.2951427957841,-3.97479978143302));
#87686=CARTESIAN_POINT('Ctrl Pts',(19.9275687119945,-17.1955979680647,-3.96600993986647));
#87687=CARTESIAN_POINT('Ctrl Pts',(19.7353207702023,-17.0859877027177,-3.95357489166082));
#87688=CARTESIAN_POINT('Ctrl Pts',(19.6870720111133,-17.0608897845281,-3.95045730470458));
#87689=CARTESIAN_POINT('Ctrl Pts',(19.6299947532243,-17.0339387053974,-3.94671185286621));
#87690=CARTESIAN_POINT('Ctrl Pts',(19.6220509553461,-17.0302478769698,-3.94618931103442));
#87691=CARTESIAN_POINT('Ctrl Pts',(19.609999507613,-17.0247392398269,-3.94539432409029));
#87692=CARTESIAN_POINT('Ctrl Pts',(19.6059084887512,-17.0228849797303,-3.94512406649636));
#87693=CARTESIAN_POINT('Ctrl Pts',(19.5985603566445,-17.0195825772687,-3.94463788927883));
#87694=CARTESIAN_POINT('Ctrl Pts',(19.5953054615797,-17.0181296301149,-3.94442226859365));
#87695=CARTESIAN_POINT('Ctrl Pts',(19.5882316074162,-17.0149933457851,-3.94395307218101));
#87696=CARTESIAN_POINT('Ctrl Pts',(19.5844113861944,-17.0133131013187,-3.94369931754476));
#87697=CARTESIAN_POINT('Ctrl Pts',(19.5736835928425,-17.0086325152324,-3.94298576058678));
#87698=CARTESIAN_POINT('Ctrl Pts',(19.5667650228792,-17.0056577562786,-3.94252444476115));
#87699=CARTESIAN_POINT('Ctrl Pts',(19.5256520504304,-16.9882398576705,-3.93977708139106));
#87700=CARTESIAN_POINT('Ctrl Pts',(19.4911006580505,-16.9746621254663,-3.93744359018556));
#87701=CARTESIAN_POINT('Ctrl Pts',(19.3770088902704,-16.9332558136414,-3.92969917909186));
#87702=CARTESIAN_POINT('Ctrl Pts',(19.2961644863234,-16.9092670826731,-3.92415347546493));
#87703=CARTESIAN_POINT('Ctrl Pts',(19.0393710327426,-16.8494711556924,-3.90673697666808));
#87704=CARTESIAN_POINT('Ctrl Pts',(18.8601281991922,-16.8311521249555,-3.894940877039));
#87705=CARTESIAN_POINT('Ctrl Pts',(18.6580305910556,-16.836242012828,-3.88250129712701));
#87706=CARTESIAN_POINT('Ctrl Pts',(18.6353715300587,-16.8371771471193,-3.88111727139148));
#87707=CARTESIAN_POINT('Ctrl Pts',(18.6032524350829,-16.8390200625245,-3.87916992712946));
#87708=CARTESIAN_POINT('Ctrl Pts',(18.5937773638064,-16.8396276940846,-3.87859725428967));
#87709=CARTESIAN_POINT('Ctrl Pts',(18.5783640516092,-16.8407203068642,-3.87766850697028));
#87710=CARTESIAN_POINT('Ctrl Pts',(18.5724232827596,-16.8411666440355,-3.87731122428192));
#87711=CARTESIAN_POINT('Ctrl Pts',(18.5599720562675,-16.8421549931263,-3.87656380481841));
#87712=CARTESIAN_POINT('Ctrl Pts',(18.553462055257,-16.8427020764688,-3.87617383144571));
#87713=CARTESIAN_POINT('Ctrl Pts',(18.5379446023199,-16.8440784880761,-3.87524615496126));
#87714=CARTESIAN_POINT('Ctrl Pts',(18.5289396809375,-16.8449354331668,-3.87470932552772));
#87715=CARTESIAN_POINT('Ctrl Pts',(18.4984479531313,-16.8480344748612,-3.87289646801807));
#87716=CARTESIAN_POINT('Ctrl Pts',(18.4769896258437,-16.8505477839949,-3.87162897072507));
#87717=CARTESIAN_POINT('Ctrl Pts',(18.4259255110994,-16.8573225665961,-3.86863011270599));
#87718=CARTESIAN_POINT('Ctrl Pts',(18.3963638303689,-16.8618838834215,-3.86690807199501));
#87719=CARTESIAN_POINT('Ctrl Pts',(18.1995919624353,-16.8965293882015,-3.85551679721451));
#87720=CARTESIAN_POINT('Ctrl Pts',(18.0364365937917,-16.9460193165672,-3.84647866167954));
#87721=CARTESIAN_POINT('Ctrl Pts',(17.7897507366714,-17.0546305161837,-3.83172673165066));
#87722=CARTESIAN_POINT('Ctrl Pts',(17.7015159568439,-17.1011653010719,-3.82618577307012));
#87723=CARTESIAN_POINT('Ctrl Pts',(17.608846029193,-17.1587327608825,-3.81972237605751));
#87724=CARTESIAN_POINT('Ctrl Pts',(17.6008281332082,-17.1637885019697,-3.81915758100142));
#87725=CARTESIAN_POINT('Ctrl Pts',(17.5889725964014,-17.1713758458612,-3.81831372157468));
#87726=CARTESIAN_POINT('Ctrl Pts',(17.5851086877815,-17.1738664602762,-3.81803730486337));
#87727=CARTESIAN_POINT('Ctrl Pts',(17.578316151441,-17.178276204665,-3.81754886996845));
#87728=CARTESIAN_POINT('Ctrl Pts',(17.575384133208,-17.1801900403714,-3.81733720612231));
#87729=CARTESIAN_POINT('Ctrl Pts',(17.5724288914134,-17.1821295073329,-3.81712301687775));
#87730=CARTESIAN_POINT('Ctrl Pts',(17.5724009498372,-17.1821478457854,-3.81712099165907));
#87731=CARTESIAN_POINT('Ctrl Pts',(17.5723459289161,-17.1821839586603,-3.81711700356618));
#87732=CARTESIAN_POINT('Ctrl Pts',(17.5723188494479,-17.182201733106,-3.81711504068768));
#87733=CARTESIAN_POINT('Ctrl Pts',(17.5722654881884,-17.1822367601698,-3.81711117260956));
#87734=CARTESIAN_POINT('Ctrl Pts',(17.5722392061731,-17.1822540128834,-3.81710926739788));
#87735=CARTESIAN_POINT('Ctrl Pts',(17.5721873807932,-17.1822880350787,-3.8171055103868));
#87736=CARTESIAN_POINT('Ctrl Pts',(17.572161837702,-17.1823048043344,-3.81710365861098));
#87737=CARTESIAN_POINT('Ctrl Pts',(17.5721114379439,-17.1823378937641,-3.81710000469647));
#87738=CARTESIAN_POINT('Ctrl Pts',(17.5720865812556,-17.1823542139101,-3.81709820255963));
#87739=CARTESIAN_POINT('Ctrl Pts',(17.5720375071393,-17.1823864359629,-3.81709464451364));
#87740=CARTESIAN_POINT('Ctrl Pts',(17.5720132894813,-17.1824023379826,-3.8170928885909));
#87741=CARTESIAN_POINT('Ctrl Pts',(17.5719654496359,-17.1824337524244,-3.81708941980716));
#87742=CARTESIAN_POINT('Ctrl Pts',(17.5719418276003,-17.1824492647122,-3.81708770695996));
#87743=CARTESIAN_POINT('Ctrl Pts',(17.5718951398951,-17.1824799252673,-3.81708432150007));
#87744=CARTESIAN_POINT('Ctrl Pts',(17.5718720741621,-17.1824950735448,-3.81708264888532));
#87745=CARTESIAN_POINT('Ctrl Pts',(17.5718264632201,-17.1825250295254,-3.81707934129875));
#87746=CARTESIAN_POINT('Ctrl Pts',(17.5718039178955,-17.1825398372756,-3.81707770632088));
#87747=CARTESIAN_POINT('Ctrl Pts',(17.5717593143917,-17.1825691340396,-3.81707447159432));
#87748=CARTESIAN_POINT('Ctrl Pts',(17.5717372563277,-17.1825836229514,-3.81707287185612));
#87749=CARTESIAN_POINT('Ctrl Pts',(17.571693597412,-17.1826123016221,-3.81706970544434));
#87750=CARTESIAN_POINT('Ctrl Pts',(17.5716719964266,-17.1826264914448,-3.81706813876303));
#87751=CARTESIAN_POINT('Ctrl Pts',(17.5716292235413,-17.1826545903424,-3.8170650364308));
#87752=CARTESIAN_POINT('Ctrl Pts',(17.5716080516702,-17.1826684993761,-3.81706350078379));
#87753=CARTESIAN_POINT('Ctrl Pts',(17.5715661111001,-17.1826960536543,-3.81706045864593));
#87754=CARTESIAN_POINT('Ctrl Pts',(17.5715453425134,-17.1827096988043,-3.81705895216489));
#87755=CARTESIAN_POINT('Ctrl Pts',(17.5715041845188,-17.1827367410179,-3.81705596662349));
#87756=CARTESIAN_POINT('Ctrl Pts',(17.5714837952355,-17.1827501379807,-3.81705448757369));
#87757=CARTESIAN_POINT('Ctrl Pts',(17.5714433739743,-17.1827766981361,-3.81705155531261));
#87758=CARTESIAN_POINT('Ctrl Pts',(17.5714233418685,-17.1827898613951,-3.81705010209346));
#87759=CARTESIAN_POINT('Ctrl Pts',(17.5713836146902,-17.182815967412,-3.8170472200272));
#87760=CARTESIAN_POINT('Ctrl Pts',(17.5713639193692,-17.1828289103168,-3.81704579116339));
#87761=CARTESIAN_POINT('Ctrl Pts',(17.5713248456554,-17.1828545887894,-3.81704295635311));
#87762=CARTESIAN_POINT('Ctrl Pts',(17.5713054675604,-17.1828673241465,-3.81704155042945));
#87763=CARTESIAN_POINT('Ctrl Pts',(17.5712670110983,-17.182892598783,-3.81703876025517));
#87764=CARTESIAN_POINT('Ctrl Pts',(17.5712479325239,-17.1829051381847,-3.81703737599063));
#87765=CARTESIAN_POINT('Ctrl Pts',(17.571210058131,-17.1829300320241,-3.81703462790649));
#87766=CARTESIAN_POINT('Ctrl Pts',(17.571191262281,-17.1829423864695,-3.81703326408565));
#87767=CARTESIAN_POINT('Ctrl Pts',(17.5711539374934,-17.1829669207715,-3.81703055574244));
#87768=CARTESIAN_POINT('Ctrl Pts',(17.5711354086296,-17.1829791005676,-3.81702921122638));
#87769=CARTESIAN_POINT('Ctrl Pts',(17.5710986029691,-17.1830032952937,-3.81702654041839));
#87770=CARTESIAN_POINT('Ctrl Pts',(17.571080326287,-17.183015310137,-3.81702521413569));
#87771=CARTESIAN_POINT('Ctrl Pts',(17.5710440112129,-17.1830391839811,-3.81702257879733));
#87772=CARTESIAN_POINT('Ctrl Pts',(17.5710259728216,-17.1830510429709,-3.81702126974257));
#87773=CARTESIAN_POINT('Ctrl Pts',(17.5709901215587,-17.1830746134723,-3.81701866793588));
#87774=CARTESIAN_POINT('Ctrl Pts',(17.5709723085161,-17.1830863250864,-3.81701737517233));
#87775=CARTESIAN_POINT('Ctrl Pts',(17.5709368953272,-17.1831096091073,-3.81701480503424));
#87776=CARTESIAN_POINT('Ctrl Pts',(17.5709192952055,-17.1831211814885,-3.81701352766225));
#87777=CARTESIAN_POINT('Ctrl Pts',(17.5708842964279,-17.1831441945321,-3.81701098747986));
#87778=CARTESIAN_POINT('Ctrl Pts',(17.5708668976816,-17.1831556352452,-3.81700972466362));
#87779=CARTESIAN_POINT('Ctrl Pts',(17.5708322903486,-17.1831783923616,-3.81700721277418));
#87780=CARTESIAN_POINT('Ctrl Pts',(17.5708150818517,-17.1831897086978,-3.81700596370815));
#87781=CARTESIAN_POINT('Ctrl Pts',(17.5707808447363,-17.1832122237976,-3.81700347857482));
#87782=CARTESIAN_POINT('Ctrl Pts',(17.5707638160636,-17.1832234225894,-3.81700224250417));
#87783=CARTESIAN_POINT('Ctrl Pts',(17.5707299289429,-17.1832457089267,-3.81699978266266));
#87784=CARTESIAN_POINT('Ctrl Pts',(17.570713070344,-17.1832567965647,-3.81699855888138));
#87785=CARTESIAN_POINT('Ctrl Pts',(17.5706795133068,-17.1832788671927,-3.81699612288973));
#87786=CARTESIAN_POINT('Ctrl Pts',(17.5706628150943,-17.1832898500277,-3.81699491069625));
#87787=CARTESIAN_POINT('Ctrl Pts',(17.5706295705404,-17.1833117164827,-3.81699249727998));
#87788=CARTESIAN_POINT('Ctrl Pts',(17.5706130239909,-17.1833226002335,-3.81699129604257));
#87789=CARTESIAN_POINT('Ctrl Pts',(17.5705800738538,-17.1833442743622,-3.81698890389308));
#87790=CARTESIAN_POINT('Ctrl Pts',(17.5705636703381,-17.183355064687,-3.81698771298669));
#87791=CARTESIAN_POINT('Ctrl Pts',(17.5705309980389,-17.1833765573602,-3.81698534090316));
#87792=CARTESIAN_POINT('Ctrl Pts',(17.5705147293416,-17.1833872596467,-3.81698415973269));
#87793=CARTESIAN_POINT('Ctrl Pts',(17.5704823191981,-17.1834085811487,-3.81698180657913));
#87794=CARTESIAN_POINT('Ctrl Pts',(17.5704661776557,-17.1834192004225,-3.81698063458944));
#87795=CARTESIAN_POINT('Ctrl Pts',(17.5669362988661,-17.1857415229316,-3.81672433495168));
#87796=CARTESIAN_POINT('Ctrl Pts',(17.5634294937014,-17.1880636691209,-3.81646850327567));
#87797=CARTESIAN_POINT('Ctrl Pts',(17.5533063828614,-17.1948105007833,-3.81572654851427));
#87798=CARTESIAN_POINT('Ctrl Pts',(17.5467081660945,-17.199262013236,-3.81523867130936));
#87799=CARTESIAN_POINT('Ctrl Pts',(17.5025881638244,-17.2293911872176,-3.81194846959107));
#87800=CARTESIAN_POINT('Ctrl Pts',(17.4658797455245,-17.2562327482212,-3.80907482768865));
#87801=CARTESIAN_POINT('Ctrl Pts',(17.3337634640967,-17.3595270044605,-3.79830199559183));
#87802=CARTESIAN_POINT('Ctrl Pts',(17.2441660399604,-17.4430183007227,-3.79014604798256));
#87803=CARTESIAN_POINT('Ctrl Pts',(17.0664194241312,-17.6400024163357,-3.77268281766358));
#87804=CARTESIAN_POINT('Ctrl Pts',(16.9815645504966,-17.755694625775,-3.76347483767858));
#87805=CARTESIAN_POINT('Ctrl Pts',(16.901795132617,-17.8913786301542,-3.75386464117407));
#87806=CARTESIAN_POINT('Ctrl Pts',(16.8946919720711,-17.9037450881326,-3.75299843143494));
#87807=CARTESIAN_POINT('Ctrl Pts',(16.8835815735337,-17.9235487443865,-3.75162638229171));
#87808=CARTESIAN_POINT('Ctrl Pts',(16.8794930478376,-17.9309396169716,-3.75111762977918));
#87809=CARTESIAN_POINT('Ctrl Pts',(16.8723579144689,-17.9440221148231,-3.75022284251099));
#87810=CARTESIAN_POINT('Ctrl Pts',(16.8692929236678,-17.9497035405955,-3.74983615435323));
#87811=CARTESIAN_POINT('Ctrl Pts',(16.8630050086398,-17.9614878232486,-3.74903797206499));
#87812=CARTESIAN_POINT('Ctrl Pts',(16.8597858409595,-17.9675926057907,-3.74862661474516));
#87813=CARTESIAN_POINT('Ctrl Pts',(16.8515946320148,-17.98331212891,-3.74757279810752));
#87814=CARTESIAN_POINT('Ctrl Pts',(16.8466663336164,-17.9929495324342,-3.74693188645952));
#87815=CARTESIAN_POINT('Ctrl Pts',(16.8263674565624,-18.0334069568143,-3.74426243128477));
#87816=CARTESIAN_POINT('Ctrl Pts',(16.8116756834781,-18.0645629483003,-3.74225761538301));
#87817=CARTESIAN_POINT('Ctrl Pts',(16.7753496865696,-18.1467376515201,-3.73708924114751));
#87818=CARTESIAN_POINT('Ctrl Pts',(16.7549461831935,-18.1982724997234,-3.73396556158161));
#87819=CARTESIAN_POINT('Ctrl Pts',(16.7029519421197,-18.3463289493196,-3.72524230346317));
#87820=CARTESIAN_POINT('Ctrl Pts',(16.6762484995271,-18.4444043621154,-3.71976223416452));
#87821=CARTESIAN_POINT('Ctrl Pts',(16.6333350831171,-18.6629057711412,-3.70765435626206));
#87822=CARTESIAN_POINT('Ctrl Pts',(16.6202380799738,-18.7835631244798,-3.7010311353847));
#87823=CARTESIAN_POINT('Ctrl Pts',(16.6172719941243,-18.9161664058184,-3.69321455419334));
#87824=CARTESIAN_POINT('Ctrl Pts',(16.6171084528581,-18.9276758995571,-3.69253161992972));
#87825=CARTESIAN_POINT('Ctrl Pts',(16.6170172171078,-18.9427485195498,-3.69163072932575));
#87826=CARTESIAN_POINT('Ctrl Pts',(16.6170046457328,-18.9463111909341,-3.69141731051467));
#87827=CARTESIAN_POINT('Ctrl Pts',(16.6170002823543,-18.9506557850236,-3.69115645016002));
#87828=CARTESIAN_POINT('Ctrl Pts',(16.6169999302637,-18.9514377208871,-3.69110947701853));
#87829=CARTESIAN_POINT('Ctrl Pts',(16.6170000113955,-18.952219655168,-3.69106248006748));
#87830=CARTESIAN_POINT('Ctrl Pts',(16.6170000023184,-18.952099076172,-3.6890562790225));
#87831=CARTESIAN_POINT('Ctrl Pts',(16.6170002492315,-18.9573749670544,-3.68873698393553));
#87832=CARTESIAN_POINT('Ctrl Pts',(16.6170202186042,-18.9626508039048,-3.68841768884856));
#87833=CARTESIAN_POINT('Ctrl Pts',(16.6170599094811,-18.9679264921966,-3.68809839376159));
#87834=CARTESIAN_POINT('Ctrl Pts',(16.6176052825337,-19.0404171615204,-3.6837111151193));
#87835=CARTESIAN_POINT('Ctrl Pts',(16.6218794874508,-19.1130212561194,-3.67932383647701));
#87836=CARTESIAN_POINT('Ctrl Pts',(16.6298970753153,-19.1853235571758,-3.67493655783472));
#87837=CARTESIAN_POINT('Ctrl Pts',(16.6379042320844,-19.2575317910134,-3.67055498715875));
#87838=CARTESIAN_POINT('Ctrl Pts',(16.6496450608728,-19.3294385348527,-3.66617341648278));
#87839=CARTESIAN_POINT('Ctrl Pts',(16.6650821233697,-19.4006288218111,-3.66179184580682));
#87840=CARTESIAN_POINT('Ctrl Pts',(16.6805014135,-19.4717371488836,-3.65741531954138));
#87841=CARTESIAN_POINT('Ctrl Pts',(16.699608383448,-19.5421301883611,-3.65303879327594));
#87842=CARTESIAN_POINT('Ctrl Pts',(16.7223140614304,-19.6114002461034,-3.64866226701051));
#87843=CARTESIAN_POINT('Ctrl Pts',(16.729642720702,-19.633758382747,-3.64724966573001));
#87844=CARTESIAN_POINT('Ctrl Pts',(16.7373458912453,-19.6559996038205,-3.64583706444951));
#87845=CARTESIAN_POINT('Ctrl Pts',(16.7454194499637,-19.6781104571739,-3.64442446316901));
#87846=CARTESIAN_POINT('Origin',(18.734,-18.952,0.));
#87847=CARTESIAN_POINT('',(16.7477770216415,-19.6772709618372,-2.84456321880205));
#87848=CARTESIAN_POINT('',(16.7454194663415,-19.6781105020273,-3.06515442754877));
#87849=CARTESIAN_POINT('',(16.7454194499637,-19.6781104571739,0.));
#87850=CARTESIAN_POINT('Ctrl Pts',(16.7454194663415,-19.6781105020273,-3.06515442754877));
#87851=CARTESIAN_POINT('Ctrl Pts',(16.6929878119308,-19.5345172513892,-3.0751266878066));
#87852=CARTESIAN_POINT('Ctrl Pts',(16.6562469386904,-19.3856243212607,-3.08537383313559));
#87853=CARTESIAN_POINT('Ctrl Pts',(16.6280919228878,-19.1761614896224,-3.09899375775158));
#87854=CARTESIAN_POINT('Ctrl Pts',(16.6227108922585,-19.118001419432,-3.10269879205228));
#87855=CARTESIAN_POINT('Ctrl Pts',(16.6179213238052,-19.0239677147122,-3.10855848048557));
#87856=CARTESIAN_POINT('Ctrl Pts',(16.6170073709165,-18.988204547134,-3.11075698713295));
#87857=CARTESIAN_POINT('Ctrl Pts',(16.6169977968599,-18.9414601925486,-3.11359307297547));
#87858=CARTESIAN_POINT('Ctrl Pts',(16.6170808697555,-18.9304867773714,-3.11425616960496));
#87859=CARTESIAN_POINT('Ctrl Pts',(16.6173556709538,-18.9125808571879,-3.11533391888877));
#87860=CARTESIAN_POINT('Ctrl Pts',(16.6174961453154,-18.9056478761124,-3.11575016938094));
#87861=CARTESIAN_POINT('Ctrl Pts',(16.6178328490637,-18.8922747946274,-3.11655110933349));
#87862=CARTESIAN_POINT('Ctrl Pts',(16.618024418735,-18.8858346634128,-3.11693594024069));
#87863=CARTESIAN_POINT('Ctrl Pts',(16.61853734898,-18.8708874658032,-3.11782711206487));
#87864=CARTESIAN_POINT('Ctrl Pts',(16.6188806299516,-18.8623812255126,-3.11833276088101));
#87865=CARTESIAN_POINT('Ctrl Pts',(16.6201365679445,-18.8353134801192,-3.11993715889321));
#87866=CARTESIAN_POINT('Ctrl Pts',(16.6212423392476,-18.8167614964382,-3.12102985744796));
#87867=CARTESIAN_POINT('Ctrl Pts',(16.6243860783612,-18.7735960961615,-3.12355754005255));
#87868=CARTESIAN_POINT('Ctrl Pts',(16.6266107576611,-18.7489987587108,-3.12498672114695));
#87869=CARTESIAN_POINT('Ctrl Pts',(16.6359173801211,-18.66291851234,-3.12995531942993));
#87870=CARTESIAN_POINT('Ctrl Pts',(16.6452643311255,-18.6017101858117,-3.13342815559401));
#87871=CARTESIAN_POINT('Ctrl Pts',(16.6848813788517,-18.4015335039668,-3.14471623957749));
#87872=CARTESIAN_POINT('Ctrl Pts',(16.7264586032257,-18.2652135679846,-3.15226968718797));
#87873=CARTESIAN_POINT('Ctrl Pts',(16.8104679516061,-18.0646549989625,-3.16430895658454));
#87874=CARTESIAN_POINT('Ctrl Pts',(16.8432342673644,-17.9968251012381,-3.16856362054279));
#87875=CARTESIAN_POINT('Ctrl Pts',(16.884114370491,-17.9225816389908,-3.17358677619475));
#87876=CARTESIAN_POINT('Ctrl Pts',(16.888746046659,-17.9143021420719,-3.17415227598234));
#87877=CARTESIAN_POINT('Ctrl Pts',(16.895695423448,-17.9020732166805,-3.17499587372488));
#87878=CARTESIAN_POINT('Ctrl Pts',(16.8979706149233,-17.8980995954386,-3.17527130581961));
#87879=CARTESIAN_POINT('Ctrl Pts',(16.9020434262671,-17.8910396478425,-3.17576307170795));
#87880=CARTESIAN_POINT('Ctrl Pts',(16.9038359826543,-17.887950458731,-3.17597907716988));
#87881=CARTESIAN_POINT('Ctrl Pts',(16.9077088544987,-17.881314912925,-3.17644484920485));
#87882=CARTESIAN_POINT('Ctrl Pts',(16.9097916553653,-17.8777701277092,-3.17669477185982));
#87883=CARTESIAN_POINT('Ctrl Pts',(16.9155744490497,-17.8679935233195,-3.17738706504045));
#87884=CARTESIAN_POINT('Ctrl Pts',(16.9192960972128,-17.8617746712057,-3.17783080994103));
#87885=CARTESIAN_POINT('Ctrl Pts',(16.9399457462415,-17.8276679181774,-3.18028261422351));
#87886=CARTESIAN_POINT('Ctrl Pts',(16.9574837344677,-17.800156702163,-3.18232721188365));
#87887=CARTESIAN_POINT('Ctrl Pts',(17.0662163423063,-17.6379850569763,-3.19473510295501));
#87888=CARTESIAN_POINT('Ctrl Pts',(17.1720438904539,-17.5137960322802,-3.20568689909559));
#87889=CARTESIAN_POINT('Ctrl Pts',(17.3764983370213,-17.3233449860685,-3.22393799246217));
#87890=CARTESIAN_POINT('Ctrl Pts',(17.468403675699,-17.2509410167191,-3.23137711130904));
#87891=CARTESIAN_POINT('Ctrl Pts',(17.5777443369557,-17.1785947960711,-3.23938256626324));
#87892=CARTESIAN_POINT('Ctrl Pts',(17.589740723416,-17.170830749392,-3.24025052130294));
#87893=CARTESIAN_POINT('Ctrl Pts',(17.6089588009776,-17.1586671313934,-3.24162480304224));
#87894=CARTESIAN_POINT('Ctrl Pts',(17.6161296676214,-17.1541884413684,-3.24213405763158));
#87895=CARTESIAN_POINT('Ctrl Pts',(17.6288239824135,-17.1463653029585,-3.24302942879101));
#87896=CARTESIAN_POINT('Ctrl Pts',(17.6343362260577,-17.1430029644247,-3.24341620145572));
#87897=CARTESIAN_POINT('Ctrl Pts',(17.6457691797278,-17.1361007005969,-3.24421427160267));
#87898=CARTESIAN_POINT('Ctrl Pts',(17.6516919883643,-17.1325643860132,-3.24462543368715));
#87899=CARTESIAN_POINT('Ctrl Pts',(17.6669394887133,-17.1235614048688,-3.24567815661206));
#87900=CARTESIAN_POINT('Ctrl Pts',(17.6762890268787,-17.1181370457937,-3.24631817607566));
#87901=CARTESIAN_POINT('Ctrl Pts',(17.7154849584691,-17.0957960615331,-3.24897894475541));
#87902=CARTESIAN_POINT('Ctrl Pts',(17.7456997747558,-17.0795340290371,-3.25097616290278));
#87903=CARTESIAN_POINT('Ctrl Pts',(17.82544479408,-17.0390824939131,-3.25612052479162));
#87904=CARTESIAN_POINT('Ctrl Pts',(17.8755487072211,-17.0160795546499,-3.25922827383286));
#87905=CARTESIAN_POINT('Ctrl Pts',(18.0275780153212,-16.9533468909902,-3.26837301596235));
#87906=CARTESIAN_POINT('Ctrl Pts',(18.1317424557326,-16.9195303189857,-3.27426128077102));
#87907=CARTESIAN_POINT('Ctrl Pts',(18.2827866595482,-16.8831324711306,-3.28272016959122));
#87908=CARTESIAN_POINT('Ctrl Pts',(18.3278589516331,-16.8738143642051,-3.28523621522726));
#87909=CARTESIAN_POINT('Ctrl Pts',(18.3949986035987,-16.8622017907978,-3.28901509345587));
#87910=CARTESIAN_POINT('Ctrl Pts',(18.4168568565131,-16.85877314151,-3.2902502108794));
#87911=CARTESIAN_POINT('Ctrl Pts',(18.4897456676548,-16.8485077904856,-3.29439632997475));
#87912=CARTESIAN_POINT('Ctrl Pts',(18.5409676587761,-16.8431905624212,-3.29735450970791));
#87913=CARTESIAN_POINT('Ctrl Pts',(18.6009479067983,-16.8391675926959,-3.30092249109881));
#87914=CARTESIAN_POINT('Ctrl Pts',(18.6095713250742,-16.8386422120369,-3.30143796809104));
#87915=CARTESIAN_POINT('Ctrl Pts',(18.6226566738216,-16.8379253543991,-3.3022242864335));
#87916=CARTESIAN_POINT('Ctrl Pts',(18.6271165120674,-16.8376951821878,-3.30249301091803));
#87917=CARTESIAN_POINT('Ctrl Pts',(18.6351357098835,-16.8373067488918,-3.30297756050041));
#87918=CARTESIAN_POINT('Ctrl Pts',(18.6386947665896,-16.8371433603391,-3.30319309540201));
#87919=CARTESIAN_POINT('Ctrl Pts',(18.6464437549328,-16.8368072218244,-3.3036634342197));
#87920=CARTESIAN_POINT('Ctrl Pts',(18.650633738967,-16.8366379386228,-3.30391842431085));
#87921=CARTESIAN_POINT('Ctrl Pts',(18.6624420185504,-16.8361959995301,-3.30463888035573));
#87922=CARTESIAN_POINT('Ctrl Pts',(18.6700612330957,-16.8359520461146,-3.30510590624734));
#87923=CARTESIAN_POINT('Ctrl Pts',(18.7164060655347,-16.8347186983736,-3.30795908111973));
#87924=CARTESIAN_POINT('Ctrl Pts',(18.7551489221768,-16.8347513273524,-3.3103969363245));
#87925=CARTESIAN_POINT('Ctrl Pts',(18.8845066755227,-16.8384108649624,-3.31866554155012));
#87926=CARTESIAN_POINT('Ctrl Pts',(18.9748834288029,-16.8467958622333,-3.32465014995911));
#87927=CARTESIAN_POINT('Ctrl Pts',(19.1307356709466,-16.8714243693294,-3.33507705698038));
#87928=CARTESIAN_POINT('Ctrl Pts',(19.1964996704821,-16.8850484410584,-3.33951160002356));
#87929=CARTESIAN_POINT('Ctrl Pts',(19.3726439820372,-16.9303689816104,-3.35138287256244));
#87930=CARTESIAN_POINT('Ctrl Pts',(19.4812855501041,-16.9679561905951,-3.35868685817627));
#87931=CARTESIAN_POINT('Ctrl Pts',(19.5994118911057,-17.0199144461165,-3.36656624067994));
#87932=CARTESIAN_POINT('Ctrl Pts',(19.6124062894499,-17.0257874636828,-3.36743236959852));
#87933=CARTESIAN_POINT('Ctrl Pts',(19.6330013210753,-17.0353474606847,-3.36880431539321));
#87934=CARTESIAN_POINT('Ctrl Pts',(19.6406407670703,-17.038949333009,-3.36931304469359));
#87935=CARTESIAN_POINT('Ctrl Pts',(19.6540808180703,-17.0453846850884,-3.37020780503022));
#87936=CARTESIAN_POINT('Ctrl Pts',(19.6598903629394,-17.0481991416946,-3.37059448934382));
#87937=CARTESIAN_POINT('Ctrl Pts',(19.6718842896612,-17.054077532836,-3.37139267702283));
#87938=CARTESIAN_POINT('Ctrl Pts',(19.6780667506292,-17.0571452287181,-3.37180404351184));
#87939=CARTESIAN_POINT('Ctrl Pts',(19.6939072324825,-17.0651019419504,-3.37285791127719));
#87940=CARTESIAN_POINT('Ctrl Pts',(19.703543032472,-17.070034938896,-3.37349886458995));
#87941=CARTESIAN_POINT('Ctrl Pts',(19.7436809711016,-17.09097343798,-3.37616872547413));
#87942=CARTESIAN_POINT('Ctrl Pts',(19.7738290176351,-17.1076488021566,-3.37817389622223));
#87943=CARTESIAN_POINT('Ctrl Pts',(19.8513821287972,-17.1530510833581,-3.3833433927107));
#87944=CARTESIAN_POINT('Ctrl Pts',(19.8980906208808,-17.1829172694466,-3.38646781697899));
#87945=CARTESIAN_POINT('Ctrl Pts',(20.0335283536706,-17.2772079866678,-3.39564163839637));
#87946=CARTESIAN_POINT('Ctrl Pts',(20.1184839030284,-17.3467251308334,-3.40154240748138));
#87947=CARTESIAN_POINT('Ctrl Pts',(20.2426880705409,-17.4655844554062,-3.41090353833762));
#87948=CARTESIAN_POINT('Ctrl Pts',(20.2857763120577,-17.5106255145485,-3.41431590378571));
#87949=CARTESIAN_POINT('Ctrl Pts',(20.3638835055738,-17.5998403304361,-3.42096846609233));
#87950=CARTESIAN_POINT('Ctrl Pts',(20.3992470852891,-17.6436395828636,-3.42419095948977));
#87951=CARTESIAN_POINT('Ctrl Pts',(20.4380913535933,-17.6958791140761,-3.42805324093422));
#87952=CARTESIAN_POINT('Ctrl Pts',(20.4433174521482,-17.7030000548105,-3.42858011390047));
#87953=CARTESIAN_POINT('Ctrl Pts',(20.4511428251084,-17.7138037977882,-3.42938041123623));
#87954=CARTESIAN_POINT('Ctrl Pts',(20.4537752252823,-17.7174626410534,-3.42965160424009));
#87955=CARTESIAN_POINT('Ctrl Pts',(20.4584690464068,-17.7240308546511,-3.43013878125471));
#87956=CARTESIAN_POINT('Ctrl Pts',(20.4605348191367,-17.7269370497912,-3.4303544610024));
#87957=CARTESIAN_POINT('Ctrl Pts',(20.4649957846162,-17.7332465742658,-3.43082299075424));
#87958=CARTESIAN_POINT('Ctrl Pts',(20.4673882545621,-17.7366517053306,-3.43107601535337));
#87959=CARTESIAN_POINT('Ctrl Pts',(20.4740509429589,-17.7461942037436,-3.43178550586733));
#87960=CARTESIAN_POINT('Ctrl Pts',(20.4782986614297,-17.7523471009167,-3.43224345821451));
#87961=CARTESIAN_POINT('Ctrl Pts',(20.5029243404329,-17.788425139012,-3.43493088254932));
#87962=CARTESIAN_POINT('Ctrl Pts',(20.5225632323499,-17.8188446795622,-3.43720546748143));
#87963=CARTESIAN_POINT('Ctrl Pts',(20.5834759133727,-17.9187261157347,-3.44466425493239));
#87964=CARTESIAN_POINT('Ctrl Pts',(20.6215550303776,-17.990048678822,-3.4499732776991));
#87965=CARTESIAN_POINT('Ctrl Pts',(20.7329367226437,-18.2308858046551,-3.46749356162998));
#87966=CARTESIAN_POINT('Ctrl Pts',(20.7881878558816,-18.4078555835435,-3.47965047893929));
#87967=CARTESIAN_POINT('Ctrl Pts',(20.823580026576,-18.6116510388398,-3.4923723548316));
#87968=CARTESIAN_POINT('Ctrl Pts',(20.8270351885077,-18.6335885343617,-3.49372726039878));
#87969=CARTESIAN_POINT('Ctrl Pts',(20.8313312375178,-18.6639678923453,-3.49558414298879));
#87970=CARTESIAN_POINT('Ctrl Pts',(20.8324674404825,-18.6723659187258,-3.49609541872434));
#87971=CARTESIAN_POINT('Ctrl Pts',(20.8343324294193,-18.6868025691583,-3.49697089150009));
#87972=CARTESIAN_POINT('Ctrl Pts',(20.8350856687601,-18.6928378786808,-3.49733585726129));
#87973=CARTESIAN_POINT('Ctrl Pts',(20.8365837295177,-18.7052770325794,-3.498085985456));
#87974=CARTESIAN_POINT('Ctrl Pts',(20.8373253294104,-18.7116812067996,-3.49847104254219));
#87975=CARTESIAN_POINT('Ctrl Pts',(20.8389811831568,-18.7265756518922,-3.49936398498728));
#87976=CARTESIAN_POINT('Ctrl Pts',(20.8398733486626,-18.7350683038006,-3.49987116946171));
#87977=CARTESIAN_POINT('Ctrl Pts',(20.8425577771957,-18.7622007744136,-3.50148543461715));
#87978=CARTESIAN_POINT('Ctrl Pts',(20.8441541585666,-18.7808593962848,-3.50258635738023));
#87979=CARTESIAN_POINT('Ctrl Pts',(20.8472984892433,-18.8244061696206,-3.50513586265569));
#87980=CARTESIAN_POINT('Ctrl Pts',(20.8486547298727,-18.8493056134864,-3.50657850053666));
#87981=CARTESIAN_POINT('Ctrl Pts',(20.8518764099744,-18.9369379110832,-3.51160921368987));
#87982=CARTESIAN_POINT('Ctrl Pts',(20.8513923696498,-18.9997262945109,-3.51512876620645));
#87983=CARTESIAN_POINT('Ctrl Pts',(20.8429272825505,-19.1618232678387,-3.52410228098342));
#87984=CARTESIAN_POINT('Ctrl Pts',(20.8307287512515,-19.2607541322247,-3.52946528721185));
#87985=CARTESIAN_POINT('Ctrl Pts',(20.7977315712765,-19.4294192163148,-3.5388261351708));
#87986=CARTESIAN_POINT('Ctrl Pts',(20.7802235413917,-19.4996175919569,-3.54279176801564));
#87987=CARTESIAN_POINT('Ctrl Pts',(20.745811363295,-19.6126083085533,-3.54947847157277));
#87988=CARTESIAN_POINT('Ctrl Pts',(20.7310441134659,-19.6559903652426,-3.55212194170258));
#87989=CARTESIAN_POINT('Ctrl Pts',(20.7121911226638,-19.7059940873989,-3.55529550344302));
#87990=CARTESIAN_POINT('Ctrl Pts',(20.7094611695431,-19.7131178392859,-3.55575067104188));
#87991=CARTESIAN_POINT('Ctrl Pts',(20.705020057454,-19.7245219619774,-3.55648446637239));
#87992=CARTESIAN_POINT('Ctrl Pts',(20.7033332897576,-19.7288118443712,-3.55676166916453));
#87993=CARTESIAN_POINT('Ctrl Pts',(20.7003103909126,-19.7364267253825,-3.55725586860305));
#87994=CARTESIAN_POINT('Ctrl Pts',(20.6989798136129,-19.7397538783283,-3.55747252923452));
#87995=CARTESIAN_POINT('Ctrl Pts',(20.6961295307234,-19.7468289504677,-3.55793482807171));
#87996=CARTESIAN_POINT('Ctrl Pts',(20.6946075546993,-19.7505758396426,-3.55818059702074));
#87997=CARTESIAN_POINT('Ctrl Pts',(20.6904434649384,-19.7607435791892,-3.55885003843898));
#87998=CARTESIAN_POINT('Ctrl Pts',(20.6877805113774,-19.7671557634323,-3.55927494237368));
#87999=CARTESIAN_POINT('Ctrl Pts',(20.6740339861199,-19.7998019850031,-3.56145175709801));
#88000=CARTESIAN_POINT('Ctrl Pts',(20.6624539592293,-19.8258221875199,-3.56323137952491));
#88001=CARTESIAN_POINT('Ctrl Pts',(20.6268633544729,-19.9016383523107,-3.56853243317356));
#88002=CARTESIAN_POINT('Ctrl Pts',(20.6014240454178,-19.9507348377574,-3.57211444958112));
#88003=CARTESIAN_POINT('Ctrl Pts',(20.5047213131587,-20.1207255460475,-3.58492306465189));
#88004=CARTESIAN_POINT('Ctrl Pts',(20.4233892784576,-20.2354883471711,-3.59429839358696));
#88005=CARTESIAN_POINT('Ctrl Pts',(20.2725645290536,-20.4088863033187,-3.6091303704621));
#88006=CARTESIAN_POINT('Ctrl Pts',(20.2096010753973,-20.4726260587315,-3.61476942843988));
#88007=CARTESIAN_POINT('Ctrl Pts',(20.1325547703226,-20.5413147378914,-3.62106716907435));
#88008=CARTESIAN_POINT('Ctrl Pts',(20.1222376773322,-20.55033442895,-3.62189908283746));
#88009=CARTESIAN_POINT('Ctrl Pts',(20.1055446783812,-20.5646446632317,-3.62322717749021));
#88010=CARTESIAN_POINT('Ctrl Pts',(20.099224162141,-20.5699989508024,-3.62372598789833));
#88011=CARTESIAN_POINT('Ctrl Pts',(20.0879418613428,-20.5794433261227,-3.6246092828644));
#88012=CARTESIAN_POINT('Ctrl Pts',(20.0829925918295,-20.5835481397254,-3.62499436775926));
#88013=CARTESIAN_POINT('Ctrl Pts',(20.0726375354417,-20.5920570616006,-3.62579512269359));
#88014=CARTESIAN_POINT('Ctrl Pts',(20.0672285306139,-20.596457145548,-3.62621062672019));
#88015=CARTESIAN_POINT('Ctrl Pts',(20.0531161477256,-20.6078218017888,-3.62728758829109));
#88016=CARTESIAN_POINT('Ctrl Pts',(20.0443792552369,-20.6147445579825,-3.6279473628926));
#88017=CARTESIAN_POINT('Ctrl Pts',(20.006115289842,-20.6445744417216,-3.63080729705498));
#88018=CARTESIAN_POINT('Ctrl Pts',(19.976038190382,-20.6667673127824,-3.63297919132641));
#88019=CARTESIAN_POINT('Ctrl Pts',(19.8944835086819,-20.7236714762194,-3.63868555838165));
#88020=CARTESIAN_POINT('Ctrl Pts',(19.842039305766,-20.7569353336805,-3.64216835312113));
#88021=CARTESIAN_POINT('Ctrl Pts',(19.7066140021285,-20.8347010921331,-3.65080589663979));
#88022=CARTESIAN_POINT('Ctrl Pts',(19.6219877195809,-20.8760633537659,-3.65588386369722));
#88023=CARTESIAN_POINT('Ctrl Pts',(19.4209112203347,-20.9582410457526,-3.66770034735924));
#88024=CARTESIAN_POINT('Ctrl Pts',(19.3031012787516,-20.9947836263324,-3.67444428234046));
#88025=CARTESIAN_POINT('Ctrl Pts',(19.1735781040909,-21.0228812693016,-3.68230000478838));
#88026=CARTESIAN_POINT('Ctrl Pts',(19.1643381602837,-21.0248210731927,-3.68286282137508));
#88027=CARTESIAN_POINT('Ctrl Pts',(19.1506071096526,-21.0276079592811,-3.68370317429446));
#88028=CARTESIAN_POINT('Ctrl Pts',(19.146125590979,-21.0285024393932,-3.68397807446866));
#88029=CARTESIAN_POINT('Ctrl Pts',(19.1381372401925,-21.030069980058,-3.68446925961072));
#88030=CARTESIAN_POINT('Ctrl Pts',(19.1346315676104,-21.0307486855619,-3.68468521926273));
#88031=CARTESIAN_POINT('Ctrl Pts',(19.1270798011099,-21.0321909102926,-3.6851513149039));
#88032=CARTESIAN_POINT('Ctrl Pts',(19.1230332507196,-21.0329514848914,-3.68540160920954));
#88033=CARTESIAN_POINT('Ctrl Pts',(19.1118310092363,-21.0350232000108,-3.68609595633987));
#88034=CARTESIAN_POINT('Ctrl Pts',(19.1046708183316,-21.0363092534995,-3.68654139671802));
#88035=CARTESIAN_POINT('Ctrl Pts',(19.0661909303955,-21.0430161400399,-3.68894348415039));
#88036=CARTESIAN_POINT('Ctrl Pts',(19.034760551346,-21.0477676758665,-3.69093469815174));
#88037=CARTESIAN_POINT('Ctrl Pts',(18.8413360407889,-21.0725685285995,-3.70331903437222));
#88038=CARTESIAN_POINT('Ctrl Pts',(18.677582087001,-21.0745335751913,-3.71431231851128));
#88039=CARTESIAN_POINT('Ctrl Pts',(18.3988799792387,-21.0455775596452,-3.73261605511738));
#88040=CARTESIAN_POINT('Ctrl Pts',(18.2837177635398,-21.0238653845563,-3.7400678636223));
#88041=CARTESIAN_POINT('Ctrl Pts',(18.157146194391,-20.9889420546946,-3.74808512920842));
#88042=CARTESIAN_POINT('Ctrl Pts',(18.1434080704915,-20.9850013368793,-3.7489532384406));
#88043=CARTESIAN_POINT('Ctrl Pts',(18.1216072735578,-20.9785082378315,-3.75032771740004));
#88044=CARTESIAN_POINT('Ctrl Pts',(18.1135183529135,-20.9760461996375,-3.75083701632456));
#88045=CARTESIAN_POINT('Ctrl Pts',(18.0992786498256,-20.9716186516714,-3.75173243905438));
#88046=CARTESIAN_POINT('Ctrl Pts',(18.0931217435938,-20.9696733512748,-3.75211921919221));
#88047=CARTESIAN_POINT('Ctrl Pts',(18.0804060419492,-20.9655916958743,-3.75291727950037));
#88048=CARTESIAN_POINT('Ctrl Pts',(18.0738485877795,-20.963451390009,-3.7533284243975));
#88049=CARTESIAN_POINT('Ctrl Pts',(18.0570440857223,-20.9578754926461,-3.75438105103633));
#88050=CARTESIAN_POINT('Ctrl Pts',(18.0468125934279,-20.9543933870944,-3.75502099195474));
#88051=CARTESIAN_POINT('Ctrl Pts',(18.0048406986407,-20.9397494122098,-3.75764268417117));
#88052=CARTESIAN_POINT('Ctrl Pts',(17.9733408712749,-20.9279096356135,-3.75960190936131));
#88053=CARTESIAN_POINT('Ctrl Pts',(17.8921213235861,-20.8951514618229,-3.76464267812894));
#88054=CARTESIAN_POINT('Ctrl Pts',(17.8428941577103,-20.8730747767913,-3.76768656685087));
#88055=CARTESIAN_POINT('Ctrl Pts',(17.6804863961486,-20.7926526121985,-3.7777732338643));
#88056=CARTESIAN_POINT('Ctrl Pts',(17.5717408942585,-20.7259918550786,-3.78458690825506));
#88057=CARTESIAN_POINT('Ctrl Pts',(17.3877478764065,-20.5889848486864,-3.79713119948763));
#88058=CARTESIAN_POINT('Ctrl Pts',(17.3103837739456,-20.5221673271203,-3.80279980197864));
#88059=CARTESIAN_POINT('Ctrl Pts',(17.2312943914325,-20.4431937398383,-3.80942141152686));
#88060=CARTESIAN_POINT('Ctrl Pts',(17.2244840385472,-20.4362993194805,-3.80999891040315));
#88061=CARTESIAN_POINT('Ctrl Pts',(17.2144981906804,-20.4260504008823,-3.81085700423173));
#88062=CARTESIAN_POINT('Ctrl Pts',(17.2112858427278,-20.4227317658848,-3.81113479857101));
#88063=CARTESIAN_POINT('Ctrl Pts',(17.2056059510784,-20.4168253876997,-3.81162915932021));
#88064=CARTESIAN_POINT('Ctrl Pts',(17.2031340761522,-20.4142418774679,-3.81184538401416));
#88065=CARTESIAN_POINT('Ctrl Pts',(17.1978517143835,-20.4086928766961,-3.81230979083259));
#88066=CARTESIAN_POINT('Ctrl Pts',(17.1950433058898,-20.4057255536794,-3.81255811939621));
#88067=CARTESIAN_POINT('Ctrl Pts',(17.1892976396484,-20.3996194587759,-3.81306906338758));
#88068=CARTESIAN_POINT('Ctrl Pts',(17.1863613190114,-20.3964798343598,-3.81333174696066));
#88069=CARTESIAN_POINT('Ctrl Pts',(17.1729076005358,-20.3820064999248,-3.81454244666627));
#88070=CARTESIAN_POINT('Ctrl Pts',(17.1625053224303,-20.3705670643121,-3.81549867412406));
#88071=CARTESIAN_POINT('Ctrl Pts',(17.0941973460345,-20.2937750436813,-3.82190711715058));
#88072=CARTESIAN_POINT('Ctrl Pts',(17.0402625680135,-20.2250135063294,-3.82759172307141));
#88073=CARTESIAN_POINT('Ctrl Pts',(16.9494514018129,-20.0932138424625,-3.83812736757958));
#88074=CARTESIAN_POINT('Ctrl Pts',(16.9112865270765,-20.0312119709267,-3.84295320930795));
#88075=CARTESIAN_POINT('Ctrl Pts',(16.8741060748315,-19.9631905116076,-3.84805125670443));
#88076=CARTESIAN_POINT('Ctrl Pts',(16.8718368428655,-19.9590054816583,-3.84836415855552));
#88077=CARTESIAN_POINT('Ctrl Pts',(16.8216174704287,-19.8656381923011,-3.8553278644878));
#88078=CARTESIAN_POINT('Ctrl Pts',(16.7801280770989,-19.773166078775,-3.86186882433325));
#88079=CARTESIAN_POINT('Ctrl Pts',(16.7454195176904,-19.6781106426554,-3.8681936027756));
#88080=CARTESIAN_POINT('',(16.6170008393112,-18.9501148891278,-2.8890562790225));
#88081=CARTESIAN_POINT('Ctrl Pts',(16.7454194499637,-19.6781104571739,-3.64442446316901));
#88082=CARTESIAN_POINT('Ctrl Pts',(16.7704138786351,-19.7465620738999,-3.64005127865668));
#88083=CARTESIAN_POINT('Ctrl Pts',(16.7989618298144,-19.8137628460192,-3.63567809414436));
#88084=CARTESIAN_POINT('Ctrl Pts',(16.8309082925844,-19.8793246212443,-3.63130490963203));
#88085=CARTESIAN_POINT('Ctrl Pts',(16.8628484343729,-19.9448734243051,-3.62693259040543));
#88086=CARTESIAN_POINT('Ctrl Pts',(16.8981855408596,-20.0087834410941,-3.62256027117883));
#88087=CARTESIAN_POINT('Ctrl Pts',(16.9367174467763,-20.0706887073167,-3.61818795195223));
#88088=CARTESIAN_POINT('Ctrl Pts',(16.9752544392512,-20.1326021455912,-3.61381505554016));
#88089=CARTESIAN_POINT('Ctrl Pts',(17.0169868114736,-20.1925098997059,-3.6094421591281));
#88090=CARTESIAN_POINT('Ctrl Pts',(17.0616685465372,-20.2500741541835,-3.60506926271603));
#88091=CARTESIAN_POINT('Ctrl Pts',(17.1063995656089,-20.3077019021036,-3.60069154299392));
#88092=CARTESIAN_POINT('Ctrl Pts',(17.1540861421439,-20.3629806112168,-3.59631382327181));
#88093=CARTESIAN_POINT('Ctrl Pts',(17.2044419174547,-20.4156055042669,-3.5919361035497));
#88094=CARTESIAN_POINT('Ctrl Pts',(17.2548300001719,-20.4682641605506,-3.58755557515729));
#88095=CARTESIAN_POINT('Ctrl Pts',(17.3078903383435,-20.5182652822583,-3.58317504676489));
#88096=CARTESIAN_POINT('Ctrl Pts',(17.3633016190121,-20.5653427869976,-3.57879451837249));
#88097=CARTESIAN_POINT('Ctrl Pts',(17.4188056844067,-20.6124991217751,-3.574406654901));
#88098=CARTESIAN_POINT('Ctrl Pts',(17.4766681642482,-20.6567217793341,-3.57001879142951));
#88099=CARTESIAN_POINT('Ctrl Pts',(17.5365374607371,-20.6977870623481,-3.56563092795801));
#88100=CARTESIAN_POINT('Ctrl Pts',(17.557951455484,-20.7124752548995,-3.56406148099873));
#88101=CARTESIAN_POINT('Ctrl Pts',(17.5796219547575,-20.7267599352232,-3.56249203403944));
#88102=CARTESIAN_POINT('Ctrl Pts',(17.6015321394765,-20.7406323112595,-3.56092258708016));
#88103=CARTESIAN_POINT('Ctrl Pts',(17.6627935078072,-20.7794197860744,-3.55653437814988));
#88104=CARTESIAN_POINT('Ctrl Pts',(17.7261694924202,-20.8151319931224,-3.55214616921959));
#88105=CARTESIAN_POINT('Ctrl Pts',(17.7913186157341,-20.8475318007774,-3.54775796028931));
#88106=CARTESIAN_POINT('Ctrl Pts',(17.856371046947,-20.8798835217459,-3.54337626418866));
#88107=CARTESIAN_POINT('Ctrl Pts',(17.9231909643684,-20.908932389527,-3.53899456808801));
#88108=CARTESIAN_POINT('Ctrl Pts',(17.9914091442166,-20.9344852637301,-3.53461287198736));
#88109=CARTESIAN_POINT('Ctrl Pts',(18.0595471622743,-20.9600081112723,-3.53023632472835));
#88110=CARTESIAN_POINT('Ctrl Pts',(18.129079729305,-20.982042957579,-3.52585977746933));
#88111=CARTESIAN_POINT('Ctrl Pts',(18.1996158698655,-21.0004439463799,-3.52148323021032));
#88112=CARTESIAN_POINT('Ctrl Pts',(18.2701072774307,-21.018833265541,-3.51710945849398));
#88113=CARTESIAN_POINT('Ctrl Pts',(18.3416005301147,-21.033593178237,-3.51273568677764));
#88114=CARTESIAN_POINT('Ctrl Pts',(18.4136889989953,-21.0446275021215,-3.5083619150613));
#88115=CARTESIAN_POINT('Ctrl Pts',(18.4857555311126,-21.0556584682242,-3.50398947429839));
#88116=CARTESIAN_POINT('Ctrl Pts',(18.5584164432973,-21.0629660233357,-3.49961703353548));
#88117=CARTESIAN_POINT('Ctrl Pts',(18.631256065406,-21.0665053047709,-3.49524459277256));
#88118=CARTESIAN_POINT('Ctrl Pts',(18.7040975500317,-21.0700446767059,-3.49087204020586));
#88119=CARTESIAN_POINT('Ctrl Pts',(18.7771172717475,-21.0698155622466,-3.48649948763916));
#88120=CARTESIAN_POINT('Ctrl Pts',(18.8498972932268,-21.0658251624538,-3.48212693507246));
#88121=CARTESIAN_POINT('Ctrl Pts',(18.9227528485576,-21.0618306212735,-3.47774984450578));
#88122=CARTESIAN_POINT('Ctrl Pts',(18.9953677242811,-21.0540670274162,-3.47337275393909));
#88123=CARTESIAN_POINT('Ctrl Pts',(19.0673276840493,-21.0425936130789,-3.46899566337241));
#88124=CARTESIAN_POINT('Ctrl Pts',(19.1393269438223,-21.0311139326842,-3.46461618231411));
#88125=CARTESIAN_POINT('Ctrl Pts',(19.2106701033903,-21.0159204984676,-3.46023670125581));
#88126=CARTESIAN_POINT('Ctrl Pts',(19.2809543980021,-20.997123440408,-3.45585722019751));
#88127=CARTESIAN_POINT('Ctrl Pts',(19.3513632710544,-20.9782930646891,-3.45146997653843));
#88128=CARTESIAN_POINT('Ctrl Pts',(19.420709071857,-20.9558464584345,-3.44708273287935));
#88129=CARTESIAN_POINT('Ctrl Pts',(19.4886059995044,-20.9299430693303,-3.44269548922027));
#88130=CARTESIAN_POINT('Ctrl Pts',(19.5347693678672,-20.912331260748,-3.43971258627975));
#88131=CARTESIAN_POINT('Ctrl Pts',(19.5802633709749,-20.8931225055476,-3.43672968333924));
#88132=CARTESIAN_POINT('Ctrl Pts',(19.6249733426256,-20.872378999763,-3.43374678039872));
#88133=CARTESIAN_POINT('Ctrl Pts',(19.6907470875159,-20.841862808246,-3.4293585714646));
#88134=CARTESIAN_POINT('Ctrl Pts',(19.7550796205686,-20.8079039749602,-3.42497036253047));
#88135=CARTESIAN_POINT('Ctrl Pts',(19.8175867162743,-20.7706612736609,-3.42058215359634));
#88136=CARTESIAN_POINT('Ctrl Pts',(19.8800010410864,-20.7334738467051,-3.41620045749183));
#88137=CARTESIAN_POINT('Ctrl Pts',(19.9405948958128,-20.6930124717672,-3.41181876138733));
#88138=CARTESIAN_POINT('Ctrl Pts',(19.9990060261196,-20.6494830643871,-3.40743706528282));
#88139=CARTESIAN_POINT('Ctrl Pts',(20.0573485186997,-20.6060048075249,-3.40306051801995));
#88140=CARTESIAN_POINT('Ctrl Pts',(20.1135129971335,-20.5594659667509,-3.39868397075708));
#88141=CARTESIAN_POINT('Ctrl Pts',(20.1671651917874,-20.5101163413073,-3.3943074234942));
#88142=CARTESIAN_POINT('Ctrl Pts',(20.2207833609993,-20.460798012679,-3.389933651774));
#88143=CARTESIAN_POINT('Ctrl Pts',(20.271892053496,-20.4086727619653,-3.38555988005379));
#88144=CARTESIAN_POINT('Ctrl Pts',(20.3201902946221,-20.35403043806,-3.38118610833359));
#88145=CARTESIAN_POINT('Ctrl Pts',(20.3684738384311,-20.2994047419976,-3.37681366756681));
#88146=CARTESIAN_POINT('Ctrl Pts',(20.4139483094908,-20.2422638546087,-3.37244122680004));
#88147=CARTESIAN_POINT('Ctrl Pts',(20.4563509910175,-20.1829330053829,-3.36806878603326));
#88148=CARTESIAN_POINT('Ctrl Pts',(20.4987547567854,-20.123600639061,-3.36369623346271));
#88149=CARTESIAN_POINT('Ctrl Pts',(20.5380862982223,-20.0620785933403,-3.35932368089216));
#88150=CARTESIAN_POINT('Ctrl Pts',(20.5741254487321,-19.9987221851707,-3.3549511283216));
#88151=CARTESIAN_POINT('Ctrl Pts',(20.6102020020313,-19.9353000233316,-3.35057403775111));
#88152=CARTESIAN_POINT('Ctrl Pts',(20.6429791031822,-19.8700401182239,-3.34619694718061));
#88153=CARTESIAN_POINT('Ctrl Pts',(20.67228233881,-19.8033228383271,-3.34181985661012));
#88154=CARTESIAN_POINT('Ctrl Pts',(20.7016015780221,-19.7365691216478,-3.33744037554803));
#88155=CARTESIAN_POINT('Ctrl Pts',(20.7274430033812,-19.6683568969028,-3.33306089448594));
#88156=CARTESIAN_POINT('Ctrl Pts',(20.7496812078499,-19.5990844367782,-3.32868141342385));
#88157=CARTESIAN_POINT('Ctrl Pts',(20.7719588293865,-19.5296891916842,-3.32429416976104));
#88158=CARTESIAN_POINT('Ctrl Pts',(20.790620352471,-19.4592304251149,-3.31990692609824));
#88159=CARTESIAN_POINT('Ctrl Pts',(20.8055910206615,-19.3881188405866,-3.31551968243543));
#88160=CARTESIAN_POINT('Ctrl Pts',(20.8157696323556,-19.3397698159036,-3.31253677952939));
#88161=CARTESIAN_POINT('Ctrl Pts',(20.8242431499885,-19.2911192245624,-3.30955387662334));
#88162=CARTESIAN_POINT('Ctrl Pts',(20.8310018039417,-19.2422971482213,-3.30657097371729));
#88163=CARTESIAN_POINT('Ctrl Pts',(20.8409445967654,-19.1704740021267,-3.30218276479086));
#88164=CARTESIAN_POINT('Ctrl Pts',(20.8472125720511,-19.0979992504157,-3.29779455586442));
#88165=CARTESIAN_POINT('Ctrl Pts',(20.8497312594192,-19.0252819071575,-3.29340634693799));
#88166=CARTESIAN_POINT('Ctrl Pts',(20.8522462086376,-18.9526724884933,-3.28902465084117));
#88167=CARTESIAN_POINT('Ctrl Pts',(20.8510228997994,-18.8798216711261,-3.28464295474436));
#88168=CARTESIAN_POINT('Ctrl Pts',(20.8460383938858,-18.807145511798,-3.28026125864754));
#88169=CARTESIAN_POINT('Ctrl Pts',(20.8410597451633,-18.7345547527403,-3.27588471139231));
#88170=CARTESIAN_POINT('Ctrl Pts',(20.8323287119824,-18.6621387228754,-3.27150816413708));
#88171=CARTESIAN_POINT('Ctrl Pts',(20.8198744021611,-18.5903137016567,-3.26713161688185));
#88172=CARTESIAN_POINT('Ctrl Pts',(20.8074279906819,-18.5185342308222,-3.26275784516925));
#88173=CARTESIAN_POINT('Ctrl Pts',(20.7912630697951,-18.4473454990803,-3.25838407345666));
#88174=CARTESIAN_POINT('Ctrl Pts',(20.7714604446778,-18.3771574681937,-3.25401030174407));
#88175=CARTESIAN_POINT('Ctrl Pts',(20.7516638455656,-18.3069907957601,-3.24963786098486));
#88176=CARTESIAN_POINT('Ctrl Pts',(20.7282318707952,-18.2378246835973,-3.24526542022566));
#88177=CARTESIAN_POINT('Ctrl Pts',(20.7012957832858,-18.1700560754979,-3.24089297946646));
#88178=CARTESIAN_POINT('Ctrl Pts',(20.6743590070175,-18.102285734547,-3.23652042690342));
#88179=CARTESIAN_POINT('Ctrl Pts',(20.6439181201481,-18.0359134161341,-3.23214787434038));
#88180=CARTESIAN_POINT('Ctrl Pts',(20.610152715999,-17.9713165718493,-3.22777532177735));
#88181=CARTESIAN_POINT('Ctrl Pts',(20.5763522688392,-17.9066526865215,-3.22339823121424));
#88182=CARTESIAN_POINT('Ctrl Pts',(20.5392206395602,-17.8437683827178,-3.21902114065113));
#88183=CARTESIAN_POINT('Ctrl Pts',(20.4989832512062,-17.7830162007275,-3.21464405008802));
#88184=CARTESIAN_POINT('Ctrl Pts',(20.4587238877206,-17.7222308397152,-3.21026456903325));
#88185=CARTESIAN_POINT('Ctrl Pts',(20.4153556750976,-17.6635803070159,-3.20588508797848));
#88186=CARTESIAN_POINT('Ctrl Pts',(20.3691456171871,-17.607385627552,-3.20150560692372));
#88187=CARTESIAN_POINT('Ctrl Pts',(20.3228536522578,-17.5510913433943,-3.19711836326805));
#88188=CARTESIAN_POINT('Ctrl Pts',(20.2737101085744,-17.4972619617622,-3.19273111961239));
#88189=CARTESIAN_POINT('Ctrl Pts',(20.2220198585541,-17.4461826470157,-3.18834387595673));
#88190=CARTESIAN_POINT('Ctrl Pts',(20.1868754689112,-17.4114536344952,-3.18536097298311));
#88191=CARTESIAN_POINT('Ctrl Pts',(20.1505545743033,-17.3779951039876,-3.18237807000949));
#88192=CARTESIAN_POINT('Ctrl Pts',(20.1131612647175,-17.3458856809359,-3.17939516703586));
#88193=CARTESIAN_POINT('Ctrl Pts',(20.0581512102737,-17.2986488589,-3.17500695810766));
#88194=CARTESIAN_POINT('Ctrl Pts',(20.000604149589,-17.2541492751002,-3.17061874917945));
#88195=CARTESIAN_POINT('Ctrl Pts',(19.9408236893637,-17.212670938899,-3.16623054025124));
#88196=CARTESIAN_POINT('Ctrl Pts',(19.881131953254,-17.1712541634265,-3.16184884415272));
#88197=CARTESIAN_POINT('Ctrl Pts',(19.8192137908515,-17.1328500068488,-3.1574671480542));
#88198=CARTESIAN_POINT('Ctrl Pts',(19.7554066235781,-17.0977029608742,-3.15308545195568));
#88199=CARTESIAN_POINT('Ctrl Pts',(19.6916744348054,-17.0625972154763,-3.14870890469885));
#88200=CARTESIAN_POINT('Ctrl Pts',(19.6260580710933,-17.0307412091793,-3.14433235744203));
#88201=CARTESIAN_POINT('Ctrl Pts',(19.5589233130942,-17.0023357910877,-3.13995581018521));
#88202=CARTESIAN_POINT('Ctrl Pts',(19.4918311309837,-16.9739483872997,-3.1355820384711));
#88203=CARTESIAN_POINT('Ctrl Pts',(19.4232229083471,-16.9490074173244,-3.13120826675699));
#88204=CARTESIAN_POINT('Ctrl Pts',(19.3534870964588,-16.9276668413225,-3.12683449504287));
#88205=CARTESIAN_POINT('Ctrl Pts',(19.2837725054129,-16.9063327593298,-3.12246205428222));
#88206=CARTESIAN_POINT('Ctrl Pts',(19.2129314673181,-16.8885970372539,-3.11808961352157));
#88207=CARTESIAN_POINT('Ctrl Pts',(19.1413687992148,-16.874564161899,-3.11371717276092));
#88208=CARTESIAN_POINT('Ctrl Pts',(19.0698043012467,-16.8605309277221,-3.10934462019651));
#88209=CARTESIAN_POINT('Ctrl Pts',(18.9975186103825,-16.850200819109,-3.1049720676321));
#88210=CARTESIAN_POINT('Ctrl Pts',(18.9249263141352,-16.8436271338848,-3.10059951506769));
#88211=CARTESIAN_POINT('Ctrl Pts',(18.8522586788652,-16.8370466262422,-3.09622242450332));
#88212=CARTESIAN_POINT('Ctrl Pts',(18.7792842843309,-16.8342303693192,-3.09184533393896));
#88213=CARTESIAN_POINT('Ctrl Pts',(18.7064215783436,-16.8351796413822,-3.0874682433746));
#88214=CARTESIAN_POINT('Ctrl Pts',(18.6335190793285,-16.8361294318778,-3.08308876231864));
#88215=CARTESIAN_POINT('Ctrl Pts',(18.5607288720061,-16.8408488145897,-3.07870928126269));
#88216=CARTESIAN_POINT('Ctrl Pts',(18.4884654116526,-16.8492870462364,-3.07432980020673));
#88217=CARTESIAN_POINT('Ctrl Pts',(18.4160738648006,-16.8577402345921,-3.06994255655));
#88218=CARTESIAN_POINT('Ctrl Pts',(18.3442114053978,-16.8699253543968,-3.06555531289326));
#88219=CARTESIAN_POINT('Ctrl Pts',(18.2732828332001,-16.8857404102543,-3.06116806923653));
#88220=CARTESIAN_POINT('Ctrl Pts',(18.2250582383153,-16.896493124403,-3.05818516627583));
#88221=CARTESIAN_POINT('Ctrl Pts',(18.1772650979177,-16.9089227808441,-3.05520226331513));
#88222=CARTESIAN_POINT('Ctrl Pts',(18.1300258654966,-16.9229844148329,-3.05221936035442));
#88223=CARTESIAN_POINT('Ctrl Pts',(18.0605312740272,-16.9436707693599,-3.04783115140135));
#88224=CARTESIAN_POINT('Ctrl Pts',(17.9919650333991,-16.9679719598254,-3.04344294244828));
#88225=CARTESIAN_POINT('Ctrl Pts',(17.9247302870922,-16.9957864299187,-3.03905473349521));
#88226=CARTESIAN_POINT('Ctrl Pts',(17.8575953282951,-17.0235596187273,-3.0346730373717));
#88227=CARTESIAN_POINT('Ctrl Pts',(17.7917883829318,-17.0548355532124,-3.03029134124819));
#88228=CARTESIAN_POINT('Ctrl Pts',(17.727697669656,-17.0894628540766,-3.02590964512468));
#88229=CARTESIAN_POINT('Ctrl Pts',(17.6636822680685,-17.1240494651069,-3.02153309784279));
#88230=CARTESIAN_POINT('Ctrl Pts',(17.6013795146522,-17.1619793912541,-3.01715655056091));
#88231=CARTESIAN_POINT('Ctrl Pts',(17.5411562818509,-17.2030537846829,-3.01278000327903));
#88232=CARTESIAN_POINT('Ctrl Pts',(17.4809712417485,-17.2441021293283,-3.00840623153983));
#88233=CARTESIAN_POINT('Ctrl Pts',(17.4228635031204,-17.2882907134209,-3.00403245980062));
#88234=CARTESIAN_POINT('Ctrl Pts',(17.3671727834067,-17.3353762466239,-2.99965868806142));
#88235=CARTESIAN_POINT('Ctrl Pts',(17.3114990105664,-17.3824474515407,-2.99528624727568));
#88236=CARTESIAN_POINT('Ctrl Pts',(17.2582411645733,-17.43241354416,-2.99091380648995));
#88237=CARTESIAN_POINT('Ctrl Pts',(17.2077062220826,-17.4849906941363,-2.98654136570421));
#88238=CARTESIAN_POINT('Ctrl Pts',(17.1571699874087,-17.5375691885152,-2.98216881311475));
#88239=CARTESIAN_POINT('Ctrl Pts',(17.1093571273004,-17.5927585236412,-2.9777962605253));
#88240=CARTESIAN_POINT('Ctrl Pts',(17.0645368651535,-17.650238946124,-2.97342370793584));
#88241=CARTESIAN_POINT('Ctrl Pts',(17.0196700868509,-17.7077790239535,-2.96904661734668));
#88242=CARTESIAN_POINT('Ctrl Pts',(16.977802404763,-17.7676145553151,-2.96466952675751));
#88243=CARTESIAN_POINT('Ctrl Pts',(16.9391613915751,-17.8293943837182,-2.96029243616834));
#88244=CARTESIAN_POINT('Ctrl Pts',(16.9004992750969,-17.8912079523768,-2.95591295508767));
#88245=CARTESIAN_POINT('Ctrl Pts',(16.8650675705235,-17.9549675102763,-2.951533474007));
#88246=CARTESIAN_POINT('Ctrl Pts',(16.833047947568,-18.0202970997391,-2.94715399292634));
#88247=CARTESIAN_POINT('Ctrl Pts',(16.8009715700491,-18.0857424854538,-2.94276674924532));
#88248=CARTESIAN_POINT('Ctrl Pts',(16.7723195413291,-18.1527630160747,-2.93837950556431));
#88249=CARTESIAN_POINT('Ctrl Pts',(16.7472252098534,-18.2209631108913,-2.93399226188329));
#88250=CARTESIAN_POINT('Ctrl Pts',(16.7301634837495,-18.2673326003173,-2.93100935914652));
#88251=CARTESIAN_POINT('Ctrl Pts',(16.7147453386169,-18.3142470017708,-2.92802645640976));
#88252=CARTESIAN_POINT('Ctrl Pts',(16.7009992479662,-18.3615790127122,-2.92504355367299));
#88253=CARTESIAN_POINT('Ctrl Pts',(16.6758066766596,-18.4483247712722,-2.91957676374658));
#88254=CARTESIAN_POINT('Ctrl Pts',(16.6561521069762,-18.5367464915003,-2.91410997382017));
#88255=CARTESIAN_POINT('Ctrl Pts',(16.642218086188,-18.6262126075965,-2.90864318389376));
#88256=CARTESIAN_POINT('Ctrl Pts',(16.6285119268969,-18.714215694215,-2.90326579177692));
#88257=CARTESIAN_POINT('Ctrl Pts',(16.6203407792491,-18.8032293912184,-2.89788839966009));
#88258=CARTESIAN_POINT('Ctrl Pts',(16.6178326248384,-18.8926313188492,-2.89251100754326));
#88259=CARTESIAN_POINT('Ctrl Pts',(16.6172955000024,-18.9117768688659,-2.89135943136967));
#88260=CARTESIAN_POINT('Ctrl Pts',(16.6170179137274,-18.9309401417671,-2.89020785519609));
#88261=CARTESIAN_POINT('Ctrl Pts',(16.6170008393112,-18.9501148891278,-2.8890562790225));
#88262=CARTESIAN_POINT('Ctrl Pts',(16.618038032075,-18.9501158127103,-2.8890562790225));
#88263=CARTESIAN_POINT('Ctrl Pts',(16.6201501825404,-19.1969463155021,-2.87422525894902));
#88264=CARTESIAN_POINT('Ctrl Pts',(16.664522062029,-19.4444420314544,-2.85939423887553));
#88265=CARTESIAN_POINT('Ctrl Pts',(16.7477770216415,-19.6772709618372,-2.84456321880205));
#88266=CARTESIAN_POINT('Origin',(18.734,-18.952,0.));
#88267=CARTESIAN_POINT('',(16.7454194493934,-19.6781104556121,-2.04625066941376));
#88268=CARTESIAN_POINT('',(16.7454194499845,-19.6781104572309,-2.26547385582022));
#88269=CARTESIAN_POINT('',(16.7454194499637,-19.6781104571739,0.));
#88270=CARTESIAN_POINT('',(16.617000743883,-18.9537747113038,-2.31031846929929));
#88271=CARTESIAN_POINT('Ctrl Pts',(16.7454194499845,-19.6781104572309,-2.26547385582022));
#88272=CARTESIAN_POINT('Ctrl Pts',(16.7104732804469,-19.5824042566824,-2.27104574889238));
#88273=CARTESIAN_POINT('Ctrl Pts',(16.6824859377261,-19.4843109672804,-2.27670318400123));
#88274=CARTESIAN_POINT('Ctrl Pts',(16.6596908892846,-19.3751129893312,-2.28331203840856));
#88275=CARTESIAN_POINT('Ctrl Pts',(16.6577760537803,-19.3656145616665,-2.2838894546805));
#88276=CARTESIAN_POINT('Ctrl Pts',(16.6550449338362,-19.3515699728654,-2.28474744876694));
#88277=CARTESIAN_POINT('Ctrl Pts',(16.6541781832451,-19.347033593467,-2.28502522690602));
#88278=CARTESIAN_POINT('Ctrl Pts',(16.652666747724,-19.3389802036193,-2.28551956976332));
#88279=CARTESIAN_POINT('Ctrl Pts',(16.6520161213478,-19.3354643579864,-2.28573579285723));
#88280=CARTESIAN_POINT('Ctrl Pts',(16.6506410990766,-19.3279273650159,-2.28620020863802));
#88281=CARTESIAN_POINT('Ctrl Pts',(16.6499194471366,-19.3239058245693,-2.28644854782864));
#88282=CARTESIAN_POINT('Ctrl Pts',(16.6484623845843,-19.3156486440134,-2.28695951762119));
#88283=CARTESIAN_POINT('Ctrl Pts',(16.6477282255922,-19.311412804693,-2.28722221639482));
#88284=CARTESIAN_POINT('Ctrl Pts',(16.6459029140947,-19.30068734686,-2.28788879786091));
#88285=CARTESIAN_POINT('Ctrl Pts',(16.644829118727,-19.2941948747727,-2.28829360523636));
#88286=CARTESIAN_POINT('Ctrl Pts',(16.6260482815475,-19.1772563681001,-2.29560690850301));
#88287=CARTESIAN_POINT('Ctrl Pts',(16.6170944875345,-19.0655986682839,-2.30293671225118));
#88288=CARTESIAN_POINT('Ctrl Pts',(16.617000743883,-18.9537747113038,-2.31031846929929));
#88289=CARTESIAN_POINT('Ctrl Pts',(16.6170007453241,-18.9537764294638,-2.31031835587959));
#88290=CARTESIAN_POINT('Ctrl Pts',(16.6169157267001,-18.8524583825956,-2.3170065931235));
#88291=CARTESIAN_POINT('Ctrl Pts',(16.624104387429,-18.751255842761,-2.32371995685458));
#88292=CARTESIAN_POINT('Ctrl Pts',(16.6510544988285,-18.5636665537717,-2.33599025543251));
#88293=CARTESIAN_POINT('Ctrl Pts',(16.6690366508714,-18.4772425906475,-2.34157367536228));
#88294=CARTESIAN_POINT('Ctrl Pts',(16.6977848563535,-18.3723986625979,-2.34824549634076));
#88295=CARTESIAN_POINT('Ctrl Pts',(16.7034969582071,-18.3526943473505,-2.34949515434532));
#88296=CARTESIAN_POINT('Ctrl Pts',(16.7120848616524,-18.3246032652549,-2.35127114804834));
#88297=CARTESIAN_POINT('Ctrl Pts',(16.7147281849505,-18.3161471631551,-2.35180504107459));
#88298=CARTESIAN_POINT('Ctrl Pts',(16.7194026267417,-18.3015165893118,-2.35272758592687));
#88299=CARTESIAN_POINT('Ctrl Pts',(16.7214092263582,-18.2953344662358,-2.35311703688876));
#88300=CARTESIAN_POINT('Ctrl Pts',(16.7253221590219,-18.2834655559935,-2.35386406073909));
#88301=CARTESIAN_POINT('Ctrl Pts',(16.7272242478572,-18.2777774451925,-2.35422176907291));
#88302=CARTESIAN_POINT('Ctrl Pts',(16.7322704288395,-18.2628976165899,-2.35515677610282));
#88303=CARTESIAN_POINT('Ctrl Pts',(16.7354536843469,-18.2537192542765,-2.35573277519751));
#88304=CARTESIAN_POINT('Ctrl Pts',(16.7467207700364,-18.2219408543608,-2.35772474837877));
#88305=CARTESIAN_POINT('Ctrl Pts',(16.7551258655886,-18.1994560987812,-2.35913005312993));
#88306=CARTESIAN_POINT('Ctrl Pts',(16.8192013078531,-18.0365482671872,-2.36929206489179));
#88307=CARTESIAN_POINT('Ctrl Pts',(16.8893770781872,-17.9022957692239,-2.37751640320179));
#88308=CARTESIAN_POINT('Ctrl Pts',(17.010444033627,-17.7209310046249,-2.3893581083965));
#88309=CARTESIAN_POINT('Ctrl Pts',(17.0502564563995,-17.6670162703443,-2.39299175397592));
#88310=CARTESIAN_POINT('Ctrl Pts',(17.1266260981131,-17.5732510489217,-2.39967845901954));
#88311=CARTESIAN_POINT('Ctrl Pts',(17.162280234728,-17.5327411408619,-2.40270478382399));
#88312=CARTESIAN_POINT('Ctrl Pts',(17.2186822880118,-17.4733920444582,-2.40743003576606));
#88313=CARTESIAN_POINT('Ctrl Pts',(17.2383226321031,-17.4535280131053,-2.40906498891257));
#88314=CARTESIAN_POINT('Ctrl Pts',(17.2632324301722,-17.429312199152,-2.41113481132057));
#88315=CARTESIAN_POINT('Ctrl Pts',(17.2681385497757,-17.4245885985822,-2.41154229695243));
#88316=CARTESIAN_POINT('Ctrl Pts',(17.2760238299547,-17.417069650961,-2.4121971076798));
#88317=CARTESIAN_POINT('Ctrl Pts',(17.2789884850262,-17.4142590662059,-2.41244327356044));
#88318=CARTESIAN_POINT('Ctrl Pts',(17.2845632967386,-17.4090045271771,-2.41290616490901));
#88319=CARTESIAN_POINT('Ctrl Pts',(17.2871715164566,-17.406558598833,-2.4131227341679));
#88320=CARTESIAN_POINT('Ctrl Pts',(17.2931635024018,-17.4009679156958,-2.41362026277763));
#88321=CARTESIAN_POINT('Ctrl Pts',(17.2965513637841,-17.3978276296821,-2.4139015569804));
#88322=CARTESIAN_POINT('Ctrl Pts',(17.3070809758866,-17.3881313723651,-2.41477572904382));
#88323=CARTESIAN_POINT('Ctrl Pts',(17.3142573847721,-17.3816134602653,-2.4153713724465));
#88324=CARTESIAN_POINT('Ctrl Pts',(17.3958754273366,-17.3085012945656,-2.42214147294141));
#88325=CARTESIAN_POINT('Ctrl Pts',(17.4748875437639,-17.2472136638242,-2.42865076829811));
#88326=CARTESIAN_POINT('Ctrl Pts',(17.6997491507202,-17.0969771327951,-2.44646869862621));
#88327=CARTESIAN_POINT('Ctrl Pts',(17.8525403061836,-17.0196875560976,-2.45779497513617));
#88328=CARTESIAN_POINT('Ctrl Pts',(18.0405779362481,-16.9515707138203,-2.47032890480205));
#88329=CARTESIAN_POINT('Ctrl Pts',(18.0683963355061,-16.9421434421884,-2.47215154346896));
#88330=CARTESIAN_POINT('Ctrl Pts',(18.1167124537869,-16.9268830388013,-2.47526360868176));
#88331=CARTESIAN_POINT('Ctrl Pts',(18.1371181024035,-16.9207750805008,-2.47656174562872));
#88332=CARTESIAN_POINT('Ctrl Pts',(18.1662673119798,-16.9125271544833,-2.47839376932748));
#88333=CARTESIAN_POINT('Ctrl Pts',(18.1749371893979,-16.9101335326837,-2.47893588316393));
#88334=CARTESIAN_POINT('Ctrl Pts',(18.1899213291353,-16.9060992312121,-2.47986809349407));
#88335=CARTESIAN_POINT('Ctrl Pts',(18.1962283538843,-16.9044323664579,-2.48025903543764));
#88336=CARTESIAN_POINT('Ctrl Pts',(18.2083198987657,-16.9012964504983,-2.48100581831021));
#88337=CARTESIAN_POINT('Ctrl Pts',(18.2141031140155,-16.8998226573126,-2.48136180949962));
#88338=CARTESIAN_POINT('Ctrl Pts',(18.2291591998643,-16.8960534979491,-2.48228556538595));
#88339=CARTESIAN_POINT('Ctrl Pts',(18.2384415780601,-16.8937963881657,-2.48285209172705));
#88340=CARTESIAN_POINT('Ctrl Pts',(18.2701539036314,-16.8863121704246,-2.48477764924978));
#88341=CARTESIAN_POINT('Ctrl Pts',(18.2926542168509,-16.8813881649859,-2.48612695359053));
#88342=CARTESIAN_POINT('Ctrl Pts',(18.4867167624519,-16.8422263379409,-2.49763049943239));
#88343=CARTESIAN_POINT('Ctrl Pts',(18.6618284568133,-16.8290087383454,-2.50703923594699));
#88344=CARTESIAN_POINT('Ctrl Pts',(18.9238618204368,-16.8417211768299,-2.52131227346742));
#88345=CARTESIAN_POINT('Ctrl Pts',(19.0107864267335,-16.8513546041382,-2.5260947730487));
#88346=CARTESIAN_POINT('Ctrl Pts',(19.1342164402318,-16.8728286295504,-2.53324710796108));
#88347=CARTESIAN_POINT('Ctrl Pts',(19.1713895143418,-16.8803299496605,-2.53544951018984));
#88348=CARTESIAN_POINT('Ctrl Pts',(19.2157229109256,-16.8905225080335,-2.5381560102116));
#88349=CARTESIAN_POINT('Ctrl Pts',(19.2230980911231,-16.8922598547094,-2.53860893189092));
#88350=CARTESIAN_POINT('Ctrl Pts',(19.234530439768,-16.8950177978229,-2.53931539356148));
#88351=CARTESIAN_POINT('Ctrl Pts',(19.2385942632114,-16.8960109119826,-2.53956737935247));
#88352=CARTESIAN_POINT('Ctrl Pts',(19.2461143690509,-16.8978723085235,-2.54003532144812));
#88353=CARTESIAN_POINT('Ctrl Pts',(19.2495714127354,-16.8987372750501,-2.54025108545263));
#88354=CARTESIAN_POINT('Ctrl Pts',(19.2573681691612,-16.9007089876509,-2.54073916213289));
#88355=CARTESIAN_POINT('Ctrl Pts',(19.2617065382762,-16.901820772117,-2.54101176133799));
#88356=CARTESIAN_POINT('Ctrl Pts',(19.2744608351391,-16.9051324533573,-2.54181609981238));
#88357=CARTESIAN_POINT('Ctrl Pts',(19.2828666506179,-16.9073704341119,-2.54234996337193));
#88358=CARTESIAN_POINT('Ctrl Pts',(19.3423525785472,-16.9236013393259,-2.54615349330763));
#88359=CARTESIAN_POINT('Ctrl Pts',(19.3929012966376,-16.939453838755,-2.54951885175871));
#88360=CARTESIAN_POINT('Ctrl Pts',(19.4568597127052,-16.9621795200576,-2.55390448736739));
#88361=CARTESIAN_POINT('Ctrl Pts',(19.4708683067114,-16.9673245126588,-2.55487308977862));
#88362=CARTESIAN_POINT('Ctrl Pts',(19.6170531287681,-17.0227754547697,-2.56505777558374));
#88363=CARTESIAN_POINT('Ctrl Pts',(19.7439283666313,-17.086058305033,-2.57452807062539));
#88364=CARTESIAN_POINT('Ctrl Pts',(19.9496497124028,-17.2158410060306,-2.59031032917732));
#88365=CARTESIAN_POINT('Ctrl Pts',(20.0317277331629,-17.2763030431253,-2.59675072266805));
#88366=CARTESIAN_POINT('Ctrl Pts',(20.1203794467244,-17.3520439602973,-2.60386108689854));
#88367=CARTESIAN_POINT('Ctrl Pts',(20.1315122679663,-17.3617588932709,-2.60475721462031));
#88368=CARTESIAN_POINT('Ctrl Pts',(20.1483371791712,-17.3767541175907,-2.60611671649479));
#88369=CARTESIAN_POINT('Ctrl Pts',(20.1541032746538,-17.3819503389213,-2.60658358309978));
#88370=CARTESIAN_POINT('Ctrl Pts',(20.1645426076581,-17.3914624930856,-2.60743061977818));
#88371=CARTESIAN_POINT('Ctrl Pts',(20.169225198764,-17.3957679822686,-2.60781122426496));
#88372=CARTESIAN_POINT('Ctrl Pts',(20.1792933467162,-17.4051094076467,-2.60863104962916));
#88373=CARTESIAN_POINT('Ctrl Pts',(20.1846721564752,-17.4101525174941,-2.60906995727571));
#88374=CARTESIAN_POINT('Ctrl Pts',(20.1991874877773,-17.4239051232286,-2.61025700308935));
#88375=CARTESIAN_POINT('Ctrl Pts',(20.2082727311446,-17.4326684853727,-2.61100280888896));
#88376=CARTESIAN_POINT('Ctrl Pts',(20.2521097091861,-17.4757158377018,-2.61461612905962));
#88377=CARTESIAN_POINT('Ctrl Pts',(20.2857484979255,-17.5111151482182,-2.61743409475524));
#88378=CARTESIAN_POINT('Ctrl Pts',(20.3451760363231,-17.5781505238545,-2.62252471944323));
#88379=CARTESIAN_POINT('Ctrl Pts',(20.3713310545648,-17.6094286367836,-2.62480961838324));
#88380=CARTESIAN_POINT('Ctrl Pts',(20.4697251199958,-17.7342510388125,-2.63362949005832));
#88381=CARTESIAN_POINT('Ctrl Pts',(20.5349825190024,-17.833019847798,-2.63996753077614));
#88382=CARTESIAN_POINT('Ctrl Pts',(20.6274746363598,-18.0022525173367,-2.65050223644797));
#88383=CARTESIAN_POINT('Ctrl Pts',(20.6597957065887,-18.0696306559827,-2.6546248085828));
#88384=CARTESIAN_POINT('Ctrl Pts',(20.7017512318337,-18.1704401716056,-2.66088070154777));
#88385=CARTESIAN_POINT('Ctrl Pts',(20.7142329780273,-18.2026284504811,-2.66289096454807));
#88386=CARTESIAN_POINT('Ctrl Pts',(20.7284180183301,-18.2420421694957,-2.66538431436342));
#88387=CARTESIAN_POINT('Ctrl Pts',(20.7308783061947,-18.2489919064815,-2.66582514823603));
#88388=CARTESIAN_POINT('Ctrl Pts',(20.734663004152,-18.259862966046,-2.66651677603205));
#88389=CARTESIAN_POINT('Ctrl Pts',(20.7360123274733,-18.2637756398353,-2.6667661188903));
#88390=CARTESIAN_POINT('Ctrl Pts',(20.7385035381253,-18.2710688013267,-2.66723170512251));
#88391=CARTESIAN_POINT('Ctrl Pts',(20.7396483557959,-18.2744482278453,-2.66744777238327));
#88392=CARTESIAN_POINT('Ctrl Pts',(20.7422300765555,-18.2821331761196,-2.66793985755675));
#88393=CARTESIAN_POINT('Ctrl Pts',(20.7436616732755,-18.2864404157414,-2.66821618275783));
#88394=CARTESIAN_POINT('Ctrl Pts',(20.7478845501271,-18.2992836196729,-2.66904160543179));
#88395=CARTESIAN_POINT('Ctrl Pts',(20.750635335215,-18.307832651712,-2.66959299347377));
#88396=CARTESIAN_POINT('Ctrl Pts',(20.771487346728,-18.3740803590518,-2.67387940629834));
#88397=CARTESIAN_POINT('Ctrl Pts',(20.7871615666049,-18.4325079965425,-2.67773895612883));
#88398=CARTESIAN_POINT('Ctrl Pts',(20.8133953508008,-18.5502268830383,-2.68556754238047));
#88399=CARTESIAN_POINT('Ctrl Pts',(20.823969939628,-18.6094626852835,-2.68953238882852));
#88400=CARTESIAN_POINT('Ctrl Pts',(20.8465536991121,-18.7769254187073,-2.70069588184445));
#88401=CARTESIAN_POINT('Ctrl Pts',(20.8527612528954,-18.8857544456839,-2.70788913114571));
#88402=CARTESIAN_POINT('Ctrl Pts',(20.8490664369905,-19.0693984680566,-2.71968940138976));
#88403=CARTESIAN_POINT('Ctrl Pts',(20.8435955456403,-19.1440864297013,-2.72439685678408));
#88404=CARTESIAN_POINT('Ctrl Pts',(20.8318169690626,-19.2369660491584,-2.73013210059552));
#88405=CARTESIAN_POINT('Ctrl Pts',(20.8292064467372,-19.2555649289488,-2.73127472609475));
#88406=CARTESIAN_POINT('Ctrl Pts',(20.8250478441223,-19.2825767731772,-2.73292612749323));
#88407=CARTESIAN_POINT('Ctrl Pts',(20.8236957881941,-19.2910185917114,-2.73344107780867));
#88408=CARTESIAN_POINT('Ctrl Pts',(20.8212342700186,-19.3058130639097,-2.7343415863058));
#88409=CARTESIAN_POINT('Ctrl Pts',(20.8201468576687,-19.312169226613,-2.73472783867462));
#88410=CARTESIAN_POINT('Ctrl Pts',(20.8179779285443,-19.3245076488993,-2.73547642559675));
#88411=CARTESIAN_POINT('Ctrl Pts',(20.8168996538134,-19.3304904073792,-2.73583885903512));
#88412=CARTESIAN_POINT('Ctrl Pts',(20.8142586323714,-19.3447908430385,-2.73670390423305));
#88413=CARTESIAN_POINT('Ctrl Pts',(20.8126717417312,-19.3531039980098,-2.73720574370037));
#88414=CARTESIAN_POINT('Ctrl Pts',(20.8067546261789,-19.3831231257994,-2.73901436199857));
#88415=CARTESIAN_POINT('Ctrl Pts',(20.8021338201563,-19.4047708541332,-2.74031188241666));
#88416=CARTESIAN_POINT('Ctrl Pts',(20.755647546784,-19.6069649012208,-2.75237798096232));
#88417=CARTESIAN_POINT('Ctrl Pts',(20.6905855127162,-19.7813473298862,-2.76229272251722));
#88418=CARTESIAN_POINT('Ctrl Pts',(20.5659711476454,-20.0159642293777,-2.77677404847788));
#88419=CARTESIAN_POINT('Ctrl Pts',(20.524298620227,-20.0846813329277,-2.7811898915694));
#88420=CARTESIAN_POINT('Ctrl Pts',(20.4583989091041,-20.1805921910746,-2.78784597860492));
#88421=CARTESIAN_POINT('Ctrl Pts',(20.4372145872169,-20.2097957265714,-2.78994422700567));
#88422=CARTESIAN_POINT('Ctrl Pts',(20.4107574033016,-20.244373551044,-2.79253523742792));
#88423=CARTESIAN_POINT('Ctrl Pts',(20.4061874580466,-20.2502811276242,-2.79298177026394));
#88424=CARTESIAN_POINT('Ctrl Pts',(20.3990237391862,-20.2594411087297,-2.79368039379265));
#88425=CARTESIAN_POINT('Ctrl Pts',(20.3964514258274,-20.2627103268574,-2.79393098518313));
#88426=CARTESIAN_POINT('Ctrl Pts',(20.3916562811557,-20.2687677733069,-2.79439767245135));
#88427=CARTESIAN_POINT('Ctrl Pts',(20.3894360349361,-20.2715579748176,-2.79461358453165));
#88428=CARTESIAN_POINT('Ctrl Pts',(20.3843918206881,-20.277864312852,-2.79510372197686));
#88429=CARTESIAN_POINT('Ctrl Pts',(20.3815636745789,-20.2813770252365,-2.79537824459905));
#88430=CARTESIAN_POINT('Ctrl Pts',(20.3742331264094,-20.2904226447702,-2.79608901776612));
#88431=CARTESIAN_POINT('Ctrl Pts',(20.3697139862928,-20.2959418278869,-2.7965264340528));
#88432=CARTESIAN_POINT('Ctrl Pts',(20.3418038920467,-20.3296788566898,-2.79922269906642));
#88433=CARTESIAN_POINT('Ctrl Pts',(20.3177127680746,-20.3573063305051,-2.80152770030752));
#88434=CARTESIAN_POINT('Ctrl Pts',(20.1775005399055,-20.5099144196942,-2.8147531387914));
#88435=CARTESIAN_POINT('Ctrl Pts',(20.047323332482,-20.6211243468025,-2.82626428826224));
#88436=CARTESIAN_POINT('Ctrl Pts',(19.8257930265195,-20.7682503569405,-2.84354607192485));
#88437=CARTESIAN_POINT('Ctrl Pts',(19.7428987052606,-20.8155731859445,-2.84960289451251));
#88438=CARTESIAN_POINT('Ctrl Pts',(19.6378403464578,-20.8664761590398,-2.85677370751244));
#88439=CARTESIAN_POINT('Ctrl Pts',(19.6184542690078,-20.8755090418604,-2.85807722426939));
#88440=CARTESIAN_POINT('Ctrl Pts',(19.5907115234959,-20.8879275614428,-2.85991545080504));
#88441=CARTESIAN_POINT('Ctrl Pts',(19.5824654666089,-20.8915557515932,-2.86045846365643));
#88442=CARTESIAN_POINT('Ctrl Pts',(19.5682062357659,-20.8977213435956,-2.86139173415881));
#88443=CARTESIAN_POINT('Ctrl Pts',(19.5622040752749,-20.9002837580529,-2.86178284235533));
#88444=CARTESIAN_POINT('Ctrl Pts',(19.5506934294096,-20.9051350241594,-2.86252961278044));
#88445=CARTESIAN_POINT('Ctrl Pts',(19.5451869406504,-20.9074284258645,-2.86288542685636));
#88446=CARTESIAN_POINT('Ctrl Pts',(19.5308526032992,-20.9133275756213,-2.86380801029628));
#88447=CARTESIAN_POINT('Ctrl Pts',(19.522009891795,-20.9168970317126,-2.86437354764334));
#88448=CARTESIAN_POINT('Ctrl Pts',(19.491824715731,-20.9288450588684,-2.86629208835762));
#88449=CARTESIAN_POINT('Ctrl Pts',(19.4703699202056,-20.9369367968764,-2.86763546233721));
#88450=CARTESIAN_POINT('Ctrl Pts',(19.2828170677453,-21.0042132700977,-2.87921454337805));
#88451=CARTESIAN_POINT('Ctrl Pts',(19.1100620526455,-21.0427805890613,-2.88869091057756));
#88452=CARTESIAN_POINT('Ctrl Pts',(18.8484861431891,-21.0676675513043,-2.90298972081201));
#88453=CARTESIAN_POINT('Ctrl Pts',(18.7620473751143,-21.0705767034938,-2.90772225827461));
#88454=CARTESIAN_POINT('Ctrl Pts',(18.6380215811988,-21.0671587206841,-2.91480722856474));
#88455=CARTESIAN_POINT('Ctrl Pts',(18.6003996697387,-21.065115904893,-2.91699580783972));
#88456=CARTESIAN_POINT('Ctrl Pts',(18.5553166277762,-21.0614592798462,-2.91968698669883));
#88457=CARTESIAN_POINT('Ctrl Pts',(18.5477817190871,-21.0608074707712,-2.92013908174524));
#88458=CARTESIAN_POINT('Ctrl Pts',(18.5360877334676,-21.0597327180037,-2.92084452954647));
#88459=CARTESIAN_POINT('Ctrl Pts',(18.5319260564627,-21.0593377983695,-2.92109633525314));
#88460=CARTESIAN_POINT('Ctrl Pts',(18.5242186248803,-21.0585833656314,-2.92156411387037));
#88461=CARTESIAN_POINT('Ctrl Pts',(18.5206725982112,-21.0582272243907,-2.92177989557451));
#88462=CARTESIAN_POINT('Ctrl Pts',(18.5126685294896,-21.0574029242214,-2.92226823193328));
#88463=CARTESIAN_POINT('Ctrl Pts',(18.5082110906084,-21.0569295619329,-2.9225410744761));
#88464=CARTESIAN_POINT('Ctrl Pts',(18.4950899266296,-21.0554939893562,-2.92334678203535));
#88465=CARTESIAN_POINT('Ctrl Pts',(18.486430725204,-21.054492433896,-2.9238817819525));
#88466=CARTESIAN_POINT('Ctrl Pts',(18.4248693935503,-21.0469864481336,-2.92770744946584));
#88467=CARTESIAN_POINT('Ctrl Pts',(18.3722277688613,-21.0385401430755,-2.93109502138744));
#88468=CARTESIAN_POINT('Ctrl Pts',(18.3023662881824,-21.0246078762941,-2.93569887498028));
#88469=CARTESIAN_POINT('Ctrl Pts',(18.2848122311734,-21.0208744265362,-2.93686496398954));
#88470=CARTESIAN_POINT('Ctrl Pts',(18.2202645661322,-21.0062860186564,-2.94118251760858));
#88471=CARTESIAN_POINT('Ctrl Pts',(18.1735992369101,-20.9940494347733,-2.94436203543676));
#88472=CARTESIAN_POINT('Ctrl Pts',(18.0226006314629,-20.9488885436691,-2.95477314597037));
#88473=CARTESIAN_POINT('Ctrl Pts',(17.9203858758801,-20.9094699078853,-2.96200572004032));
#88474=CARTESIAN_POINT('Ctrl Pts',(17.753380782476,-20.8297119156859,-2.97390170928805));
#88475=CARTESIAN_POINT('Ctrl Pts',(17.6868835548687,-20.7934574222726,-2.97866451213787));
#88476=CARTESIAN_POINT('Ctrl Pts',(17.6063837261286,-20.7437945036205,-2.98445946774088));
#88477=CARTESIAN_POINT('Ctrl Pts',(17.5904362791863,-20.7336587936744,-2.98560916449256));
#88478=CARTESIAN_POINT('Ctrl Pts',(17.567455414304,-20.7186171570415,-2.98726883608506));
#88479=CARTESIAN_POINT('Ctrl Pts',(17.5603130665701,-20.7138800854883,-2.98778507263282));
#88480=CARTESIAN_POINT('Ctrl Pts',(17.5478447349675,-20.705501158092,-2.98868706526776));
#88481=CARTESIAN_POINT('Ctrl Pts',(17.5425063035609,-20.701878109175,-2.98907352259808));
#88482=CARTESIAN_POINT('Ctrl Pts',(17.5321751850707,-20.6947974621759,-2.98982195238016));
#88483=CARTESIAN_POINT('Ctrl Pts',(17.5271806548056,-20.6913426773335,-2.99018402632301));
#88484=CARTESIAN_POINT('Ctrl Pts',(17.5152808115313,-20.6830354609618,-2.99104733259559));
#88485=CARTESIAN_POINT('Ctrl Pts',(17.5083894795699,-20.678163110136,-2.99154779975037));
#88486=CARTESIAN_POINT('Ctrl Pts',(17.4836528536416,-20.6604508542082,-2.99334629434098));
#88487=CARTESIAN_POINT('Ctrl Pts',(17.4659782969115,-20.6473740948702,-2.99463520021195));
#88488=CARTESIAN_POINT('Ctrl Pts',(17.3000934833205,-20.520596329793,-3.00677957041232));
#88489=CARTESIAN_POINT('Ctrl Pts',(17.1673452117098,-20.3880296027907,-3.01676512262662));
#88490=CARTESIAN_POINT('Ctrl Pts',(17.0054419400624,-20.1767742720821,-3.03127849722977));
#88491=CARTESIAN_POINT('Ctrl Pts',(16.9607582404278,-20.1111361796354,-3.03564442048094));
#88492=CARTESIAN_POINT('Ctrl Pts',(16.9014072608096,-20.0124600760732,-3.04223259877066));
#88493=CARTESIAN_POINT('Ctrl Pts',(16.8837303625087,-19.9813073624741,-3.04431617115616));
#88494=CARTESIAN_POINT('Ctrl Pts',(16.8633406663623,-19.9431499418684,-3.0468908986835));
#88495=CARTESIAN_POINT('Ctrl Pts',(16.8598628495763,-19.9365580162922,-3.04733650074735));
#88496=CARTESIAN_POINT('Ctrl Pts',(16.8544998906645,-19.92626157436,-3.04803398195452));
#88497=CARTESIAN_POINT('Ctrl Pts',(16.8525906881932,-19.9225695632107,-3.04828436972068));
#88498=CARTESIAN_POINT('Ctrl Pts',(16.8490636424379,-19.9156994581905,-3.04875087592216));
#88499=CARTESIAN_POINT('Ctrl Pts',(16.8474429522759,-19.9125228903311,-3.04896681180847));
#88500=CARTESIAN_POINT('Ctrl Pts',(16.8437887971301,-19.9053157864152,-3.04945726008974));
#88501=CARTESIAN_POINT('Ctrl Pts',(16.8417602037729,-19.9012828518333,-3.04973207134966));
#88502=CARTESIAN_POINT('Ctrl Pts',(16.8357860126926,-19.889310652084,-3.05054889576093));
#88503=CARTESIAN_POINT('Ctrl Pts',(16.8318774283855,-19.8813531709565,-3.05109313093092));
#88504=CARTESIAN_POINT('Ctrl Pts',(16.8031430628197,-19.8219122699709,-3.05516697329311));
#88505=CARTESIAN_POINT('Ctrl Pts',(16.7803635901166,-19.7694713478007,-3.05880792375393));
#88506=CARTESIAN_POINT('Ctrl Pts',(16.7548404842599,-19.7035321072633,-3.06338856020301));
#88507=CARTESIAN_POINT('Ctrl Pts',(16.750068293043,-19.6908421265627,-3.06427024202607));
#88508=CARTESIAN_POINT('Ctrl Pts',(16.7454194663415,-19.6781105020273,-3.06515442754877));
#88509=CARTESIAN_POINT('',(16.6200858902598,-18.9528284544197,-2.08900426920411));
#88510=CARTESIAN_POINT('Ctrl Pts',(16.7477770216415,-19.6772709618372,-2.84456321880205));
#88511=CARTESIAN_POINT('Ctrl Pts',(16.835153111315,-19.9216249510097,-2.82899806153188));
#88512=CARTESIAN_POINT('Ctrl Pts',(17.3199691704515,-20.7713282302527,-2.77104096870124));
#88513=CARTESIAN_POINT('Ctrl Pts',(19.0938031538723,-21.4292709570805,-2.67069194031012));
#88514=CARTESIAN_POINT('Ctrl Pts',(21.0117474660562,-19.9903622879567,-2.54351613362868));
#88515=CARTESIAN_POINT('Ctrl Pts',(20.8399998530167,-17.5988206232279,-2.41634032694726));
#88516=CARTESIAN_POINT('Ctrl Pts',(18.7361280842055,-16.4487371345171,-2.28916452026581));
#88517=CARTESIAN_POINT('Ctrl Pts',(16.9296978913047,-17.4322383584724,-2.18006983762423));
#88518=CARTESIAN_POINT('Ctrl Pts',(16.621605651229,-18.5471996814609,-2.11336709054313));
#88519=CARTESIAN_POINT('Ctrl Pts',(16.6201761380985,-18.9528314139021,-2.0890562790225));
#88520=CARTESIAN_POINT('Ctrl Pts',(16.6170001249202,-18.9527272634281,-2.08722594301759));
#88521=CARTESIAN_POINT('Ctrl Pts',(16.6170670028625,-19.1474030713124,-2.07601658058626));
#88522=CARTESIAN_POINT('Ctrl Pts',(16.6439835862141,-19.3411372612755,-2.06573526128042));
#88523=CARTESIAN_POINT('Ctrl Pts',(16.7112838360481,-19.5789443055377,-2.05215235255094));
#88524=CARTESIAN_POINT('Ctrl Pts',(16.7274347388846,-19.6288561785945,-2.04923738357229));
#88525=CARTESIAN_POINT('Ctrl Pts',(16.7454194493934,-19.6781104556121,-2.04625066941376));
#88526=CARTESIAN_POINT('Origin',(18.734,-18.952,0.));
#88527=CARTESIAN_POINT('',(16.7454193881274,-19.6781102878245,-1.24458621709266));
#88528=CARTESIAN_POINT('',(16.7454194501222,-19.6781104576079,-1.46829794770746));
#88529=CARTESIAN_POINT('',(16.7454194499637,-19.6781104571739,0.));
#88530=CARTESIAN_POINT('Ctrl Pts',(16.7454194501221,-19.6781104576079,-1.46829794770746));
#88531=CARTESIAN_POINT('Ctrl Pts',(16.6959068596802,-19.5425115644984,-1.47674752143155));
#88532=CARTESIAN_POINT('Ctrl Pts',(16.660389350048,-19.4021955419597,-1.4846915217345));
#88533=CARTESIAN_POINT('Ctrl Pts',(16.6244283767819,-19.1571126854122,-1.49816091871139));
#88534=CARTESIAN_POINT('Ctrl Pts',(16.6169334231157,-19.0539337982303,-1.50372411700594));
#88535=CARTESIAN_POINT('Ctrl Pts',(16.6170394069824,-18.8905719711407,-1.51286251429508));
#88536=CARTESIAN_POINT('Ctrl Pts',(16.6196337799717,-18.830551892442,-1.51629224317771));
#88537=CARTESIAN_POINT('Ctrl Pts',(16.6255428334935,-18.761795416016,-1.52038548468644));
#88538=CARTESIAN_POINT('Ctrl Pts',(16.6263673814007,-18.7528665137208,-1.52092024802311));
#88539=CARTESIAN_POINT('Ctrl Pts',(16.6276944044936,-18.7394292741622,-1.5217302094326));
#88540=CARTESIAN_POINT('Ctrl Pts',(16.6281546985465,-18.7349167426731,-1.52200309516185));
#88541=CARTESIAN_POINT('Ctrl Pts',(16.6290029479853,-18.7268575103288,-1.52249209211128));
#88542=CARTESIAN_POINT('Ctrl Pts',(16.6293853699247,-18.7233102795055,-1.52270788943703));
#88543=CARTESIAN_POINT('Ctrl Pts',(16.6302310218749,-18.7156480721986,-1.52317526420203));
#88544=CARTESIAN_POINT('Ctrl Pts',(16.6306973521562,-18.7115335408175,-1.52342700864471));
#88545=CARTESIAN_POINT('Ctrl Pts',(16.6320285811685,-18.700088018914,-1.52412938350687));
#88546=CARTESIAN_POINT('Ctrl Pts',(16.6329197472915,-18.6927602272319,-1.52458145350547));
#88547=CARTESIAN_POINT('Ctrl Pts',(16.6382144774426,-18.651044958285,-1.5271680003287));
#88548=CARTESIAN_POINT('Ctrl Pts',(16.6434236342425,-18.6167671986935,-1.52934380418233));
#88549=CARTESIAN_POINT('Ctrl Pts',(16.6625928143832,-18.508584992473,-1.53633889899296));
#88550=CARTESIAN_POINT('Ctrl Pts',(16.6796496639882,-18.4352914324905,-1.54126751716177));
#88551=CARTESIAN_POINT('Ctrl Pts',(16.7543348565868,-18.177423254658,-1.55897625627325));
#88552=CARTESIAN_POINT('Ctrl Pts',(16.8332855111721,-17.9999711949643,-1.5717449037263));
#88553=CARTESIAN_POINT('Ctrl Pts',(16.9464403168688,-17.8176410045259,-1.58492998889398));
#88554=CARTESIAN_POINT('Ctrl Pts',(16.9579092324591,-17.7997666953292,-1.58622484210071));
#88555=CARTESIAN_POINT('Ctrl Pts',(16.974242179433,-17.7751352678872,-1.58801296802193));
#88556=CARTESIAN_POINT('Ctrl Pts',(16.9788797337915,-17.76823015794,-1.58851466901488));
#88557=CARTESIAN_POINT('Ctrl Pts',(16.9869555328482,-17.7563574430456,-1.58937808933288));
#88558=CARTESIAN_POINT('Ctrl Pts',(16.9903745411024,-17.7513769307287,-1.58974053015028));
#88559=CARTESIAN_POINT('Ctrl Pts',(16.9974994157034,-17.7410926615325,-1.59048946944054));
#88560=CARTESIAN_POINT('Ctrl Pts',(17.0012083753689,-17.735791116354,-1.59087584489431));
#88561=CARTESIAN_POINT('Ctrl Pts',(17.009952791334,-17.7234131486053,-1.59177869310054));
#88562=CARTESIAN_POINT('Ctrl Pts',(17.0150076288238,-17.7163505107052,-1.5922944158827));
#88563=CARTESIAN_POINT('Ctrl Pts',(17.031567848859,-17.6935108063976,-1.59396424933792));
#88564=CARTESIAN_POINT('Ctrl Pts',(17.0432482893916,-17.6778614790923,-1.59511157949382));
#88565=CARTESIAN_POINT('Ctrl Pts',(17.1041455636488,-17.5985843175102,-1.60094402637634));
#88566=CARTESIAN_POINT('Ctrl Pts',(17.1567461429151,-17.5376337818345,-1.60549251926172));
#88567=CARTESIAN_POINT('Ctrl Pts',(17.329516956635,-17.3590976113531,-1.61926736492122));
#88568=CARTESIAN_POINT('Ctrl Pts',(17.4602834509425,-17.2527209135448,-1.62810923135766));
#88569=CARTESIAN_POINT('Ctrl Pts',(17.6034467604446,-17.1621563124989,-1.6376217276704));
#88570=CARTESIAN_POINT('Ctrl Pts',(17.6046584667641,-17.1613915127949,-1.6377022319051));
#88571=CARTESIAN_POINT('Ctrl Pts',(17.6514445974002,-17.1319276205065,-1.64081038340964));
#88572=CARTESIAN_POINT('Ctrl Pts',(17.6980928740948,-17.1049794135023,-1.64389968791362));
#88573=CARTESIAN_POINT('Ctrl Pts',(17.7534415275718,-17.0757616215067,-1.64761365576674));
#88574=CARTESIAN_POINT('Ctrl Pts',(17.7611948902049,-17.0717299174897,-1.64813499645596));
#88575=CARTESIAN_POINT('Ctrl Pts',(17.7729668113755,-17.0657008863011,-1.64892851218767));
#88576=CARTESIAN_POINT('Ctrl Pts',(17.7769672333537,-17.0636680856661,-1.64919851184222));
#88577=CARTESIAN_POINT('Ctrl Pts',(17.7841567259295,-17.0600434839143,-1.64968441595113));
#88578=CARTESIAN_POINT('Ctrl Pts',(17.7873433781023,-17.0584470052359,-1.64990002294738));
#88579=CARTESIAN_POINT('Ctrl Pts',(17.7942731678303,-17.0549971200321,-1.65036941252753));
#88580=CARTESIAN_POINT('Ctrl Pts',(17.7980177138375,-17.0531467658083,-1.65062337523431));
#88581=CARTESIAN_POINT('Ctrl Pts',(17.8085431263604,-17.0479843684589,-1.65133809092136));
#88582=CARTESIAN_POINT('Ctrl Pts',(17.8153361833368,-17.0446975231667,-1.65180036515255));
#88583=CARTESIAN_POINT('Ctrl Pts',(17.8558860173623,-17.025344221543,-1.65456511199464));
#88584=CARTESIAN_POINT('Ctrl Pts',(17.8900437993385,-17.0101389880646,-1.65691571542617));
#88585=CARTESIAN_POINT('Ctrl Pts',(18.0033901188386,-16.9632385817009,-1.66474444330013));
#88586=CARTESIAN_POINT('Ctrl Pts',(18.0840901881355,-16.935424153876,-1.67036035145717));
#88587=CARTESIAN_POINT('Ctrl Pts',(18.3376426344206,-16.8648380641333,-1.6877475323215));
#88588=CARTESIAN_POINT('Ctrl Pts',(18.5144120315916,-16.8389099282527,-1.69943894507714));
#88589=CARTESIAN_POINT('Ctrl Pts',(18.7151607496233,-16.8349610471212,-1.71179547501948));
#88590=CARTESIAN_POINT('Ctrl Pts',(18.7379628773226,-16.834880918614,-1.71318717317304));
#88591=CARTESIAN_POINT('Ctrl Pts',(18.7702765490289,-16.8352894524244,-1.71514332247176));
#88592=CARTESIAN_POINT('Ctrl Pts',(18.7797897258551,-16.8354738754609,-1.71571724340865));
#88593=CARTESIAN_POINT('Ctrl Pts',(18.7952605429755,-16.8358781507666,-1.71664745859521));
#88594=CARTESIAN_POINT('Ctrl Pts',(18.8012189891902,-16.8360590406275,-1.71700496868391));
#88595=CARTESIAN_POINT('Ctrl Pts',(18.8137022580778,-16.8364907977761,-1.71775242172126));
#88596=CARTESIAN_POINT('Ctrl Pts',(18.820226852909,-16.8367466898862,-1.71814220320791));
#88597=CARTESIAN_POINT('Ctrl Pts',(18.8357687662672,-16.8374282682119,-1.71906861637003));
#88598=CARTESIAN_POINT('Ctrl Pts',(18.8447847983785,-16.8378814548477,-1.71960438069374));
#88599=CARTESIAN_POINT('Ctrl Pts',(18.8752582740957,-16.8396086695274,-1.72140982073752));
#88600=CARTESIAN_POINT('Ctrl Pts',(18.8966995662194,-16.8411518448067,-1.72267106170812));
#88601=CARTESIAN_POINT('Ctrl Pts',(19.0969103816754,-16.8586302869528,-1.73437240113143));
#88602=CARTESIAN_POINT('Ctrl Pts',(19.2729932943878,-16.89691024181,-1.74401549097663));
#88603=CARTESIAN_POINT('Ctrl Pts',(19.555680165295,-16.9972509061845,-1.76034065820621));
#88604=CARTESIAN_POINT('Ctrl Pts',(19.665548618835,-17.0471611578171,-1.7669501206697));
#88605=CARTESIAN_POINT('Ctrl Pts',(19.7788406048874,-17.1107810285964,-1.77465075512426));
#88606=CARTESIAN_POINT('Ctrl Pts',(19.7870896100963,-17.1154866034291,-1.77521683153408));
#88607=CARTESIAN_POINT('Ctrl Pts',(19.7992701083452,-17.1225439113445,-1.77606112593602));
#88608=CARTESIAN_POINT('Ctrl Pts',(19.8032262087672,-17.1248532358804,-1.776336671653));
#88609=CARTESIAN_POINT('Ctrl Pts',(19.8102536264388,-17.1289860423741,-1.77682856121645));
#88610=CARTESIAN_POINT('Ctrl Pts',(19.813327854645,-17.1308044750554,-1.77704457608362));
#88611=CARTESIAN_POINT('Ctrl Pts',(19.8199297925728,-17.1347321664726,-1.77751027796089));
#88612=CARTESIAN_POINT('Ctrl Pts',(19.8234559143078,-17.1368438901057,-1.77776012057472));
#88613=CARTESIAN_POINT('Ctrl Pts',(19.8331776616163,-17.1427045821478,-1.77845197327704));
#88614=CARTESIAN_POINT('Ctrl Pts',(19.8393601668363,-17.1464750516987,-1.77889535492862));
#88615=CARTESIAN_POINT('Ctrl Pts',(19.8732150762711,-17.1673609015836,-1.78134148895371));
#88616=CARTESIAN_POINT('Ctrl Pts',(19.9005077969649,-17.1850798003169,-1.78338058488923));
#88617=CARTESIAN_POINT('Ctrl Pts',(20.0617667978381,-17.2951366058749,-1.79578659081906));
#88618=CARTESIAN_POINT('Ctrl Pts',(20.1851293400508,-17.4020372440554,-1.80674338849313));
#88619=CARTESIAN_POINT('Ctrl Pts',(20.3739339838297,-17.6081435535026,-1.82500093318393));
#88620=CARTESIAN_POINT('Ctrl Pts',(20.4455825376158,-17.7006700503044,-1.8324416789022));
#88621=CARTESIAN_POINT('Ctrl Pts',(20.5170242133553,-17.8106333459433,-1.84044864655322));
#88622=CARTESIAN_POINT('Ctrl Pts',(20.5246877072974,-17.8226945784887,-1.8413166204403));
#88623=CARTESIAN_POINT('Ctrl Pts',(20.5366901870894,-17.8420141587161,-1.84269092574387));
#88624=CARTESIAN_POINT('Ctrl Pts',(20.5411087188692,-17.8492223433959,-1.84320018521964));
#88625=CARTESIAN_POINT('Ctrl Pts',(20.5488253331642,-17.8619817895322,-1.84409556143304));
#88626=CARTESIAN_POINT('Ctrl Pts',(20.552141399816,-17.8675219961872,-1.84448233429578));
#88627=CARTESIAN_POINT('Ctrl Pts',(20.5589476646209,-17.8790122999689,-1.8452804014591));
#88628=CARTESIAN_POINT('Ctrl Pts',(20.5624342350925,-17.88496446512,-1.84569156037906));
#88629=CARTESIAN_POINT('Ctrl Pts',(20.5713091019736,-17.9002865930589,-1.84674426816887));
#88630=CARTESIAN_POINT('Ctrl Pts',(20.5766548865702,-17.9096810458922,-1.84738427573947));
#88631=CARTESIAN_POINT('Ctrl Pts',(20.5986660020505,-17.9490610492703,-1.85004493600299));
#88632=CARTESIAN_POINT('Ctrl Pts',(20.6146737458542,-17.9794094919502,-1.85204205999933));
#88633=CARTESIAN_POINT('Ctrl Pts',(20.6544540153659,-18.059485616522,-1.85718612639655));
#88634=CARTESIAN_POINT('Ctrl Pts',(20.6770353996593,-18.1097769708,-1.86029367990828));
#88635=CARTESIAN_POINT('Ctrl Pts',(20.7384916002391,-18.2623196121299,-1.86943807922409));
#88636=CARTESIAN_POINT('Ctrl Pts',(20.7714349183699,-18.3667603483404,-1.8753261953939));
#88637=CARTESIAN_POINT('Ctrl Pts',(20.8065014060671,-18.5178142363522,-1.88376889397428));
#88638=CARTESIAN_POINT('Ctrl Pts',(20.8153945084739,-18.5626723507075,-1.88626879020511));
#88639=CARTESIAN_POINT('Ctrl Pts',(20.8265372287805,-18.6302900001255,-1.89006877648479));
#88640=CARTESIAN_POINT('Ctrl Pts',(20.8298822214581,-18.6528561555841,-1.89134223616384));
#88641=CARTESIAN_POINT('Ctrl Pts',(20.8330041677115,-18.6765518350039,-1.89268888892799));
#88642=CARTESIAN_POINT('Ctrl Pts',(20.8331456863524,-18.677632408744,-1.89275031974608));
#88643=CARTESIAN_POINT('Ctrl Pts',(20.8357822149616,-18.6978852213276,-1.89390208910439));
#88644=CARTESIAN_POINT('Ctrl Pts',(20.8380152338742,-18.7170901156452,-1.89500086273349));
#88645=CARTESIAN_POINT('Ctrl Pts',(20.8433022300961,-18.7687150004179,-1.89797846519824));
#88646=CARTESIAN_POINT('Ctrl Pts',(20.8458716164511,-18.8011779070191,-1.89987614786798));
#88647=CARTESIAN_POINT('Ctrl Pts',(20.84807483845,-18.8405383825168,-1.90222141491291));
#88648=CARTESIAN_POINT('Ctrl Pts',(20.8484251155452,-18.8473933913309,-1.90263149309796));
#88649=CARTESIAN_POINT('Ctrl Pts',(20.8489464635304,-18.8586723182389,-1.90330907026286));
#88650=CARTESIAN_POINT('Ctrl Pts',(20.849137007669,-18.8630953445978,-1.90357550317239));
#88651=CARTESIAN_POINT('Ctrl Pts',(20.8494557736874,-18.8710768935609,-1.90405764659642));
#88652=CARTESIAN_POINT('Ctrl Pts',(20.8495888923784,-18.8746351650505,-1.90427308002196));
#88653=CARTESIAN_POINT('Ctrl Pts',(20.8498603283221,-18.8824160900512,-1.90474524763149));
#88654=CARTESIAN_POINT('Ctrl Pts',(20.8499949809104,-18.8866387765287,-1.90500217933183));
#88655=CARTESIAN_POINT('Ctrl Pts',(20.8503413494707,-18.8986272932997,-1.90573352465153));
#88656=CARTESIAN_POINT('Ctrl Pts',(20.850522956719,-18.9063938305408,-1.90620957280006));
#88657=CARTESIAN_POINT('Ctrl Pts',(20.8514032121794,-18.9556341826149,-1.90924132112767));
#88658=CARTESIAN_POINT('Ctrl Pts',(20.8509254808769,-18.9971170656735,-1.91185635046042));
#88659=CARTESIAN_POINT('Ctrl Pts',(20.8415154411867,-19.2270774408199,-1.9265951086465));
#88660=CARTESIAN_POINT('Ctrl Pts',(20.8086346485021,-19.4137259082036,-1.93936820897715));
#88661=CARTESIAN_POINT('Ctrl Pts',(20.742225650577,-19.6225553661527,-1.95345843539751));
#88662=CARTESIAN_POINT('Ctrl Pts',(20.7323805677967,-19.6513496975902,-1.9553992464878));
#88663=CARTESIAN_POINT('Ctrl Pts',(20.7030258713015,-19.7315157831484,-1.960794254304));
#88664=CARTESIAN_POINT('Ctrl Pts',(20.6821313652457,-19.7823570290993,-1.96420534021535));
#88665=CARTESIAN_POINT('Ctrl Pts',(20.6543086333005,-19.8432052003897,-1.96827775162737));
#88666=CARTESIAN_POINT('Ctrl Pts',(20.6492445721393,-19.8540366923927,-1.96900231598644));
#88667=CARTESIAN_POINT('Ctrl Pts',(20.6407076163965,-19.8719002992084,-1.97019683697838));
#88668=CARTESIAN_POINT('Ctrl Pts',(20.6372869747759,-19.8789569510705,-1.97066859078805));
#88669=CARTESIAN_POINT('Ctrl Pts',(20.6310186624264,-19.8917072509704,-1.97152082030682));
#88670=CARTESIAN_POINT('Ctrl Pts',(20.6281843830802,-19.897407344686,-1.97190175676418));
#88671=CARTESIAN_POINT('Ctrl Pts',(20.6220398102003,-19.909626297976,-1.97271826294207));
#88672=CARTESIAN_POINT('Ctrl Pts',(20.6187213637344,-19.9161409827491,-1.97315354101601));
#88673=CARTESIAN_POINT('Ctrl Pts',(20.6095568407958,-19.9339043960364,-1.97434034252751));
#88674=CARTESIAN_POINT('Ctrl Pts',(20.6036433092963,-19.9451181261748,-1.97508948241279));
#88675=CARTESIAN_POINT('Ctrl Pts',(20.5714518772119,-20.0048554513749,-1.97908088540586));
#88676=CARTESIAN_POINT('Ctrl Pts',(20.543383744079,-20.0523932187758,-1.98225856180017));
#88677=CARTESIAN_POINT('Ctrl Pts',(20.4045754762848,-20.2677850080817,-1.99676178879126));
#88678=CARTESIAN_POINT('Ctrl Pts',(20.2721580848393,-20.4203910497828,-2.00723938597097));
#88679=CARTESIAN_POINT('Ctrl Pts',(20.0760807655472,-20.5902669747901,-2.02177024819191));
#88680=CARTESIAN_POINT('Ctrl Pts',(20.0303833966853,-20.6266606372342,-2.02510930740973));
#88681=CARTESIAN_POINT('Ctrl Pts',(19.9760513928753,-20.6663735688224,-2.02910148379458));
#88682=CARTESIAN_POINT('Ctrl Pts',(19.9688247502487,-20.6715860623682,-2.0296329185514));
#88683=CARTESIAN_POINT('Ctrl Pts',(19.9578797944069,-20.679375962364,-2.03043880605199));
#88684=CARTESIAN_POINT('Ctrl Pts',(19.954185667365,-20.6819873996058,-2.03071098081464));
#88685=CARTESIAN_POINT('Ctrl Pts',(19.9475640087384,-20.686636595846,-2.03119921254773));
#88686=CARTESIAN_POINT('Ctrl Pts',(19.9446396727346,-20.6886788147173,-2.03141495967418));
#88687=CARTESIAN_POINT('Ctrl Pts',(19.9383021034834,-20.6930808890209,-2.03188281384409));
#88688=CARTESIAN_POINT('Ctrl Pts',(19.9348871363444,-20.6954380699205,-2.03213509104795));
#88689=CARTESIAN_POINT('Ctrl Pts',(19.92534527731,-20.70198300181,-2.03284042616234));
#88690=CARTESIAN_POINT('Ctrl Pts',(19.9192033315884,-20.7061485499906,-2.03329494306932));
#88691=CARTESIAN_POINT('Ctrl Pts',(19.883722832002,-20.7299404824401,-2.03592286957803));
#88692=CARTESIAN_POINT('Ctrl Pts',(19.8539207880316,-20.7488617197514,-2.03813913853463));
#88693=CARTESIAN_POINT('Ctrl Pts',(19.7572519413887,-20.8068973882745,-2.04532195273009));
#88694=CARTESIAN_POINT('Ctrl Pts',(19.6887082243677,-20.8430894835651,-2.05040399350328));
#88695=CARTESIAN_POINT('Ctrl Pts',(19.4459888701783,-20.9546845728264,-2.06803347255593));
#88696=CARTESIAN_POINT('Ctrl Pts',(19.2637255529462,-21.0104202644713,-2.08055055417731));
#88697=CARTESIAN_POINT('Ctrl Pts',(19.0550779585259,-21.0446220455466,-2.09354732554634));
#88698=CARTESIAN_POINT('Ctrl Pts',(19.0336518283081,-21.0477974418953,-2.09486833251379));
#88699=CARTESIAN_POINT('Ctrl Pts',(19.0038655028294,-21.0517456887764,-2.09668649192162));
#88700=CARTESIAN_POINT('Ctrl Pts',(18.9955443399767,-21.0527983978826,-2.09719244640404));
#88701=CARTESIAN_POINT('Ctrl Pts',(18.9812014007374,-21.0545263805028,-2.09806121414425));
#88702=CARTESIAN_POINT('Ctrl Pts',(18.9751826239734,-21.0552252985158,-2.09842476978755));
#88703=CARTESIAN_POINT('Ctrl Pts',(18.9627416061524,-21.0566158793265,-2.09917420018124));
#88704=CARTESIAN_POINT('Ctrl Pts',(18.956319027622,-21.0573040097057,-2.09955995987141));
#88705=CARTESIAN_POINT('Ctrl Pts',(18.941319896432,-21.0588416497312,-2.10045826831727));
#88706=CARTESIAN_POINT('Ctrl Pts',(18.9327410661623,-21.0596682064475,-2.1009700895789));
#88707=CARTESIAN_POINT('Ctrl Pts',(18.9050768148987,-21.0621632047661,-2.10261438659748));
#88708=CARTESIAN_POINT('Ctrl Pts',(18.8859733772833,-21.0636250035493,-2.10374037181206));
#88709=CARTESIAN_POINT('Ctrl Pts',(18.7060367786558,-21.0749392184033,-2.11426346527496));
#88710=CARTESIAN_POINT('Ctrl Pts',(18.5445898530113,-21.0666594822605,-2.12302931712828));
#88711=CARTESIAN_POINT('Ctrl Pts',(18.3790956223689,-21.0390495329574,-2.13214074052811));
#88712=CARTESIAN_POINT('Ctrl Pts',(18.3725676077833,-21.0379289288149,-2.13250044424435));
#88713=CARTESIAN_POINT('Ctrl Pts',(18.3040941985539,-21.0258436423303,-2.13627738645831));
#88714=CARTESIAN_POINT('Ctrl Pts',(18.2426636085114,-21.012153992812,-2.13969897445675));
#88715=CARTESIAN_POINT('Ctrl Pts',(18.16033766413,-20.9899158601766,-2.1444281328191));
#88716=CARTESIAN_POINT('Ctrl Pts',(18.1388336305284,-20.9837397649306,-2.14567707794279));
#88717=CARTESIAN_POINT('Ctrl Pts',(18.068302377477,-20.9622669278466,-2.14983037512416));
#88718=CARTESIAN_POINT('Ctrl Pts',(18.019737415036,-20.9455281503479,-2.15278144658085));
#88719=CARTESIAN_POINT('Ctrl Pts',(17.9644860062333,-20.9242066923814,-2.15629650326148));
#88720=CARTESIAN_POINT('Ctrl Pts',(17.9571545816596,-20.9213303978051,-2.15676618659363));
#88721=CARTESIAN_POINT('Ctrl Pts',(17.9454906688202,-20.9166790970874,-2.15751890115621));
#88722=CARTESIAN_POINT('Ctrl Pts',(17.9411476445557,-20.9149304779826,-2.15780038808813));
#88723=CARTESIAN_POINT('Ctrl Pts',(17.9334819694323,-20.9118144791046,-2.15829943990884));
#88724=CARTESIAN_POINT('Ctrl Pts',(17.9301569547186,-20.9104530293502,-2.15851664503251));
#88725=CARTESIAN_POINT('Ctrl Pts',(17.9231343395083,-20.9075566747733,-2.15897698170939));
#88726=CARTESIAN_POINT('Ctrl Pts',(17.9194376800836,-20.9060197680609,-2.15922022824439));
#88727=CARTESIAN_POINT('Ctrl Pts',(17.9096363108687,-20.9019121478584,-2.15986759874973));
#88728=CARTESIAN_POINT('Ctrl Pts',(17.903539326646,-20.8993232766162,-2.16027280075813));
#88729=CARTESIAN_POINT('Ctrl Pts',(17.8745153525016,-20.8868381651829,-2.16221332577391));
#88730=CARTESIAN_POINT('Ctrl Pts',(17.8517535552687,-20.8765658389402,-2.16376981215767));
#88731=CARTESIAN_POINT('Ctrl Pts',(17.7878648028456,-20.8463615398583,-2.16822656341672));
#88732=CARTESIAN_POINT('Ctrl Pts',(17.7471954762113,-20.8254977315505,-2.17116834600413));
#88733=CARTESIAN_POINT('Ctrl Pts',(17.6162479728418,-20.7528733084796,-2.18091824183866));
#88734=CARTESIAN_POINT('Ctrl Pts',(17.5291052774362,-20.6957725579613,-2.1878464578787));
#88735=CARTESIAN_POINT('Ctrl Pts',(17.4082739301036,-20.6031995852273,-2.19785403650203));
#88736=CARTESIAN_POINT('Ctrl Pts',(17.3710430952452,-20.572604367932,-2.20100111399996));
#88737=CARTESIAN_POINT('Ctrl Pts',(17.2665817762122,-20.4806126403095,-2.20999133998629));
#88738=CARTESIAN_POINT('Ctrl Pts',(17.2022198594721,-20.4161127904904,-2.21572963037585));
#88739=CARTESIAN_POINT('Ctrl Pts',(17.1331431674519,-20.3373285685086,-2.22212281904182));
#88740=CARTESIAN_POINT('Ctrl Pts',(17.1241842624665,-20.3269076864318,-2.2229571073976));
#88741=CARTESIAN_POINT('Ctrl Pts',(17.1099813555459,-20.3100578946565,-2.22428825044668));
#88742=CARTESIAN_POINT('Ctrl Pts',(17.1046726808629,-20.3036842430632,-2.22478775387328));
#88743=CARTESIAN_POINT('Ctrl Pts',(17.0953144889517,-20.2923134563686,-2.22567184531886));
#88744=CARTESIAN_POINT('Ctrl Pts',(17.0912500513045,-20.2873287883209,-2.22605703735929));
#88745=CARTESIAN_POINT('Ctrl Pts',(17.0828301025854,-20.2769058506258,-2.22685758995079));
#88746=CARTESIAN_POINT('Ctrl Pts',(17.0784785900895,-20.2714644391807,-2.22727278660493));
#88747=CARTESIAN_POINT('Ctrl Pts',(17.0672500840754,-20.2572805971603,-2.22834803722952));
#88748=CARTESIAN_POINT('Ctrl Pts',(17.0604149301437,-20.2485052027094,-2.22900641839605));
#88749=CARTESIAN_POINT('Ctrl Pts',(17.0310548901661,-20.2101918694923,-2.23185181854944));
#88750=CARTESIAN_POINT('Ctrl Pts',(17.0092396348382,-20.1801167525585,-2.23401093391364));
#88751=CARTESIAN_POINT('Ctrl Pts',(16.9324166012404,-20.0681186760313,-2.24180569687976));
#88752=CARTESIAN_POINT('Ctrl Pts',(16.8823605285191,-19.9829498781371,-2.24726112357411));
#88753=CARTESIAN_POINT('Ctrl Pts',(16.8038714931498,-19.8251066139317,-2.2568815426041));
#88754=CARTESIAN_POINT('Ctrl Pts',(16.7731660847066,-19.7537739034998,-2.26106805065016));
#88755=CARTESIAN_POINT('Ctrl Pts',(16.746103513988,-19.6799818359296,-2.26536490179543));
#88756=CARTESIAN_POINT('Ctrl Pts',(16.7457611493293,-19.679046260681,-2.26541937453551));
#88757=CARTESIAN_POINT('Ctrl Pts',(16.7454194499845,-19.6781104572309,-2.26547385582022));
#88758=CARTESIAN_POINT('Ctrl Pts',(16.7454194493934,-19.6781104556121,-2.04625066941376));
#88759=CARTESIAN_POINT('Ctrl Pts',(16.7489322042769,-19.6877307495858,-2.04566730752196));
#88760=CARTESIAN_POINT('Ctrl Pts',(16.7525149176216,-19.6973259561389,-2.04508119867915));
#88761=CARTESIAN_POINT('Ctrl Pts',(16.7671937064808,-19.7357845184218,-2.04271339922677));
#88762=CARTESIAN_POINT('Ctrl Pts',(16.7788510681905,-19.7644269782853,-2.04090763254374));
#88763=CARTESIAN_POINT('Ctrl Pts',(16.7939618142905,-19.799343877772,-2.03864174812154));
#88764=CARTESIAN_POINT('Ctrl Pts',(16.7968258180322,-19.8058711815232,-2.03821535303688));
#88765=CARTESIAN_POINT('Ctrl Pts',(16.8013829451204,-19.8161163158947,-2.03754146458505));
#88766=CARTESIAN_POINT('Ctrl Pts',(16.8030539897001,-19.8198439910864,-2.0372953031527));
#88767=CARTESIAN_POINT('Ctrl Pts',(16.8062079246767,-19.8268254112815,-2.03683241629392));
#88768=CARTESIAN_POINT('Ctrl Pts',(16.8076882727646,-19.8300802439065,-2.03661584705281));
#88769=CARTESIAN_POINT('Ctrl Pts',(16.8111000197593,-19.83753148228,-2.03611831334066));
#88770=CARTESIAN_POINT('Ctrl Pts',(16.8130369074569,-19.8417253150674,-2.03583701398533));
#88771=CARTESIAN_POINT('Ctrl Pts',(16.8190812869548,-19.8547011230306,-2.0349628074716));
#88772=CARTESIAN_POINT('Ctrl Pts',(16.823235323712,-19.8634611010553,-2.03436713444438));
#88773=CARTESIAN_POINT('Ctrl Pts',(16.8705007704965,-19.9613906274576,-2.02764872667878));
#88774=CARTESIAN_POINT('Ctrl Pts',(16.9197541448603,-20.0474479169737,-2.02119664022092));
#88775=CARTESIAN_POINT('Ctrl Pts',(17.0685229099909,-20.2696614655017,-2.00358061007281));
#88776=CARTESIAN_POINT('Ctrl Pts',(17.1785833180263,-20.3979396429235,-1.99239379543893));
#88777=CARTESIAN_POINT('Ctrl Pts',(17.3255701391486,-20.5328156825826,-1.97986693659284));
#88778=CARTESIAN_POINT('Ctrl Pts',(17.3489054613338,-20.5533013993503,-1.97793721896634));
#88779=CARTESIAN_POINT('Ctrl Pts',(17.3842828575061,-20.5830064443116,-1.97509725632832));
#88780=CARTESIAN_POINT('Ctrl Pts',(17.395986180175,-20.5926210478915,-1.97417117321999));
#88781=CARTESIAN_POINT('Ctrl Pts',(17.4148934815203,-20.6078170193875,-1.97269612455211));
#88782=CARTESIAN_POINT('Ctrl Pts',(17.422031901074,-20.6134787751463,-1.97214394376681));
#88783=CARTESIAN_POINT('Ctrl Pts',(17.4357160690194,-20.6241890329257,-1.97109431184133));
#88784=CARTESIAN_POINT('Ctrl Pts',(17.442255254385,-20.6292456118536,-1.97059654411106));
#88785=CARTESIAN_POINT('Ctrl Pts',(17.4537843402227,-20.6380533295884,-1.96972554579386));
#88786=CARTESIAN_POINT('Ctrl Pts',(17.4587614956294,-20.6418209147777,-1.96935166816042));
#88787=CARTESIAN_POINT('Ctrl Pts',(17.4686168009528,-20.6492128003572,-1.96861551823935));
#88788=CARTESIAN_POINT('Ctrl Pts',(17.4734940342832,-20.6528382173812,-1.96825320437367));
#88789=CARTESIAN_POINT('Ctrl Pts',(17.4851944062822,-20.6614575401038,-1.96738873621035));
#88790=CARTESIAN_POINT('Ctrl Pts',(17.4920320191164,-20.6664316929905,-1.96688735184414));
#88791=CARTESIAN_POINT('Ctrl Pts',(17.5168351183849,-20.6842489267646,-1.96508210256015));
#88792=CARTESIAN_POINT('Ctrl Pts',(17.5349718879817,-20.6968519518936,-1.96378745037299));
#88793=CARTESIAN_POINT('Ctrl Pts',(17.7074882102058,-20.8127710615573,-1.95169893375997));
#88794=CARTESIAN_POINT('Ctrl Pts',(17.8746326967339,-20.8956278545903,-1.94176357574396));
#88795=CARTESIAN_POINT('Ctrl Pts',(18.126205239552,-20.9814531380444,-1.92727266167189));
#88796=CARTESIAN_POINT('Ctrl Pts',(18.2033517901554,-21.0029765934799,-1.92287097926848));
#88797=CARTESIAN_POINT('Ctrl Pts',(18.3166937727788,-21.0277746973354,-1.9162341472376));
#88798=CARTESIAN_POINT('Ctrl Pts',(18.3520512099398,-21.0345704922844,-1.91414004919831));
#88799=CARTESIAN_POINT('Ctrl Pts',(18.3949261222642,-21.0416826611219,-1.91155364284013));
#88800=CARTESIAN_POINT('Ctrl Pts',(18.4022962792941,-21.0428652172394,-1.91110737185292));
#88801=CARTESIAN_POINT('Ctrl Pts',(18.4137822629527,-21.0446459083493,-1.91040906938291));
#88802=CARTESIAN_POINT('Ctrl Pts',(18.4178939427768,-21.0452709468089,-1.91015853496584));
#88803=CARTESIAN_POINT('Ctrl Pts',(18.4255344371366,-21.0464093947285,-1.9096918964591));
#88804=CARTESIAN_POINT('Ctrl Pts',(18.4290627166577,-21.0469260055718,-1.90947597580671));
#88805=CARTESIAN_POINT('Ctrl Pts',(18.4370574613303,-21.0480759716808,-1.90898574519351));
#88806=CARTESIAN_POINT('Ctrl Pts',(18.4415246333013,-21.0487039632081,-1.90871113750847));
#88807=CARTESIAN_POINT('Ctrl Pts',(18.4530651639789,-21.0502887232309,-1.9080000067286));
#88808=CARTESIAN_POINT('Ctrl Pts',(18.4601413492167,-21.0512239957201,-1.9075623160122));
#88809=CARTESIAN_POINT('Ctrl Pts',(18.503651929787,-21.0567511303766,-1.90486141668591));
#88810=CARTESIAN_POINT('Ctrl Pts',(18.5401936350737,-21.0604298119851,-1.90255187832858));
#88811=CARTESIAN_POINT('Ctrl Pts',(18.7466642944294,-21.0758029792542,-1.88933830343072));
#88812=CARTESIAN_POINT('Ctrl Pts',(18.9174225550322,-21.0679061203798,-1.87784605114837));
#88813=CARTESIAN_POINT('Ctrl Pts',(19.1795609411833,-21.023782620099,-1.86057005990105));
#88814=CARTESIAN_POINT('Ctrl Pts',(19.2725577202418,-21.0015774257592,-1.85450266049592));
#88815=CARTESIAN_POINT('Ctrl Pts',(19.3841839191674,-20.9667972656394,-1.84732074826407));
#88816=CARTESIAN_POINT('Ctrl Pts',(19.4045222174015,-20.9601203049497,-1.8460160539593));
#88817=CARTESIAN_POINT('Ctrl Pts',(19.4332751455721,-20.9501953075874,-1.84417646704904));
#88818=CARTESIAN_POINT('Ctrl Pts',(19.4417751705084,-20.9472003729995,-1.84363325479264));
#88819=CARTESIAN_POINT('Ctrl Pts',(19.4563977975804,-20.9419429693114,-1.84269974633085));
#88820=CARTESIAN_POINT('Ctrl Pts',(19.4625294869523,-20.9397063131113,-1.84230859846981));
#88821=CARTESIAN_POINT('Ctrl Pts',(19.4742444575106,-20.9353715527305,-1.84156182341194));
#88822=CARTESIAN_POINT('Ctrl Pts',(19.4798293983894,-20.9332781436928,-1.84120604402413));
#88823=CARTESIAN_POINT('Ctrl Pts',(19.4943170105604,-20.9277777977739,-1.84028370387048));
#88824=CARTESIAN_POINT('Ctrl Pts',(19.503205714463,-20.9243342607374,-1.83971837377366));
#88825=CARTESIAN_POINT('Ctrl Pts',(19.5333737536923,-20.9124120193906,-1.83780132305922));
#88826=CARTESIAN_POINT('Ctrl Pts',(19.5545390778004,-20.9036478590996,-1.83645921105149));
#88827=CARTESIAN_POINT('Ctrl Pts',(19.7376084146322,-20.8243375502823,-1.82486496401925));
#88828=CARTESIAN_POINT('Ctrl Pts',(19.8902352961146,-20.7341347697657,-1.8153749742479));
#88829=CARTESIAN_POINT('Ctrl Pts',(20.0980782170554,-20.5732382974583,-1.80107084229505));
#88830=CARTESIAN_POINT('Ctrl Pts',(20.1629639637541,-20.5163473527647,-1.79634826998978));
#88831=CARTESIAN_POINT('Ctrl Pts',(20.2509188782263,-20.4291803186487,-1.78927674433768));
#88832=CARTESIAN_POINT('Ctrl Pts',(20.2769299780823,-20.4019900917892,-1.78709093369609));
#88833=CARTESIAN_POINT('Ctrl Pts',(20.3072797516479,-20.3685228489651,-1.78440282271994));
#88834=CARTESIAN_POINT('Ctrl Pts',(20.3123283810147,-20.3628953456445,-1.78395089266901));
#88835=CARTESIAN_POINT('Ctrl Pts',(20.3201211831639,-20.3541148537573,-1.78324564659932));
#88836=CARTESIAN_POINT('Ctrl Pts',(20.3228864021304,-20.3509805113868,-1.78299387619146));
#88837=CARTESIAN_POINT('Ctrl Pts',(20.327992186836,-20.345158501459,-1.78252613113828));
#88838=CARTESIAN_POINT('Ctrl Pts',(20.3303352547559,-20.3424731049976,-1.78231034749362));
#88839=CARTESIAN_POINT('Ctrl Pts',(20.3356104994543,-20.3363962249681,-1.78182196459464));
#88840=CARTESIAN_POINT('Ctrl Pts',(20.3385386735938,-20.3330013554498,-1.78154907719995));
#88841=CARTESIAN_POINT('Ctrl Pts',(20.3471307612879,-20.3229756363641,-1.78074310563295));
#88842=CARTESIAN_POINT('Ctrl Pts',(20.3527644316675,-20.3163191552111,-1.78020788444492));
#88843=CARTESIAN_POINT('Ctrl Pts',(20.3925765091302,-20.2686853366594,-1.77637829095071));
#88844=CARTESIAN_POINT('Ctrl Pts',(20.425233109386,-20.2264668866777,-1.77298679910305));
#88845=CARTESIAN_POINT('Ctrl Pts',(20.4665197727916,-20.1687069051944,-1.76839817527937));
#88846=CARTESIAN_POINT('Ctrl Pts',(20.4766022656412,-20.1542220159567,-1.76725152215736));
#88847=CARTESIAN_POINT('Ctrl Pts',(20.5136850673665,-20.0995007462578,-1.76293918727684));
#88848=CARTESIAN_POINT('Ctrl Pts',(20.5394820045799,-20.0584679821908,-1.75974486644343));
#88849=CARTESIAN_POINT('Ctrl Pts',(20.6188535390919,-19.9220415972636,-1.74931868869326));
#88850=CARTESIAN_POINT('Ctrl Pts',(20.6664533299026,-19.8233674069179,-1.74208589179603));
#88851=CARTESIAN_POINT('Ctrl Pts',(20.726242996681,-19.6701176975957,-1.73151223824997));
#88852=CARTESIAN_POINT('Ctrl Pts',(20.7442598175681,-19.61801912314,-1.72802300249035));
#88853=CARTESIAN_POINT('Ctrl Pts',(20.7701617717284,-19.5324403361156,-1.72246530201314));
#88854=CARTESIAN_POINT('Ctrl Pts',(20.7793001312507,-19.4993694674331,-1.72035839536925));
#88855=CARTESIAN_POINT('Ctrl Pts',(20.7902558605439,-19.4556046636963,-1.71762182929286));
#88856=CARTESIAN_POINT('Ctrl Pts',(20.7928002588466,-19.4450997082502,-1.71696882716814));
#88857=CARTESIAN_POINT('Ctrl Pts',(20.796836531,-19.4278592520601,-1.71590333490508));
#88858=CARTESIAN_POINT('Ctrl Pts',(20.798376109843,-19.4211352259861,-1.71548931529222));
#88859=CARTESIAN_POINT('Ctrl Pts',(20.8012930918354,-19.4081030150994,-1.71468981237898));
#88860=CARTESIAN_POINT('Ctrl Pts',(20.8026745525849,-19.4017958257325,-1.71430420272409));
#88861=CARTESIAN_POINT('Ctrl Pts',(20.8057982323911,-19.3872155344339,-1.71341580275816));
#88862=CARTESIAN_POINT('Ctrl Pts',(20.8075197981364,-19.378938083393,-1.71291367847392));
#88863=CARTESIAN_POINT('Ctrl Pts',(20.8120175439487,-19.3566433861434,-1.71156711253913));
#88864=CARTESIAN_POINT('Ctrl Pts',(20.8147014981895,-19.3426078253813,-1.71072561209479));
#88865=CARTESIAN_POINT('Ctrl Pts',(20.8380194335241,-19.2136011640022,-1.70304550942558));
#88866=CARTESIAN_POINT('Ctrl Pts',(20.8492485225456,-19.0971271651064,-1.69652342597104));
#88867=CARTESIAN_POINT('Ctrl Pts',(20.852986022774,-18.8176429758351,-1.68122171400578));
#88868=CARTESIAN_POINT('Ctrl Pts',(20.8364045221451,-18.6552897483496,-1.67262496729782));
#88869=CARTESIAN_POINT('Ctrl Pts',(20.7943954072476,-18.4646383929559,-1.66141638514543));
#88870=CARTESIAN_POINT('Ctrl Pts',(20.7866511669756,-18.4329879635266,-1.65951617515095));
#88871=CARTESIAN_POINT('Ctrl Pts',(20.7762964575871,-18.3945355054772,-1.65714514738014));
#88872=CARTESIAN_POINT('Ctrl Pts',(20.7743768450401,-18.3875499932671,-1.65671186957185));
#88873=CARTESIAN_POINT('Ctrl Pts',(20.7713118682583,-18.3766164326263,-1.65602952505341));
#88874=CARTESIAN_POINT('Ctrl Pts',(20.7701907735971,-18.372661557458,-1.65578184655573));
#88875=CARTESIAN_POINT('Ctrl Pts',(20.7680740731689,-18.3652765369688,-1.65531769667394));
#88876=CARTESIAN_POINT('Ctrl Pts',(20.767081303078,-18.3618456374567,-1.65510139106755));
#88877=CARTESIAN_POINT('Ctrl Pts',(20.7647957461462,-18.3540212281235,-1.65460656268978));
#88878=CARTESIAN_POINT('Ctrl Pts',(20.7634973863276,-18.3496294062956,-1.65432771862164));
#88879=CARTESIAN_POINT('Ctrl Pts',(20.7594644043921,-18.3361485275235,-1.65346849318304));
#88880=CARTESIAN_POINT('Ctrl Pts',(20.7566829421758,-18.3270737664884,-1.65288547812979));
#88881=CARTESIAN_POINT('Ctrl Pts',(20.7312360812672,-18.2460010856649,-1.64763738004858));
#88882=CARTESIAN_POINT('Ctrl Pts',(20.7047984183217,-18.1752519623246,-1.64277935846478));
#88883=CARTESIAN_POINT('Ctrl Pts',(20.6205227880263,-17.9819147909825,-1.62898784800352));
#88884=CARTESIAN_POINT('Ctrl Pts',(20.5546065873095,-17.8632259766173,-1.61993455239341));
#88885=CARTESIAN_POINT('Ctrl Pts',(20.4268036808233,-17.6775610453561,-1.60532712693758));
#88886=CARTESIAN_POINT('Ctrl Pts',(20.3711302633979,-17.6067910745857,-1.59962724702033));
#88887=CARTESIAN_POINT('Ctrl Pts',(20.2972856710032,-17.5243247070143,-1.59283221782233));
#88888=CARTESIAN_POINT('Ctrl Pts',(20.2832287957971,-17.5090831563693,-1.59156906340394));
#88889=CARTESIAN_POINT('Ctrl Pts',(20.2628224658996,-17.4875990887467,-1.58977744674432));
#88890=CARTESIAN_POINT('Ctrl Pts',(20.2566543662652,-17.4811866720112,-1.58924124340499));
#88891=CARTESIAN_POINT('Ctrl Pts',(20.2459061214758,-17.4701527710375,-1.58831598793813));
#88892=CARTESIAN_POINT('Ctrl Pts',(20.241344794358,-17.4655132013609,-1.58792612370734));
#88893=CARTESIAN_POINT('Ctrl Pts',(20.2325437817913,-17.4566433863577,-1.58717919205395));
#88894=CARTESIAN_POINT('Ctrl Pts',(20.2283073981052,-17.4524099663535,-1.58682198496484));
#88895=CARTESIAN_POINT('Ctrl Pts',(20.2171857297862,-17.4413900062779,-1.58589024093901));
#88896=CARTESIAN_POINT('Ctrl Pts',(20.2102717719477,-17.434632502577,-1.58531698576174));
#88897=CARTESIAN_POINT('Ctrl Pts',(20.1862331043846,-17.4114576343401,-1.58334411946047));
#88898=CARTESIAN_POINT('Ctrl Pts',(20.1688785050395,-17.3952805286651,-1.58195490273184));
#88899=CARTESIAN_POINT('Ctrl Pts',(20.0307355927917,-17.2707838304731,-1.57115663692911));
#88900=CARTESIAN_POINT('Ctrl Pts',(19.8981299120915,-17.17638192739,-1.56237387389386));
#88901=CARTESIAN_POINT('Ctrl Pts',(19.6418773318728,-17.0351175034129,-1.54647744047427));
#88902=CARTESIAN_POINT('Ctrl Pts',(19.5221729686457,-16.9828750013885,-1.53938838462176));
#88903=CARTESIAN_POINT('Ctrl Pts',(19.3871558638748,-16.9382428548846,-1.53099654513051));
#88904=CARTESIAN_POINT('Ctrl Pts',(19.3758337329098,-16.9346056739711,-1.53028982396407));
#88905=CARTESIAN_POINT('Ctrl Pts',(19.3596897369035,-16.9295691476304,-1.52927706601121));
#88906=CARTESIAN_POINT('Ctrl Pts',(19.3548923729526,-16.9280911928868,-1.52897548174137));
#88907=CARTESIAN_POINT('Ctrl Pts',(19.3466139669694,-16.9255730145929,-1.52845390213791));
#88908=CARTESIAN_POINT('Ctrl Pts',(19.3431353839694,-16.9245246527862,-1.52823438145548));
#88909=CARTESIAN_POINT('Ctrl Pts',(19.3363837882651,-16.9225088272918,-1.52780760180038));
#88910=CARTESIAN_POINT('Ctrl Pts',(19.333111127962,-16.921540321889,-1.5276004110663));
#88911=CARTESIAN_POINT('Ctrl Pts',(19.324271786898,-16.9189476534943,-1.52703995934316));
#88912=CARTESIAN_POINT('Ctrl Pts',(19.3187007994672,-16.9173384558301,-1.52668584075044));
#88913=CARTESIAN_POINT('Ctrl Pts',(19.2979796407993,-16.9114452110633,-1.52536556985298));
#88914=CARTESIAN_POINT('Ctrl Pts',(19.2827888656673,-16.9073074487301,-1.52439146148075));
#88915=CARTESIAN_POINT('Ctrl Pts',(19.1401771138437,-16.8701655900877,-1.51519762888554));
#88916=CARTESIAN_POINT('Ctrl Pts',(19.0099955933185,-16.8489463441904,-1.50645979768121));
#88917=CARTESIAN_POINT('Ctrl Pts',(18.7197391250688,-16.8290602835138,-1.48724159268695));
#88918=CARTESIAN_POINT('Ctrl Pts',(18.5600276785025,-16.8361483424727,-1.47686847792856));
#88919=CARTESIAN_POINT('Ctrl Pts',(18.3815830380192,-16.8644310420887,-1.46577185052176));
#88920=CARTESIAN_POINT('Ctrl Pts',(18.360615531112,-16.8680791859056,-1.46447480585023));
#88921=CARTESIAN_POINT('Ctrl Pts',(18.330871940363,-16.8737176293326,-1.46264402126102));
#88922=CARTESIAN_POINT('Ctrl Pts',(18.3220485566474,-16.8754485662734,-1.46210207030407));
#88923=CARTESIAN_POINT('Ctrl Pts',(18.3068432029953,-16.8785322225203,-1.46117003357844));
#88924=CARTESIAN_POINT('Ctrl Pts',(18.3004560173903,-16.8798583132191,-1.46077910342147));
#88925=CARTESIAN_POINT('Ctrl Pts',(18.2882362840569,-16.8824543158398,-1.46003227046569));
#88926=CARTESIAN_POINT('Ctrl Pts',(18.2824027876492,-16.8837194126042,-1.45967621774577));
#88927=CARTESIAN_POINT('Ctrl Pts',(18.2672434753084,-16.8870741703093,-1.45875214469929));
#88928=CARTESIAN_POINT('Ctrl Pts',(18.2579262536683,-16.8892023540657,-1.45818536421874));
#88929=CARTESIAN_POINT('Ctrl Pts',(18.2261829697846,-16.8966794924995,-1.45625813314305));
#88930=CARTESIAN_POINT('Ctrl Pts',(18.2038295264439,-16.9023317695011,-1.45490743175076));
#88931=CARTESIAN_POINT('Ctrl Pts',(18.013001869802,-16.9539151669752,-1.44342145295145));
#88932=CARTESIAN_POINT('Ctrl Pts',(17.8507181972532,-17.0201611612086,-1.43402845207069));
#88933=CARTESIAN_POINT('Ctrl Pts',(17.6219897127354,-17.1484486544967,-1.4197611584354));
#88934=CARTESIAN_POINT('Ctrl Pts',(17.5483186253048,-17.1960041053664,-1.41496680559605));
#88935=CARTESIAN_POINT('Ctrl Pts',(17.4472435822859,-17.2705158003249,-1.4077984934582));
#88936=CARTESIAN_POINT('Ctrl Pts',(17.4172897233129,-17.2938670632764,-1.4055928155219));
#88937=CARTESIAN_POINT('Ctrl Pts',(17.382131184565,-17.3228292997282,-1.40288267925138));
#88938=CARTESIAN_POINT('Ctrl Pts',(17.3763062231341,-17.32768042889,-1.40242955523674));
#88939=CARTESIAN_POINT('Ctrl Pts',(17.3673067243913,-17.3352575967854,-1.40172284187863));
#88940=CARTESIAN_POINT('Ctrl Pts',(17.3641139356787,-17.3379619961014,-1.40147080842526));
#88941=CARTESIAN_POINT('Ctrl Pts',(17.3582169964193,-17.3429870029163,-1.40100283730267));
#88942=CARTESIAN_POINT('Ctrl Pts',(17.3555106795324,-17.3453049789996,-1.40078709230361));
#88943=CARTESIAN_POINT('Ctrl Pts',(17.3494172706157,-17.3505507470784,-1.40029912782624));
#88944=CARTESIAN_POINT('Ctrl Pts',(17.3460336267236,-17.3534824398855,-1.40002662231347));
#88945=CARTESIAN_POINT('Ctrl Pts',(17.3361072826802,-17.3621382062456,-1.39922271506096));
#88946=CARTESIAN_POINT('Ctrl Pts',(17.3295906039502,-17.3678917919791,-1.39868919181648));
#88947=CARTESIAN_POINT('Ctrl Pts',(17.2837281424468,-17.4088892562776,-1.39489463916299));
#88948=CARTESIAN_POINT('Ctrl Pts',(17.245681420375,-17.445551851493,-1.39153840666891));
#88949=CARTESIAN_POINT('Ctrl Pts',(17.1955076965282,-17.4976576891516,-1.38686501324219));
#88950=CARTESIAN_POINT('Ctrl Pts',(17.1821619048552,-17.5119067326764,-1.38559625225881));
#88951=CARTESIAN_POINT('Ctrl Pts',(17.0704045412418,-17.634585567685,-1.37476374261636));
#88952=CARTESIAN_POINT('Ctrl Pts',(16.9832811504003,-17.7527838577972,-1.36495842800338));
#88953=CARTESIAN_POINT('Ctrl Pts',(16.8777709018671,-17.9322388823302,-1.35150931092586));
#88954=CARTESIAN_POINT('Ctrl Pts',(16.8488256589445,-17.986796377786,-1.34758320257808));
#88955=CARTESIAN_POINT('Ctrl Pts',(16.8063135109703,-18.0761579407601,-1.34141720640087));
#88956=CARTESIAN_POINT('Ctrl Pts',(16.7912114292385,-18.1101880506984,-1.33912754616097));
#88957=CARTESIAN_POINT('Ctrl Pts',(16.7727688572228,-18.1548894141365,-1.33619297516809));
#88958=CARTESIAN_POINT('Ctrl Pts',(16.7686050699074,-18.1652118088877,-1.33552028607714));
#88959=CARTESIAN_POINT('Ctrl Pts',(16.7619671080002,-18.1820494622976,-1.33443092439064));
#88960=CARTESIAN_POINT('Ctrl Pts',(16.7594433952834,-18.1885448446606,-1.33401258755429));
#88961=CARTESIAN_POINT('Ctrl Pts',(16.7546526300679,-18.2010577012257,-1.33321029920873));
#88962=CARTESIAN_POINT('Ctrl Pts',(16.7523808363813,-18.2070732661978,-1.33282619209593));
#88963=CARTESIAN_POINT('Ctrl Pts',(16.7472431548165,-18.2208673482705,-1.33194900658151));
#88964=CARTESIAN_POINT('Ctrl Pts',(16.7443954641745,-18.2286525659721,-1.33145654054589));
#88965=CARTESIAN_POINT('Ctrl Pts',(16.7369541499678,-18.249372590471,-1.33015264909309));
#88966=CARTESIAN_POINT('Ctrl Pts',(16.7324404237938,-18.2623358209321,-1.32934387770879));
#88967=CARTESIAN_POINT('Ctrl Pts',(16.6991412232663,-18.3610510614911,-1.32323611835754));
#88968=CARTESIAN_POINT('Ctrl Pts',(16.6757502479701,-18.448530311514,-1.31812043025284));
#88969=CARTESIAN_POINT('Ctrl Pts',(16.6306361033598,-18.6743412206997,-1.30537418636804));
#88970=CARTESIAN_POINT('Ctrl Pts',(16.6168948152901,-18.8138052075209,-1.29793912209419));
#88971=CARTESIAN_POINT('Ctrl Pts',(16.6170159594122,-18.9738905047867,-1.28909419685754));
#88972=CARTESIAN_POINT('Ctrl Pts',(16.6173229666978,-18.9941773247999,-1.28796711722982));
#88973=CARTESIAN_POINT('Ctrl Pts',(16.6196735818504,-19.0738185473015,-1.28350784889897));
#88974=CARTESIAN_POINT('Ctrl Pts',(16.6239226733544,-19.1330753310935,-1.28011460693867));
#88975=CARTESIAN_POINT('Ctrl Pts',(16.6316702820024,-19.2009553189979,-1.27606205837487));
#88976=CARTESIAN_POINT('Ctrl Pts',(16.6327408137604,-19.2098348694499,-1.27552865093646));
#88977=CARTESIAN_POINT('Ctrl Pts',(16.6344383637595,-19.2232018874069,-1.27472036628638));
#88978=CARTESIAN_POINT('Ctrl Pts',(16.6350235911957,-19.2276946907578,-1.27444778780645));
#88979=CARTESIAN_POINT('Ctrl Pts',(16.6360953416554,-19.2357212874388,-1.2739591405539));
#88980=CARTESIAN_POINT('Ctrl Pts',(16.636576377512,-19.2392557606317,-1.27374338405155));
#88981=CARTESIAN_POINT('Ctrl Pts',(16.6376355523248,-19.2468936662814,-1.27327586526396));
#88982=CARTESIAN_POINT('Ctrl Pts',(16.6382167990403,-19.2509965648376,-1.27302393473658));
#88983=CARTESIAN_POINT('Ctrl Pts',(16.6398690473528,-19.262417879234,-1.27232047861236));
#88984=CARTESIAN_POINT('Ctrl Pts',(16.6409663500989,-19.2697323453013,-1.27186750610077));
#88985=CARTESIAN_POINT('Ctrl Pts',(16.647461038454,-19.3115308720028,-1.26926547983125));
#88986=CARTESIAN_POINT('Ctrl Pts',(16.6536719489209,-19.3458808933004,-1.26707452376865));
#88987=CARTESIAN_POINT('Ctrl Pts',(16.6761041766525,-19.4545296219449,-1.26000955504875));
#88988=CARTESIAN_POINT('Ctrl Pts',(16.6954799615833,-19.5281125873802,-1.25502391782212));
#88989=CARTESIAN_POINT('Ctrl Pts',(16.7271552087958,-19.6265459974599,-1.24820176060518));
#88990=CARTESIAN_POINT('Ctrl Pts',(16.7360405261747,-19.6524246263578,-1.24639313502365));
#88991=CARTESIAN_POINT('Ctrl Pts',(16.7454193881274,-19.6781102878244,-1.24458621709267));
#88992=CARTESIAN_POINT('Origin',(18.734,-18.952,0.));
#88993=CARTESIAN_POINT('',(16.7454194499637,-19.6781104571739,-0.444429617385103));
#88994=CARTESIAN_POINT('',(16.7454194499637,-19.6781104571739,-0.666446448202515));
#88995=CARTESIAN_POINT('',(16.7454194499637,-19.6781104571739,0.));
#88996=CARTESIAN_POINT('',(20.3539256943887,-17.5890877707427,0.));
#88997=CARTESIAN_POINT('Ctrl Pts',(16.7454194499637,-19.6781104571739,-0.444429617385103));
#88998=CARTESIAN_POINT('Ctrl Pts',(16.770110945612,-19.7457324388056,-0.440115253521716));
#88999=CARTESIAN_POINT('Ctrl Pts',(16.798260129574,-19.8121054314175,-0.43580088965833));
#89000=CARTESIAN_POINT('Ctrl Pts',(16.8297062682848,-19.8768537091617,-0.431486525794943));
#89001=CARTESIAN_POINT('Ctrl Pts',(16.8611790959266,-19.9416569399905,-0.42716850024957));
#89002=CARTESIAN_POINT('Ctrl Pts',(16.895954251445,-20.0048322531576,-0.422850474704197));
#89003=CARTESIAN_POINT('Ctrl Pts',(16.933824202708,-20.0660269740199,-0.418532449158824));
#89004=CARTESIAN_POINT('Ctrl Pts',(16.9717096227299,-20.1272466911221,-0.414212659827284));
#89005=CARTESIAN_POINT('Ctrl Pts',(17.0126920725612,-20.186483796078,-0.409892870495744));
#89006=CARTESIAN_POINT('Ctrl Pts',(17.0565212752466,-20.2434155520202,-0.405573081164204));
#89007=CARTESIAN_POINT('Ctrl Pts',(17.1004272507063,-20.3004470316303,-0.401245725137602));
#89008=CARTESIAN_POINT('Ctrl Pts',(17.1471896150003,-20.3551647188214,-0.396918369111001));
#89009=CARTESIAN_POINT('Ctrl Pts',(17.1965189468866,-20.4072803892437,-0.3925910130844));
#89010=CARTESIAN_POINT('Ctrl Pts',(17.238558447032,-20.4516944660317,-0.388903148737701));
#89011=CARTESIAN_POINT('Ctrl Pts',(17.2824615173146,-20.49421925598,-0.385215284391002));
#89012=CARTESIAN_POINT('Ctrl Pts',(17.328030443818,-20.5346997842577,-0.381527420044303));
#89013=CARTESIAN_POINT('Ctrl Pts',(17.3823195205318,-20.5829267378796,-0.377133839466685));
#89014=CARTESIAN_POINT('Ctrl Pts',(17.4391958931759,-20.628448704409,-0.372740258889068));
#89015=CARTESIAN_POINT('Ctrl Pts',(17.498359246263,-20.6709767094712,-0.368346678311451));
#89016=CARTESIAN_POINT('Ctrl Pts',(17.5574363013708,-20.7134426815229,-0.363959506382193));
#89017=CARTESIAN_POINT('Ctrl Pts',(17.6187933267003,-20.7529230838071,-0.359572334452935));
#89018=CARTESIAN_POINT('Ctrl Pts',(17.6820956518213,-20.7891679951172,-0.355185162523678));
#89019=CARTESIAN_POINT('Ctrl Pts',(17.7453255105041,-20.8253714144342,-0.350803012885832));
#89020=CARTESIAN_POINT('Ctrl Pts',(17.8104958295947,-20.8583464631661,-0.346420863247986));
#89021=CARTESIAN_POINT('Ctrl Pts',(17.8772429582996,-20.8878864562512,-0.342038713610141));
#89022=CARTESIAN_POINT('Ctrl Pts',(17.9439489461201,-20.9174082417899,-0.33765926499503));
#89023=CARTESIAN_POINT('Ctrl Pts',(18.0122293762549,-20.9434989788705,-0.33327981637992));
#89024=CARTESIAN_POINT('Ctrl Pts',(18.081697252437,-20.9659985415888,-0.32890036776481));
#89025=CARTESIAN_POINT('Ctrl Pts',(18.1511450535803,-20.9884916023148,-0.324522184736118));
#89026=CARTESIAN_POINT('Ctrl Pts',(18.2217791621869,-21.0073954011508,-0.320144001707427));
#89027=CARTESIAN_POINT('Ctrl Pts',(18.2931954849953,-21.0225990388174,-0.315765818678735));
#89028=CARTESIAN_POINT('Ctrl Pts',(18.3646145496345,-21.0378032601853,-0.311387467561893));
#89029=CARTESIAN_POINT('Ctrl Pts',(18.4368154173397,-21.0493069401342,-0.30700911644505));
#89030=CARTESIAN_POINT('Ctrl Pts',(18.5093834475756,-21.0570502142175,-0.302630765328207));
#89031=CARTESIAN_POINT('Ctrl Pts',(18.5820274277171,-21.0648015924333,-0.298247831816702));
#89032=CARTESIAN_POINT('Ctrl Pts',(18.6550388584148,-21.0687846559847,-0.293864898305197));
#89033=CARTESIAN_POINT('Ctrl Pts',(18.7279984288039,-21.0689914929312,-0.289481964793691));
#89034=CARTESIAN_POINT('Ctrl Pts',(18.8009983528725,-21.0691984442785,-0.285096607097214));
#89035=CARTESIAN_POINT('Ctrl Pts',(18.8739458788801,-21.0656250338833,-0.280711249400737));
#89036=CARTESIAN_POINT('Ctrl Pts',(18.946424858768,-21.0583154273227,-0.27632589170426));
#89037=CARTESIAN_POINT('Ctrl Pts',(19.0190319251111,-21.0509929030637,-0.271932784106735));
#89038=CARTESIAN_POINT('Ctrl Pts',(19.091168316046,-21.0399210701979,-0.267539676509209));
#89039=CARTESIAN_POINT('Ctrl Pts',(19.1624267103003,-21.0251954934114,-0.263146568911683));
#89040=CARTESIAN_POINT('Ctrl Pts',(19.2099795641009,-21.0153686764113,-0.260214917062078));
#89041=CARTESIAN_POINT('Ctrl Pts',(19.2571416600211,-21.003915800001,-0.257283265212474));
#89042=CARTESIAN_POINT('Ctrl Pts',(19.3037962227791,-20.9908774520571,-0.254351613362869));
#89043=CARTESIAN_POINT('Ctrl Pts',(19.3728933262966,-20.971567184758,-0.250009730396774));
#89044=CARTESIAN_POINT('Ctrl Pts',(19.4411588243116,-20.9486979955926,-0.245667847430679));
#89045=CARTESIAN_POINT('Ctrl Pts',(19.5081940324577,-20.9223584953269,-0.241325964464583));
#89046=CARTESIAN_POINT('Ctrl Pts',(19.5751282952576,-20.8960586585461,-0.236990619747436));
#89047=CARTESIAN_POINT('Ctrl Pts',(19.6408354886486,-20.8662990562217,-0.232655275030289));
#89048=CARTESIAN_POINT('Ctrl Pts',(19.7049304077652,-20.833218526189,-0.228319930313142));
#89049=CARTESIAN_POINT('Ctrl Pts',(19.7689516598175,-20.8001760170412,-0.223989568395299));
#89050=CARTESIAN_POINT('Ctrl Pts',(19.8313638797399,-20.7638203813565,-0.219659206477455));
#89051=CARTESIAN_POINT('Ctrl Pts',(19.8918019327492,-20.7243384791067,-0.215328844559612));
#89052=CARTESIAN_POINT('Ctrl Pts',(19.952202841651,-20.6848808417024,-0.211001144001965));
#89053=CARTESIAN_POINT('Ctrl Pts',(20.0106315769706,-20.6423010159659,-0.206673443444318));
#89054=CARTESIAN_POINT('Ctrl Pts',(20.0667491221407,-20.5968309267013,-0.202345742886671));
#89055=CARTESIAN_POINT('Ctrl Pts',(20.1228516204485,-20.5513730293844,-0.198019202720377));
#89056=CARTESIAN_POINT('Ctrl Pts',(20.1766437747633,-20.5030267163447,-0.193692662554083));
#89057=CARTESIAN_POINT('Ctrl Pts',(20.2278184819436,-20.4520651129214,-0.189366122387789));
#89058=CARTESIAN_POINT('Ctrl Pts',(20.2789971971884,-20.401099518124,-0.18503924336167));
#89059=CARTESIAN_POINT('Ctrl Pts',(20.3275577103422,-20.3475185761416,-0.180712364335552));
#89060=CARTESIAN_POINT('Ctrl Pts',(20.3732300428321,-20.2916319892705,-0.176385485309434));
#89061=CARTESIAN_POINT('Ctrl Pts',(20.4189571873855,-20.2356783320532,-0.172053413529732));
#89062=CARTESIAN_POINT('Ctrl Pts',(20.461788919467,-20.1774138895481,-0.167721341750031));
#89063=CARTESIAN_POINT('Ctrl Pts',(20.5014963977798,-20.11718045119,-0.163389269970329));
#89064=CARTESIAN_POINT('Ctrl Pts',(20.5412283831299,-20.0569098373883,-0.159054524481558));
#89065=CARTESIAN_POINT('Ctrl Pts',(20.5778320305151,-19.994668236685,-0.154719778992786));
#89066=CARTESIAN_POINT('Ctrl Pts',(20.6111241303052,-19.9308227620085,-0.150385033504014));
#89067=CARTESIAN_POINT('Ctrl Pts',(20.6444832806256,-19.8668487020833,-0.146041557806415));
#89068=CARTESIAN_POINT('Ctrl Pts',(20.6745173629453,-19.8012647680478,-0.141698082108817));
#89069=CARTESIAN_POINT('Ctrl Pts',(20.7010912717234,-19.7344582600432,-0.137354606411219));
#89070=CARTESIAN_POINT('Ctrl Pts',(20.721849646991,-19.6822719379232,-0.133961673167958));
#89071=CARTESIAN_POINT('Ctrl Pts',(20.7404975804328,-19.6293400279684,-0.130568739924696));
#89072=CARTESIAN_POINT('Ctrl Pts',(20.7569922863659,-19.5758519129603,-0.127175806681435));
#89073=CARTESIAN_POINT('Ctrl Pts',(20.7789195445138,-19.5047474197739,-0.12266540659273));
#89074=CARTESIAN_POINT('Ctrl Pts',(20.7971288584811,-19.4323721967961,-0.118155006504025));
#89075=CARTESIAN_POINT('Ctrl Pts',(20.8114809541406,-19.3591386559676,-0.113644606415321));
#89076=CARTESIAN_POINT('Ctrl Pts',(20.8265483375802,-19.2822552609233,-0.108909414481349));
#89077=CARTESIAN_POINT('Ctrl Pts',(20.8373637838653,-19.2044262083738,-0.104174222547377));
#89078=CARTESIAN_POINT('Ctrl Pts',(20.8438249724136,-19.1261481719107,-0.0994390306134055));
#89079=CARTESIAN_POINT('Ctrl Pts',(20.8499589701725,-19.0518340891932,-0.0949436260150769));
#89080=CARTESIAN_POINT('Ctrl Pts',(20.852168892667,-18.9771159048155,-0.0904482214167483));
#89081=CARTESIAN_POINT('Ctrl Pts',(20.8504195396485,-18.9024285143068,-0.0859528168184197));
#89082=CARTESIAN_POINT('Ctrl Pts',(20.848671831534,-18.8278113518075,-0.0814616392162973));
#89083=CARTESIAN_POINT('Ctrl Pts',(20.842972258343,-18.7532253737159,-0.0769704616141749));
#89084=CARTESIAN_POINT('Ctrl Pts',(20.833337630623,-18.6791071407126,-0.0724792840120526));
#89085=CARTESIAN_POINT('Ctrl Pts',(20.8237095451823,-18.6050392368129,-0.067991156090602));
#89086=CARTESIAN_POINT('Ctrl Pts',(20.810151776091,-18.5314388917089,-0.0635030281691514));
#89087=CARTESIAN_POINT('Ctrl Pts',(20.7927329926196,-18.4587379346641,-0.0590149002477008));
#89088=CARTESIAN_POINT('Ctrl Pts',(20.775321490724,-18.3860673688074,-0.0545286484988));
#89089=CARTESIAN_POINT('Ctrl Pts',(20.7540522902898,-18.3142958801147,-0.0500423967498992));
#89090=CARTESIAN_POINT('Ctrl Pts',(20.7290449663564,-18.2438442387327,-0.0455561450009983));
#89091=CARTESIAN_POINT('Ctrl Pts',(20.704034536135,-18.1733838461909,-0.0410693359917531));
#89092=CARTESIAN_POINT('Ctrl Pts',(20.6752851982857,-18.1042440551513,-0.0365825269825079));
#89093=CARTESIAN_POINT('Ctrl Pts',(20.6429658444502,-18.0368287566131,-0.0320957179732627));
#89094=CARTESIAN_POINT('Ctrl Pts',(20.610644937254,-17.9694102179022,-0.0276086933151065));
#89095=CARTESIAN_POINT('Ctrl Pts',(20.5747538739462,-17.9037167392705,-0.0231216686569502));
#89096=CARTESIAN_POINT('Ctrl Pts',(20.5355082322583,-17.8401290141812,-0.018634643998794));
#89097=CARTESIAN_POINT('Ctrl Pts',(20.496235508383,-17.7764974091956,-0.0141445229855435));
#89098=CARTESIAN_POINT('Ctrl Pts',(20.4536038273032,-17.7149748381304,-0.00965440197229298));
#89099=CARTESIAN_POINT('Ctrl Pts',(20.4078725225403,-17.6559136686608,-0.0051642809590425));
#89100=CARTESIAN_POINT('Ctrl Pts',(20.3903400101855,-17.6332707397352,-0.003442853972695));
#89101=CARTESIAN_POINT('Ctrl Pts',(20.3723523439628,-17.6109892567414,-0.0017214269863475));
#89102=CARTESIAN_POINT('Ctrl Pts',(20.3539256943887,-17.5890877707427,0.));
#89103=CARTESIAN_POINT('',(17.1140597194292,-17.5891051077268,-2.19245913160046E-7));
#89104=CARTESIAN_POINT('Origin',(18.734,-18.952,0.));
#89105=CARTESIAN_POINT('Ctrl Pts',(17.1140597194292,-17.5891051077268,-2.19245913160046E-7));
#89106=CARTESIAN_POINT('Ctrl Pts',(17.1607064768662,-17.5336606550706,-0.00438522828538202));
#89107=CARTESIAN_POINT('Ctrl Pts',(17.2102946586576,-17.480504861525,-0.00877023732485088));
#89108=CARTESIAN_POINT('Ctrl Pts',(17.2625708870034,-17.42996670029,-0.0131552463643197));
#89109=CARTESIAN_POINT('Ctrl Pts',(17.3147694940964,-17.3795035795757,-0.0175337444157827));
#89110=CARTESIAN_POINT('Ctrl Pts',(17.3696478802626,-17.3316507087744,-0.0219122424672457));
#89111=CARTESIAN_POINT('Ctrl Pts',(17.4269129074635,-17.2867035301411,-0.0262907405187087));
#89112=CARTESIAN_POINT('Ctrl Pts',(17.4841105391579,-17.2418092500747,-0.0306640854931849));
#89113=CARTESIAN_POINT('Ctrl Pts',(17.5436888539644,-17.1998141657853,-0.035037430467661));
#89114=CARTESIAN_POINT('Ctrl Pts',(17.6053196809544,-17.1609752270281,-0.0394107754421372));
#89115=CARTESIAN_POINT('Ctrl Pts',(17.6669115101636,-17.1221608641608,-0.0437813531204912));
#89116=CARTESIAN_POINT('Ctrl Pts',(17.7305528669281,-17.0864989413485,-0.0481519307988453));
#89117=CARTESIAN_POINT('Ctrl Pts',(17.7958856448175,-17.0542037894968,-0.0525225084771994));
#89118=CARTESIAN_POINT('Ctrl Pts',(17.8611987192173,-17.0219183774296,-0.0568917680479496));
#89119=CARTESIAN_POINT('Ctrl Pts',(17.9282017691101,-16.9929979344006,-0.0612610276186998));
#89120=CARTESIAN_POINT('Ctrl Pts',(17.9965125678451,-16.9676106008614,-0.06563028718945));
#89121=CARTESIAN_POINT('Ctrl Pts',(18.0648253874041,-16.9422225162941,-0.0699996760150934));
#89122=CARTESIAN_POINT('Ctrl Pts',(18.1344455789651,-16.9203679149719,-0.0743690648407367));
#89123=CARTESIAN_POINT('Ctrl Pts',(18.20497303869,-16.9021659886208,-0.07873845366638));
#89124=CARTESIAN_POINT('Ctrl Pts',(18.2755722935749,-16.8839455331716,-0.0831122904187012));
#89125=CARTESIAN_POINT('Ctrl Pts',(18.3470801915499,-16.8693852963437,-0.0874861271710225));
#89126=CARTESIAN_POINT('Ctrl Pts',(18.4190844938149,-16.8585537446679,-0.0918599639233437));
#89127=CARTESIAN_POINT('Ctrl Pts',(18.4911286186646,-16.8477162025113,-0.0962362196628439));
#89128=CARTESIAN_POINT('Ctrl Pts',(18.563669213288,-16.8406114978773,-0.100612475402344));
#89129=CARTESIAN_POINT('Ctrl Pts',(18.6362896320945,-16.8372561185799,-0.104988731141844));
#89130=CARTESIAN_POINT('Ctrl Pts',(18.7090341909997,-16.8338950034698,-0.109372467818921));
#89131=CARTESIAN_POINT('Ctrl Pts',(18.7818583632858,-16.8342960068782,-0.113756204495997));
#89132=CARTESIAN_POINT('Ctrl Pts',(18.8543469087348,-16.8384234999513,-0.118139941173074));
#89133=CARTESIAN_POINT('Ctrl Pts',(18.8963550317497,-16.8408154397493,-0.120680377713149));
#89134=CARTESIAN_POINT('Ctrl Pts',(18.9382505435929,-16.8444579003275,-0.123220814253224));
#89135=CARTESIAN_POINT('Ctrl Pts',(18.9799541383555,-16.8493360796775,-0.125761250793299));
#89136=CARTESIAN_POINT('Ctrl Pts',(19.0521147745614,-16.8577768994061,-0.130157023340392));
#89137=CARTESIAN_POINT('Ctrl Pts',(19.1239757332627,-16.8699525193612,-0.134552795887486));
#89138=CARTESIAN_POINT('Ctrl Pts',(19.1951211678868,-16.8858305324764,-0.138948568434579));
#89139=CARTESIAN_POINT('Ctrl Pts',(19.2661637754887,-16.901685596982,-0.143337987739136));
#89140=CARTESIAN_POINT('Ctrl Pts',(19.3364924469684,-16.9212323267426,-0.147727407043693));
#89141=CARTESIAN_POINT('Ctrl Pts',(19.4056976986063,-16.9443866901998,-0.152116826348249));
#89142=CARTESIAN_POINT('Ctrl Pts',(19.4748249321719,-16.967514950742,-0.156501297270644));
#89143=CARTESIAN_POINT('Ctrl Pts',(19.5428308084353,-16.9942426135354,-0.160885768193038));
#89144=CARTESIAN_POINT('Ctrl Pts',(19.6093188916084,-17.0244352571202,-0.165270239115432));
#89145=CARTESIAN_POINT('Ctrl Pts',(19.6757666906329,-17.0546096074276,-0.169652053551584));
#89146=CARTESIAN_POINT('Ctrl Pts',(19.7406980849855,-17.0882445743231,-0.174033867987736));
#89147=CARTESIAN_POINT('Ctrl Pts',(19.8037359157053,-17.1251573492361,-0.178415682423888));
#89148=CARTESIAN_POINT('Ctrl Pts',(19.866756139595,-17.1620598141979,-0.182796272993973));
#89149=CARTESIAN_POINT('Ctrl Pts',(19.9278834356518,-17.2022380266862,-0.187176863564057));
#89150=CARTESIAN_POINT('Ctrl Pts',(19.9867660616866,-17.2454636849201,-0.191557454134142));
#89151=CARTESIAN_POINT('Ctrl Pts',(20.0456514706292,-17.288691386083,-0.195938251739488));
#89152=CARTESIAN_POINT('Ctrl Pts',(20.1022916128047,-17.3349665330802,-0.200319049344834));
#89153=CARTESIAN_POINT('Ctrl Pts',(20.156365861705,-17.3840190194215,-0.204699846950181));
#89154=CARTESIAN_POINT('Ctrl Pts',(20.2104972294524,-17.4331233201017,-0.209085272009689));
#89155=CARTESIAN_POINT('Ctrl Pts',(20.2620569360998,-17.4850104938255,-0.213470697069196));
#89156=CARTESIAN_POINT('Ctrl Pts',(20.3107600562501,-17.5393724039882,-0.217856122128704));
#89157=CARTESIAN_POINT('Ctrl Pts',(20.359490421265,-17.593764724582,-0.222244000425527));
#89158=CARTESIAN_POINT('Ctrl Pts',(20.4053607162012,-17.6506341638863,-0.22663187872235));
#89159=CARTESIAN_POINT('Ctrl Pts',(20.4481270165511,-17.7096403213523,-0.231019757019172));
#89160=CARTESIAN_POINT('Ctrl Pts',(20.4909690532251,-17.7687509748684,-0.235415405961804));
#89161=CARTESIAN_POINT('Ctrl Pts',(20.5306958563841,-17.8300054996603,-0.239811054904435));
#89162=CARTESIAN_POINT('Ctrl Pts',(20.5671077585183,-17.8930359091735,-0.244206703847067));
#89163=CARTESIAN_POINT('Ctrl Pts',(20.5912140801738,-17.9347648834031,-0.247116821722955));
#89164=CARTESIAN_POINT('Ctrl Pts',(20.6138684164928,-17.9772717133338,-0.250026939598844));
#89165=CARTESIAN_POINT('Ctrl Pts',(20.6350244530402,-18.0204448331188,-0.252937057474733));
#89166=CARTESIAN_POINT('Ctrl Pts',(20.6668851000169,-18.0854628493841,-0.257319647668149));
#89167=CARTESIAN_POINT('Ctrl Pts',(20.6954700316101,-18.1522473407963,-0.261702237861565));
#89168=CARTESIAN_POINT('Ctrl Pts',(20.7205801862023,-18.2204344432736,-0.266084828054982));
#89169=CARTESIAN_POINT('Ctrl Pts',(20.7456525615808,-18.2885189555772,-0.270460824469328));
#89170=CARTESIAN_POINT('Ctrl Pts',(20.767260371406,-18.3580014400403,-0.274836820883674));
#89171=CARTESIAN_POINT('Ctrl Pts',(20.7852512326706,-18.4284950998631,-0.27921281729802));
#89172=CARTESIAN_POINT('Ctrl Pts',(20.8032205403917,-18.4989043063546,-0.28358357114905));
#89173=CARTESIAN_POINT('Ctrl Pts',(20.8175813879169,-18.5703218155193,-0.287954325000079));
#89174=CARTESIAN_POINT('Ctrl Pts',(20.8282307190733,-18.642344230976,-0.292325078851108));
#89175=CARTESIAN_POINT('Ctrl Pts',(20.8388731539879,-18.7143200065093,-0.296693002310752));
#89176=CARTESIAN_POINT('Ctrl Pts',(20.845808770299,-18.7868994338195,-0.301060925770397));
#89177=CARTESIAN_POINT('Ctrl Pts',(20.8489855691776,-18.8596688450713,-0.305428849230041));
#89178=CARTESIAN_POINT('Ctrl Pts',(20.8521613662237,-18.9324153078249,-0.309795395225149));
#89179=CARTESIAN_POINT('Ctrl Pts',(20.8515806778355,-19.0053511525545,-0.314161941220256));
#89180=CARTESIAN_POINT('Ctrl Pts',(20.8472434965741,-19.0780592090539,-0.318528487215364));
#89181=CARTESIAN_POINT('Ctrl Pts',(20.8429062422304,-19.1507684906965,-0.32289510678752));
#89182=CARTESIAN_POINT('Ctrl Pts',(20.8348124001615,-19.2232494936619,-0.327261726359677));
#89183=CARTESIAN_POINT('Ctrl Pts',(20.8230139692876,-19.2950883794611,-0.331628345931833));
#89184=CARTESIAN_POINT('Ctrl Pts',(20.8112033262543,-19.3670016232775,-0.335999485245205));
#89185=CARTESIAN_POINT('Ctrl Pts',(20.7956805170945,-19.438270944489,-0.340370624558577));
#89186=CARTESIAN_POINT('Ctrl Pts',(20.7765488721863,-19.5084917831655,-0.344741763871949));
#89187=CARTESIAN_POINT('Ctrl Pts',(20.757406850392,-19.5787507091909,-0.349115274064269));
#89188=CARTESIAN_POINT('Ctrl Pts',(20.7346522472,-19.6479595605984,-0.353488784256589));
#89189=CARTESIAN_POINT('Ctrl Pts',(20.7084377550415,-19.7157306799303,-0.35786229444891));
#89190=CARTESIAN_POINT('Ctrl Pts',(20.682176526986,-19.7836226234244,-0.36224360185205));
#89191=CARTESIAN_POINT('Ctrl Pts',(20.6524432899172,-19.8500712742597,-0.366624909255191));
#89192=CARTESIAN_POINT('Ctrl Pts',(20.6194379320409,-19.914711173936,-0.371006216658332));
#89193=CARTESIAN_POINT('Ctrl Pts',(20.5965704686666,-19.9594963431777,-0.374041765824277));
#89194=CARTESIAN_POINT('Ctrl Pts',(20.5721332694026,-20.0034137682888,-0.377077314990223));
#89195=CARTESIAN_POINT('Ctrl Pts',(20.5462048528608,-20.0463502964169,-0.380112864156168));
#89196=CARTESIAN_POINT('Ctrl Pts',(20.5087129331597,-20.1084355711665,-0.384502201445419));
#89197=CARTESIAN_POINT('Ctrl Pts',(20.4679538690257,-20.1687127167994,-0.38889153873467));
#89198=CARTESIAN_POINT('Ctrl Pts',(20.424127447363,-20.2268169326104,-0.393280876023921));
#89199=CARTESIAN_POINT('Ctrl Pts',(20.3803660122869,-20.2848349904712,-0.397663704726861));
#89200=CARTESIAN_POINT('Ctrl Pts',(20.333546536813,-20.3406861331264,-0.4020465334298));
#89201=CARTESIAN_POINT('Ctrl Pts',(20.2839132740569,-20.3940325387807,-0.40642936213274));
#89202=CARTESIAN_POINT('Ctrl Pts',(20.234338311065,-20.4473162831732,-0.410807042717946));
#89203=CARTESIAN_POINT('Ctrl Pts',(20.181956453283,-20.4981007839427,-0.415184723303152));
#89204=CARTESIAN_POINT('Ctrl Pts',(20.1270525278191,-20.5460808181321,-0.419562403888359));
#89205=CARTESIAN_POINT('Ctrl Pts',(20.0721834146416,-20.5940304301855,-0.423937308769121));
#89206=CARTESIAN_POINT('Ctrl Pts',(20.0147957688626,-20.6391787874444,-0.428312213649883));
#89207=CARTESIAN_POINT('Ctrl Pts',(19.9552106047207,-20.6812581238548,-0.432687118530645));
#89208=CARTESIAN_POINT('Ctrl Pts',(19.8956435930083,-20.72332464093,-0.437060690610635));
#89209=CARTESIAN_POINT('Ctrl Pts',(19.8338807856146,-20.7623237154589,-0.441434262690625));
#89210=CARTESIAN_POINT('Ctrl Pts',(19.7702742054051,-20.7980294610899,-0.445807834770615));
#89211=CARTESIAN_POINT('Ctrl Pts',(19.7066660505843,-20.8337360906338,-0.450181515120482));
#89212=CARTESIAN_POINT('Ctrl Pts',(19.6412144536897,-20.86614899517,-0.454555195470349));
#89213=CARTESIAN_POINT('Ctrl Pts',(19.5742967209257,-20.8950878572009,-0.458928875820215));
#89214=CARTESIAN_POINT('Ctrl Pts',(19.5073097608989,-20.92405665686,-0.463307080799149));
#89215=CARTESIAN_POINT('Ctrl Pts',(19.4388540801552,-20.949544046669,-0.467685285778082));
#89216=CARTESIAN_POINT('Ctrl Pts',(19.3693269154527,-20.9714179137814,-0.472063490757016));
#89217=CARTESIAN_POINT('Ctrl Pts',(19.2997618805805,-20.9933036951876,-0.476444080463784));
#89218=CARTESIAN_POINT('Ctrl Pts',(19.2291246668025,-21.0115719142762,-0.480824670170553));
#89219=CARTESIAN_POINT('Ctrl Pts',(19.1578249890647,-21.0261411183052,-0.485205259877322));
#89220=CARTESIAN_POINT('Ctrl Pts',(19.0863993186969,-21.0407360673641,-0.489593590460845));
#89221=CARTESIAN_POINT('Ctrl Pts',(19.0143093237697,-21.0516188761684,-0.493981921044368));
#89222=CARTESIAN_POINT('Ctrl Pts',(18.9419715779475,-21.0587597923745,-0.498370251627891));
#89223=CARTESIAN_POINT('Ctrl Pts',(18.892967495442,-21.0635972951603,-0.501343058031128));
#89224=CARTESIAN_POINT('Ctrl Pts',(18.843849807491,-21.0667186668706,-0.504315864434365));
#89225=CARTESIAN_POINT('Ctrl Pts',(18.7947475334652,-21.0681282421389,-0.507288670837602));
#89226=CARTESIAN_POINT('Ctrl Pts',(18.7222522711166,-21.0702093581544,-0.511677762471143));
#89227=CARTESIAN_POINT('Ctrl Pts',(18.6495091063873,-21.0685648466706,-0.516066854104684));
#89228=CARTESIAN_POINT('Ctrl Pts',(18.5769328970345,-21.0631653002941,-0.520455945738225));
#89229=CARTESIAN_POINT('Ctrl Pts',(18.5044640538338,-21.0577737417766,-0.524838544336596));
#89230=CARTESIAN_POINT('Ctrl Pts',(18.4321621525778,-21.0486382115291,-0.529221142934967));
#89231=CARTESIAN_POINT('Ctrl Pts',(18.3604434250555,-21.0357812949817,-0.533603741533338));
#89232=CARTESIAN_POINT('Ctrl Pts',(18.2888085422895,-21.0229394091672,-0.537981216533954));
#89233=CARTESIAN_POINT('Ctrl Pts',(18.2177559511464,-21.0063848642472,-0.54235869153457));
#89234=CARTESIAN_POINT('Ctrl Pts',(18.1476964269545,-20.9861920067275,-0.546736166535186));
#89235=CARTESIAN_POINT('Ctrl Pts',(18.0776810830246,-20.966011883033,-0.551110881054696));
#89236=CARTESIAN_POINT('Ctrl Pts',(18.0086580256525,-20.9421981323211,-0.555485595574205));
#89237=CARTESIAN_POINT('Ctrl Pts',(17.9410261110428,-20.9148758013262,-0.559860310093715));
#89238=CARTESIAN_POINT('Ctrl Pts',(17.8734145608305,-20.8875616972581,-0.564233707359007));
#89239=CARTESIAN_POINT('Ctrl Pts',(17.8071937685408,-20.8567412908305,-0.568607104624299));
#89240=CARTESIAN_POINT('Ctrl Pts',(17.742744149092,-20.8225883668089,-0.572980501889591));
#89241=CARTESIAN_POINT('Ctrl Pts',(17.6782926999987,-20.7884344732282,-0.577354023310197));
#89242=CARTESIAN_POINT('Ctrl Pts',(17.6156129486707,-20.7509481017458,-0.581727544730802));
#89243=CARTESIAN_POINT('Ctrl Pts',(17.5550606677985,-20.7103489559778,-0.586101066151407));
#89244=CARTESIAN_POINT('Ctrl Pts',(17.494445385749,-20.6697075691258,-0.590479137970353));
#89245=CARTESIAN_POINT('Ctrl Pts',(17.4359623948806,-20.6259472108894,-0.594857209789298));
#89246=CARTESIAN_POINT('Ctrl Pts',(17.3799377143115,-20.5793304294077,-0.599235281608243));
#89247=CARTESIAN_POINT('Ctrl Pts',(17.3238823352031,-20.5326881044139,-0.603615752377232));
#89248=CARTESIAN_POINT('Ctrl Pts',(17.2702883027459,-20.4831865672914,-0.60799622314622));
#89249=CARTESIAN_POINT('Ctrl Pts',(17.2194457820157,-20.4311262693854,-0.612376693915209));
#89250=CARTESIAN_POINT('Ctrl Pts',(17.1685131321094,-20.3789736835344,-0.616764929999834));
#89251=CARTESIAN_POINT('Ctrl Pts',(17.1203420532452,-20.3242536410107,-0.621153166084459));
#89252=CARTESIAN_POINT('Ctrl Pts',(17.0751829425931,-20.2673003345456,-0.625541402169084));
#89253=CARTESIAN_POINT('Ctrl Pts',(17.0445739735742,-20.228697227267,-0.628515760619068));
#89254=CARTESIAN_POINT('Ctrl Pts',(17.0153478864754,-20.1890687880074,-0.631490119069052));
#89255=CARTESIAN_POINT('Ctrl Pts',(16.987570942693,-20.1485260330615,-0.634464477519036));
#89256=CARTESIAN_POINT('Ctrl Pts',(16.9460065404289,-20.087859338098,-0.638915198666084));
#89257=CARTESIAN_POINT('Ctrl Pts',(16.9075293837875,-20.0249114258276,-0.643365919813133));
#89258=CARTESIAN_POINT('Ctrl Pts',(16.8723941675653,-19.9600241686811,-0.647816640960181));
#89259=CARTESIAN_POINT('Ctrl Pts',(16.8373240479938,-19.8952571311764,-0.652259116048976));
#89260=CARTESIAN_POINT('Ctrl Pts',(16.8055837807463,-19.8285582959246,-0.65670159113777));
#89261=CARTESIAN_POINT('Ctrl Pts',(16.7773849658163,-19.760298588398,-0.661144066226565));
#89262=CARTESIAN_POINT('Ctrl Pts',(16.7661659280022,-19.7331411265748,-0.662911526885215));
#89263=CARTESIAN_POINT('Ctrl Pts',(16.7555069751172,-19.7057369100368,-0.664678987543865));
#89264=CARTESIAN_POINT('Ctrl Pts',(16.7454194499637,-19.6781104571739,-0.666446448202515));
#89265=CARTESIAN_POINT('Origin',(18.734,19.211,0.));
#89266=CARTESIAN_POINT('',(16.7454194502785,18.4848895419639,-21.2464098152238));
#89267=CARTESIAN_POINT('',(16.7454194503473,18.4848895417754,-21.4658225266004));
#89268=CARTESIAN_POINT('',(16.7454194503191,18.4848895418526,0.));
#89269=CARTESIAN_POINT('',(16.617000615865,19.2093852021581,-21.5109437210328));
#89270=CARTESIAN_POINT('Ctrl Pts',(16.7454194503473,18.4848895417754,-21.4658225266004));
#89271=CARTESIAN_POINT('Ctrl Pts',(16.7444837857047,18.4874520231283,-21.4659708484036));
#89272=CARTESIAN_POINT('Ctrl Pts',(16.7435530647692,18.4900163385141,-21.4661192068269));
#89273=CARTESIAN_POINT('Ctrl Pts',(16.7287346786323,18.5310912408272,-21.4684945740052));
#89274=CARTESIAN_POINT('Ctrl Pts',(16.7159623155329,18.5699940118298,-21.4707298273544));
#89275=CARTESIAN_POINT('Ctrl Pts',(16.6989532213983,18.6273640677302,-21.4740349431173));
#89276=CARTESIAN_POINT('Ctrl Pts',(16.6938233211382,18.6455573547552,-21.4750843617813));
#89277=CARTESIAN_POINT('Ctrl Pts',(16.6733049261105,18.7222435064227,-21.4795220655559));
#89278=CARTESIAN_POINT('Ctrl Pts',(16.660184570789,18.7813079897161,-21.4829745480814));
#89279=CARTESIAN_POINT('Ctrl Pts',(16.6480276910104,18.8497652108745,-21.4870987813877));
#89280=CARTESIAN_POINT('Ctrl Pts',(16.6465012109118,18.8586935344976,-21.4876390532542));
#89281=CARTESIAN_POINT('Ctrl Pts',(16.6443057399693,18.8720502176631,-21.4884512204757));
#89282=CARTESIAN_POINT('Ctrl Pts',(16.6435934062264,18.8764714852112,-21.4887207018453));
#89283=CARTESIAN_POINT('Ctrl Pts',(16.6423404486739,18.8844085510691,-21.4892056795517));
#89284=CARTESIAN_POINT('Ctrl Pts',(16.6417946532296,18.8879234771593,-21.4894208785406));
#89285=CARTESIAN_POINT('Ctrl Pts',(16.6407480096736,18.8947777570967,-21.489841359319));
#89286=CARTESIAN_POINT('Ctrl Pts',(16.6402462936361,18.8981169249839,-21.4900465848015));
#89287=CARTESIAN_POINT('Ctrl Pts',(16.6391505510578,18.9055302987083,-21.490503036673));
#89288=CARTESIAN_POINT('Ctrl Pts',(16.6385604188792,18.9096050541868,-21.4907544778999));
#89289=CARTESIAN_POINT('Ctrl Pts',(16.6371205628663,18.9197556620745,-21.4913821743024));
#89290=CARTESIAN_POINT('Ctrl Pts',(16.6362853629232,18.9258334915099,-21.4917592042927));
#89291=CARTESIAN_POINT('Ctrl Pts',(16.6323979093108,18.9550643923089,-21.4935779299754));
#89292=CARTESIAN_POINT('Ctrl Pts',(16.6297026242297,18.9782623033748,-21.495037625376));
#89293=CARTESIAN_POINT('Ctrl Pts',(16.620518749016,19.0706094574266,-21.5009008934511));
#89294=CARTESIAN_POINT('Ctrl Pts',(16.6170514760726,19.1400099214158,-21.50542257889));
#89295=CARTESIAN_POINT('Ctrl Pts',(16.6170005689228,19.209447963039,-21.5099894604535));
#89296=CARTESIAN_POINT('',(20.3539256943888,17.8480877707428,-22.));
#89297=CARTESIAN_POINT('Ctrl Pts',(16.617000615865,19.2093852021581,-21.5109437210328));
#89298=CARTESIAN_POINT('Ctrl Pts',(16.6169439839438,19.283629630336,-21.5154240901546));
#89299=CARTESIAN_POINT('Ctrl Pts',(16.6207979179101,19.3580185411302,-21.5199044592764));
#89300=CARTESIAN_POINT('Ctrl Pts',(16.6285774612815,19.4320993746177,-21.5243848283982));
#89301=CARTESIAN_POINT('Ctrl Pts',(16.6360763258001,19.5035074389758,-21.5287035498749));
#89302=CARTESIAN_POINT('Ctrl Pts',(16.6472223384959,19.5746287285795,-21.5330222713516));
#89303=CARTESIAN_POINT('Ctrl Pts',(16.6619760547724,19.6450573353873,-21.5373409928283));
#89304=CARTESIAN_POINT('Ctrl Pts',(16.6767199425251,19.7154390245761,-21.5416568372905));
#89305=CARTESIAN_POINT('Ctrl Pts',(16.6950666677318,19.7851284610469,-21.5459726817526));
#89306=CARTESIAN_POINT('Ctrl Pts',(16.7169252865665,19.8537274697937,-21.5502885262148));
#89307=CARTESIAN_POINT('Ctrl Pts',(16.73877701468,19.9223048533567,-21.5546030101481));
#89308=CARTESIAN_POINT('Ctrl Pts',(16.7641382890675,19.9897920183359,-21.5589174940814));
#89309=CARTESIAN_POINT('Ctrl Pts',(16.7928681454194,20.05580537589,-21.5632319780147));
#89310=CARTESIAN_POINT('Ctrl Pts',(16.8215990265588,20.1218210881255,-21.5675466158447));
#89311=CARTESIAN_POINT('Ctrl Pts',(16.8536985269025,20.186362434556,-21.5718612536747));
#89312=CARTESIAN_POINT('Ctrl Pts',(16.8889780731175,20.2490669965483,-21.5761758915047));
#89313=CARTESIAN_POINT('Ctrl Pts',(16.9242925085236,20.3118335692998,-21.5804947962326));
#89314=CARTESIAN_POINT('Ctrl Pts',(16.9627930183938,20.3727593011758,-21.5848137009605));
#89315=CARTESIAN_POINT('Ctrl Pts',(17.0042462838075,20.4315085338981,-21.5891326056885));
#89316=CARTESIAN_POINT('Ctrl Pts',(17.0457242048903,20.4902927096252,-21.5934540792245));
#89317=CARTESIAN_POINT('Ctrl Pts',(17.0901580661956,20.546897422732,-21.5977755527606));
#89318=CARTESIAN_POINT('Ctrl Pts',(17.1372743798887,20.6010202495217,-21.6020970262967));
#89319=CARTESIAN_POINT('Ctrl Pts',(17.1844652826668,20.6552287572955,-21.6064253410887));
#89320=CARTESIAN_POINT('Ctrl Pts',(17.2343467602729,20.7069471894049,-21.6107536558806));
#89321=CARTESIAN_POINT('Ctrl Pts',(17.2866094610681,20.7559108802162,-21.6150819706726));
#89322=CARTESIAN_POINT('Ctrl Pts',(17.3002562194486,20.7686962060366,-21.6162121737669));
#89323=CARTESIAN_POINT('Ctrl Pts',(17.3140651710174,20.7812939269501,-21.6173423768613));
#89324=CARTESIAN_POINT('Ctrl Pts',(17.3280304725231,20.7936998097575,-21.6184725799557));
#89325=CARTESIAN_POINT('Ctrl Pts',(17.3823193345552,20.8419265709082,-21.62286614352));
#89326=CARTESIAN_POINT('Ctrl Pts',(17.4391954779977,20.8874483717554,-21.6272597070843));
#89327=CARTESIAN_POINT('Ctrl Pts',(17.4983585908499,20.9299762383447,-21.6316532706486));
#89328=CARTESIAN_POINT('Ctrl Pts',(17.5574354044305,20.9724420709446,-21.6360404254673));
#89329=CARTESIAN_POINT('Ctrl Pts',(17.618792177104,21.011922361068,-21.6404275802861));
#89330=CARTESIAN_POINT('Ctrl Pts',(17.6820942417089,21.0481671877306,-21.6448147351048));
#89331=CARTESIAN_POINT('Ctrl Pts',(17.7453238390215,21.0843705218375,-21.6491968675719));
#89332=CARTESIAN_POINT('Ctrl Pts',(17.8104938888271,21.1173455129229,-21.6535790000389));
#89333=CARTESIAN_POINT('Ctrl Pts',(17.877240743402,21.1468854760118,-21.657961132506));
#89334=CARTESIAN_POINT('Ctrl Pts',(17.9439464566845,21.1764072313176,-21.662340563923));
#89335=CARTESIAN_POINT('Ctrl Pts',(18.0122266074123,21.2024979658372,-21.6667199953401));
#89336=CARTESIAN_POINT('Ctrl Pts',(18.0816942022227,21.2249975536693,-21.6710994267571));
#89337=CARTESIAN_POINT('Ctrl Pts',(18.1511417219742,21.2474906394691,-21.6754775925863));
#89338=CARTESIAN_POINT('Ctrl Pts',(18.2217755472184,21.2663944910457,-21.6798557584155));
#89339=CARTESIAN_POINT('Ctrl Pts',(18.293191587477,21.2815982090809,-21.6842339242447));
#89340=CARTESIAN_POINT('Ctrl Pts',(18.3646103699649,21.2968025109076,-21.6886122581865));
#89341=CARTESIAN_POINT('Ctrl Pts',(18.4368109563363,21.3083062989017,-21.6929905921282));
#89342=CARTESIAN_POINT('Ctrl Pts',(18.5093787087696,21.3160497085641,-21.69736892607));
#89343=CARTESIAN_POINT('Ctrl Pts',(18.5820224137337,21.3238012228122,-21.7017518425644));
#89344=CARTESIAN_POINT('Ctrl Pts',(18.6550335728178,21.3277844496845,-21.7061347590588));
#89345=CARTESIAN_POINT('Ctrl Pts',(18.7279928778285,21.3279914771872,-21.7105176755531));
#89346=CARTESIAN_POINT('Ctrl Pts',(18.8009925375781,21.3281986191995,-21.7149030162955));
#89347=CARTESIAN_POINT('Ctrl Pts',(18.8739398055028,21.3246254266109,-21.7192883570379));
#89348=CARTESIAN_POINT('Ctrl Pts',(18.9464185362625,21.3173160649466,-21.7236736977803));
#89349=CARTESIAN_POINT('Ctrl Pts',(19.0190253583242,21.3099937854836,-21.7280667887137));
#89350=CARTESIAN_POINT('Ctrl Pts',(19.0911615138916,21.2989222240549,-21.7324598796471));
#89351=CARTESIAN_POINT('Ctrl Pts',(19.1624196844616,21.2841969452915,-21.7368529705805));
#89352=CARTESIAN_POINT('Ctrl Pts',(19.2099750592608,21.2743697753681,-21.7397847759327));
#89353=CARTESIAN_POINT('Ctrl Pts',(19.2571396374613,21.2629163751623,-21.7427165812849));
#89354=CARTESIAN_POINT('Ctrl Pts',(19.3037966250894,21.2498773396251,-21.7456483866371));
#89355=CARTESIAN_POINT('Ctrl Pts',(19.3728942477398,21.2305669125471,-21.7499903038977));
#89356=CARTESIAN_POINT('Ctrl Pts',(19.4411602368598,21.2076975140762,-21.7543322211583));
#89357=CARTESIAN_POINT('Ctrl Pts',(19.5081959039851,21.1813577599646,-21.7586741384189));
#89358=CARTESIAN_POINT('Ctrl Pts',(19.5751306276509,21.1550576687074,-21.7630095175459));
#89359=CARTESIAN_POINT('Ctrl Pts',(19.6408382497924,21.1252977672376,-21.7673448966729));
#89360=CARTESIAN_POINT('Ctrl Pts',(19.7049335619748,21.0922168982419,-21.7716802757999));
#89361=CARTESIAN_POINT('Ctrl Pts',(19.7689552079216,21.0591740498597,-21.7760106721746));
#89362=CARTESIAN_POINT('Ctrl Pts',(19.8313677860799,21.0228180350837,-21.7803410685494));
#89363=CARTESIAN_POINT('Ctrl Pts',(19.8918061585171,20.9833357185646,-21.7846714649241));
#89364=CARTESIAN_POINT('Ctrl Pts',(19.9522073873422,20.9438776666937,-21.7889991999671));
#89365=CARTESIAN_POINT('Ctrl Pts',(20.0106364037878,20.9012973912839,-21.79332693501));
#89366=CARTESIAN_POINT('Ctrl Pts',(20.0667541884382,20.8558268216443,-21.797654670053));
#89367=CARTESIAN_POINT('Ctrl Pts',(20.1228569262381,20.8103684440195,-21.8019812447012));
#89368=CARTESIAN_POINT('Ctrl Pts',(20.1766492784224,20.7620216199763,-21.8063078193494));
#89369=CARTESIAN_POINT('Ctrl Pts',(20.2278241391937,20.7110594792081,-21.8106343939976));
#89370=CARTESIAN_POINT('Ctrl Pts',(20.2790030075947,20.6600933474689,-21.8149613074705));
#89371=CARTESIAN_POINT('Ctrl Pts',(20.3275636296709,20.6065118422404,-21.8192882209435));
#89372=CARTESIAN_POINT('Ctrl Pts',(20.3732360242913,20.550624670072,-21.8236151344164));
#89373=CARTESIAN_POINT('Ctrl Pts',(20.4189632278337,20.4946704307904,-21.8279472403796));
#89374=CARTESIAN_POINT('Ctrl Pts',(20.4617949724119,20.436405384436,-21.8322793463428));
#89375=CARTESIAN_POINT('Ctrl Pts',(20.5015024142213,20.3761713246222,-21.836611452306));
#89376=CARTESIAN_POINT('Ctrl Pts',(20.541234362149,20.3159000903411,-21.8409462319015));
#89377=CARTESIAN_POINT('Ctrl Pts',(20.5778379231948,20.253657851612,-21.845281011497));
#89378=CARTESIAN_POINT('Ctrl Pts',(20.6111298851782,20.1898117255995,-21.8496157910926));
#89379=CARTESIAN_POINT('Ctrl Pts',(20.6444888929844,20.1258370215219,-21.8539593003889));
#89380=CARTESIAN_POINT('Ctrl Pts',(20.6745227819993,20.0602524303901,-21.8583028096851));
#89381=CARTESIAN_POINT('Ctrl Pts',(20.7010964440932,19.9934452566384,-21.8626463189814));
#89382=CARTESIAN_POINT('Ctrl Pts',(20.7218525789006,19.9412635626139,-21.8660389437605));
#89383=CARTESIAN_POINT('Ctrl Pts',(20.7404986559915,19.8883364226189,-21.8694315685395));
#89384=CARTESIAN_POINT('Ctrl Pts',(20.7569919001287,19.8348531654274,-21.8728241933186));
#89385=CARTESIAN_POINT('Ctrl Pts',(20.7789190860527,19.7637490627714,-21.8773345682141));
#89386=CARTESIAN_POINT('Ctrl Pts',(20.7971283710036,19.6913742316258,-21.8818449431095));
#89387=CARTESIAN_POINT('Ctrl Pts',(20.8114804792732,19.6181410790364,-21.886355318005));
#89388=CARTESIAN_POINT('Ctrl Pts',(20.8265479701327,19.54125761101,-21.8910905130881));
#89389=CARTESIAN_POINT('Ctrl Pts',(20.8373635164913,19.4634284696821,-21.8958257081712));
#89390=CARTESIAN_POINT('Ctrl Pts',(20.8438247940449,19.3851503328552,-21.9005609032544));
#89391=CARTESIAN_POINT('Ctrl Pts',(20.8499588376022,19.3108366237006,-21.9050562824811));
#89392=CARTESIAN_POINT('Ctrl Pts',(20.8521688454906,19.2361188075755,-21.9095516617078));
#89393=CARTESIAN_POINT('Ctrl Pts',(20.8504196160406,19.1614317759201,-21.9140470409345));
#89394=CARTESIAN_POINT('Ctrl Pts',(20.8486720313618,19.0868149712324,-21.9185381932313));
#89395=CARTESIAN_POINT('Ctrl Pts',(20.8429726196327,19.0122293415783,-21.923029345528));
#89396=CARTESIAN_POINT('Ctrl Pts',(20.8333381899733,18.9381114437731,-21.9275204978248));
#89397=CARTESIAN_POINT('Ctrl Pts',(20.823710302195,18.8640438728158,-21.9320086005809));
#89398=CARTESIAN_POINT('Ctrl Pts',(20.8101527670998,18.7904438474655,-21.9364967033371));
#89399=CARTESIAN_POINT('Ctrl Pts',(20.7927342525461,18.7177431932619,-21.9409848060932));
#89400=CARTESIAN_POINT('Ctrl Pts',(20.7753230186655,18.6450729268217,-21.945471032891));
#89401=CARTESIAN_POINT('Ctrl Pts',(20.7540541207903,18.5733017207355,-21.9499572596887));
#89402=CARTESIAN_POINT('Ctrl Pts',(20.7290471325623,18.502850341485,-21.9544434864864));
#89403=CARTESIAN_POINT('Ctrl Pts',(20.7040370351564,18.432390202848,-21.9589302710673));
#89404=CARTESIAN_POINT('Ctrl Pts',(20.6752880624039,18.3632506455487,-21.9634170556482));
#89405=CARTESIAN_POINT('Ctrl Pts',(20.6429691045691,18.2958355569623,-21.9679038402291));
#89406=CARTESIAN_POINT('Ctrl Pts',(20.6106485910926,18.228417223416,-21.9723908407771));
#89407=CARTESIAN_POINT('Ctrl Pts',(20.5747579519087,18.1627239264085,-21.976877841325));
#89408=CARTESIAN_POINT('Ctrl Pts',(20.5355127633241,18.099136355671,-21.9813648418729));
#89409=CARTESIAN_POINT('Ctrl Pts',(20.4962404866784,18.0355048951203,-21.9858549394666));
#89410=CARTESIAN_POINT('Ctrl Pts',(20.4536092807961,17.9739824418484,-21.9903450370603));
#89411=CARTESIAN_POINT('Ctrl Pts',(20.4078784777144,17.914921359699,-21.994835134654));
#89412=CARTESIAN_POINT('Ctrl Pts',(20.3903440822918,17.892275783879,-21.996556756436));
#89413=CARTESIAN_POINT('Ctrl Pts',(20.3723544291116,17.8699917351007,-21.998278378218));
#89414=CARTESIAN_POINT('Ctrl Pts',(20.3539256943888,17.8480877707428,-22.));
#89415=CARTESIAN_POINT('',(17.1140599594606,17.8481048224249,-21.9999997809097));
#89416=CARTESIAN_POINT('Origin',(18.734,19.211,-22.));
#89417=CARTESIAN_POINT('',(16.6170002905214,19.2098909158485,-21.2890562790225));
#89418=CARTESIAN_POINT('Ctrl Pts',(17.1140599594606,17.8481048224249,-21.9999997809097));
#89419=CARTESIAN_POINT('Ctrl Pts',(17.1607068911252,17.7926601825033,-21.9956147575322));
#89420=CARTESIAN_POINT('Ctrl Pts',(17.2102952620655,17.739504224746,-21.9912297341546));
#89421=CARTESIAN_POINT('Ctrl Pts',(17.2625716911555,17.6889659228745,-21.9868447107771));
#89422=CARTESIAN_POINT('Ctrl Pts',(17.3147705007786,17.6385026597179,-21.9824661982341));
#89423=CARTESIAN_POINT('Ctrl Pts',(17.3696491012488,17.5906496701831,-21.9780876856911));
#89424=CARTESIAN_POINT('Ctrl Pts',(17.4269143514077,17.5457023967939,-21.9737091731481));
#89425=CARTESIAN_POINT('Ctrl Pts',(17.4841122081179,17.5008080202619,-21.9693358135217));
#89426=CARTESIAN_POINT('Ctrl Pts',(17.5436907567674,17.4588128636585,-21.9649624538953));
#89427=CARTESIAN_POINT('Ctrl Pts',(17.605321823504,17.4199738768232,-21.960589094269));
#89428=CARTESIAN_POINT('Ctrl Pts',(17.6669138937314,17.3811594650113,-21.956218501847));
#89429=CARTESIAN_POINT('Ctrl Pts',(17.7305554975065,17.3454975176011,-21.951847909425));
#89430=CARTESIAN_POINT('Ctrl Pts',(17.7958885256649,17.3132023654455,-21.947477317003));
#89431=CARTESIAN_POINT('Ctrl Pts',(17.8612018513836,17.2809169525184,-21.9431080426178));
#89432=CARTESIAN_POINT('Ctrl Pts',(17.9282051559123,17.2519965330214,-21.9387387682326));
#89433=CARTESIAN_POINT('Ctrl Pts',(17.9965162100301,17.2266092472671,-21.9343694938474));
#89434=CARTESIAN_POINT('Ctrl Pts',(18.0648292857548,17.2012212101981,-21.9300000901573));
#89435=CARTESIAN_POINT('Ctrl Pts',(18.1344497342609,17.179366680706,-21.9256306864672));
#89436=CARTESIAN_POINT('Ctrl Pts',(18.2049774492685,17.1611648503313,-21.9212612827771));
#89437=CARTESIAN_POINT('Ctrl Pts',(18.275576959088,17.142944491113,-21.9168874311828));
#89438=CARTESIAN_POINT('Ctrl Pts',(18.3470851103194,17.1283843746466,-21.9125135795885));
#89439=CARTESIAN_POINT('Ctrl Pts',(18.4190896618186,17.1175529672556,-21.9081397279943));
#89440=CARTESIAN_POINT('Ctrl Pts',(18.4911340360637,17.1067155694601,-21.9037634574032));
#89441=CARTESIAN_POINT('Ctrl Pts',(18.5636748760598,17.0996110331389,-21.8993871868121));
#89442=CARTESIAN_POINT('Ctrl Pts',(18.6362955339105,17.0962558458986,-21.895010916221));
#89443=CARTESIAN_POINT('Ctrl Pts',(18.7090403295018,17.0928949233017,-21.8906271648337));
#89444=CARTESIAN_POINT('Ctrl Pts',(18.7818647321215,17.0932961427629,-21.8862434134464));
#89445=CARTESIAN_POINT('Ctrl Pts',(18.8543534992707,17.0974238752263,-21.8818596620591));
#89446=CARTESIAN_POINT('Ctrl Pts',(18.8963594228442,17.0998158211955,-21.879319357775));
#89447=CARTESIAN_POINT('Ctrl Pts',(18.9382527448405,17.103458157136,-21.8767790534908));
#89448=CARTESIAN_POINT('Ctrl Pts',(18.9799541720406,17.1083360836178,-21.8742387492067));
#89449=CARTESIAN_POINT('Ctrl Pts',(19.0521148556278,17.1167769100605,-21.8698429741465));
#89450=CARTESIAN_POINT('Ctrl Pts',(19.1239758590327,17.1289525413789,-21.8654471990862));
#89451=CARTESIAN_POINT('Ctrl Pts',(19.1951213352851,17.1448305698358,-21.861051424026));
#89452=CARTESIAN_POINT('Ctrl Pts',(19.2661639857042,17.1606856499397,-21.8566620021347));
#89453=CARTESIAN_POINT('Ctrl Pts',(19.3364926969102,17.1802323993941,-21.8522725802435));
#89454=CARTESIAN_POINT('Ctrl Pts',(19.4056979848776,17.2033867859791,-21.8478831583522));
#89455=CARTESIAN_POINT('Ctrl Pts',(19.4748252563206,17.2265150701546,-21.8434986847453));
#89456=CARTESIAN_POINT('Ctrl Pts',(19.5428311670215,17.2532427601722,-21.8391142111383));
#89457=CARTESIAN_POINT('Ctrl Pts',(19.6093192809603,17.2834354339272,-21.8347297375313));
#89458=CARTESIAN_POINT('Ctrl Pts',(19.6757671116488,17.3136098148032,-21.8303479203518));
#89459=CARTESIAN_POINT('Ctrl Pts',(19.7406985339571,17.3472448153046,-21.8259661031722));
#89460=CARTESIAN_POINT('Ctrl Pts',(19.8037363887647,17.3841576262434,-21.8215842859927));
#89461=CARTESIAN_POINT('Ctrl Pts',(19.8667566375372,17.4210601276904,-21.8172036926242));
#89462=CARTESIAN_POINT('Ctrl Pts',(19.9278839545639,17.4612383791652,-21.8128230992558));
#89463=CARTESIAN_POINT('Ctrl Pts',(19.9867665975567,17.5044640783018,-21.8084425058873));
#89464=CARTESIAN_POINT('Ctrl Pts',(20.0456520241437,17.5476918208727,-21.8040617054325));
#89465=CARTESIAN_POINT('Ctrl Pts',(20.1022921799,17.5939670112651,-21.7996809049776));
#89466=CARTESIAN_POINT('Ctrl Pts',(20.156366438267,17.6430195424395,-21.7953001045228));
#89467=CARTESIAN_POINT('Ctrl Pts',(20.2104978161903,17.6921238886346,-21.7909146765541));
#89468=CARTESIAN_POINT('Ctrl Pts',(20.2620575288253,17.7440111093862,-21.7865292485854));
#89469=CARTESIAN_POINT('Ctrl Pts',(20.3107606507593,17.7983730675734,-21.7821438206167));
#89470=CARTESIAN_POINT('Ctrl Pts',(20.3594910179605,17.8527654366668,-21.777755939373));
#89471=CARTESIAN_POINT('Ctrl Pts',(20.4053613108282,17.9096349255095,-21.7733680581292));
#89472=CARTESIAN_POINT('Ctrl Pts',(20.4481276048669,17.9686411330726,-21.7689801768854));
#89473=CARTESIAN_POINT('Ctrl Pts',(20.4909696354496,18.0277518370932,-21.7645845249669));
#89474=CARTESIAN_POINT('Ctrl Pts',(20.5306964282269,18.0890064129735,-21.7601888730484));
#89475=CARTESIAN_POINT('Ctrl Pts',(20.56710831572,18.1520368737118,-21.7557932211298));
#89476=CARTESIAN_POINT('Ctrl Pts',(20.5912144042082,18.1937654950115,-21.7528831282617));
#89477=CARTESIAN_POINT('Ctrl Pts',(20.6138685324289,18.2362719576463,-21.7499730353935));
#89478=CARTESIAN_POINT('Ctrl Pts',(20.6350243872034,18.2794446987657,-21.7470629425253));
#89479=CARTESIAN_POINT('Ctrl Pts',(20.6668849874923,18.3444626081263,-21.7426803587599));
#89480=CARTESIAN_POINT('Ctrl Pts',(20.6954698849173,18.4112469909798,-21.7382977749946));
#89481=CARTESIAN_POINT('Ctrl Pts',(20.720580017359,18.4794339847767,-21.7339151912293));
#89482=CARTESIAN_POINT('Ctrl Pts',(20.7456523700338,18.5475183869707,-21.7295392013357));
#89483=CARTESIAN_POINT('Ctrl Pts',(20.7672601692967,18.6170007611369,-21.7251632114421));
#89484=CARTESIAN_POINT('Ctrl Pts',(20.7852510315621,18.6874943118595,-21.7207872215485));
#89485=CARTESIAN_POINT('Ctrl Pts',(20.8032203398046,18.7579034075081,-21.7164164743267));
#89486=CARTESIAN_POINT('Ctrl Pts',(20.8175811995767,18.8293208069692,-21.7120457271049));
#89487=CARTESIAN_POINT('Ctrl Pts',(20.8282305540802,18.9013431151147,-21.7076749798831));
#89488=CARTESIAN_POINT('Ctrl Pts',(20.838873012161,18.9733187822846,-21.7033070631165));
#89489=CARTESIAN_POINT('Ctrl Pts',(20.8458086628383,19.0458981036007,-21.6989391463499));
#89490=CARTESIAN_POINT('Ctrl Pts',(20.848985506631,19.1186674123577,-21.6945712295833));
#89491=CARTESIAN_POINT('Ctrl Pts',(20.8521613485358,19.1914137717031,-21.6902046903359));
#89492=CARTESIAN_POINT('Ctrl Pts',(20.8515807156441,19.2643495165153,-21.6858381510884));
#89493=CARTESIAN_POINT('Ctrl Pts',(20.8472435998573,19.3370574776133,-21.681471611841));
#89494=CARTESIAN_POINT('Ctrl Pts',(20.8429064110345,19.4097666630956,-21.6771049990621));
#89495=CARTESIAN_POINT('Ctrl Pts',(20.8348126445421,19.4822475744202,-21.6727383862833));
#89496=CARTESIAN_POINT('Ctrl Pts',(20.8230142986461,19.5540863740405,-21.6683717735044));
#89497=CARTESIAN_POINT('Ctrl Pts',(20.8112037407264,19.6259995312979,-21.664000641009));
#89498=CARTESIAN_POINT('Ctrl Pts',(20.7956810261304,19.6972687714271,-21.6596295085136));
#89499=CARTESIAN_POINT('Ctrl Pts',(20.7765494845939,19.7674895353779,-21.6552583760183));
#89500=CARTESIAN_POINT('Ctrl Pts',(20.7574075663198,19.8377483862984,-21.6508848726687));
#89501=CARTESIAN_POINT('Ctrl Pts',(20.7346530755002,19.906957168973,-21.6465113693192));
#89502=CARTESIAN_POINT('Ctrl Pts',(20.7084387039386,19.9747282267858,-21.6421378659696));
#89503=CARTESIAN_POINT('Ctrl Pts',(20.6821775964101,20.0426201093875,-21.637756565374));
#89504=CARTESIAN_POINT('Ctrl Pts',(20.6524444880472,20.109068706537,-21.6333752647783));
#89505=CARTESIAN_POINT('Ctrl Pts',(20.6194392664437,20.1737085605479,-21.6289939641826));
#89506=CARTESIAN_POINT('Ctrl Pts',(20.5965714078508,20.2184946570858,-21.6259583547363));
#89507=CARTESIAN_POINT('Ctrl Pts',(20.572133749745,20.2624129761557,-21.6229227452901));
#89508=CARTESIAN_POINT('Ctrl Pts',(20.5462048156797,20.3053503579875,-21.6198871358438));
#89509=CARTESIAN_POINT('Ctrl Pts',(20.5087128685692,20.3674356733592,-21.6154977957915));
#89510=CARTESIAN_POINT('Ctrl Pts',(20.4679537734929,20.4277128557231,-21.6111084557392));
#89511=CARTESIAN_POINT('Ctrl Pts',(20.4241273179606,20.4858171041695,-21.6067191156869));
#89512=CARTESIAN_POINT('Ctrl Pts',(20.3803658487493,20.5438351950362,-21.6023362841933));
#89513=CARTESIAN_POINT('Ctrl Pts',(20.3335463361778,20.5996863665837,-21.5979534526998));
#89514=CARTESIAN_POINT('Ctrl Pts',(20.2839130339366,20.6530327968647,-21.5935706212063));
#89515=CARTESIAN_POINT('Ctrl Pts',(20.2343380311571,20.70631656623,-21.5891929378029));
#89516=CARTESIAN_POINT('Ctrl Pts',(20.1819561311663,20.7571010876826,-21.5848152543996));
#89517=CARTESIAN_POINT('Ctrl Pts',(20.1270521616165,20.8050811381531,-21.5804375709962));
#89518=CARTESIAN_POINT('Ctrl Pts',(20.0721830041647,20.8530307666663,-21.5760626632818));
#89519=CARTESIAN_POINT('Ctrl Pts',(20.0147953122166,20.8981791359674,-21.5716877555675));
#89520=CARTESIAN_POINT('Ctrl Pts',(19.9552101005245,20.9402584799205,-21.5673128478531));
#89521=CARTESIAN_POINT('Ctrl Pts',(19.8956430411106,20.9823250046532,-21.5629392729282));
#89522=CARTESIAN_POINT('Ctrl Pts',(19.8338801846224,21.0213240823263,-21.5585656980033));
#89523=CARTESIAN_POINT('Ctrl Pts',(19.7702735544122,21.0570298265266,-21.5541921230784));
#89524=CARTESIAN_POINT('Ctrl Pts',(19.7066653494861,21.0927364546977,-21.5498184398764));
#89525=CARTESIAN_POINT('Ctrl Pts',(19.6412137015734,21.1251493532758,-21.5454447566744));
#89526=CARTESIAN_POINT('Ctrl Pts',(19.574295917344,21.154088204713,-21.5410710734725));
#89527=CARTESIAN_POINT('Ctrl Pts',(19.5073089059773,21.1830569936903,-21.5366928656502));
#89528=CARTESIAN_POINT('Ctrl Pts',(19.4388531734526,21.2085443681914,-21.5323146578279));
#89529=CARTESIAN_POINT('Ctrl Pts',(19.3693259569769,21.2304182153262,-21.5279364500056));
#89530=CARTESIAN_POINT('Ctrl Pts',(19.2997608703362,21.2523039767335,-21.523555857456));
#89531=CARTESIAN_POINT('Ctrl Pts',(19.2291236047978,21.270572171152,-21.5191752649063));
#89532=CARTESIAN_POINT('Ctrl Pts',(19.1578238757517,21.2851413457966,-21.5147946723567));
#89533=CARTESIAN_POINT('Ctrl Pts',(19.086398154594,21.2997362652946,-21.5104063389627));
#89534=CARTESIAN_POINT('Ctrl Pts',(19.0143081093411,21.3106190398704,-21.5060180055687));
#89535=CARTESIAN_POINT('Ctrl Pts',(18.9419703140981,21.3177599171367,-21.5016296721748));
#89536=CARTESIAN_POINT('Ctrl Pts',(18.8929666481794,21.3225973491147,-21.4986568911707));
#89537=CARTESIAN_POINT('Ctrl Pts',(18.8438493793155,21.3257186793944,-21.4956841101665));
#89538=CARTESIAN_POINT('Ctrl Pts',(18.7947475234683,21.3271282424259,-21.4927113291624));
#89539=CARTESIAN_POINT('Ctrl Pts',(18.7222522479351,21.3292093584771,-21.4883222368506));
#89540=CARTESIAN_POINT('Ctrl Pts',(18.6495090705527,21.3275648456576,-21.4839331445389));
#89541=CARTESIAN_POINT('Ctrl Pts',(18.576932849213,21.3221652967363,-21.4795440522271));
#89542=CARTESIAN_POINT('Ctrl Pts',(18.5044639937146,21.3167737356532,-21.4751614529316));
#89543=CARTESIAN_POINT('Ctrl Pts',(18.4321620808264,21.3076382016009,-21.4707788536361));
#89544=CARTESIAN_POINT('Ctrl Pts',(18.3604433424476,21.2947812801727,-21.4663962543406));
#89545=CARTESIAN_POINT('Ctrl Pts',(18.2888084484159,21.2819393894075,-21.4620187786179));
#89546=CARTESIAN_POINT('Ctrl Pts',(18.2177558467876,21.2653848384199,-21.4576413028952));
#89547=CARTESIAN_POINT('Ctrl Pts',(18.1476963129808,21.2451919738775,-21.4532638271725));
#89548=CARTESIAN_POINT('Ctrl Pts',(18.0776809591945,21.2250118430934,-21.4488891119159));
#89549=CARTESIAN_POINT('Ctrl Pts',(18.0086578928418,21.2011980843124,-21.4445143966593));
#89550=CARTESIAN_POINT('Ctrl Pts',(17.9410259701971,21.1738757444266,-21.4401396814027));
#89551=CARTESIAN_POINT('Ctrl Pts',(17.8734144117325,21.1465616313814,-21.4357662833863));
#89552=CARTESIAN_POINT('Ctrl Pts',(17.8071936121441,21.1157412151327,-21.43139288537));
#89553=CARTESIAN_POINT('Ctrl Pts',(17.7427439864028,21.0815882805972,-21.4270194873536));
#89554=CARTESIAN_POINT('Ctrl Pts',(17.6782925308258,21.0474343764011,-21.4226459651689));
#89555=CARTESIAN_POINT('Ctrl Pts',(17.6156127740304,21.0099479935908,-21.4182724429842));
#89556=CARTESIAN_POINT('Ctrl Pts',(17.5550604887456,20.9693488359262,-21.4138989207996));
#89557=CARTESIAN_POINT('Ctrl Pts',(17.4944452020835,20.9287074370344,-21.4095208482016));
#89558=CARTESIAN_POINT('Ctrl Pts',(17.4359622076729,20.8849470661681,-21.4051427756037));
#89559=CARTESIAN_POINT('Ctrl Pts',(17.3799375246599,20.8383302716031,-21.4007647030058));
#89560=CARTESIAN_POINT('Ctrl Pts',(17.3238821429895,20.7916879334218,-21.3963842314483));
#89561=CARTESIAN_POINT('Ctrl Pts',(17.2702881090797,20.742186382646,-21.3920037598908));
#89562=CARTESIAN_POINT('Ctrl Pts',(17.2194455880259,20.6901260707491,-21.3876232883333));
#89563=CARTESIAN_POINT('Ctrl Pts',(17.1685129377324,20.637973470818,-21.3832350514533));
#89564=CARTESIAN_POINT('Ctrl Pts',(17.1203418596204,20.5832534138692,-21.3788468145733));
#89565=CARTESIAN_POINT('Ctrl Pts',(17.0751827508733,20.5263000927544,-21.3744585776934));
#89566=CARTESIAN_POINT('Ctrl Pts',(17.0445738577713,20.4876970696618,-21.3714842259559));
#89567=CARTESIAN_POINT('Ctrl Pts',(17.0153478403718,20.4480687194866,-21.3685098742184));
#89568=CARTESIAN_POINT('Ctrl Pts',(16.9875709596013,20.4075260577406,-21.3655355224809));
#89569=CARTESIAN_POINT('Ctrl Pts',(16.9460128341117,20.3468685260888,-21.3610854733995));
#89570=CARTESIAN_POINT('Ctrl Pts',(16.9075410202164,20.283930466216,-21.3566354243181));
#89571=CARTESIAN_POINT('Ctrl Pts',(16.872410100661,20.2190535931582,-21.3521853752368));
#89572=CARTESIAN_POINT('Ctrl Pts',(16.8373354740495,20.1542806772475,-21.3477424568074));
#89573=CARTESIAN_POINT('Ctrl Pts',(16.8055913293712,20.087575522894,-21.3432995383781));
#89574=CARTESIAN_POINT('Ctrl Pts',(16.777389334652,20.0193091637773,-21.3388566199487));
#89575=CARTESIAN_POINT('Ctrl Pts',(16.7492306455235,19.9511476311114,-21.3344205238456));
#89576=CARTESIAN_POINT('Ctrl Pts',(16.7246034665895,19.8814300877347,-21.3299844277425));
#89577=CARTESIAN_POINT('Ctrl Pts',(16.7036730262164,19.8105509815909,-21.3255483316393));
#89578=CARTESIAN_POINT('Ctrl Pts',(16.6827615749465,19.739736180385,-21.3211162601762));
#89579=CARTESIAN_POINT('Ctrl Pts',(16.6655403322362,19.6677623532215,-21.316684188713));
#89580=CARTESIAN_POINT('Ctrl Pts',(16.6521256152427,19.5950417244147,-21.3122521172498));
#89581=CARTESIAN_POINT('Ctrl Pts',(16.6387184405169,19.5223619819308,-21.307822537667));
#89582=CARTESIAN_POINT('Ctrl Pts',(16.6291136261334,19.4489367276423,-21.3033929580842));
#89583=CARTESIAN_POINT('Ctrl Pts',(16.6233766950828,19.3751897217871,-21.2989633785014));
#89584=CARTESIAN_POINT('Ctrl Pts',(16.6190996641549,19.3202094157473,-21.2956610120084));
#89585=CARTESIAN_POINT('Ctrl Pts',(16.6169713926914,19.2650505695404,-21.2923586455155));
#89586=CARTESIAN_POINT('Ctrl Pts',(16.6170002905214,19.2098909158485,-21.2890562790225));
#89587=CARTESIAN_POINT('Ctrl Pts',(16.6170002427963,19.2099860969743,-21.2873807964582));
#89588=CARTESIAN_POINT('Ctrl Pts',(16.6170353690335,19.136643544728,-21.2832143048811));
#89589=CARTESIAN_POINT('Ctrl Pts',(16.6208818290681,19.0633472797757,-21.2791524291455));
#89590=CARTESIAN_POINT('Ctrl Pts',(16.6454751492164,18.828628323952,-21.2662360119634));
#89591=CARTESIAN_POINT('Ctrl Pts',(16.6810081481163,18.6693758580667,-21.257641722875));
#89592=CARTESIAN_POINT('Ctrl Pts',(16.7380003564599,18.5054548669163,-21.24767578307));
#89593=CARTESIAN_POINT('Ctrl Pts',(16.7416702055317,18.4951575047746,-21.2470446570357));
#89594=CARTESIAN_POINT('Ctrl Pts',(16.7454194502785,18.4848895419639,-21.2464098152238));
#89595=CARTESIAN_POINT('Origin',(18.734,19.211,0.));
#89596=CARTESIAN_POINT('',(16.7454193207648,18.4848898966599,-20.4442392307736));
#89597=CARTESIAN_POINT('',(16.7454194503208,18.4848895418481,-20.6683679253911));
#89598=CARTESIAN_POINT('',(16.7454194503191,18.4848895418526,0.));
#89599=CARTESIAN_POINT('Ctrl Pts',(16.7454194503208,18.4848895418481,-20.6683679253911));
#89600=CARTESIAN_POINT('Ctrl Pts',(16.7441348059686,18.4884077652029,-20.6685903690978));
#89601=CARTESIAN_POINT('Ctrl Pts',(16.7428594915517,18.4919294163847,-20.6688125036898));
#89602=CARTESIAN_POINT('Ctrl Pts',(16.7369541254702,18.5083726599832,-20.6698472613802));
#89603=CARTESIAN_POINT('Ctrl Pts',(16.7324403978101,18.5213358962243,-20.6706560331205));
#89604=CARTESIAN_POINT('Ctrl Pts',(16.6991411766923,18.6200512110015,-20.6767637970217));
#89605=CARTESIAN_POINT('Ctrl Pts',(16.6757501909395,18.7075305319096,-20.6818794890831));
#89606=CARTESIAN_POINT('Ctrl Pts',(16.6306360838819,18.9333414187323,-20.6946257313365));
#89607=CARTESIAN_POINT('Ctrl Pts',(16.6168948154794,19.0728053060284,-20.7020607908923));
#89608=CARTESIAN_POINT('Ctrl Pts',(16.617015959299,19.2328903772826,-20.7109057039679));
#89609=CARTESIAN_POINT('Ctrl Pts',(16.617322962857,19.253177071559,-20.7120327766097));
#89610=CARTESIAN_POINT('Ctrl Pts',(16.6196735634269,19.3328182834745,-20.716492044051));
#89611=CARTESIAN_POINT('Ctrl Pts',(16.6239226573551,19.3920751822671,-20.7198852923422));
#89612=CARTESIAN_POINT('Ctrl Pts',(16.6316702786931,19.4599552913066,-20.7239378480795));
#89613=CARTESIAN_POINT('Ctrl Pts',(16.6327408111966,19.4688348488019,-20.7244712559343));
#89614=CARTESIAN_POINT('Ctrl Pts',(16.6344383623655,19.4822018766633,-20.725279541175));
#89615=CARTESIAN_POINT('Ctrl Pts',(16.6350235901553,19.4866946828842,-20.7255521198264));
#89616=CARTESIAN_POINT('Ctrl Pts',(16.6360953412416,19.4947212844047,-20.7260407673693));
#89617=CARTESIAN_POINT('Ctrl Pts',(16.6365763773629,19.4982557595681,-20.7262565239901));
#89618=CARTESIAN_POINT('Ctrl Pts',(16.6376355527491,19.5058936693281,-20.7267240430256));
#89619=CARTESIAN_POINT('Ctrl Pts',(16.638216799776,19.5099965700238,-20.7269759736824));
#89620=CARTESIAN_POINT('Ctrl Pts',(16.6398690489288,19.5214178899476,-20.7276794301417));
#89621=CARTESIAN_POINT('Ctrl Pts',(16.640966352227,19.5287323593995,-20.7281324028595));
#89622=CARTESIAN_POINT('Ctrl Pts',(16.6474610431044,19.5705309000328,-20.7307344299766));
#89623=CARTESIAN_POINT('Ctrl Pts',(16.6536719560285,19.6048809317908,-20.7329253866801));
#89624=CARTESIAN_POINT('Ctrl Pts',(16.6761041950024,19.7135297019645,-20.7399903579684));
#89625=CARTESIAN_POINT('Ctrl Pts',(16.6954799915677,19.787112697731,-20.7449759971092));
#89626=CARTESIAN_POINT('Ctrl Pts',(16.7775784075566,20.0422401502929,-20.7626581998136));
#89627=CARTESIAN_POINT('Ctrl Pts',(16.8609882667792,20.2161881709999,-20.775336111035));
#89628=CARTESIAN_POINT('Ctrl Pts',(16.9785112285705,20.3943876233088,-20.7884543683585));
#89629=CARTESIAN_POINT('Ctrl Pts',(16.9905653835143,20.4120757196994,-20.789759589673));
#89630=CARTESIAN_POINT('Ctrl Pts',(17.007689957475,20.4364029080444,-20.7915596447329));
#89631=CARTESIAN_POINT('Ctrl Pts',(17.0125342137028,20.443198928621,-20.7920630537977));
#89632=CARTESIAN_POINT('Ctrl Pts',(17.0209583857816,20.4548705764766,-20.7929286275569));
#89633=CARTESIAN_POINT('Ctrl Pts',(17.0245192153128,20.4597597971723,-20.7932915220664));
#89634=CARTESIAN_POINT('Ctrl Pts',(17.0319298852457,20.4698439663237,-20.7940406732722));
#89635=CARTESIAN_POINT('Ctrl Pts',(17.0357826741008,20.4750366776866,-20.7944268101332));
#89636=CARTESIAN_POINT('Ctrl Pts',(17.0448502079774,20.4871414292851,-20.7953278534073));
#89637=CARTESIAN_POINT('Ctrl Pts',(17.0500837117351,20.4940393232245,-20.7958420189095));
#89638=CARTESIAN_POINT('Ctrl Pts',(17.0671665107623,20.516270324212,-20.7975015757596));
#89639=CARTESIAN_POINT('Ctrl Pts',(17.0791842625905,20.5314731773975,-20.7986403046101));
#89640=CARTESIAN_POINT('Ctrl Pts',(17.1414400752355,20.6080438292411,-20.8043989483798));
#89641=CARTESIAN_POINT('Ctrl Pts',(17.1948920375782,20.6667222325826,-20.8088862591104));
#89642=CARTESIAN_POINT('Ctrl Pts',(17.367930989628,20.8364655078474,-20.822334799419));
#89643=CARTESIAN_POINT('Ctrl Pts',(17.497141287945,20.9368208092079,-20.8309358220121));
#89644=CARTESIAN_POINT('Ctrl Pts',(17.688822419663,21.0530165625757,-20.8434650797091));
#89645=CARTESIAN_POINT('Ctrl Pts',(17.7424061819017,21.082406269016,-20.8469515340758));
#89646=CARTESIAN_POINT('Ctrl Pts',(17.8053528288565,21.1134685269262,-20.851114699853));
#89647=CARTESIAN_POINT('Ctrl Pts',(17.8135516410907,21.1174487604598,-20.8516582382615));
#89648=CARTESIAN_POINT('Ctrl Pts',(17.8258412984466,21.1233171992305,-20.8524752689664));
#89649=CARTESIAN_POINT('Ctrl Pts',(17.8299130095316,21.1252455460269,-20.8527463345065));
#89650=CARTESIAN_POINT('Ctrl Pts',(17.8372191560455,21.1286771989755,-20.8532334482917));
#89651=CARTESIAN_POINT('Ctrl Pts',(17.8404512609448,21.1301853407614,-20.8534491934587));
#89652=CARTESIAN_POINT('Ctrl Pts',(17.8474673905303,21.1334375913452,-20.8539180889718));
#89653=CARTESIAN_POINT('Ctrl Pts',(17.8512527076603,21.1351786760712,-20.8541714152487));
#89654=CARTESIAN_POINT('Ctrl Pts',(17.8618589949822,21.1400192326833,-20.8548821489742));
#89655=CARTESIAN_POINT('Ctrl Pts',(17.8686912367068,21.1430936501654,-20.8553410489826));
#89656=CARTESIAN_POINT('Ctrl Pts',(17.9088201111944,21.1608955664536,-20.8580419950941));
#89657=CARTESIAN_POINT('Ctrl Pts',(17.94247377324,21.1747974521252,-20.8603296315244));
#89658=CARTESIAN_POINT('Ctrl Pts',(18.0526120484764,21.2170032460245,-20.8678505622547));
#89659=CARTESIAN_POINT('Ctrl Pts',(18.1303749387868,21.2417569011278,-20.8732106832107));
#89660=CARTESIAN_POINT('Ctrl Pts',(18.3869083829587,21.3073779180171,-20.8906947603445));
#89661=CARTESIAN_POINT('Ctrl Pts',(18.5696370348791,21.329557146948,-20.9027594061845));
#89662=CARTESIAN_POINT('Ctrl Pts',(18.775275819617,21.3277152085025,-20.9154088485089));
#89663=CARTESIAN_POINT('Ctrl Pts',(18.7975861840113,21.3271625231044,-20.9167705151485));
#89664=CARTESIAN_POINT('Ctrl Pts',(18.8283705348903,21.325912607305,-20.918635213115));
#89665=CARTESIAN_POINT('Ctrl Pts',(18.8368546841449,21.3255169783263,-20.919147639218));
#89666=CARTESIAN_POINT('Ctrl Pts',(18.8514164671393,21.3247500902328,-20.9200246560591));
#89667=CARTESIAN_POINT('Ctrl Pts',(18.8574952526452,21.3244036515755,-20.9203900205261));
#89668=CARTESIAN_POINT('Ctrl Pts',(18.8700078158497,21.3236363726226,-20.9211405841342));
#89669=CARTESIAN_POINT('Ctrl Pts',(18.8764413407258,21.3232123555106,-20.9215256795733));
#89670=CARTESIAN_POINT('Ctrl Pts',(18.8913808605135,21.3221591626785,-20.9224180679941));
#89671=CARTESIAN_POINT('Ctrl Pts',(18.8998852281543,21.3215079577544,-20.9229246643069));
#89672=CARTESIAN_POINT('Ctrl Pts',(18.9269819601036,21.3192682830074,-20.924534489904));
#89673=CARTESIAN_POINT('Ctrl Pts',(18.9455576820423,21.3174853596041,-20.9256316137445));
#89674=CARTESIAN_POINT('Ctrl Pts',(19.1238298334764,21.2979925299181,-20.9361046018898));
#89675=CARTESIAN_POINT('Ctrl Pts',(19.2810475931405,21.2624024994584,-20.944851978839));
#89676=CARTESIAN_POINT('Ctrl Pts',(19.5595120461599,21.1650354449125,-20.9608717263319));
#89677=CARTESIAN_POINT('Ctrl Pts',(19.6817603834485,21.1087526181623,-20.9681342429073));
#89678=CARTESIAN_POINT('Ctrl Pts',(19.8113926765788,21.0334049665116,-20.9769255568039));
#89679=CARTESIAN_POINT('Ctrl Pts',(19.8248600809897,21.025375675751,-20.9778530679659));
#89680=CARTESIAN_POINT('Ctrl Pts',(19.8431757147607,21.0141782347737,-20.979135784132));
#89681=CARTESIAN_POINT('Ctrl Pts',(19.848102348477,21.0111384579813,-20.9794829513984));
#89682=CARTESIAN_POINT('Ctrl Pts',(19.8559119978043,21.0062754955064,-20.9800367823594));
#89683=CARTESIAN_POINT('Ctrl Pts',(19.8588032234084,21.0044654565429,-20.9802425849317));
#89684=CARTESIAN_POINT('Ctrl Pts',(19.8647631117974,21.0007142146323,-20.9806684349294));
#89685=CARTESIAN_POINT('Ctrl Pts',(19.8678311470892,20.9987721091241,-20.9808885453299));
#89686=CARTESIAN_POINT('Ctrl Pts',(19.8751298005123,20.9941256238551,-20.9814142770803));
#89687=CARTESIAN_POINT('Ctrl Pts',(19.8793558082276,20.9914140763968,-20.9817203715041));
#89688=CARTESIAN_POINT('Ctrl Pts',(19.8935799952022,20.9822157624576,-20.9827562488797));
#89689=CARTESIAN_POINT('Ctrl Pts',(19.9035328190337,20.9756597441554,-20.9834904435821));
#89690=CARTESIAN_POINT('Ctrl Pts',(19.9273113393503,20.9597070902291,-20.9852661621062));
#89691=CARTESIAN_POINT('Ctrl Pts',(19.9410819417546,20.9502301713864,-20.9863123320942));
#89692=CARTESIAN_POINT('Ctrl Pts',(19.9923066907291,20.9140759588294,-20.9902670125705));
#89693=CARTESIAN_POINT('Ctrl Pts',(20.0289987630996,20.886345071146,-20.9932278342395));
#89694=CARTESIAN_POINT('Ctrl Pts',(20.1225691377199,20.8107157722418,-21.0010639092873));
#89695=CARTESIAN_POINT('Ctrl Pts',(20.1778790765798,20.7609766008822,-21.0059869591076));
#89696=CARTESIAN_POINT('Ctrl Pts',(20.3402647246819,20.5986968103234,-21.0211538277651));
#89697=CARTESIAN_POINT('Ctrl Pts',(20.437687782884,20.4771963961483,-21.0312701565337));
#89698=CARTESIAN_POINT('Ctrl Pts',(20.5337906758965,20.3259060871407,-21.0423125560435));
#89699=CARTESIAN_POINT('Ctrl Pts',(20.5462830667372,20.3054826266784,-21.0437748099299));
#89700=CARTESIAN_POINT('Ctrl Pts',(20.5633463681499,20.2764928094153,-21.0458116367639));
#89701=CARTESIAN_POINT('Ctrl Pts',(20.5682085305829,20.268100814879,-21.0463967827793));
#89702=CARTESIAN_POINT('Ctrl Pts',(20.5759804521956,20.2544715625901,-21.0473399793466));
#89703=CARTESIAN_POINT('Ctrl Pts',(20.5789259099059,20.2492549187509,-21.0476993172911));
#89704=CARTESIAN_POINT('Ctrl Pts',(20.5850181695699,20.2383572459213,-21.04844653149));
#89705=CARTESIAN_POINT('Ctrl Pts',(20.588161057374,20.232674091672,-21.0488342642145));
#89706=CARTESIAN_POINT('Ctrl Pts',(20.5955279349209,20.2192069123638,-21.0497485338234));
#89707=CARTESIAN_POINT('Ctrl Pts',(20.5997293508403,20.2114106275309,-21.0502742603779));
#89708=CARTESIAN_POINT('Ctrl Pts',(20.6135045548538,20.1854602837429,-21.0520126115366));
#89709=CARTESIAN_POINT('Ctrl Pts',(20.6228634553418,20.1671930281683,-21.0532176312098));
#89710=CARTESIAN_POINT('Ctrl Pts',(20.6710806053891,20.0696084923807,-21.0595612255425));
#89711=CARTESIAN_POINT('Ctrl Pts',(20.705214565554,19.9880492372561,-21.0645333292169));
#89712=CARTESIAN_POINT('Ctrl Pts',(20.7770398441386,19.7809208602852,-21.0766341031006));
#89713=CARTESIAN_POINT('Ctrl Pts',(20.8083604747271,19.6535480043561,-21.0836115738199));
#89714=CARTESIAN_POINT('Ctrl Pts',(20.8332965312334,19.48679992769,-21.0929118329183));
#89715=CARTESIAN_POINT('Ctrl Pts',(20.83787667287,19.449357379994,-21.0950121627494));
#89716=CARTESIAN_POINT('Ctrl Pts',(20.8458050284077,19.3661528405492,-21.0997434618513));
#89717=CARTESIAN_POINT('Ctrl Pts',(20.848670499354,19.3203658311744,-21.1023896722293));
#89718=CARTESIAN_POINT('Ctrl Pts',(20.8502755330067,19.2669020701046,-21.1055661136968));
#89719=CARTESIAN_POINT('Ctrl Pts',(20.8504631980438,19.2592773280437,-21.1060211745932));
#89720=CARTESIAN_POINT('Ctrl Pts',(20.8506981210273,19.2470456578,-21.1067547148459));
#89721=CARTESIAN_POINT('Ctrl Pts',(20.8507715510948,19.2424392201348,-21.107031768016));
#89722=CARTESIAN_POINT('Ctrl Pts',(20.8508753362342,19.2342515957803,-21.1075256948554));
#89723=CARTESIAN_POINT('Ctrl Pts',(20.8509116410061,19.2306705324151,-21.1077422325706));
#89724=CARTESIAN_POINT('Ctrl Pts',(20.8509695837588,19.223046773013,-21.1082043185131));
#89725=CARTESIAN_POINT('Ctrl Pts',(20.850988728364,19.2190041643376,-21.1084499976598));
#89726=CARTESIAN_POINT('Ctrl Pts',(20.851009275933,19.2080238754976,-21.1091190199955));
#89727=CARTESIAN_POINT('Ctrl Pts',(20.8509881545895,19.2010862745621,-21.1095435926024));
#89728=CARTESIAN_POINT('Ctrl Pts',(20.850706745412,19.1657337806965,-21.1117162145323));
#89729=CARTESIAN_POINT('Ctrl Pts',(20.8499084726236,19.1373275600108,-21.1134918608024));
#89730=CARTESIAN_POINT('Ctrl Pts',(20.8458832247719,19.0539238340679,-21.1187767399629));
#89731=CARTESIAN_POINT('Ctrl Pts',(20.8410811084631,18.9990281919281,-21.1223461858666));
#89732=CARTESIAN_POINT('Ctrl Pts',(20.8165229471249,18.8055808884817,-21.1351170656333));
#89733=CARTESIAN_POINT('Ctrl Pts',(20.785181551683,18.668850858788,-21.1444683302288));
#89734=CARTESIAN_POINT('Ctrl Pts',(20.7117604886859,18.450522780286,-21.1593418081366));
#89735=CARTESIAN_POINT('Ctrl Pts',(20.6774819019281,18.3667583339117,-21.1650403571787));
#89736=CARTESIAN_POINT('Ctrl Pts',(20.631942870125,18.2730818528837,-21.1713957995858));
#89737=CARTESIAN_POINT('Ctrl Pts',(20.6258186638608,18.2607896306808,-21.1722295424608));
#89738=CARTESIAN_POINT('Ctrl Pts',(20.6158043914846,18.2411701042999,-21.1735601263159));
#89739=CARTESIAN_POINT('Ctrl Pts',(20.6119901939496,18.233804713023,-21.1740596096502));
#89740=CARTESIAN_POINT('Ctrl Pts',(20.6051404657361,18.220765807402,-21.1749438456652));
#89741=CARTESIAN_POINT('Ctrl Pts',(20.6021221885951,18.2150833927478,-21.175329201168));
#89742=CARTESIAN_POINT('Ctrl Pts',(20.595778956129,18.2032714937467,-21.1761302720531));
#89743=CARTESIAN_POINT('Ctrl Pts',(20.5924495241137,18.1971444916021,-21.1765458225587));
#89744=CARTESIAN_POINT('Ctrl Pts',(20.5837232567908,18.1812733646736,-21.1776223761956));
#89745=CARTESIAN_POINT('Ctrl Pts',(20.5782796386975,18.1715551040744,-21.1782817014597));
#89746=CARTESIAN_POINT('Ctrl Pts',(20.5542940635624,18.1295163392991,-21.1811348533844));
#89747=CARTESIAN_POINT('Ctrl Pts',(20.5349766564033,18.0976443879412,-21.183300611405));
#89748=CARTESIAN_POINT('Ctrl Pts',(20.4814021730998,18.014297940566,-21.1889868948962));
#89749=CARTESIAN_POINT('Ctrl Pts',(20.4457142261337,17.9637849262658,-21.1924562736943));
#89750=CARTESIAN_POINT('Ctrl Pts',(20.3212210573194,17.8030062838189,-21.2037065296048));
#89751=CARTESIAN_POINT('Ctrl Pts',(20.223580476937,17.7000848238373,-21.2112288528991));
#89752=CARTESIAN_POINT('Ctrl Pts',(20.0589910540881,17.5581737212588,-21.223258989424));
#89753=CARTESIAN_POINT('Ctrl Pts',(19.9989652733674,17.511795401496,-21.2275420500309));
#89754=CARTESIAN_POINT('Ctrl Pts',(19.9287638339729,17.4633390476997,-21.2325973897706));
#89755=CARTESIAN_POINT('Ctrl Pts',(19.920901837859,17.4579901760586,-21.2331641805212));
#89756=CARTESIAN_POINT('Ctrl Pts',(19.9091944341673,17.450139959414,-21.2340095541564));
#89757=CARTESIAN_POINT('Ctrl Pts',(19.9053763767621,17.4475977703068,-21.2342854624305));
#89758=CARTESIAN_POINT('Ctrl Pts',(19.8985631496353,17.4430931889431,-21.2347782479248));
#89759=CARTESIAN_POINT('Ctrl Pts',(19.8955712358379,17.4411259689354,-21.2349947973145));
#89760=CARTESIAN_POINT('Ctrl Pts',(19.8891187543368,17.4369067922628,-21.2354621522842));
#89761=CARTESIAN_POINT('Ctrl Pts',(19.8856566296387,17.4346573942227,-21.2357131168411));
#89762=CARTESIAN_POINT('Ctrl Pts',(19.8760735140468,17.4284708820815,-21.2364082908274));
#89763=CARTESIAN_POINT('Ctrl Pts',(19.869938833672,17.4245552260579,-21.2368538795575));
#89764=CARTESIAN_POINT('Ctrl Pts',(19.8360674586041,17.4031807460777,-21.2393166948758));
#89765=CARTESIAN_POINT('Ctrl Pts',(19.8079500119816,17.3863372265402,-21.2413706024959));
#89766=CARTESIAN_POINT('Ctrl Pts',(19.6371361431522,17.2893284568902,-21.2538526767675));
#89767=CARTESIAN_POINT('Ctrl Pts',(19.4859285474865,17.225280941433,-21.2648702342628));
#89768=CARTESIAN_POINT('Ctrl Pts',(19.2190528685793,17.147143832183,-21.283011092152));
#89769=CARTESIAN_POINT('Ctrl Pts',(19.1068141512045,17.123945737257,-21.2902909633051));
#89770=CARTESIAN_POINT('Ctrl Pts',(18.9790743667114,17.1081849592177,-21.2981493943807));
#89771=CARTESIAN_POINT('Ctrl Pts',(18.9648973957373,17.1065810898969,-21.2990159651469));
#89772=CARTESIAN_POINT('Ctrl Pts',(18.9422909751092,17.1042547815452,-21.3003891248715));
#89773=CARTESIAN_POINT('Ctrl Pts',(18.9338717259411,17.1034393621537,-21.3008986184488));
#89774=CARTESIAN_POINT('Ctrl Pts',(18.9190042014309,17.1020893080248,-21.3017950291876));
#89775=CARTESIAN_POINT('Ctrl Pts',(18.9125579804854,17.1015337380471,-21.3021825985334));
#89776=CARTESIAN_POINT('Ctrl Pts',(18.8992097611272,17.1004449415831,-21.3029829150406));
#89777=CARTESIAN_POINT('Ctrl Pts',(18.8923074835671,17.0999159983141,-21.3033955234339));
#89778=CARTESIAN_POINT('Ctrl Pts',(18.8745622019329,17.0986436410164,-21.3044532160175));
#89779=CARTESIAN_POINT('Ctrl Pts',(18.863715758035,17.0979498470878,-21.3050967408568));
#89780=CARTESIAN_POINT('Ctrl Pts',(18.8182380611991,17.0953923527664,-21.3077829835866));
#89781=CARTESIAN_POINT('Ctrl Pts',(18.7835678675167,17.0942961952269,-21.3098016666494));
#89782=CARTESIAN_POINT('Ctrl Pts',(18.693003011674,17.0936594081099,-21.3150107871875));
#89783=CARTESIAN_POINT('Ctrl Pts',(18.637124974149,17.0954792997746,-21.3181606271481));
#89784=CARTESIAN_POINT('Ctrl Pts',(18.3834491881285,17.1138150099211,-21.3322947095872));
#89785=CARTESIAN_POINT('Ctrl Pts',(18.1885431799121,17.1558775600461,-21.342605255844));
#89786=CARTESIAN_POINT('Ctrl Pts',(17.9724263212463,17.2354715466881,-21.3558294456999));
#89787=CARTESIAN_POINT('Ctrl Pts',(17.9427390876854,17.2471738721778,-21.3576899943198));
#89788=CARTESIAN_POINT('Ctrl Pts',(17.9070441482946,17.2621851007477,-21.3599939118244));
#89789=CARTESIAN_POINT('Ctrl Pts',(17.9007717155182,17.2648586599888,-21.3604013040156));
#89790=CARTESIAN_POINT('Ctrl Pts',(17.8904604959179,17.2693126960198,-21.3610753803084));
#89791=CARTESIAN_POINT('Ctrl Pts',(17.8864141130897,17.2710756084621,-21.3613410179109));
#89792=CARTESIAN_POINT('Ctrl Pts',(17.8791231719682,17.2742792633292,-21.361821717315));
#89793=CARTESIAN_POINT('Ctrl Pts',(17.8758766949128,17.2757155258024,-21.3620365029464));
#89794=CARTESIAN_POINT('Ctrl Pts',(17.8695650932791,17.2785268236595,-21.362455541007));
#89795=CARTESIAN_POINT('Ctrl Pts',(17.8664996722056,17.2799009693586,-21.3626597309355));
#89796=CARTESIAN_POINT('Ctrl Pts',(17.8574560073678,17.2839808797593,-21.3632640922099));
#89797=CARTESIAN_POINT('Ctrl Pts',(17.8514871251231,17.2867071210871,-21.3636655049622));
#89798=CARTESIAN_POINT('Ctrl Pts',(17.8231310026218,17.2998182435485,-21.3655842077487));
#89799=CARTESIAN_POINT('Ctrl Pts',(17.8009148365565,17.3105658416356,-21.3671223586615));
#89800=CARTESIAN_POINT('Ctrl Pts',(17.7387157586516,17.3420096297731,-21.3715176022644));
#89801=CARTESIAN_POINT('Ctrl Pts',(17.699199331507,17.3635956648401,-21.3744154557977));
#89802=CARTESIAN_POINT('Ctrl Pts',(17.578475095543,17.4346308214865,-21.3835372372572));
#89803=CARTESIAN_POINT('Ctrl Pts',(17.4998881911085,17.4883007398057,-21.38986235151));
#89804=CARTESIAN_POINT('Ctrl Pts',(17.3073653770202,17.6397364544719,-21.4060185248264));
#89805=CARTESIAN_POINT('Ctrl Pts',(17.1997103750265,17.7446689067703,-21.4156928981247));
#89806=CARTESIAN_POINT('Ctrl Pts',(17.0950141872719,17.8709947166576,-21.4257089298281));
#89807=CARTESIAN_POINT('Ctrl Pts',(17.0861067058801,17.8819641238075,-21.4265670501198));
#89808=CARTESIAN_POINT('Ctrl Pts',(17.0720934375621,17.899578719601,-21.427926882228));
#89809=CARTESIAN_POINT('Ctrl Pts',(17.0669162429172,17.9061663144287,-21.4284314702998));
#89810=CARTESIAN_POINT('Ctrl Pts',(17.0578483025584,17.917846661631,-21.4293192384057));
#89811=CARTESIAN_POINT('Ctrl Pts',(17.0539413443175,17.9229266386391,-21.4297030642928));
#89812=CARTESIAN_POINT('Ctrl Pts',(17.0459025254215,17.9334778199166,-21.4304956127581));
#89813=CARTESIAN_POINT('Ctrl Pts',(17.041774050096,17.9389515180365,-21.4309041982847));
#89814=CARTESIAN_POINT('Ctrl Pts',(17.0312337451951,17.9530684062924,-21.431951442157));
#89815=CARTESIAN_POINT('Ctrl Pts',(17.0248610484235,17.9617406739723,-21.4325885592966));
#89816=CARTESIAN_POINT('Ctrl Pts',(16.9984529420413,17.9982584079331,-21.4352459079366));
#89817=CARTESIAN_POINT('Ctrl Pts',(16.9790290475874,18.0265410883396,-21.4372424455854));
#89818=CARTESIAN_POINT('Ctrl Pts',(16.9301556403247,18.1015480927593,-21.4423912319857));
#89819=CARTESIAN_POINT('Ctrl Pts',(16.9018312389291,18.148975380904,-21.4455036084188));
#89820=CARTESIAN_POINT('Ctrl Pts',(16.8405503212993,18.2613508687033,-21.4526165738726));
#89821=CARTESIAN_POINT('Ctrl Pts',(16.8090251672351,18.326999033245,-21.4565793428513));
#89822=CARTESIAN_POINT('Ctrl Pts',(16.768406775433,18.4241151244899,-21.4622948417452));
#89823=CARTESIAN_POINT('Ctrl Pts',(16.7565625292272,18.4543722703703,-21.46405612283));
#89824=CARTESIAN_POINT('Ctrl Pts',(16.7454194503473,18.4848895417754,-21.4658225266004));
#89825=CARTESIAN_POINT('Ctrl Pts',(16.7454194502785,18.4848895419639,-21.2464098152238));
#89826=CARTESIAN_POINT('Ctrl Pts',(16.7527638959619,18.4647754922724,-21.245166215107));
#89827=CARTESIAN_POINT('Ctrl Pts',(16.7604130101027,18.4447742578277,-21.243908357521));
#89828=CARTESIAN_POINT('Ctrl Pts',(16.7710464259282,18.4181857438961,-21.2422033215757));
#89829=CARTESIAN_POINT('Ctrl Pts',(16.7737629920154,18.4114926218315,-21.2417712954919));
#89830=CARTESIAN_POINT('Ctrl Pts',(16.778076386766,18.4010193472518,-21.2410906451708));
#89831=CARTESIAN_POINT('Ctrl Pts',(16.7796500728174,18.3972296392127,-21.2408434012105));
#89832=CARTESIAN_POINT('Ctrl Pts',(16.7826138710416,18.3901504835426,-21.240379722062));
#89833=CARTESIAN_POINT('Ctrl Pts',(16.7840012921163,18.3868599684955,-21.2401634505022));
#89834=CARTESIAN_POINT('Ctrl Pts',(16.7871888982541,18.3793531083702,-21.2396683632493));
#89835=CARTESIAN_POINT('Ctrl Pts',(16.7889944540061,18.3751391004608,-21.2393892238339));
#89836=CARTESIAN_POINT('Ctrl Pts',(16.7945891480335,18.3621978617488,-21.2385283034645));
#89837=CARTESIAN_POINT('Ctrl Pts',(16.7984233825829,18.3534904239784,-21.2379438745834));
#89838=CARTESIAN_POINT('Ctrl Pts',(16.8514177160967,18.2353082466656,-21.2299441362284));
#89839=CARTESIAN_POINT('Ctrl Pts',(16.9097358236781,18.1301928946525,-21.2220488041687));
#89840=CARTESIAN_POINT('Ctrl Pts',(17.0373255766414,17.9402392757908,-21.2069315721899));
#89841=CARTESIAN_POINT('Ctrl Pts',(17.1049006033556,17.8546904660381,-21.1997374915614));
#89842=CARTESIAN_POINT('Ctrl Pts',(17.2157140416318,17.7346993717156,-21.1892443898919));
#89843=CARTESIAN_POINT('Ctrl Pts',(17.2542010033776,17.6961232655033,-21.1857967859413));
#89844=CARTESIAN_POINT('Ctrl Pts',(17.3107065019804,17.6436979985561,-21.181006856892));
#89845=CARTESIAN_POINT('Ctrl Pts',(17.3275227324188,17.628589906926,-21.1796131082781));
#89846=CARTESIAN_POINT('Ctrl Pts',(17.3536807704653,17.6058354046499,-21.1774926542392));
#89847=CARTESIAN_POINT('Ctrl Pts',(17.3628509736745,17.5979950680005,-21.176757991135));
#89848=CARTESIAN_POINT('Ctrl Pts',(17.3799856616499,17.5835969800569,-21.1754011419974));
#89849=CARTESIAN_POINT('Ctrl Pts',(17.38793198132,17.5770182642513,-21.1747781082329));
#89850=CARTESIAN_POINT('Ctrl Pts',(17.4010997668257,17.5662779744504,-21.1737557539507));
#89851=CARTESIAN_POINT('Ctrl Pts',(17.406293329267,17.5620826063739,-21.1733550677939));
#89852=CARTESIAN_POINT('Ctrl Pts',(17.4165504002975,17.5538768082451,-21.1725686783795));
#89853=CARTESIAN_POINT('Ctrl Pts',(17.4216125853113,17.5498648472801,-21.1721829161296));
#89854=CARTESIAN_POINT('Ctrl Pts',(17.4333448195624,17.5406537425252,-21.1712942157636));
#89855=CARTESIAN_POINT('Ctrl Pts',(17.4400278479259,17.5354712502974,-21.1707919435669));
#89856=CARTESIAN_POINT('Ctrl Pts',(17.4580877972068,17.5216387894874,-21.1694450867428));
#89857=CARTESIAN_POINT('Ctrl Pts',(17.4695216754146,17.5130636553794,-21.1686034424332));
#89858=CARTESIAN_POINT('Ctrl Pts',(17.5748866282003,17.4356971170166,-21.1609454221046));
#89859=CARTESIAN_POINT('Ctrl Pts',(17.6742615063459,17.3746439131274,-21.154443169733));
#89860=CARTESIAN_POINT('Ctrl Pts',(17.9233755373307,17.2485876644494,-21.1391557000502));
#89861=CARTESIAN_POINT('Ctrl Pts',(18.0765562199388,17.192106719694,-21.1305551663233));
#89862=CARTESIAN_POINT('Ctrl Pts',(18.266459240139,17.1460146277258,-21.1193368266112));
#89863=CARTESIAN_POINT('Ctrl Pts',(18.2984190236616,17.1390376699283,-21.1174292941519));
#89864=CARTESIAN_POINT('Ctrl Pts',(18.3376489249934,17.1314213214243,-21.1150499678368));
#89865=CARTESIAN_POINT('Ctrl Pts',(18.3447792426289,17.1300750004835,-21.1146159886861));
#89866=CARTESIAN_POINT('Ctrl Pts',(18.3559636171692,17.1280227014596,-21.1139326859989));
#89867=CARTESIAN_POINT('Ctrl Pts',(18.3600131283766,17.1272918265339,-21.1136847550195));
#89868=CARTESIAN_POINT('Ctrl Pts',(18.3675825380436,17.1259484398437,-21.1132202884411));
#89869=CARTESIAN_POINT('Ctrl Pts',(18.3711018644598,17.1253330305354,-21.1130039196444));
#89870=CARTESIAN_POINT('Ctrl Pts',(18.3791347787413,17.1239492968614,-21.112509106204));
#89871=CARTESIAN_POINT('Ctrl Pts',(18.3836492936083,17.1231867074972,-21.1122303413077));
#89872=CARTESIAN_POINT('Ctrl Pts',(18.3975214270781,17.1208896943121,-21.111371748493));
#89873=CARTESIAN_POINT('Ctrl Pts',(18.4068867606263,17.1194035186212,-21.1107892932738));
#89874=CARTESIAN_POINT('Ctrl Pts',(18.5359034258415,17.0998176758328,-21.1027298189923));
#89875=CARTESIAN_POINT('Ctrl Pts',(18.6568688960735,17.0919490118058,-21.0947647638725));
#89876=CARTESIAN_POINT('Ctrl Pts',(18.9567054216094,17.0981577753165,-21.0749511707336));
#89877=CARTESIAN_POINT('Ctrl Pts',(19.1344308515458,17.1245244433609,-21.0632060404949));
#89878=CARTESIAN_POINT('Ctrl Pts',(19.3274192740309,17.17875890594,-21.0508913153535));
#89879=CARTESIAN_POINT('Ctrl Pts',(19.3480071303989,17.1848841108301,-21.0495820777288));
#89880=CARTESIAN_POINT('Ctrl Pts',(19.3771084755845,17.1940265418937,-21.0477372462095));
#89881=CARTESIAN_POINT('Ctrl Pts',(19.3857008491468,17.1967863943371,-21.0471932686109));
#89882=CARTESIAN_POINT('Ctrl Pts',(19.4004789189037,17.2016375436408,-21.0462588492245));
#89883=CARTESIAN_POINT('Ctrl Pts',(19.4066730193373,17.203702652593,-21.0458675515026));
#89884=CARTESIAN_POINT('Ctrl Pts',(19.418504608993,17.2077082127442,-21.0451207645081));
#89885=CARTESIAN_POINT('Ctrl Pts',(19.4241436394943,17.2096438841114,-21.04476512172));
#89886=CARTESIAN_POINT('Ctrl Pts',(19.438764144066,17.2147317058771,-21.043843726122));
#89887=CARTESIAN_POINT('Ctrl Pts',(19.4477327341011,17.2179206765278,-21.0432791987971));
#89888=CARTESIAN_POINT('Ctrl Pts',(19.4781302344891,17.2289606422007,-21.0413679003346));
#89889=CARTESIAN_POINT('Ctrl Pts',(19.4994540483372,17.2370977781957,-21.0400306581472));
#89890=CARTESIAN_POINT('Ctrl Pts',(19.6856724696758,17.3116300658952,-21.0283732534292));
#89891=CARTESIAN_POINT('Ctrl Pts',(19.8417242553545,17.3982010041257,-21.0188269506874));
#89892=CARTESIAN_POINT('Ctrl Pts',(20.0540677428375,17.5537694809917,-21.0044991662263));
#89893=CARTESIAN_POINT('Ctrl Pts',(20.1198771180721,17.6083976954555,-20.9998161647084));
#89894=CARTESIAN_POINT('Ctrl Pts',(20.2095008235223,17.6924522552349,-20.9927980021979));
#89895=CARTESIAN_POINT('Ctrl Pts',(20.2361160809054,17.7187745394609,-20.9906232038976));
#89896=CARTESIAN_POINT('Ctrl Pts',(20.2672424102436,17.7512350550082,-20.9879473165036));
#89897=CARTESIAN_POINT('Ctrl Pts',(20.2724377462836,17.7567114178692,-20.9874960708343));
#89898=CARTESIAN_POINT('Ctrl Pts',(20.2804622239475,17.7652610754076,-20.9867916748433));
#89899=CARTESIAN_POINT('Ctrl Pts',(20.2833118054406,17.7683152191111,-20.9865400643781));
#89900=CARTESIAN_POINT('Ctrl Pts',(20.2885758113405,17.7739906932484,-20.9860724860825));
#89901=CARTESIAN_POINT('Ctrl Pts',(20.2909926624724,17.7766096942194,-20.9858567084005));
#89902=CARTESIAN_POINT('Ctrl Pts',(20.2964367537521,17.7825391102994,-20.985368171404));
#89903=CARTESIAN_POINT('Ctrl Pts',(20.2994600745885,17.7858530332306,-20.9850951229519));
#89904=CARTESIAN_POINT('Ctrl Pts',(20.3083387009505,17.7956474163333,-20.9842881671894));
#89905=CARTESIAN_POINT('Ctrl Pts',(20.3141643781015,17.8021544394278,-20.9837521148015));
#89906=CARTESIAN_POINT('Ctrl Pts',(20.3555539695298,17.8489644449988,-20.9798974988602));
#89907=CARTESIAN_POINT('Ctrl Pts',(20.3896088126729,17.890569565895,-20.9764803818685));
#89908=CARTESIAN_POINT('Ctrl Pts',(20.5153598001475,18.056721939522,-20.9630097009873));
#89909=CARTESIAN_POINT('Ctrl Pts',(20.5948898223481,18.1898764151451,-20.952619438118));
#89910=CARTESIAN_POINT('Ctrl Pts',(20.6978949182326,18.4150996133364,-20.9365437916937));
#89911=CARTESIAN_POINT('Ctrl Pts',(20.7309679248523,18.5021532301219,-20.9306407298613));
#89912=CARTESIAN_POINT('Ctrl Pts',(20.7643902908689,18.6112919632435,-20.9236315493787));
#89913=CARTESIAN_POINT('Ctrl Pts',(20.7702684598198,18.6315646949074,-20.9223453074031));
#89914=CARTESIAN_POINT('Ctrl Pts',(20.7782090643501,18.6605650857446,-20.9205270515309));
#89915=CARTESIAN_POINT('Ctrl Pts',(20.780520614879,18.6692226745821,-20.9199869760399));
#89916=CARTESIAN_POINT('Ctrl Pts',(20.7844182317344,18.6842016095812,-20.919057205311));
#89917=CARTESIAN_POINT('Ctrl Pts',(20.7860301923636,18.6905160326393,-20.9186666758591));
#89918=CARTESIAN_POINT('Ctrl Pts',(20.7890639176096,18.7026330225814,-20.9179199534781));
#89919=CARTESIAN_POINT('Ctrl Pts',(20.790490325767,18.7084343522047,-20.9175636138014));
#89920=CARTESIAN_POINT('Ctrl Pts',(20.7941422285357,18.7235628803697,-20.9166373739574));
#89921=CARTESIAN_POINT('Ctrl Pts',(20.7963289592036,18.732899366223,-20.9160687260988));
#89922=CARTESIAN_POINT('Ctrl Pts',(20.8036013484556,18.7649282008543,-20.9141279005866));
#89923=CARTESIAN_POINT('Ctrl Pts',(20.8083766171052,18.7876898241974,-20.9127656655612));
#89924=CARTESIAN_POINT('Ctrl Pts',(20.845241861615,18.9790496212848,-20.9014446205915));
#89925=CARTESIAN_POINT('Ctrl Pts',(20.857096166532,19.1508943033247,-20.8921988796554));
#89926=CARTESIAN_POINT('Ctrl Pts',(20.8433539222923,19.4119216027589,-20.8779848727349));
#89927=CARTESIAN_POINT('Ctrl Pts',(20.8329416094389,19.5011465531038,-20.8730802610273));
#89928=CARTESIAN_POINT('Ctrl Pts',(20.8100173883943,19.62732161828,-20.8657636090026));
#89929=CARTESIAN_POINT('Ctrl Pts',(20.8021016595428,19.6650121064817,-20.8635279366092));
#89930=CARTESIAN_POINT('Ctrl Pts',(20.7913966032449,19.7098648360944,-20.8607845992553));
#89931=CARTESIAN_POINT('Ctrl Pts',(20.7895901366942,19.7172569443252,-20.8603297544147));
#89932=CARTESIAN_POINT('Ctrl Pts',(20.7867272403788,19.7287040025151,-20.8596209541419));
#89933=CARTESIAN_POINT('Ctrl Pts',(20.7856985376896,19.7327659124137,-20.8593685699367));
#89934=CARTESIAN_POINT('Ctrl Pts',(20.7837728184429,19.740276003082,-20.8589002766002));
#89935=CARTESIAN_POINT('Ctrl Pts',(20.7828791535374,19.7437249837284,-20.8586845622513));
#89936=CARTESIAN_POINT('Ctrl Pts',(20.780844840466,19.7514953042835,-20.8581971046279));
#89937=CARTESIAN_POINT('Ctrl Pts',(20.7796992186585,19.7558152722044,-20.8579250779148));
#89938=CARTESIAN_POINT('Ctrl Pts',(20.7762947799886,19.7684907614031,-20.8571239732019));
#89939=CARTESIAN_POINT('Ctrl Pts',(20.7739984209429,19.7768359780909,-20.8565927959621));
#89940=CARTESIAN_POINT('Ctrl Pts',(20.7575867844008,19.8350789705842,-20.8528604802505));
#89941=CARTESIAN_POINT('Ctrl Pts',(20.7416946143209,19.8844533466567,-20.8495675972214));
#89942=CARTESIAN_POINT('Ctrl Pts',(20.7166532929313,19.9534551774318,-20.8448281585302));
#89943=CARTESIAN_POINT('Ctrl Pts',(20.7089898900291,19.9736064913446,-20.843426985138));
#89944=CARTESIAN_POINT('Ctrl Pts',(20.6839297042274,20.0365908746419,-20.8390002873614));
#89945=CARTESIAN_POINT('Ctrl Pts',(20.6654371256026,20.0789726806086,-20.8359523654633));
#89946=CARTESIAN_POINT('Ctrl Pts',(20.5985795303598,20.2194598390507,-20.8256748347791));
#89947=CARTESIAN_POINT('Ctrl Pts',(20.5440021641236,20.3144236286371,-20.8184438758655));
#89948=CARTESIAN_POINT('Ctrl Pts',(20.4512734484407,20.4502311454526,-20.80787401141));
#89949=CARTESIAN_POINT('Ctrl Pts',(20.418454238454,20.4944861381966,-20.8043867236253));
#89950=CARTESIAN_POINT('Ctrl Pts',(20.3624588546783,20.5641395459459,-20.7988317161779));
#89951=CARTESIAN_POINT('Ctrl Pts',(20.3403266230553,20.5903403743556,-20.7967256051754));
#89952=CARTESIAN_POINT('Ctrl Pts',(20.3103939659607,20.624077444834,-20.7939898715823));
#89953=CARTESIAN_POINT('Ctrl Pts',(20.3031594625429,20.6321067478945,-20.7933369267554));
#89954=CARTESIAN_POINT('Ctrl Pts',(20.2912071382511,20.645169624564,-20.7922714823085));
#89955=CARTESIAN_POINT('Ctrl Pts',(20.2865257054468,20.6502360887362,-20.791857453829));
#89956=CARTESIAN_POINT('Ctrl Pts',(20.2774141983572,20.660000796708,-20.7910579020173));
#89957=CARTESIAN_POINT('Ctrl Pts',(20.2729872327527,20.6647018247911,-20.7906722524881));
#89958=CARTESIAN_POINT('Ctrl Pts',(20.2627134855329,20.6755120634761,-20.7897837149294));
#89959=CARTESIAN_POINT('Ctrl Pts',(20.2568514459799,20.6816066712615,-20.7892814932977));
#89960=CARTESIAN_POINT('Ctrl Pts',(20.2409826764744,20.6979083780975,-20.7879345635319));
#89961=CARTESIAN_POINT('Ctrl Pts',(20.2309087190409,20.7080496363955,-20.7870927985867));
#89962=CARTESIAN_POINT('Ctrl Pts',(20.1373585181349,20.8003362920003,-20.7793944137813));
#89963=CARTESIAN_POINT('Ctrl Pts',(20.0472983544054,20.8755292731566,-20.7728560863591));
#89964=CARTESIAN_POINT('Ctrl Pts',(19.81740811117,21.0371351496082,-20.7574736466199));
#89965=CARTESIAN_POINT('Ctrl Pts',(19.6728753792947,21.1154798236972,-20.7488161660152));
#89966=CARTESIAN_POINT('Ctrl Pts',(19.4917871752002,21.1879731076745,-20.7376000975935));
#89967=CARTESIAN_POINT('Ctrl Pts',(19.4625461418193,21.1989346964479,-20.7357770028248));
#89968=CARTESIAN_POINT('Ctrl Pts',(19.4263259160233,21.2116061466475,-20.7334917901452));
#89969=CARTESIAN_POINT('Ctrl Pts',(19.4195648288067,21.2139330967818,-20.7330640753817));
#89970=CARTESIAN_POINT('Ctrl Pts',(19.4089178709198,21.2175372156843,-20.732388550745));
#89971=CARTESIAN_POINT('Ctrl Pts',(19.4050397935629,21.2188374748014,-20.7321420833069));
#89972=CARTESIAN_POINT('Ctrl Pts',(19.3977650548435,21.2212531515996,-20.731678929481));
#89973=CARTESIAN_POINT('Ctrl Pts',(19.3943693280501,21.2223712067753,-20.7314624011407));
#89974=CARTESIAN_POINT('Ctrl Pts',(19.3865863820361,21.2249119359246,-20.7309653635711));
#89975=CARTESIAN_POINT('Ctrl Pts',(19.3821973483342,21.2263288734997,-20.7306845220782));
#89976=CARTESIAN_POINT('Ctrl Pts',(19.3686045105854,21.2306681325474,-20.7298131417432));
#89977=CARTESIAN_POINT('Ctrl Pts',(19.35938546631,21.2335417822388,-20.7292198623444));
#89978=CARTESIAN_POINT('Ctrl Pts',(19.2481026467415,21.2673959472365,-20.7220336719855));
#89979=CARTESIAN_POINT('Ctrl Pts',(19.1438693330105,21.2906796746592,-20.7150597754286));
#89980=CARTESIAN_POINT('Ctrl Pts',(18.9301071896042,21.3217327058625,-20.7008103069896));
#89981=CARTESIAN_POINT('Ctrl Pts',(18.8208111528296,21.3290456101083,-20.6935552862598));
#89982=CARTESIAN_POINT('Ctrl Pts',(18.6488221090727,21.3272123274248,-20.6824362339002));
#89983=CARTESIAN_POINT('Ctrl Pts',(18.586264940794,21.3237672403705,-20.6784512248014));
#89984=CARTESIAN_POINT('Ctrl Pts',(18.4991746404988,21.3150831384411,-20.6729961128224));
#89985=CARTESIAN_POINT('Ctrl Pts',(18.4744463772579,21.3121760521088,-20.6714575296165));
#89986=CARTESIAN_POINT('Ctrl Pts',(18.4312405861266,21.3063223000883,-20.6687868417886));
#89987=CARTESIAN_POINT('Ctrl Pts',(18.4127405147806,21.3035656936721,-20.6676489558615));
#89988=CARTESIAN_POINT('Ctrl Pts',(18.385854476093,21.2991945650397,-20.6660031009818));
#89989=CARTESIAN_POINT('Ctrl Pts',(18.3774382922013,21.2977739693465,-20.6654890158072));
#89990=CARTESIAN_POINT('Ctrl Pts',(18.3626811095882,21.2951911706103,-20.6645895046686));
#89991=CARTESIAN_POINT('Ctrl Pts',(18.3563364422925,21.2940508377454,-20.6642033892572));
#89992=CARTESIAN_POINT('Ctrl Pts',(18.3440146539,21.2917780843284,-20.6634546926165));
#89993=CARTESIAN_POINT('Ctrl Pts',(18.3380370168394,21.2906488462115,-20.6630920142653));
#89994=CARTESIAN_POINT('Ctrl Pts',(18.3237394641117,21.2878840090065,-20.6622257859679));
#89995=CARTESIAN_POINT('Ctrl Pts',(18.3154243029064,21.2862241525087,-20.6617230131681));
#89996=CARTESIAN_POINT('Ctrl Pts',(18.2853398151381,21.2800305668477,-20.6599074352307));
#89997=CARTESIAN_POINT('Ctrl Pts',(18.2636318046011,21.2752037845176,-20.6586039834267));
#89998=CARTESIAN_POINT('Ctrl Pts',(18.0627480670869,21.2272035750021,-20.6465932360829));
#89999=CARTESIAN_POINT('Ctrl Pts',(17.8898577420822,21.1611502478916,-20.636728559038));
#90000=CARTESIAN_POINT('Ctrl Pts',(17.6564348815259,21.0350347338997,-20.6222691877976));
#90001=CARTESIAN_POINT('Ctrl Pts',(17.5874485616865,20.9924788914488,-20.6178175353737));
#90002=CARTESIAN_POINT('Ctrl Pts',(17.4913574536307,20.925305470127,-20.6111127793929));
#90003=CARTESIAN_POINT('Ctrl Pts',(17.4621801061937,20.9037721482331,-20.6090040747575));
#90004=CARTESIAN_POINT('Ctrl Pts',(17.4276696923469,20.8769069835119,-20.6064014686361));
#90005=CARTESIAN_POINT('Ctrl Pts',(17.4217917985262,20.8722810065139,-20.6059542820975));
#90006=CARTESIAN_POINT('Ctrl Pts',(17.4126815188217,20.8650325860968,-20.6052548588013));
#90007=CARTESIAN_POINT('Ctrl Pts',(17.4094320761689,20.8624315423432,-20.6050041269599));
#90008=CARTESIAN_POINT('Ctrl Pts',(17.4034133432647,20.8575846051757,-20.6045373186838));
#90009=CARTESIAN_POINT('Ctrl Pts',(17.4006420485626,20.8553412923782,-20.6043214269298));
#90010=CARTESIAN_POINT('Ctrl Pts',(17.3943809880378,20.8502468423371,-20.6038315177572));
#90011=CARTESIAN_POINT('Ctrl Pts',(17.3908946687434,20.8473915716002,-20.6035572042259));
#90012=CARTESIAN_POINT('Ctrl Pts',(17.3806055030626,20.838909786348,-20.6027431842953));
#90013=CARTESIAN_POINT('Ctrl Pts',(17.3738288038391,20.8332519063736,-20.6022012779455));
#90014=CARTESIAN_POINT('Ctrl Pts',(17.324210047106,20.7912956402657,-20.5981920259182));
#90015=CARTESIAN_POINT('Ctrl Pts',(17.282795608028,20.7533510133226,-20.5946171897731));
#90016=CARTESIAN_POINT('Ctrl Pts',(17.1985928197579,20.6698066685642,-20.5869375052346));
#90017=CARTESIAN_POINT('Ctrl Pts',(17.1562146579564,20.6238640788818,-20.5828222650344));
#90018=CARTESIAN_POINT('Ctrl Pts',(17.0452480462374,20.4923357600657,-20.571455376874));
#90019=CARTESIAN_POINT('Ctrl Pts',(16.9811726613987,20.4031846634318,-20.5642057676579));
#90020=CARTESIAN_POINT('Ctrl Pts',(16.8955510673252,20.2621239937673,-20.5535967724632));
#90021=CARTESIAN_POINT('Ctrl Pts',(16.8686817505602,20.2136688334086,-20.5500891281262));
#90022=CARTESIAN_POINT('Ctrl Pts',(16.8282391532386,20.1334695321404,-20.5445055521425));
#90023=CARTESIAN_POINT('Ctrl Pts',(16.8134880194395,20.102352003432,-20.5423907307492));
#90024=CARTESIAN_POINT('Ctrl Pts',(16.7951057146868,20.0609971092059,-20.5396455464173));
#90025=CARTESIAN_POINT('Ctrl Pts',(16.7907854904367,20.0510735157795,-20.5389916564798));
#90026=CARTESIAN_POINT('Ctrl Pts',(16.7838354325762,20.0347686479469,-20.537925086868));
#90027=CARTESIAN_POINT('Ctrl Pts',(16.7811604049575,20.0284069630021,-20.5375108717434));
#90028=CARTESIAN_POINT('Ctrl Pts',(16.7760434385899,20.0160694224975,-20.5367112474208));
#90029=CARTESIAN_POINT('Ctrl Pts',(16.7735976345372,20.0100952623573,-20.5363257105257));
#90030=CARTESIAN_POINT('Ctrl Pts',(16.768014752315,19.996278518032,-20.5354378438087));
#90031=CARTESIAN_POINT('Ctrl Pts',(16.7648971948507,19.9884281258775,-20.5349361774479));
#90032=CARTESIAN_POINT('Ctrl Pts',(16.7566421279442,19.9672726087486,-20.5335916499447));
#90033=CARTESIAN_POINT('Ctrl Pts',(16.7515918945119,19.9539337326075,-20.532751715932));
#90034=CARTESIAN_POINT('Ctrl Pts',(16.6965077126275,19.8038811152991,-20.5233872012149));
#90035=CARTESIAN_POINT('Ctrl Pts',(16.6605663579823,19.6624018962055,-20.5153746946421));
#90036=CARTESIAN_POINT('Ctrl Pts',(16.6244283768288,19.4161126844961,-20.5018389983019));
#90037=CARTESIAN_POINT('Ctrl Pts',(16.6169334233411,19.3129338000966,-20.4962758002309));
#90038=CARTESIAN_POINT('Ctrl Pts',(16.6170394068523,19.1495719686811,-20.487137402816));
#90039=CARTESIAN_POINT('Ctrl Pts',(16.6196337803189,19.0895518828876,-20.4837076735602));
#90040=CARTESIAN_POINT('Ctrl Pts',(16.6255428349016,19.0207954004558,-20.4796144316925));
#90041=CARTESIAN_POINT('Ctrl Pts',(16.6263673827784,19.0118664991852,-20.4790796684169));
#90042=CARTESIAN_POINT('Ctrl Pts',(16.6276944057823,18.998429261409,-20.4782697071146));
#90043=CARTESIAN_POINT('Ctrl Pts',(16.6281546997847,18.9939167306783,-20.4779968214312));
#90044=CARTESIAN_POINT('Ctrl Pts',(16.629002949118,18.9858574997488,-20.4775078245677));
#90045=CARTESIAN_POINT('Ctrl Pts',(16.6293853710041,18.9823102695823,-20.4772920272819));
#90046=CARTESIAN_POINT('Ctrl Pts',(16.6302310228264,18.9746480637434,-20.4768246526068));
#90047=CARTESIAN_POINT('Ctrl Pts',(16.6306973530316,18.9705335331746,-20.4765729082141));
#90048=CARTESIAN_POINT('Ctrl Pts',(16.6320285817631,18.9590880140098,-20.475870533521));
#90049=CARTESIAN_POINT('Ctrl Pts',(16.632919747666,18.9517602242514,-20.4754184636422));
#90050=CARTESIAN_POINT('Ctrl Pts',(16.6382144753014,18.9100449752937,-20.4728319180673));
#90051=CARTESIAN_POINT('Ctrl Pts',(16.6434236289392,18.8757672336488,-20.470656115383));
#90052=CARTESIAN_POINT('Ctrl Pts',(16.662592792622,18.7675851043797,-20.4636610256852));
#90053=CARTESIAN_POINT('Ctrl Pts',(16.6796496235097,18.6942916022204,-20.4587324116113));
#90054=CARTESIAN_POINT('Ctrl Pts',(16.7139659304942,18.5758064391525,-20.4505956078634));
#90055=CARTESIAN_POINT('Ctrl Pts',(16.7289275855916,18.5300554242867,-20.4474103353874));
#90056=CARTESIAN_POINT('Ctrl Pts',(16.7454193207648,18.4848898966601,-20.4442392307736));
#90057=CARTESIAN_POINT('Origin',(18.734,19.211,0.));
#90058=CARTESIAN_POINT('',(16.7454194502465,18.4848895420517,-19.6425235887674));
#90059=CARTESIAN_POINT('',(16.7452305124652,18.4848205810513,-19.866484321603));
#90060=CARTESIAN_POINT('',(16.7454194503191,18.4848895418526,0.));
#90061=CARTESIAN_POINT('',(16.6200797422209,19.2118282580408,-19.9109991802722));
#90062=CARTESIAN_POINT('Ctrl Pts',(16.7452305124652,18.4848205810513,-19.866484321603));
#90063=CARTESIAN_POINT('Ctrl Pts',(16.6631151030873,18.7170153086961,-19.8813041213945));
#90064=CARTESIAN_POINT('Ctrl Pts',(16.6210474027165,18.9645594739241,-19.896123921186));
#90065=CARTESIAN_POINT('Ctrl Pts',(16.620175975625,19.2118314138067,-19.9109437209775));
#90066=CARTESIAN_POINT('Ctrl Pts',(16.617000124922,19.2117272686677,-19.9127739632071));
#90067=CARTESIAN_POINT('Ctrl Pts',(16.6170670033201,19.4064030010461,-19.9239833213257));
#90068=CARTESIAN_POINT('Ctrl Pts',(16.6439835663,19.6001371164809,-19.9342646372126));
#90069=CARTESIAN_POINT('Ctrl Pts',(16.7140733651364,19.8478011973305,-19.948410553006));
#90070=CARTESIAN_POINT('Ctrl Pts',(16.7338151510888,19.9073323898861,-19.9519022938411));
#90071=CARTESIAN_POINT('Ctrl Pts',(16.767193688988,19.9947844752322,-19.9572865043126));
#90072=CARTESIAN_POINT('Ctrl Pts',(16.7788510569389,20.0234269518889,-19.9590922720175));
#90073=CARTESIAN_POINT('Ctrl Pts',(16.7939618108709,20.0583438699617,-19.9613581576324));
#90074=CARTESIAN_POINT('Ctrl Pts',(16.7968258155017,20.0648711758011,-19.9617845528516));
#90075=CARTESIAN_POINT('Ctrl Pts',(16.8013829439054,20.075116313182,-19.9624584414996));
#90076=CARTESIAN_POINT('Ctrl Pts',(16.8030539888956,20.0788439893012,-19.9627046029928));
#90077=CARTESIAN_POINT('Ctrl Pts',(16.8062079245867,20.0858254110863,-19.9631674899564));
#90078=CARTESIAN_POINT('Ctrl Pts',(16.8076882729767,20.0890802443747,-19.9633840592415));
#90079=CARTESIAN_POINT('Ctrl Pts',(16.8111000205985,20.0965314841062,-19.9638815930443));
#90080=CARTESIAN_POINT('Ctrl Pts',(16.8130369086226,20.1007253175883,-19.9641628924463));
#90081=CARTESIAN_POINT('Ctrl Pts',(16.8190812888894,20.1137011271452,-19.9650370990681));
#90082=CARTESIAN_POINT('Ctrl Pts',(16.823235326096,20.1224611060637,-19.9656327721567));
#90083=CARTESIAN_POINT('Ctrl Pts',(16.8705050515305,20.2203994966495,-19.9723517880548));
#90084=CARTESIAN_POINT('Ctrl Pts',(16.9197639317907,20.3064650150461,-19.9788045467882));
#90085=CARTESIAN_POINT('Ctrl Pts',(17.0685545516379,20.5287045103512,-19.9964228353183));
#90086=CARTESIAN_POINT('Ctrl Pts',(17.1786346335275,20.6569976269522,-20.0076111765957));
#90087=CARTESIAN_POINT('Ctrl Pts',(17.3256315799805,20.7918700503244,-20.0201380776319));
#90088=CARTESIAN_POINT('Ctrl Pts',(17.3489534005475,20.8123424983284,-20.0220665886807));
#90089=CARTESIAN_POINT('Ctrl Pts',(17.384311874298,20.8420303948361,-20.024904952664));
#90090=CARTESIAN_POINT('Ctrl Pts',(17.3960102342132,20.8516406038085,-20.0258306231042));
#90091=CARTESIAN_POINT('Ctrl Pts',(17.4149104263543,20.8668305033765,-20.0273050947322));
#90092=CARTESIAN_POINT('Ctrl Pts',(17.4220467681044,20.872490499702,-20.0278571078492));
#90093=CARTESIAN_POINT('Ctrl Pts',(17.4357273373919,20.8831977719531,-20.0289064532558));
#90094=CARTESIAN_POINT('Ctrl Pts',(17.4422650096485,20.8882531152831,-20.0294041017591));
#90095=CARTESIAN_POINT('Ctrl Pts',(17.4537923339595,20.8970593980031,-20.0302749615039));
#90096=CARTESIAN_POINT('Ctrl Pts',(17.4587692532811,20.900826767956,-20.0306488191648));
#90097=CARTESIAN_POINT('Ctrl Pts',(17.4686248253976,20.9082187852628,-20.0313849848409));
#90098=CARTESIAN_POINT('Ctrl Pts',(17.4735025664652,20.9118445428041,-20.0317473341812));
#90099=CARTESIAN_POINT('Ctrl Pts',(17.4852053358776,20.9204655358477,-20.0326119736801));
#90100=CARTESIAN_POINT('Ctrl Pts',(17.4920448515565,20.9254410003849,-20.033113493206));
#90101=CARTESIAN_POINT('Ctrl Pts',(17.5168619450707,20.943267964101,-20.0349197417771));
#90102=CARTESIAN_POINT('Ctrl Pts',(17.5350110552213,20.9558790527527,-20.036215244557));
#90103=CARTESIAN_POINT('Ctrl Pts',(17.7074238415235,21.0717212220229,-20.0482960856431));
#90104=CARTESIAN_POINT('Ctrl Pts',(17.8744321224907,21.1545254444176,-20.0582244906873));
#90105=CARTESIAN_POINT('Ctrl Pts',(18.1259430444054,21.2403783098153,-20.0727122644604));
#90106=CARTESIAN_POINT('Ctrl Pts',(18.2031781733303,21.261935339801,-20.0771188428785));
#90107=CARTESIAN_POINT('Ctrl Pts',(18.3166359031823,21.2867635031169,-20.0837623330807));
#90108=CARTESIAN_POINT('Ctrl Pts',(18.352018135063,21.2935648649068,-20.0858578674268));
#90109=CARTESIAN_POINT('Ctrl Pts',(18.3949195811649,21.3006816052478,-20.0884458673372));
#90110=CARTESIAN_POINT('Ctrl Pts',(18.4022912553874,21.301864425717,-20.0888922292708));
#90111=CARTESIAN_POINT('Ctrl Pts',(18.4137790899883,21.3036454234865,-20.0895906433832));
#90112=CARTESIAN_POINT('Ctrl Pts',(18.4178911013325,21.3042705183868,-20.0898411977216));
#90113=CARTESIAN_POINT('Ctrl Pts',(18.4255318938312,21.3054090200908,-20.0903078539977));
#90114=CARTESIAN_POINT('Ctrl Pts',(18.4290601396448,21.3059256304036,-20.0905237723762));
#90115=CARTESIAN_POINT('Ctrl Pts',(18.4370543996723,21.3070755369671,-20.0910139727954));
#90116=CARTESIAN_POINT('Ctrl Pts',(18.4415211202765,21.3077034721845,-20.0912885524036));
#90117=CARTESIAN_POINT('Ctrl Pts',(18.4530597186375,21.3092879890831,-20.0919995631071));
#90118=CARTESIAN_POINT('Ctrl Pts',(18.4601344213738,21.310223086848,-20.09243716118));
#90119=CARTESIAN_POINT('Ctrl Pts',(18.5036195860804,21.3157471699273,-20.0951364752464));
#90120=CARTESIAN_POINT('Ctrl Pts',(18.5401372204707,21.3194242060631,-20.0974444600204));
#90121=CARTESIAN_POINT('Ctrl Pts',(18.7466315537019,21.3348070585388,-20.110659309168));
#90122=CARTESIAN_POINT('Ctrl Pts',(18.917438746667,21.3269086167166,-20.1221549647551));
#90123=CARTESIAN_POINT('Ctrl Pts',(19.1796055634226,21.2827721816778,-20.1394327629003));
#90124=CARTESIAN_POINT('Ctrl Pts',(19.2725841369815,21.260569633114,-20.1454989500872));
#90125=CARTESIAN_POINT('Ctrl Pts',(19.3841906711131,21.2257950636535,-20.152679591087));
#90126=CARTESIAN_POINT('Ctrl Pts',(19.4045268847032,21.2191187233347,-20.1539841509957));
#90127=CARTESIAN_POINT('Ctrl Pts',(19.4332773989738,21.2091945173494,-20.155823583054));
#90128=CARTESIAN_POINT('Ctrl Pts',(19.4417770754778,21.206199695578,-20.1563667729496));
#90129=CARTESIAN_POINT('Ctrl Pts',(19.4563992918996,21.2009424266203,-20.1573002550792));
#90130=CARTESIAN_POINT('Ctrl Pts',(19.4625309177163,21.1987057884941,-20.1576913988416));
#90131=CARTESIAN_POINT('Ctrl Pts',(19.474245895529,21.194371016256,-20.1584381742853));
#90132=CARTESIAN_POINT('Ctrl Pts',(19.4798309067873,21.1922775761044,-20.1587939581181));
#90133=CARTESIAN_POINT('Ctrl Pts',(19.4943189797994,21.1867770420022,-20.1597163275077));
#90134=CARTESIAN_POINT('Ctrl Pts',(19.5032080723402,21.1833333432032,-20.1602816822379));
#90135=CARTESIAN_POINT('Ctrl Pts',(19.5333788628564,21.1714099659397,-20.1621989074506));
#90136=CARTESIAN_POINT('Ctrl Pts',(19.5545465204449,21.162644759941,-20.1635411669092));
#90137=CARTESIAN_POINT('Ctrl Pts',(19.7375871778113,21.083345785542,-20.1751335932724));
#90138=CARTESIAN_POINT('Ctrl Pts',(19.8901866707694,20.9931630098304,-20.1846219518578));
#90139=CARTESIAN_POINT('Ctrl Pts',(20.098028332902,20.8322815023627,-20.1989254521405));
#90140=CARTESIAN_POINT('Ctrl Pts',(20.1629330412029,20.7753768777675,-20.2036492252431));
#90141=CARTESIAN_POINT('Ctrl Pts',(20.2509094507185,20.6881901505228,-20.2107223713131));
#90142=CARTESIAN_POINT('Ctrl Pts',(20.2769247819386,20.6609957745515,-20.2129085161486));
#90143=CARTESIAN_POINT('Ctrl Pts',(20.3072787891831,20.6275239197596,-20.215596997621));
#90144=CARTESIAN_POINT('Ctrl Pts',(20.3123276497528,20.621896165514,-20.2160489478182));
#90145=CARTESIAN_POINT('Ctrl Pts',(20.3201207309801,20.6131153655055,-20.2167542186257));
#90146=CARTESIAN_POINT('Ctrl Pts',(20.3228860002234,20.6099809680736,-20.2170059934516));
#90147=CARTESIAN_POINT('Ctrl Pts',(20.327991831889,20.6041589075598,-20.2174737425594));
#90148=CARTESIAN_POINT('Ctrl Pts',(20.3303348968439,20.6014735158847,-20.2176895258141));
#90149=CARTESIAN_POINT('Ctrl Pts',(20.3356100772121,20.5953967131529,-20.2181779024908));
#90150=CARTESIAN_POINT('Ctrl Pts',(20.3385381904178,20.5920019165271,-20.2184507840204));
#90151=CARTESIAN_POINT('Ctrl Pts',(20.3471299313312,20.5819766100911,-20.2192567223996));
#90152=CARTESIAN_POINT('Ctrl Pts',(20.3527633196,20.5753204718402,-20.2197919160065));
#90153=CARTESIAN_POINT('Ctrl Pts',(20.3925706226343,20.527692464828,-20.2236210423224));
#90154=CARTESIAN_POINT('Ctrl Pts',(20.4252231437164,20.4854798149951,-20.2270120692406));
#90155=CARTESIAN_POINT('Ctrl Pts',(20.4665329483751,20.4276888084987,-20.2316031721895));
#90156=CARTESIAN_POINT('Ctrl Pts',(20.4766412820537,20.4131661330435,-20.2327528101188));
#90157=CARTESIAN_POINT('Ctrl Pts',(20.5137261870369,20.3584354181624,-20.2370658061026));
#90158=CARTESIAN_POINT('Ctrl Pts',(20.5395023995542,20.3174330925795,-20.2402577089861));
#90159=CARTESIAN_POINT('Ctrl Pts',(20.618854998902,20.1810387131874,-20.250681431172));
#90160=CARTESIAN_POINT('Ctrl Pts',(20.6664544649947,20.0823648366458,-20.2579141975047));
#90161=CARTESIAN_POINT('Ctrl Pts',(20.7262436204897,19.9291159278624,-20.2684877867674));
#90162=CARTESIAN_POINT('Ctrl Pts',(20.7442602346272,19.8770178221181,-20.2719769890089));
#90163=CARTESIAN_POINT('Ctrl Pts',(20.7701619401027,19.7914397319328,-20.2775346424689));
#90164=CARTESIAN_POINT('Ctrl Pts',(20.7793002306,19.7583690818511,-20.2796415347935));
#90165=CARTESIAN_POINT('Ctrl Pts',(20.7902558947884,19.7146045233436,-20.2823780853767));
#90166=CARTESIAN_POINT('Ctrl Pts',(20.7928002866236,19.7040995917341,-20.283031085991));
#90167=CARTESIAN_POINT('Ctrl Pts',(20.7968365513889,19.6868591636119,-20.2840965764876));
#90168=CARTESIAN_POINT('Ctrl Pts',(20.7983761289854,19.6801351416883,-20.2845105958338));
#90169=CARTESIAN_POINT('Ctrl Pts',(20.8012931104002,19.6671029310108,-20.2853100987148));
#90170=CARTESIAN_POINT('Ctrl Pts',(20.8026745717411,19.6607957376877,-20.2856957086015));
#90171=CARTESIAN_POINT('Ctrl Pts',(20.8057982552624,19.6462154258846,-20.2865841097924));
#90172=CARTESIAN_POINT('Ctrl Pts',(20.8075198239698,19.6379379582605,-20.2870862350647));
#90173=CARTESIAN_POINT('Ctrl Pts',(20.8120175823714,19.6156431907515,-20.2884328051846));
#90174=CARTESIAN_POINT('Ctrl Pts',(20.814701545353,19.601607576144,-20.2892743087983));
#90175=CARTESIAN_POINT('Ctrl Pts',(20.8380201751499,19.472596965349,-20.2969546458627));
#90176=CARTESIAN_POINT('Ctrl Pts',(20.8492493029019,19.3561189760174,-20.3034769374647));
#90177=CARTESIAN_POINT('Ctrl Pts',(20.8529854148806,19.0766185722943,-20.3187795159421));
#90178=CARTESIAN_POINT('Ctrl Pts',(20.8364003228626,18.9142532946038,-20.3273768859465));
#90179=CARTESIAN_POINT('Ctrl Pts',(20.7943873034294,18.7236051013331,-20.338585518038));
#90180=CARTESIAN_POINT('Ctrl Pts',(20.7866460999621,18.6919688322643,-20.3404849054904));
#90181=CARTESIAN_POINT('Ctrl Pts',(20.7762953124876,18.6535313231779,-20.3428550183296));
#90182=CARTESIAN_POINT('Ctrl Pts',(20.7743759484222,18.646546764826,-20.3432882379055));
#90183=CARTESIAN_POINT('Ctrl Pts',(20.7713112837595,18.6356143645867,-20.343970510917));
#90184=CARTESIAN_POINT('Ctrl Pts',(20.7701902442007,18.6316596983337,-20.3442181766205));
#90185=CARTESIAN_POINT('Ctrl Pts',(20.7680735885213,18.6242748565839,-20.3446823157286));
#90186=CARTESIAN_POINT('Ctrl Pts',(20.7670808067098,18.6208439272789,-20.3448986234359));
#90187=CARTESIAN_POINT('Ctrl Pts',(20.7647951422541,18.6130191747389,-20.3453934740329));
#90188=CARTESIAN_POINT('Ctrl Pts',(20.7634966847379,18.6086270400241,-20.3456723383312));
#90189=CARTESIAN_POINT('Ctrl Pts',(20.7594631138016,18.5951442572704,-20.3465316864651));
#90190=CARTESIAN_POINT('Ctrl Pts',(20.756681140914,18.5860679111297,-20.3471148050523));
#90191=CARTESIAN_POINT('Ctrl Pts',(20.7312131755112,18.5049290373252,-20.3523672096824));
#90192=CARTESIAN_POINT('Ctrl Pts',(20.7047480677554,18.4341176349763,-20.3572297750416));
#90193=CARTESIAN_POINT('Ctrl Pts',(20.6204437741514,18.2407673307749,-20.3710232150381));
#90194=CARTESIAN_POINT('Ctrl Pts',(20.5545411181801,18.1221220173689,-20.3800734118708));
#90195=CARTESIAN_POINT('Ctrl Pts',(20.4267690694175,17.9365166446469,-20.3946763522883));
#90196=CARTESIAN_POINT('Ctrl Pts',(20.3711079576764,17.8657654185015,-20.4003747605024));
#90197=CARTESIAN_POINT('Ctrl Pts',(20.2972795996307,17.7833180987809,-20.4071682347154));
#90198=CARTESIAN_POINT('Ctrl Pts',(20.2832245288497,17.7680786144507,-20.4084312197239));
#90199=CARTESIAN_POINT('Ctrl Pts',(20.262820376999,17.7465969108227,-20.4102226404648));
#90200=CARTESIAN_POINT('Ctrl Pts',(20.2566525961896,17.7401848424043,-20.4107588149748));
#90201=CARTESIAN_POINT('Ctrl Pts',(20.2459047273481,17.7291513489926,-20.4116840366499));
#90202=CARTESIAN_POINT('Ctrl Pts',(20.2413434535983,17.7245118421491,-20.4120738957558));
#90203=CARTESIAN_POINT('Ctrl Pts',(20.232542415171,17.715642016393,-20.4128208285973));
#90204=CARTESIAN_POINT('Ctrl Pts',(20.2283059510638,17.7114085239793,-20.4131780419467));
#90205=CARTESIAN_POINT('Ctrl Pts',(20.2171837811252,17.7003880892693,-20.4141098265386));
#90206=CARTESIAN_POINT('Ctrl Pts',(20.2102693971544,17.6936301883947,-20.4146831158009));
#90207=CARTESIAN_POINT('Ctrl Pts',(20.1862277696811,17.670452552023,-20.4166562195719));
#90208=CARTESIAN_POINT('Ctrl Pts',(20.1688705619979,17.6542731544564,-20.4180456362898));
#90209=CARTESIAN_POINT('Ctrl Pts',(20.0307900511407,17.5298343845559,-20.4288389213426));
#90210=CARTESIAN_POINT('Ctrl Pts',(19.898262515005,17.4354769657898,-20.4376172873601));
#90211=CARTESIAN_POINT('Ctrl Pts',(19.6420314168533,17.2941848320124,-20.4535133211676));
#90212=CARTESIAN_POINT('Ctrl Pts',(19.5222534792738,17.2419017260531,-20.4606065192551));
#90213=CARTESIAN_POINT('Ctrl Pts',(19.3871571164304,17.1972432588567,-20.4690032816716));
#90214=CARTESIAN_POINT('Ctrl Pts',(19.3758346180798,17.1936059533017,-20.4697100255689));
#90215=CARTESIAN_POINT('Ctrl Pts',(19.3596901894346,17.1885692874668,-20.4707228105304));
#90216=CARTESIAN_POINT('Ctrl Pts',(19.3548927620591,17.1870913120911,-20.4710243987553));
#90217=CARTESIAN_POINT('Ctrl Pts',(19.3466142814134,17.1845731096321,-20.4715459830214));
#90218=CARTESIAN_POINT('Ctrl Pts',(19.3431356872957,17.1835247438966,-20.4717655043885));
#90219=CARTESIAN_POINT('Ctrl Pts',(19.3363840983526,17.1815089193617,-20.472192283586));
#90220=CARTESIAN_POINT('Ctrl Pts',(19.3331114559672,17.180540418702,-20.4723994731696));
#90221=CARTESIAN_POINT('Ctrl Pts',(19.3242722228052,17.1779477803213,-20.4729599180046));
#90222=CARTESIAN_POINT('Ctrl Pts',(19.3187013255415,17.1763386072745,-20.4733140308232));
#90223=CARTESIAN_POINT('Ctrl Pts',(19.2979808492575,17.1704455498023,-20.4746342580403));
#90224=CARTESIAN_POINT('Ctrl Pts',(19.2827906697476,17.1663079376682,-20.4756083278444));
#90225=CARTESIAN_POINT('Ctrl Pts',(19.1401117360924,17.1291484034575,-20.484806486577));
#90226=CARTESIAN_POINT('Ctrl Pts',(19.0098595716459,17.1079241109576,-20.4935492165282));
#90227=CARTESIAN_POINT('Ctrl Pts',(18.7196001202769,17.0880664028084,-20.5127673929404));
#90228=CARTESIAN_POINT('Ctrl Pts',(18.5599586860911,17.0951592199509,-20.5231357200905));
#90229=CARTESIAN_POINT('Ctrl Pts',(18.3815824374086,17.1234311449658,-20.5342280935254));
#90230=CARTESIAN_POINT('Ctrl Pts',(18.3606150748576,17.1270792691412,-20.5355251291975));
#90231=CARTESIAN_POINT('Ctrl Pts',(18.3308716521736,17.1327176853398,-20.5373559034078));
#90232=CARTESIAN_POINT('Ctrl Pts',(18.3220482928543,17.134448618712,-20.5378978528596));
#90233=CARTESIAN_POINT('Ctrl Pts',(18.3068429680297,17.1375322709397,-20.5388298878122));
#90234=CARTESIAN_POINT('Ctrl Pts',(18.3004557869053,17.1388583614563,-20.5392208176929));
#90235=CARTESIAN_POINT('Ctrl Pts',(18.2882360530744,17.1414543655766,-20.5399676506761));
#90236=CARTESIAN_POINT('Ctrl Pts',(18.2824025517059,17.1427194641061,-20.5403237036971));
#90237=CARTESIAN_POINT('Ctrl Pts',(18.2672432067404,17.1460742308842,-20.5412477787271));
#90238=CARTESIAN_POINT('Ctrl Pts',(18.257925957516,17.1482024222824,-20.5418145608792));
#90239=CARTESIAN_POINT('Ctrl Pts',(18.2261824781334,17.1556796120282,-20.5437418037932));
#90240=CARTESIAN_POINT('Ctrl Pts',(18.2038288681629,17.1613319378218,-20.5450925151864));
#90241=CARTESIAN_POINT('Ctrl Pts',(18.013003440215,17.2129148153442,-20.556578359049));
#90242=CARTESIAN_POINT('Ctrl Pts',(17.8507219827634,17.2791596527801,-20.5659712393592));
#90243=CARTESIAN_POINT('Ctrl Pts',(17.6219937525634,17.4074460802779,-20.5802384872169));
#90244=CARTESIAN_POINT('Ctrl Pts',(17.5483211304217,17.4550023282368,-20.5850329287597));
#90245=CARTESIAN_POINT('Ctrl Pts',(17.4472443094895,17.5295152340532,-20.5922013604299));
#90246=CARTESIAN_POINT('Ctrl Pts',(17.4172901011136,17.552866753355,-20.5944070627951));
#90247=CARTESIAN_POINT('Ctrl Pts',(17.382131208064,17.5818292801119,-20.5971172261748));
#90248=CARTESIAN_POINT('Ctrl Pts',(17.3763062272557,17.5866804253275,-20.5975703516762));
#90249=CARTESIAN_POINT('Ctrl Pts',(17.3673067049478,17.5942576132068,-20.5982770668746));
#90250=CARTESIAN_POINT('Ctrl Pts',(17.3641139118947,17.5969620162727,-20.5985291006687));
#90251=CARTESIAN_POINT('Ctrl Pts',(17.35821696782,17.6019870273684,-20.5989970721733));
#90252=CARTESIAN_POINT('Ctrl Pts',(17.3555106504383,17.6043050039598,-20.599212817212));
#90253=CARTESIAN_POINT('Ctrl Pts',(17.3494172446107,17.6095507695748,-20.5997007814425));
#90254=CARTESIAN_POINT('Ctrl Pts',(17.3460336042783,17.6124824593874,-20.5999732866671));
#90255=CARTESIAN_POINT('Ctrl Pts',(17.3361072842766,17.6211382049902,-20.6007771919632));
#90256=CARTESIAN_POINT('Ctrl Pts',(17.3295906258286,17.6268917727313,-20.6013107135226));
#90257=CARTESIAN_POINT('Ctrl Pts',(17.2837290690074,17.6678884261223,-20.605105191026));
#90258=CARTESIAN_POINT('Ctrl Pts',(17.2456831712069,17.7045501633625,-20.6084613457161));
#90259=CARTESIAN_POINT('Ctrl Pts',(17.1955083637951,17.7566569480874,-20.613134828151));
#90260=CARTESIAN_POINT('Ctrl Pts',(17.1821607821879,17.7709079069263,-20.6144037596343));
#90261=CARTESIAN_POINT('Ctrl Pts',(17.0704029012836,17.8935878039253,-20.6252363496672));
#90262=CARTESIAN_POINT('Ctrl Pts',(16.9832805131874,18.0117849697411,-20.6350415605194));
#90263=CARTESIAN_POINT('Ctrl Pts',(16.8777709759383,18.1912387444812,-20.6484905850079));
#90264=CARTESIAN_POINT('Ctrl Pts',(16.8488257062074,18.2457962822831,-20.6524166966287));
#90265=CARTESIAN_POINT('Ctrl Pts',(16.8063135236479,18.3351579117933,-20.658582697587));
#90266=CARTESIAN_POINT('Ctrl Pts',(16.7912114314477,18.3691880444925,-20.6608723594011));
#90267=CARTESIAN_POINT('Ctrl Pts',(16.7727688479727,18.4138894368113,-20.6638069323112));
#90268=CARTESIAN_POINT('Ctrl Pts',(16.7686050585361,18.4242118372078,-20.6644796217732));
#90269=CARTESIAN_POINT('Ctrl Pts',(16.7619670934183,18.4410494996135,-20.6655689840445));
#90270=CARTESIAN_POINT('Ctrl Pts',(16.7594433795558,18.4475448853054,-20.6659873210957));
#90271=CARTESIAN_POINT('Ctrl Pts',(16.7546526122558,18.4600577481487,-20.6667896098439));
#90272=CARTESIAN_POINT('Ctrl Pts',(16.7523808176238,18.4660733160689,-20.6671737171445));
#90273=CARTESIAN_POINT('Ctrl Pts',(16.7485503973944,18.4763575531617,-20.6678277065683));
#90274=CARTESIAN_POINT('Ctrl Pts',(16.7469780570343,18.480621024627,-20.6680980434942));
#90275=CARTESIAN_POINT('Ctrl Pts',(16.7454194503208,18.4848895418481,-20.6683679253911));
#90276=CARTESIAN_POINT('',(16.6170007438876,19.2127747167393,-19.6896814481124));
#90277=CARTESIAN_POINT('Ctrl Pts',(16.7454193207648,18.4848898966601,-20.4442392307736));
#90278=CARTESIAN_POINT('Ctrl Pts',(16.7951094570157,18.3488046880358,-20.4346845890896));
#90279=CARTESIAN_POINT('Ctrl Pts',(16.8586919903781,18.2180328599362,-20.4252945852796));
#90280=CARTESIAN_POINT('Ctrl Pts',(16.9464403518679,18.076640949622,-20.4150699242177));
#90281=CARTESIAN_POINT('Ctrl Pts',(16.9579092607725,18.0587666519309,-20.4137750718324));
#90282=CARTESIAN_POINT('Ctrl Pts',(16.9742421992522,18.0341352382721,-20.4119869468974));
#90283=CARTESIAN_POINT('Ctrl Pts',(16.9788797521117,18.0272301307979,-20.4114852460803));
#90284=CARTESIAN_POINT('Ctrl Pts',(16.9869555489791,18.015357419482,-20.4106218260161));
#90285=CARTESIAN_POINT('Ctrl Pts',(16.9903745565624,18.0103769082832,-20.4102593852774));
#90286=CARTESIAN_POINT('Ctrl Pts',(16.9974994301775,18.0000926407794,-20.409510446105));
#90287=CARTESIAN_POINT('Ctrl Pts',(17.0012083895321,17.9947910961785,-20.4091240706906));
#90288=CARTESIAN_POINT('Ctrl Pts',(17.0099528054985,17.9824131287256,-20.4082212224996));
#90289=CARTESIAN_POINT('Ctrl Pts',(17.015007643309,17.975350490551,-20.4077054996938));
#90290=CARTESIAN_POINT('Ctrl Pts',(17.0315678675804,17.9525107809737,-20.4060356658415));
#90291=CARTESIAN_POINT('Ctrl Pts',(17.0432483121647,17.9368614487756,-20.4048883353177));
#90292=CARTESIAN_POINT('Ctrl Pts',(17.1041456268364,17.8575842380121,-20.3990558847617));
#90293=CARTESIAN_POINT('Ctrl Pts',(17.1567462473642,17.7966336620975,-20.3945073887811));
#90294=CARTESIAN_POINT('Ctrl Pts',(17.3295172094598,17.6180973747365,-20.3807325332093));
#90295=CARTESIAN_POINT('Ctrl Pts',(17.4602838261406,17.5117206194863,-20.3718906604477));
#90296=CARTESIAN_POINT('Ctrl Pts',(17.6034502233839,17.4211541223408,-20.362377959221));
#90297=CARTESIAN_POINT('Ctrl Pts',(17.6046648859707,17.4203874614015,-20.3622972585964));
#90298=CARTESIAN_POINT('Ctrl Pts',(17.6514511910329,17.3909238013793,-20.3591890968416));
#90299=CARTESIAN_POINT('Ctrl Pts',(17.6980965354763,17.3639774611268,-20.3560999837281));
#90300=CARTESIAN_POINT('Ctrl Pts',(17.7534420070124,17.334761371595,-20.3523862289768));
#90301=CARTESIAN_POINT('Ctrl Pts',(17.7611952461297,17.3307297339948,-20.3518648965471));
#90302=CARTESIAN_POINT('Ctrl Pts',(17.7729670160884,17.3247007820764,-20.3510713909671));
#90303=CARTESIAN_POINT('Ctrl Pts',(17.7769674110774,17.3226679956657,-20.3508013931219));
#90304=CARTESIAN_POINT('Ctrl Pts',(17.78415687445,17.3190434093554,-20.3503154909686));
#90305=CARTESIAN_POINT('Ctrl Pts',(17.7873435244899,17.3174469320561,-20.3500998841084));
#90306=CARTESIAN_POINT('Ctrl Pts',(17.7942733320142,17.3139970386509,-20.3496304933057));
#90307=CARTESIAN_POINT('Ctrl Pts',(17.798017898015,17.3121466749749,-20.3493765292322));
#90308=CARTESIAN_POINT('Ctrl Pts',(17.8085434240306,17.3069842233638,-20.3486618058049));
#90309=CARTESIAN_POINT('Ctrl Pts',(17.8153365749291,17.3036973341438,-20.3481995251479));
#90310=CARTESIAN_POINT('Ctrl Pts',(17.8558881362349,17.2843432208021,-20.3454346602757));
#90311=CARTESIAN_POINT('Ctrl Pts',(17.8900475910066,17.2691373054308,-20.3430839405494));
#90312=CARTESIAN_POINT('Ctrl Pts',(18.0034021983097,17.2222338429609,-20.3352546371643));
#90313=CARTESIAN_POINT('Ctrl Pts',(18.0841091410243,17.1944177488118,-20.3296382492006));
#90314=CARTESIAN_POINT('Ctrl Pts',(18.3376594501303,17.1238357381799,-20.3122512658053));
#90315=CARTESIAN_POINT('Ctrl Pts',(18.5144187994228,17.0979100826066,-20.3005605642841));
#90316=CARTESIAN_POINT('Ctrl Pts',(18.7151581518733,17.0939610613943,-20.2882046004458));
#90317=CARTESIAN_POINT('Ctrl Pts',(18.7379611010077,17.0938809064429,-20.2868128514246));
#90318=CARTESIAN_POINT('Ctrl Pts',(18.7702757283948,17.0942894377574,-20.28485664383));
#90319=CARTESIAN_POINT('Ctrl Pts',(18.7797890394258,17.0944738600074,-20.2842827146958));
#90320=CARTESIAN_POINT('Ctrl Pts',(18.7952600142245,17.0948781353936,-20.2833524899106));
#90321=CARTESIAN_POINT('Ctrl Pts',(18.8012184839367,17.0950590245106,-20.28299497837));
#90322=CARTESIAN_POINT('Ctrl Pts',(18.8137017532411,17.0954907788277,-20.2822475252268));
#90323=CARTESIAN_POINT('Ctrl Pts',(18.8202263250073,17.0957466684382,-20.2818577450732));
#90324=CARTESIAN_POINT('Ctrl Pts',(18.8357680937032,17.0964282363634,-20.2809313404213));
#90325=CARTESIAN_POINT('Ctrl Pts',(18.8447840042838,17.0968814137556,-20.2803955832328));
#90326=CARTESIAN_POINT('Ctrl Pts',(18.8752566420369,17.0986085676984,-20.2785901924775));
#90327=CARTESIAN_POINT('Ctrl Pts',(18.8966972190901,17.1001516712112,-20.2773289930256));
#90328=CARTESIAN_POINT('Ctrl Pts',(19.0968831507863,17.1176276483302,-20.265629100803));
#90329=CARTESIAN_POINT('Ctrl Pts',(19.2729427661926,17.1558991105659,-20.2559871738058));
#90330=CARTESIAN_POINT('Ctrl Pts',(19.55563534682,17.2562304319389,-20.2396619613805));
#90331=CARTESIAN_POINT('Ctrl Pts',(19.665528929809,17.306149852173,-20.2330511530822));
#90332=CARTESIAN_POINT('Ctrl Pts',(19.7788432136098,17.3697825131858,-20.225348983304));
#90333=CARTESIAN_POINT('Ctrl Pts',(19.7870915041383,17.3744876937277,-20.224782954918));
#90334=CARTESIAN_POINT('Ctrl Pts',(19.7992711526086,17.3815445198093,-20.2239387186065));
#90335=CARTESIAN_POINT('Ctrl Pts',(19.8032271129766,17.383853765417,-20.223663182423));
#90336=CARTESIAN_POINT('Ctrl Pts',(19.8102543767232,17.3879864853511,-20.2231713033203));
#90337=CARTESIAN_POINT('Ctrl Pts',(19.8133285905668,17.3898049112292,-20.2229552893266));
#90338=CARTESIAN_POINT('Ctrl Pts',(19.8199306039365,17.3937326510743,-20.2224895818453));
#90339=CARTESIAN_POINT('Ctrl Pts',(19.8234568151281,17.3958444305393,-20.2222397327143));
#90340=CARTESIAN_POINT('Ctrl Pts',(19.8331790620241,17.4017054309922,-20.2215478438911));
#90341=CARTESIAN_POINT('Ctrl Pts',(19.8393619751074,17.4054761568096,-20.2211044324042));
#90342=CARTESIAN_POINT('Ctrl Pts',(19.873223284115,17.4263660121669,-20.2186578316101));
#90343=CARTESIAN_POINT('Ctrl Pts',(19.9005218241838,17.4440889309403,-20.2166182827177));
#90344=CARTESIAN_POINT('Ctrl Pts',(20.0617804767118,17.5541481560703,-20.2042121260728));
#90345=CARTESIAN_POINT('Ctrl Pts',(20.1851376989531,17.6610456984756,-20.1932557450537));
#90346=CARTESIAN_POINT('Ctrl Pts',(20.3739364296115,17.8671467048019,-20.1749987294241));
#90347=CARTESIAN_POINT('Ctrl Pts',(20.4455836710734,17.9596717797892,-20.1675581114734));
#90348=CARTESIAN_POINT('Ctrl Pts',(20.5170242791566,18.0696334490762,-20.1595512628849));
#90349=CARTESIAN_POINT('Ctrl Pts',(20.524687757949,18.0816946591474,-20.158683290665));
#90350=CARTESIAN_POINT('Ctrl Pts',(20.536690218276,18.1010142094309,-20.1573089875403));
#90351=CARTESIAN_POINT('Ctrl Pts',(20.5411087453653,18.1082223868808,-20.1567997285898));
#90352=CARTESIAN_POINT('Ctrl Pts',(20.548825353746,18.1209818238136,-20.1559043530417));
#90353=CARTESIAN_POINT('Ctrl Pts',(20.5521414191056,18.1265220285402,-20.1555175803213));
#90354=CARTESIAN_POINT('Ctrl Pts',(20.5589476833768,18.1380123318585,-20.1547195132047));
#90355=CARTESIAN_POINT('Ctrl Pts',(20.562434254574,18.1439644984921,-20.1543083541904));
#90356=CARTESIAN_POINT('Ctrl Pts',(20.5713091275901,18.1592866376952,-20.1532556456487));
#90357=CARTESIAN_POINT('Ctrl Pts',(20.5766549174612,18.1686811003867,-20.1526156374255));
#90358=CARTESIAN_POINT('Ctrl Pts',(20.5986660895473,18.2080612082621,-20.1499549702035));
#90359=CARTESIAN_POINT('Ctrl Pts',(20.6146738802308,18.2384097479925,-20.1479578400622));
#90360=CARTESIAN_POINT('Ctrl Pts',(20.6544542897448,18.3184861920493,-20.1428137541068));
#90361=CARTESIAN_POINT('Ctrl Pts',(20.6770357547662,18.3687777742881,-20.1397061875812));
#90362=CARTESIAN_POINT('Ctrl Pts',(20.7384920387879,18.5213208553026,-20.1305617656709));
#90363=CARTESIAN_POINT('Ctrl Pts',(20.7714353469632,18.6257618034146,-20.1246736398536));
#90364=CARTESIAN_POINT('Ctrl Pts',(20.8065061135522,18.7768346781319,-20.1162298807359));
#90365=CARTESIAN_POINT('Ctrl Pts',(20.8154023161376,18.821711831227,-20.1137289265928));
#90366=CARTESIAN_POINT('Ctrl Pts',(20.8265388066548,18.8893035146133,-20.1099303719367));
#90367=CARTESIAN_POINT('Ctrl Pts',(20.8298771683697,18.9118242497901,-20.1086594736193));
#90368=CARTESIAN_POINT('Ctrl Pts',(20.83297703449,18.9353456325496,-20.1073227477522));
#90369=CARTESIAN_POINT('Ctrl Pts',(20.8331018207595,18.9362974923838,-20.1072686373755));
#90370=CARTESIAN_POINT('Ctrl Pts',(20.8354237709073,18.9541031105657,-20.1062561377202));
#90371=CARTESIAN_POINT('Ctrl Pts',(20.8374184851179,18.9709822396471,-20.1052912359404));
#90372=CARTESIAN_POINT('Ctrl Pts',(20.8428741287167,19.0224587337404,-20.1023282493572));
#90373=CARTESIAN_POINT('Ctrl Pts',(20.8456859739245,19.0571171422363,-20.100305447186));
#90374=CARTESIAN_POINT('Ctrl Pts',(20.8480377917233,19.0988287089154,-20.0978209177924));
#90375=CARTESIAN_POINT('Ctrl Pts',(20.848397780341,19.1058324823669,-20.0974020474362));
#90376=CARTESIAN_POINT('Ctrl Pts',(20.8489303620409,19.1173059700972,-20.0967128982812));
#90377=CARTESIAN_POINT('Ctrl Pts',(20.8491236036519,19.121774734787,-20.096443748811));
#90378=CARTESIAN_POINT('Ctrl Pts',(20.8494453400723,19.1298044927019,-20.0959587495865));
#90379=CARTESIAN_POINT('Ctrl Pts',(20.8495790078724,19.1333652243882,-20.0957431924547));
#90380=CARTESIAN_POINT('Ctrl Pts',(20.8498502177277,19.141111561245,-20.0952731770432));
#90381=CARTESIAN_POINT('Ctrl Pts',(20.8499843282821,19.1452971880862,-20.0950185346279));
#90382=CARTESIAN_POINT('Ctrl Pts',(20.8503267812669,19.1570771596271,-20.0943000228492));
#90383=CARTESIAN_POINT('Ctrl Pts',(20.8505066611533,19.1646721779322,-20.0938346067005));
#90384=CARTESIAN_POINT('Ctrl Pts',(20.8513458920726,19.210534729721,-20.0910118009918));
#90385=CARTESIAN_POINT('Ctrl Pts',(20.8510082092333,19.2488108662269,-20.0886039480136));
#90386=CARTESIAN_POINT('Ctrl Pts',(20.8464434638979,19.3757909155159,-20.080488521367));
#90387=CARTESIAN_POINT('Ctrl Pts',(20.837673941922,19.4642339218762,-20.0746327658124));
#90388=CARTESIAN_POINT('Ctrl Pts',(20.7955385104864,19.7225135177095,-20.0573405881421));
#90389=CARTESIAN_POINT('Ctrl Pts',(20.7468892543734,19.8891492761447,-20.0459988291737));
#90390=CARTESIAN_POINT('Ctrl Pts',(20.6693363086393,20.069311835175,-20.0339236085031));
#90391=CARTESIAN_POINT('Ctrl Pts',(20.659826333289,20.0904423431364,-20.0325090175927));
#90392=CARTESIAN_POINT('Ctrl Pts',(20.6458983529489,20.1200794130089,-20.0305266084104));
#90393=CARTESIAN_POINT('Ctrl Pts',(20.6417668286636,20.1287180521974,-20.0299489719761));
#90394=CARTESIAN_POINT('Ctrl Pts',(20.6349635673037,20.1426985469259,-20.0290143826255));
#90395=CARTESIAN_POINT('Ctrl Pts',(20.6323276219431,20.1480575795881,-20.0286561910765));
#90396=CARTESIAN_POINT('Ctrl Pts',(20.6267666007581,20.1592436946251,-20.0279086139702));
#90397=CARTESIAN_POINT('Ctrl Pts',(20.6238372083006,20.1650685703505,-20.0275193841726));
#90398=CARTESIAN_POINT('Ctrl Pts',(20.6168118450126,20.1788786568011,-20.0265966400399));
#90399=CARTESIAN_POINT('Ctrl Pts',(20.6126918949556,20.1868515797068,-20.0260639746937));
#90400=CARTESIAN_POINT('Ctrl Pts',(20.5986777256448,20.2135540683878,-20.0242799973124));
#90401=CARTESIAN_POINT('Ctrl Pts',(20.5885529357114,20.2321616606394,-20.0230368453451));
#90402=CARTESIAN_POINT('Ctrl Pts',(20.5321660056872,20.3321852333781,-20.0163493070367));
#90403=CARTESIAN_POINT('Ctrl Pts',(20.4808176932904,20.4106200244604,-20.011093074299));
#90404=CARTESIAN_POINT('Ctrl Pts',(20.3294248105633,20.611435744796,-19.9972477043145));
#90405=CARTESIAN_POINT('Ctrl Pts',(20.2206238157918,20.7264348672007,-19.9889097799719));
#90406=CARTESIAN_POINT('Ctrl Pts',(20.085155597946,20.8408614855524,-19.9789094993389));
#90407=CARTESIAN_POINT('Ctrl Pts',(20.070072716307,20.8532483264439,-19.9778002284386));
#90408=CARTESIAN_POINT('Ctrl Pts',(20.0295089309296,20.8856327032057,-19.9748214525541));
#90409=CARTESIAN_POINT('Ctrl Pts',(20.0037377900495,20.9052561105954,-19.9729335674327));
#90410=CARTESIAN_POINT('Ctrl Pts',(19.9719831792781,20.9283041648871,-19.9705992232097));
#90411=CARTESIAN_POINT('Ctrl Pts',(19.9664186391456,20.9323019031832,-19.9701898668058));
#90412=CARTESIAN_POINT('Ctrl Pts',(19.9572299776596,20.938835926303,-19.969513239724));
#90413=CARTESIAN_POINT('Ctrl Pts',(19.9536170911705,20.9413880248592,-19.9692470299863));
#90414=CARTESIAN_POINT('Ctrl Pts',(19.9470815811581,20.9459739928504,-19.968765118753));
#90415=CARTESIAN_POINT('Ctrl Pts',(19.944161806287,20.9480118251388,-19.9685496930646));
#90416=CARTESIAN_POINT('Ctrl Pts',(19.9377636838038,20.9524533786159,-19.9680773381431));
#90417=CARTESIAN_POINT('Ctrl Pts',(19.9342833133151,20.9548540200928,-19.9678202102555));
#90418=CARTESIAN_POINT('Ctrl Pts',(19.9243754486021,20.9616444168809,-19.9670877607319));
#90419=CARTESIAN_POINT('Ctrl Pts',(19.91793098244,20.9660091189213,-19.9666107969111));
#90420=CARTESIAN_POINT('Ctrl Pts',(19.8767482323292,20.9935712756114,-19.9635600755652));
#90421=CARTESIAN_POINT('Ctrl Pts',(19.8413563079454,21.0157701634958,-19.9609261472213));
#90422=CARTESIAN_POINT('Ctrl Pts',(19.6395355693048,21.1341866667008,-19.9459377789451));
#90423=CARTESIAN_POINT('Ctrl Pts',(19.4612564030848,21.2084364265669,-19.9329169427359));
#90424=CARTESIAN_POINT('Ctrl Pts',(19.2540212365793,21.2632561548984,-19.9191612501326));
#90425=CARTESIAN_POINT('Ctrl Pts',(19.2325683661098,21.2685730961572,-19.9177514742479));
#90426=CARTESIAN_POINT('Ctrl Pts',(19.1536498796683,21.2868256808884,-19.9126185722941));
#90427=CARTESIAN_POINT('Ctrl Pts',(19.0957313323204,21.2976982998993,-19.9089552601452));
#90428=CARTESIAN_POINT('Ctrl Pts',(19.0253362304984,21.3078933032022,-19.9046242368097));
#90429=CARTESIAN_POINT('Ctrl Pts',(19.0132274407544,21.3095400568895,-19.9038835015789));
#90430=CARTESIAN_POINT('Ctrl Pts',(18.9932448755306,21.3120815960814,-19.9026679476835));
#90431=CARTESIAN_POINT('Ctrl Pts',(18.9853792503067,21.3130371676208,-19.9021912196226));
#90432=CARTESIAN_POINT('Ctrl Pts',(18.9711788303664,21.3146814879064,-19.9013336332256));
#90433=CARTESIAN_POINT('Ctrl Pts',(18.9648459699464,21.3153858343157,-19.9009522873901));
#90434=CARTESIAN_POINT('Ctrl Pts',(18.9512983059785,21.3168307258475,-19.9001388121778));
#90435=CARTESIAN_POINT('Ctrl Pts',(18.9440826675226,21.3175628104853,-19.8997069538151));
#90436=CARTESIAN_POINT('Ctrl Pts',(18.9245090377018,21.3194471418206,-19.8985391994712));
#90437=CARTESIAN_POINT('Ctrl Pts',(18.9121443229789,21.3205278271144,-19.8978055583238));
#90438=CARTESIAN_POINT('Ctrl Pts',(18.8484139041408,21.3255335756306,-19.894044088778));
#90439=CARTESIAN_POINT('Ctrl Pts',(18.7969244025949,21.3276917430525,-19.8910721249936));
#90440=CARTESIAN_POINT('Ctrl Pts',(18.5728865572419,21.3288986366361,-19.8783578230477));
#90441=CARTESIAN_POINT('Ctrl Pts',(18.4009110296881,21.3087378002402,-19.8692175386638));
#90442=CARTESIAN_POINT('Ctrl Pts',(18.1458531918414,21.2466497309787,-19.8547940556994));
#90443=CARTESIAN_POINT('Ctrl Pts',(18.059876760204,21.2198156477527,-19.8497581624898));
#90444=CARTESIAN_POINT('Ctrl Pts',(17.9668659605149,21.1841415467889,-19.8438559575789));
#90445=CARTESIAN_POINT('Ctrl Pts',(17.9578762415875,21.180622832386,-19.8432806405838));
#90446=CARTESIAN_POINT('Ctrl Pts',(17.9446283920641,21.175332642627,-19.842425181036));
#90447=CARTESIAN_POINT('Ctrl Pts',(17.940351333229,21.1736084834004,-19.8421478143613));
#90448=CARTESIAN_POINT('Ctrl Pts',(17.9327687443787,21.1705229661533,-19.8416539253669));
#90449=CARTESIAN_POINT('Ctrl Pts',(17.9294609936926,21.1691671958705,-19.8414377423418));
#90450=CARTESIAN_POINT('Ctrl Pts',(17.9223759646983,21.1662422241238,-19.8409730972151));
#90451=CARTESIAN_POINT('Ctrl Pts',(17.918599852042,21.1646704757281,-19.8407244869627));
#90452=CARTESIAN_POINT('Ctrl Pts',(17.9083668935981,21.1603763300653,-19.8400481911202));
#90453=CARTESIAN_POINT('Ctrl Pts',(17.9019190381823,21.1576328293799,-19.8396192557389));
#90454=CARTESIAN_POINT('Ctrl Pts',(17.8682577773545,21.1431124890333,-19.837365775939));
#90455=CARTESIAN_POINT('Ctrl Pts',(17.8412818606033,21.1307974848635,-19.8355111455508));
#90456=CARTESIAN_POINT('Ctrl Pts',(17.7614691595869,21.0923156645977,-19.8298961231196));
#90457=CARTESIAN_POINT('Ctrl Pts',(17.7094595091302,21.0645049725264,-19.8260668971797));
#90458=CARTESIAN_POINT('Ctrl Pts',(17.5778274998539,20.9868842380858,-19.81604072932));
#90459=CARTESIAN_POINT('Ctrl Pts',(17.5002332541628,20.9338812185698,-19.8097994804667));
#90460=CARTESIAN_POINT('Ctrl Pts',(17.3244637011971,20.7958346248445,-19.7951389992581));
#90461=CARTESIAN_POINT('Ctrl Pts',(17.2300711467867,20.7065607221792,-19.7868399698015));
#90462=CARTESIAN_POINT('Ctrl Pts',(17.1340194027413,20.5973619455243,-19.7779590533407));
#90463=CARTESIAN_POINT('Ctrl Pts',(17.1237432475517,20.5854128083935,-19.7770022097991));
#90464=CARTESIAN_POINT('Ctrl Pts',(17.1084069752401,20.5671716218917,-19.7755636315011));
#90465=CARTESIAN_POINT('Ctrl Pts',(17.1032480138184,20.5609637449033,-19.7750778495655));
#90466=CARTESIAN_POINT('Ctrl Pts',(17.0940714623327,20.5497920554364,-19.7742103486278));
#90467=CARTESIAN_POINT('Ctrl Pts',(17.0900406107421,20.544839309741,-19.7738280934817));
#90468=CARTESIAN_POINT('Ctrl Pts',(17.0815397717946,20.5342971753022,-19.7730193399167));
#90469=CARTESIAN_POINT('Ctrl Pts',(17.0770755863145,20.5287031946639,-19.7725930779458));
#90470=CARTESIAN_POINT('Ctrl Pts',(17.0652157884595,20.5136863538956,-19.7714564059599));
#90471=CARTESIAN_POINT('Ctrl Pts',(17.0578715697348,20.5042230957822,-19.7707480473508));
#90472=CARTESIAN_POINT('Ctrl Pts',(17.0226437435007,20.4580266781723,-19.7673276240952));
#90473=CARTESIAN_POINT('Ctrl Pts',(16.9958839238421,20.4204497673187,-19.7646597669655));
#90474=CARTESIAN_POINT('Ctrl Pts',(16.9201884532234,20.3064483393434,-19.7568622611088));
#90475=CARTESIAN_POINT('Ctrl Pts',(16.8749127709369,20.227718291307,-19.7518591836261));
#90476=CARTESIAN_POINT('Ctrl Pts',(16.8016346996246,20.0789268562845,-19.742813827327));
#90477=CARTESIAN_POINT('Ctrl Pts',(16.7720548873629,20.0098140435765,-19.7387593446402));
#90478=CARTESIAN_POINT('Ctrl Pts',(16.7108960476806,19.8428844124266,-19.7290395779754));
#90479=CARTESIAN_POINT('Ctrl Pts',(16.6826432394489,19.7440640634662,-19.7233423083425));
#90480=CARTESIAN_POINT('Ctrl Pts',(16.6596911820583,19.6341144339448,-19.7166879664956));
#90481=CARTESIAN_POINT('Ctrl Pts',(16.6577762606434,19.6246156095647,-19.7161105263504));
#90482=CARTESIAN_POINT('Ctrl Pts',(16.6550450438842,19.6105705463484,-19.715252503474));
#90483=CARTESIAN_POINT('Ctrl Pts',(16.6541782774247,19.6060340902309,-19.7149747206897));
#90484=CARTESIAN_POINT('Ctrl Pts',(16.6526668244177,19.5979806161788,-19.7144803727382));
#90485=CARTESIAN_POINT('Ctrl Pts',(16.6520161959579,19.594464763146,-19.7142641492217));
#90486=CARTESIAN_POINT('Ctrl Pts',(16.6506411799459,19.5869278126374,-19.7137997361241));
#90487=CARTESIAN_POINT('Ctrl Pts',(16.649919536023,19.5829063221139,-19.7135514000579));
#90488=CARTESIAN_POINT('Ctrl Pts',(16.6484624925562,19.5746492623871,-19.7130404378394));
#90489=CARTESIAN_POINT('Ctrl Pts',(16.6477283444895,19.5704134939939,-19.7127777435228));
#90490=CARTESIAN_POINT('Ctrl Pts',(16.6459030700641,19.559688277618,-19.7121111772311));
#90491=CARTESIAN_POINT('Ctrl Pts',(16.6448292996858,19.553195976245,-19.7117063806325));
#90492=CARTESIAN_POINT('Ctrl Pts',(16.6260483507081,19.4362572281377,-19.7043930651482));
#90493=CARTESIAN_POINT('Ctrl Pts',(16.6170944881852,19.3245991019815,-19.6970632334726));
#90494=CARTESIAN_POINT('Ctrl Pts',(16.6170007438876,19.2127747167393,-19.6896814481124));
#90495=CARTESIAN_POINT('Ctrl Pts',(16.6170007453285,19.2127764346725,-19.6896815615171));
#90496=CARTESIAN_POINT('Ctrl Pts',(16.6169163433609,19.1121935620679,-19.6830418547794));
#90497=CARTESIAN_POINT('Ctrl Pts',(16.6240004448591,19.011723653978,-19.6763771951571));
#90498=CARTESIAN_POINT('Ctrl Pts',(16.6507394666926,18.824217512163,-19.6641100541146));
#90499=CARTESIAN_POINT('Ctrl Pts',(16.6687967940729,18.7371705642616,-19.6584854932288));
#90500=CARTESIAN_POINT('Ctrl Pts',(16.697713687571,18.6316459983499,-19.6517701141624));
#90501=CARTESIAN_POINT('Ctrl Pts',(16.703445317346,18.6118666816241,-19.650515670969));
#90502=CARTESIAN_POINT('Ctrl Pts',(16.7120584357468,18.5836882444869,-19.6487341358836));
#90503=CARTESIAN_POINT('Ctrl Pts',(16.7147054415501,18.5752192061564,-19.6481994217554));
#90504=CARTESIAN_POINT('Ctrl Pts',(16.7193842606274,18.5605734498584,-19.6472759140045));
#90505=CARTESIAN_POINT('Ctrl Pts',(16.7213914142644,18.5543890371431,-19.6468863166421));
#90506=CARTESIAN_POINT('Ctrl Pts',(16.7253038020368,18.542520741734,-19.6461393276805));
#90507=CARTESIAN_POINT('Ctrl Pts',(16.7272047463052,18.5368355205668,-19.6457817991304));
#90508=CARTESIAN_POINT('Ctrl Pts',(16.7322440872851,18.5219743757202,-19.6448479608351));
#90509=CARTESIAN_POINT('Ctrl Pts',(16.7354214541583,18.5128117403889,-19.6442729442935));
#90510=CARTESIAN_POINT('Ctrl Pts',(16.7408847780493,18.4973999849371,-19.6433068766095));
#90511=CARTESIAN_POINT('Ctrl Pts',(16.7431373831887,18.4911393820238,-19.6429147521337));
#90512=CARTESIAN_POINT('Ctrl Pts',(16.7454194502465,18.4848895420517,-19.6425235887674));
#90513=CARTESIAN_POINT('Origin',(18.734,19.211,0.));
#90514=CARTESIAN_POINT('',(16.7454194035981,18.4848896698064,-18.845275399947));
#90515=CARTESIAN_POINT('',(16.7454194503191,18.4848895418526,-19.066324519095));
#90516=CARTESIAN_POINT('',(16.7454194503191,18.4848895418526,0.));
#90517=CARTESIAN_POINT('',(16.6180378694014,19.2091158125651,-19.1109437209775));
#90518=CARTESIAN_POINT('Ctrl Pts',(16.7454194503191,18.4848895418526,-19.066324519095));
#90519=CARTESIAN_POINT('Ctrl Pts',(16.7290739265814,18.5296546188661,-19.0692018281724));
#90520=CARTESIAN_POINT('Ctrl Pts',(16.7142587320644,18.5749225375465,-19.0720791372497));
#90521=CARTESIAN_POINT('Ctrl Pts',(16.7009992479655,18.6205790127144,-19.074956446327));
#90522=CARTESIAN_POINT('Ctrl Pts',(16.6758066766554,18.7073247712869,-19.0804232362542));
#90523=CARTESIAN_POINT('Ctrl Pts',(16.6561521069702,18.7957464915279,-19.0858900261814));
#90524=CARTESIAN_POINT('Ctrl Pts',(16.6422180861817,18.885212607637,-19.0913568161086));
#90525=CARTESIAN_POINT('Ctrl Pts',(16.6285119268907,18.9732156942664,-19.0967342082262));
#90526=CARTESIAN_POINT('Ctrl Pts',(16.6203407792442,19.0622293912807,-19.1021116003437));
#90527=CARTESIAN_POINT('Ctrl Pts',(16.6178326248363,19.1516313189224,-19.1074889924612));
#90528=CARTESIAN_POINT('Ctrl Pts',(16.6172955000016,19.1707768689146,-19.1086405686333));
#90529=CARTESIAN_POINT('Ctrl Pts',(16.6170179137274,19.1899401417913,-19.1097921448054));
#90530=CARTESIAN_POINT('Ctrl Pts',(16.6170008393112,19.2091148891275,-19.1109437209775));
#90531=CARTESIAN_POINT('Ctrl Pts',(16.6180378694014,19.2091158125651,-19.1109437209775));
#90532=CARTESIAN_POINT('Ctrl Pts',(16.6223667223562,19.7149949952687,-19.1413398983212));
#90533=CARTESIAN_POINT('Ctrl Pts',(17.0578063895244,20.9330881407267,-19.2141280112252));
#90534=CARTESIAN_POINT('Ctrl Pts',(19.0938031815268,21.6882711475644,-19.3293080596899));
#90535=CARTESIAN_POINT('Ctrl Pts',(21.0117476411797,20.249362367724,-19.4564838663713));
#90536=CARTESIAN_POINT('Ctrl Pts',(20.8400000149027,17.8578205193087,-19.5836596730528));
#90537=CARTESIAN_POINT('Ctrl Pts',(18.7361280844105,16.7077369418623,-19.7108354797341));
#90538=CARTESIAN_POINT('Ctrl Pts',(17.1750895095576,17.5576360166973,-19.8051103625842));
#90539=CARTESIAN_POINT('Ctrl Pts',(16.7978195031743,18.3361166232031,-19.8569933098738));
#90540=CARTESIAN_POINT('Ctrl Pts',(16.7452305124652,18.4848205810513,-19.866484321603));
#90541=CARTESIAN_POINT('Ctrl Pts',(16.7454194502465,18.4848895420517,-19.6425235887674));
#90542=CARTESIAN_POINT('Ctrl Pts',(16.7513354922673,18.4686874257408,-19.6415095349059));
#90543=CARTESIAN_POINT('Ctrl Pts',(16.7574495349329,18.4525576420121,-19.6405019471072));
#90544=CARTESIAN_POINT('Ctrl Pts',(16.8210985510288,18.2906410055608,-19.630401539589));
#90545=CARTESIAN_POINT('Ctrl Pts',(16.8944570177936,18.1515939492392,-19.6218931420355));
#90546=CARTESIAN_POINT('Ctrl Pts',(17.0277672172459,17.9552320220489,-19.6090034063394));
#90547=CARTESIAN_POINT('Ctrl Pts',(17.0768009080434,17.8911994892854,-19.604626137739));
#90548=CARTESIAN_POINT('Ctrl Pts',(17.1558585034803,17.7993313055239,-19.5978417486546));
#90549=CARTESIAN_POINT('Ctrl Pts',(17.1832341456381,17.7693121149191,-19.5955350803859));
#90550=CARTESIAN_POINT('Ctrl Pts',(17.2274000528777,17.7235954537048,-19.5918441208389));
#90551=CARTESIAN_POINT('Ctrl Pts',(17.2436121369262,17.7073512360309,-19.5904952799347));
#90552=CARTESIAN_POINT('Ctrl Pts',(17.2647242231728,17.6868741937084,-19.5887411943746));
#90553=CARTESIAN_POINT('Ctrl Pts',(17.2693846473904,17.6823951955441,-19.5883541338572));
#90554=CARTESIAN_POINT('Ctrl Pts',(17.2765098109158,17.6756099055338,-19.5877624579846));
#90555=CARTESIAN_POINT('Ctrl Pts',(17.2789597241795,17.6732880019862,-19.5875590320492));
#90556=CARTESIAN_POINT('Ctrl Pts',(17.2840076628687,17.6685266865125,-19.5871398876463));
#90557=CARTESIAN_POINT('Ctrl Pts',(17.2866062745757,17.6660879948744,-19.5869241170202));
#90558=CARTESIAN_POINT('Ctrl Pts',(17.2924855853297,17.6605983541618,-19.5864359426865));
#90559=CARTESIAN_POINT('Ctrl Pts',(17.2957697997764,17.6575512684896,-19.5861632519385));
#90560=CARTESIAN_POINT('Ctrl Pts',(17.305464263719,17.6486138640673,-19.5853583984496));
#90561=CARTESIAN_POINT('Ctrl Pts',(17.3119011128783,17.642752718206,-19.5848241074302));
#90562=CARTESIAN_POINT('Ctrl Pts',(17.3578525104004,17.6014266866031,-19.5810118571994));
#90563=CARTESIAN_POINT('Ctrl Pts',(17.3986495521066,17.5674227057259,-19.5776377272081));
#90564=CARTESIAN_POINT('Ctrl Pts',(17.452186768306,17.5261097408508,-19.573267983812));
#90565=CARTESIAN_POINT('Ctrl Pts',(17.4637871634084,17.5173472368749,-19.5723244435688));
#90566=CARTESIAN_POINT('Ctrl Pts',(17.5917504829377,17.42274270243,-19.5619592933419));
#90567=CARTESIAN_POINT('Ctrl Pts',(17.7165273210169,17.348917410824,-19.552272336456));
#90568=CARTESIAN_POINT('Ctrl Pts',(17.9293682558012,17.2508186041958,-19.5370858385326));
#90569=CARTESIAN_POINT('Ctrl Pts',(18.0131877941661,17.2184697766245,-19.5313990558285));
#90570=CARTESIAN_POINT('Ctrl Pts',(18.1185717919286,17.1853233382743,-19.5246178700095));
#90571=CARTESIAN_POINT('Ctrl Pts',(18.1384162424899,17.1794001740588,-19.5233562283486));
#90572=CARTESIAN_POINT('Ctrl Pts',(18.1669029171781,17.1713507692091,-19.5215663617672));
#90573=CARTESIAN_POINT('Ctrl Pts',(18.175476110062,17.1689864951104,-19.5210304164706));
#90574=CARTESIAN_POINT('Ctrl Pts',(18.1903461411556,17.1649863631273,-19.520105463878));
#90575=CARTESIAN_POINT('Ctrl Pts',(18.196636042038,17.163325392389,-19.5197156459303));
#90576=CARTESIAN_POINT('Ctrl Pts',(18.2087319605123,17.1601908021249,-19.5189687046807));
#90577=CARTESIAN_POINT('Ctrl Pts',(18.2145367632638,17.1587127817454,-19.5186114421817));
#90578=CARTESIAN_POINT('Ctrl Pts',(18.2297315446572,17.154912480575,-19.517679337098));
#90579=CARTESIAN_POINT('Ctrl Pts',(18.239131372457,17.1526298659422,-19.5171057782452));
#90580=CARTESIAN_POINT('Ctrl Pts',(18.2716674053281,17.1449647118447,-19.5151307937676));
#90581=CARTESIAN_POINT('Ctrl Pts',(18.2948788631051,17.1399070677099,-19.5137397928997));
#90582=CARTESIAN_POINT('Ctrl Pts',(18.4764690829838,17.1035298024291,-19.5029863845032));
#90583=CARTESIAN_POINT('Ctrl Pts',(18.6378759286409,17.0900285354248,-19.494243235366));
#90584=CARTESIAN_POINT('Ctrl Pts',(18.9302246812665,17.0990454625842,-19.4783544374037));
#90585=CARTESIAN_POINT('Ctrl Pts',(19.0605095737166,17.1152334077911,-19.4712321465482));
#90586=CARTESIAN_POINT('Ctrl Pts',(19.2001132485262,17.1459164044562,-19.4627978898593));
#90587=CARTESIAN_POINT('Ctrl Pts',(19.2117630323281,17.1485804774142,-19.4620877402309));
#90588=CARTESIAN_POINT('Ctrl Pts',(19.2282829172218,17.1525057209427,-19.4610709165965));
#90589=CARTESIAN_POINT('Ctrl Pts',(19.233172285768,17.1536858948858,-19.4607687440908));
#90590=CARTESIAN_POINT('Ctrl Pts',(19.2415875719835,17.1557489038434,-19.4602464789165));
#90591=CARTESIAN_POINT('Ctrl Pts',(19.2451155445436,17.1566234251094,-19.4600268643563));
#90592=CARTESIAN_POINT('Ctrl Pts',(19.251948857971,17.1583359729451,-19.4596001805042));
#90593=CARTESIAN_POINT('Ctrl Pts',(19.2552544339929,17.1591729015095,-19.4593931806813));
#90594=CARTESIAN_POINT('Ctrl Pts',(19.264161731883,17.1614510265473,-19.4588338179635));
#90595=CARTESIAN_POINT('Ctrl Pts',(19.2697595447368,17.162907188394,-19.4584806030637));
#90596=CARTESIAN_POINT('Ctrl Pts',(19.2904807578836,17.1683881710774,-19.457167063065));
#90597=CARTESIAN_POINT('Ctrl Pts',(19.3055649272845,17.1725575999223,-19.456198882689));
#90598=CARTESIAN_POINT('Ctrl Pts',(19.4501596590184,17.214256212632,-19.4468117091658));
#90599=CARTESIAN_POINT('Ctrl Pts',(19.5758408856351,17.263907782423,-19.4378492738161));
#90600=CARTESIAN_POINT('Ctrl Pts',(19.8385652757954,17.3979194730604,-19.4183720679032));
#90601=CARTESIAN_POINT('Ctrl Pts',(19.9725071704624,17.486632226586,-19.4079688140199));
#90602=CARTESIAN_POINT('Ctrl Pts',(20.1094644694638,17.6016105819765,-19.3970159620179));
#90603=CARTESIAN_POINT('Ctrl Pts',(20.1235891627616,17.6137903082944,-19.3958813755409));
#90604=CARTESIAN_POINT('Ctrl Pts',(20.1439336175515,17.6318075250723,-19.3942393830913));
#90605=CARTESIAN_POINT('Ctrl Pts',(20.1502816773317,17.6374982070091,-19.3937259012378));
#90606=CARTESIAN_POINT('Ctrl Pts',(20.1613680002001,17.6475579234683,-19.3928270847801));
#90607=CARTESIAN_POINT('Ctrl Pts',(20.1661209779698,17.6519105091277,-19.392441064033));
#90608=CARTESIAN_POINT('Ctrl Pts',(20.1753237741438,17.6604156518448,-19.3916922877939));
#90609=CARTESIAN_POINT('Ctrl Pts',(20.179775702215,17.6645658233437,-19.3913294364163));
#90610=CARTESIAN_POINT('Ctrl Pts',(20.1903950005449,17.674551274101,-19.3904623741943));
#90611=CARTESIAN_POINT('Ctrl Pts',(20.1965453170217,17.6804045982764,-19.389958943916));
#90612=CARTESIAN_POINT('Ctrl Pts',(20.2187278290756,17.7017717294069,-19.3881384275946));
#90613=CARTESIAN_POINT('Ctrl Pts',(20.2345501125293,17.7175020539885,-19.3868307625447));
#90614=CARTESIAN_POINT('Ctrl Pts',(20.378213301191,17.8649185441742,-19.3748614530499));
#90615=CARTESIAN_POINT('Ctrl Pts',(20.4886678815135,18.0124510933741,-19.3650341203674));
#90616=CARTESIAN_POINT('Ctrl Pts',(20.6187025237321,18.243411240363,-19.3505913375458));
#90617=CARTESIAN_POINT('Ctrl Pts',(20.6545501775305,18.3166753695062,-19.3461133563995));
#90618=CARTESIAN_POINT('Ctrl Pts',(20.7001659539281,18.4253760411333,-19.3393728575855));
#90619=CARTESIAN_POINT('Ctrl Pts',(20.7133803079529,18.459290746977,-19.3372565100043));
#90620=CARTESIAN_POINT('Ctrl Pts',(20.7282509523279,18.5005718107286,-19.3346454222987));
#90621=CARTESIAN_POINT('Ctrl Pts',(20.7307513370133,18.5076301347739,-19.3341977522896));
#90622=CARTESIAN_POINT('Ctrl Pts',(20.7345837881141,18.5186338782765,-19.3334977333009));
#90623=CARTESIAN_POINT('Ctrl Pts',(20.7359417773079,18.5225702945408,-19.333246893332));
#90624=CARTESIAN_POINT('Ctrl Pts',(20.7384409410638,18.5298845721234,-19.3327799843039));
#90625=CARTESIAN_POINT('Ctrl Pts',(20.7395851993978,18.5332613190467,-19.3325641005641));
#90626=CARTESIAN_POINT('Ctrl Pts',(20.7421556754325,18.5409104014784,-19.3320743392664));
#90627=CARTESIAN_POINT('Ctrl Pts',(20.7435767846128,18.5451843853615,-19.3318001663998));
#90628=CARTESIAN_POINT('Ctrl Pts',(20.747831065529,18.5581168284053,-19.3309690752267));
#90629=CARTESIAN_POINT('Ctrl Pts',(20.7506219526325,18.5667889402043,-19.3304097629595));
#90630=CARTESIAN_POINT('Ctrl Pts',(20.7716710779449,18.633672122517,-19.3260821477863));
#90631=CARTESIAN_POINT('Ctrl Pts',(20.7874596168193,18.6926246247417,-19.3221871938091));
#90632=CARTESIAN_POINT('Ctrl Pts',(20.8135818915649,18.8102855888011,-19.3143614751178));
#90633=CARTESIAN_POINT('Ctrl Pts',(20.8240267881588,18.8689175186693,-19.3104372340411));
#90634=CARTESIAN_POINT('Ctrl Pts',(20.84654308009,19.0357859231841,-19.2993132865357));
#90635=CARTESIAN_POINT('Ctrl Pts',(20.8527583948964,19.1446329813134,-19.2921187092348));
#90636=CARTESIAN_POINT('Ctrl Pts',(20.8490715742645,19.3283241096571,-19.2803152120503));
#90637=CARTESIAN_POINT('Ctrl Pts',(20.8436007149766,19.4030407929438,-19.2756058924345));
#90638=CARTESIAN_POINT('Ctrl Pts',(20.8318188154508,19.495952711619,-19.2698686362723));
#90639=CARTESIAN_POINT('Ctrl Pts',(20.8292078560918,19.5145554410462,-19.2687257719568));
#90640=CARTESIAN_POINT('Ctrl Pts',(20.8250486288661,19.54157182769,-19.2670740912115));
#90641=CARTESIAN_POINT('Ctrl Pts',(20.8236964789049,19.5500143521263,-19.2665590974263));
#90642=CARTESIAN_POINT('Ctrl Pts',(20.8212348510868,19.5648096380038,-19.2656585388559));
#90643=CARTESIAN_POINT('Ctrl Pts',(20.8201474306668,19.5711659096655,-19.2652722796448));
#90644=CARTESIAN_POINT('Ctrl Pts',(20.8179785384612,19.5835042332641,-19.2645236983071));
#90645=CARTESIAN_POINT('Ctrl Pts',(20.816900311501,19.5894867845792,-19.2641612772068));
#90646=CARTESIAN_POINT('Ctrl Pts',(20.8142595004653,19.6037862282353,-19.2632962914735));
#90647=CARTESIAN_POINT('Ctrl Pts',(20.8126727801019,19.6120985998363,-19.2627944988896));
#90648=CARTESIAN_POINT('Ctrl Pts',(20.8067569002731,19.6421119290861,-19.2609862281892));
#90649=CARTESIAN_POINT('Ctrl Pts',(20.8021373076979,19.6637546730658,-19.2596890037661));
#90650=CARTESIAN_POINT('Ctrl Pts',(20.7556427629015,19.8659941808761,-19.2476201577379));
#90651=CARTESIAN_POINT('Ctrl Pts',(20.6905580517034,20.0404235711714,-19.2377029326564));
#90652=CARTESIAN_POINT('Ctrl Pts',(20.5659209151493,20.275048167134,-19.2232204951948));
#90653=CARTESIAN_POINT('Ctrl Pts',(20.5242633268284,20.3437347209994,-19.2188064093679));
#90654=CARTESIAN_POINT('Ctrl Pts',(20.4583865313407,20.4396092966767,-19.2121527114519));
#90655=CARTESIAN_POINT('Ctrl Pts',(20.437207325325,20.4688052992242,-19.2100549776856));
#90656=CARTESIAN_POINT('Ctrl Pts',(20.4107559561063,20.5033754254829,-19.2074645382492));
#90657=CARTESIAN_POINT('Ctrl Pts',(20.4061863423335,20.5092825614914,-19.2070180379725));
#90658=CARTESIAN_POINT('Ctrl Pts',(20.3990230319104,20.5184420090598,-19.2063194544273));
#90659=CARTESIAN_POINT('Ctrl Pts',(20.3964507914676,20.5217111310702,-19.2060688701841));
#90660=CARTESIAN_POINT('Ctrl Pts',(20.3916557119651,20.5277684898818,-19.2056021893234));
#90661=CARTESIAN_POINT('Ctrl Pts',(20.3894354573937,20.5305586993971,-19.2053862764597));
#90662=CARTESIAN_POINT('Ctrl Pts',(20.3843911321713,20.5368651704445,-19.2048961283016));
#90663=CARTESIAN_POINT('Ctrl Pts',(20.3815628826702,20.5403780072367,-19.2046215956941));
#90664=CARTESIAN_POINT('Ctrl Pts',(20.3742318918431,20.54942416056,-19.2039107797717));
#90665=CARTESIAN_POINT('Ctrl Pts',(20.3697124091154,20.5549437502918,-19.2034733304858));
#90666=CARTESIAN_POINT('Ctrl Pts',(20.3417964580907,20.5886877606709,-19.2007765011327));
#90667=CARTESIAN_POINT('Ctrl Pts',(20.3176994848855,20.6163215236206,-19.1984709468753));
#90668=CARTESIAN_POINT('Ctrl Pts',(20.1774751337907,20.7689386467687,-19.185244461121));
#90669=CARTESIAN_POINT('Ctrl Pts',(20.0472910970754,20.8801503528965,-19.1737328748605));
#90670=CARTESIAN_POINT('Ctrl Pts',(19.82576354334,21.027267368159,-19.1564516786444));
#90671=CARTESIAN_POINT('Ctrl Pts',(19.7428804294575,21.0745823860423,-19.1503957560952));
#90672=CARTESIAN_POINT('Ctrl Pts',(19.6378355663715,21.1254783976778,-19.1432258873204));
#90673=CARTESIAN_POINT('Ctrl Pts',(19.618450936858,21.1345105560304,-19.1419224706049));
#90674=CARTESIAN_POINT('Ctrl Pts',(19.5907099067168,21.1469282756437,-19.1400843594447));
#90675=CARTESIAN_POINT('Ctrl Pts',(19.5824640980739,21.1505563489892,-19.1395413633423));
#90676=CARTESIAN_POINT('Ctrl Pts',(19.5682051620042,21.1567218037883,-19.1386081126469));
#90677=CARTESIAN_POINT('Ctrl Pts',(19.5622030468134,21.1592841950755,-19.1382170076031));
#90678=CARTESIAN_POINT('Ctrl Pts',(19.5506923942465,21.1641354571764,-19.1374702370996));
#90679=CARTESIAN_POINT('Ctrl Pts',(19.5451858531175,21.1664288771835,-19.137114419822));
#90680=CARTESIAN_POINT('Ctrl Pts',(19.5308511744754,21.1723281576335,-19.13619181492));
#90681=CARTESIAN_POINT('Ctrl Pts',(19.5220081726605,21.1758977226645,-19.135626259429));
#90682=CARTESIAN_POINT('Ctrl Pts',(19.4918209366287,21.1878465295343,-19.1337075895897));
#90683=CARTESIAN_POINT('Ctrl Pts',(19.4703643509266,21.1959388848163,-19.1323641064201));
#90684=CARTESIAN_POINT('Ctrl Pts',(19.2828328255767,21.2632069240264,-19.1207863792827));
#90685=CARTESIAN_POINT('Ctrl Pts',(19.1101028362507,21.3017711607132,-19.111311225342));
#90686=CARTESIAN_POINT('Ctrl Pts',(18.8485351998096,21.3266656020323,-19.0970128830124));
#90687=CARTESIAN_POINT('Ctrl Pts',(18.7620791686531,21.3295769870634,-19.0922794517899));
#90688=CARTESIAN_POINT('Ctrl Pts',(18.6380316834745,21.3261592573976,-19.0851932757912));
#90689=CARTESIAN_POINT('Ctrl Pts',(18.600405371339,21.3241163437425,-19.0830044483095));
#90690=CARTESIAN_POINT('Ctrl Pts',(18.5553176942743,21.3204593710859,-19.0803129943747));
#90691=CARTESIAN_POINT('Ctrl Pts',(18.5477825347966,21.3198075437039,-19.0798608844819));
#90692=CARTESIAN_POINT('Ctrl Pts',(18.536088244582,21.3187327661038,-19.0791554184968));
#90693=CARTESIAN_POINT('Ctrl Pts',(18.5319265135599,21.3183378423083,-19.0789036095811));
#90694=CARTESIAN_POINT('Ctrl Pts',(18.5242190331953,21.3175834062839,-19.0784358280959));
#90695=CARTESIAN_POINT('Ctrl Pts',(18.5206730117286,21.3172272662644,-19.0782200467525));
#90696=CARTESIAN_POINT('Ctrl Pts',(18.5126690199395,21.3164029756263,-19.0777317151874));
#90697=CARTESIAN_POINT('Ctrl Pts',(18.5082116527515,21.3159296220783,-19.0774588771022));
#90698=CARTESIAN_POINT('Ctrl Pts',(18.4950908913945,21.3144940975508,-19.0766531945077));
#90699=CARTESIAN_POINT('Ctrl Pts',(18.4864320204656,21.3134925850316,-19.0761182152909));
#90700=CARTESIAN_POINT('Ctrl Pts',(18.4248765576603,21.3059873631538,-19.0722929152636));
#90701=CARTESIAN_POINT('Ctrl Pts',(18.3722404125648,21.2975421926583,-19.0689057101185));
#90702=CARTESIAN_POINT('Ctrl Pts',(18.3023591118912,21.2836066042052,-19.0643005755572));
#90703=CARTESIAN_POINT('Ctrl Pts',(18.2847799797367,21.2798676467466,-19.06313281346));
#90704=CARTESIAN_POINT('Ctrl Pts',(18.2202261468215,21.265275966019,-19.0588147822249));
#90705=CARTESIAN_POINT('Ctrl Pts',(18.1735793185627,21.2530435215245,-19.055636509265));
#90706=CARTESIAN_POINT('Ctrl Pts',(18.0225990922783,21.2078879835835,-19.0452266626765));
#90707=CARTESIAN_POINT('Ctrl Pts',(17.9203845661018,21.1684693515016,-19.0379941040625));
#90708=CARTESIAN_POINT('Ctrl Pts',(17.7533800121832,21.0887114999822,-19.0260981524289));
#90709=CARTESIAN_POINT('Ctrl Pts',(17.6868830898271,21.0524571441374,-19.0213353713156));
#90710=CARTESIAN_POINT('Ctrl Pts',(17.6063835888865,21.0027944167638,-19.0155404392381));
#90711=CARTESIAN_POINT('Ctrl Pts',(17.5904361816114,20.9926587305555,-19.0143907453355));
#90712=CARTESIAN_POINT('Ctrl Pts',(17.5674553637061,20.977617123585,-19.0127310771272));
#90713=CARTESIAN_POINT('Ctrl Pts',(17.5603130238832,20.9728800570067,-19.012214841149));
#90714=CARTESIAN_POINT('Ctrl Pts',(17.5478447021397,20.9645011358771,-19.0113128492244));
#90715=CARTESIAN_POINT('Ctrl Pts',(17.5425062727328,20.9608780881755,-19.0109263920377));
#90716=CARTESIAN_POINT('Ctrl Pts',(17.5321751552666,20.9537974416274,-19.0101779623279));
#90717=CARTESIAN_POINT('Ctrl Pts',(17.5271806240426,20.9503426559933,-19.0098158883146));
#90718=CARTESIAN_POINT('Ctrl Pts',(17.515280773985,20.9420354345628,-19.0089525815475));
#90719=CARTESIAN_POINT('Ctrl Pts',(17.5083894362443,20.9371630794093,-19.0084521139712));
#90720=CARTESIAN_POINT('Ctrl Pts',(17.4836527635305,20.919450788915,-19.0066536159706));
#90721=CARTESIAN_POINT('Ctrl Pts',(17.4659781666797,20.9063739981265,-19.0053647071586));
#90722=CARTESIAN_POINT('Ctrl Pts',(17.3000937186315,20.7795964859562,-18.9932203634322));
#90723=CARTESIAN_POINT('Ctrl Pts',(17.1673457687471,20.6470301461303,-18.9832348352213));
#90724=CARTESIAN_POINT('Ctrl Pts',(17.005442473164,20.435775045624,-18.9687214714853));
#90725=CARTESIAN_POINT('Ctrl Pts',(16.9607585652638,20.3701366989198,-18.9643555312532));
#90726=CARTESIAN_POINT('Ctrl Pts',(16.9014073589746,20.2714602486633,-18.9577673299044));
#90727=CARTESIAN_POINT('Ctrl Pts',(16.8837304152689,20.2403074603536,-18.9556837525783));
#90728=CARTESIAN_POINT('Ctrl Pts',(16.8633406754344,20.2021499590242,-18.9531090196168));
#90729=CARTESIAN_POINT('Ctrl Pts',(16.8598628565168,20.1955580295374,-18.9526634172904));
#90730=CARTESIAN_POINT('Ctrl Pts',(16.8544998952484,20.1852615832054,-18.9519659357869));
#90731=CARTESIAN_POINT('Ctrl Pts',(16.8525906925139,20.1815695715885,-18.9517155479896));
#90732=CARTESIAN_POINT('Ctrl Pts',(16.8490636468279,20.1746994667743,-18.951249041803));
#90733=CARTESIAN_POINT('Ctrl Pts',(16.8474429569923,20.1715228995918,-18.9510331059631));
#90734=CARTESIAN_POINT('Ctrl Pts',(16.8437888032994,20.1643157986354,-18.9505426578842));
#90735=CARTESIAN_POINT('Ctrl Pts',(16.8417602110571,20.160282866341,-18.9502678467809));
#90736=CARTESIAN_POINT('Ctrl Pts',(16.8357860253825,20.1483106776904,-18.9494510231292));
#90737=CARTESIAN_POINT('Ctrl Pts',(16.831877445271,20.1403532054228,-18.9489067885678));
#90738=CARTESIAN_POINT('Ctrl Pts',(16.8031431866498,20.0809125291191,-18.9448329616298));
#90739=CARTESIAN_POINT('Ctrl Pts',(16.7803637992109,20.0284718308009,-18.9411920268991));
#90740=CARTESIAN_POINT('Ctrl Pts',(16.6996314188873,19.8198990120479,-18.9267029874953));
#90741=CARTESIAN_POINT('Ctrl Pts',(16.6580537897843,19.6580665212596,-18.9155001378934));
#90742=CARTESIAN_POINT('Ctrl Pts',(16.6280919355396,19.435161618524,-18.9010061673904));
#90743=CARTESIAN_POINT('Ctrl Pts',(16.6227108983252,19.3770015101593,-18.8973011305402));
#90744=CARTESIAN_POINT('Ctrl Pts',(16.617921324783,19.2829677512959,-18.8914414386409));
#90745=CARTESIAN_POINT('Ctrl Pts',(16.6170073710065,19.2472045679689,-18.8892429310058));
#90746=CARTESIAN_POINT('Ctrl Pts',(16.6169977968346,19.2004601970563,-18.8864068441664));
#90747=CARTESIAN_POINT('Ctrl Pts',(16.6170808697125,19.189486781312,-18.8857437475015));
#90748=CARTESIAN_POINT('Ctrl Pts',(16.617355670881,19.1715808612138,-18.8846659982215));
#90749=CARTESIAN_POINT('Ctrl Pts',(16.6174961452151,19.1646478807895,-18.8842497477679));
#90750=CARTESIAN_POINT('Ctrl Pts',(16.6178328488804,19.1512748012638,-18.8834488079317));
#90751=CARTESIAN_POINT('Ctrl Pts',(16.6180244184906,19.1448346713578,-18.883063977102));
#90752=CARTESIAN_POINT('Ctrl Pts',(16.6185373485299,19.1298874778342,-18.8821728055198));
#90753=CARTESIAN_POINT('Ctrl Pts',(16.6188806293354,19.1213812403198,-18.8816671568674));
#90754=CARTESIAN_POINT('Ctrl Pts',(16.620136566495,19.0943135080247,-18.8800627596263));
#90755=CARTESIAN_POINT('Ctrl Pts',(16.6212423368925,19.0757615346521,-18.8789700616719));
#90756=CARTESIAN_POINT('Ctrl Pts',(16.6243860730752,19.0325961609319,-18.8764423806009));
#90757=CARTESIAN_POINT('Ctrl Pts',(16.6266107500515,19.007998839698,-18.8750132004309));
#90758=CARTESIAN_POINT('Ctrl Pts',(16.6359173607672,18.9219186647825,-18.8700446062002));
#90759=CARTESIAN_POINT('Ctrl Pts',(16.6452642980639,18.8607103928403,-18.8665717730464));
#90760=CARTESIAN_POINT('Ctrl Pts',(16.678497031111,18.6927922113537,-18.857102765276));
#90761=CARTESIAN_POINT('Ctrl Pts',(16.7079721274187,18.5874456088998,-18.8512347675934));
#90762=CARTESIAN_POINT('Ctrl Pts',(16.7454194035981,18.4848896698064,-18.845275399947));
#90763=CARTESIAN_POINT('Origin',(18.734,19.211,0.));
#90764=CARTESIAN_POINT('',(16.7454193875989,18.4848897136231,-18.0457833433865));
#90765=CARTESIAN_POINT('',(16.7454194512262,18.4848895393686,-18.2676549287063));
#90766=CARTESIAN_POINT('',(16.7454194503191,18.4848895418526,0.));
#90767=CARTESIAN_POINT('',(16.6170000023184,19.2110990761722,-18.3109437209775));
#90768=CARTESIAN_POINT('Ctrl Pts',(16.7454194512262,18.4848895393686,-18.2676549287063));
#90769=CARTESIAN_POINT('Ctrl Pts',(16.7422625743728,18.493535199011,-18.2681689766162));
#90770=CARTESIAN_POINT('Ctrl Pts',(16.7391619133878,18.5022019024759,-18.2686817414929));
#90771=CARTESIAN_POINT('Ctrl Pts',(16.7026446946734,18.6064098304461,-18.2748185764456));
#90772=CARTESIAN_POINT('Ctrl Pts',(16.6760643065157,18.7042108460221,-18.2802824916259));
#90773=CARTESIAN_POINT('Ctrl Pts',(16.6332961709258,18.9222616774293,-18.292365115819));
#90774=CARTESIAN_POINT('Ctrl Pts',(16.62023343224,19.0427466454246,-18.2989795629078));
#90775=CARTESIAN_POINT('Ctrl Pts',(16.6172718865579,19.1751735243589,-18.3067857740772));
#90776=CARTESIAN_POINT('Ctrl Pts',(16.6171084113102,19.1866806408802,-18.3074685689643));
#90777=CARTESIAN_POINT('Ctrl Pts',(16.6170172097224,19.2017503970018,-18.3083692892897));
#90778=CARTESIAN_POINT('Ctrl Pts',(16.6170046428134,19.2053125820636,-18.3085826791177));
#90779=CARTESIAN_POINT('Ctrl Pts',(16.6170002820809,19.2096563900998,-18.3088434923776));
#90780=CARTESIAN_POINT('Ctrl Pts',(16.6169999302933,19.2104380262339,-18.3088904475228));
#90781=CARTESIAN_POINT('Ctrl Pts',(16.617000011396,19.2112196607865,-18.3089374264593));
#90782=CARTESIAN_POINT('Ctrl Pts',(16.6170000023184,19.2110990761722,-18.3109437209775));
#90783=CARTESIAN_POINT('Ctrl Pts',(16.6170002492315,19.2163749670546,-18.3112630160645));
#90784=CARTESIAN_POINT('Ctrl Pts',(16.6170202186042,19.2216508039048,-18.3115823111514));
#90785=CARTESIAN_POINT('Ctrl Pts',(16.6170599094811,19.2269264921969,-18.3119016062384));
#90786=CARTESIAN_POINT('Ctrl Pts',(16.6176053981758,19.2994325325996,-18.3162898151688));
#90787=CARTESIAN_POINT('Ctrl Pts',(16.6218813020779,19.3720520465351,-18.3206780240992));
#90788=CARTESIAN_POINT('Ctrl Pts',(16.6299021760198,19.4443695505458,-18.3250662330295));
#90789=CARTESIAN_POINT('Ctrl Pts',(16.6379111456549,19.5165797233901,-18.3294479291303));
#90790=CARTESIAN_POINT('Ctrl Pts',(16.6496539988947,19.588488300638,-18.333829625231));
#90791=CARTESIAN_POINT('Ctrl Pts',(16.6650932824124,19.6596802802897,-18.3382113213318));
#90792=CARTESIAN_POINT('Ctrl Pts',(16.6805144235432,19.7307886036996,-18.3425878685909));
#90793=CARTESIAN_POINT('Ctrl Pts',(16.6996232646346,19.8011815331899,-18.3469644158501));
#90794=CARTESIAN_POINT('Ctrl Pts',(16.7223308201356,19.8704513710532,-18.3513409631092));
#90795=CARTESIAN_POINT('Ctrl Pts',(16.745023974835,19.939677278992,-18.3557147348257));
#90796=CARTESIAN_POINT('Ctrl Pts',(16.7713111657671,20.0077810512476,-18.3600885065421));
#90797=CARTESIAN_POINT('Ctrl Pts',(16.8010531665407,20.0743687155669,-18.3644622782586));
#90798=CARTESIAN_POINT('Ctrl Pts',(16.8307861167235,20.1409361170363,-18.3688347190217));
#90799=CARTESIAN_POINT('Ctrl Pts',(16.8639715929647,20.20598788633,-18.3732071597847));
#90800=CARTESIAN_POINT('Ctrl Pts',(16.9004223233179,20.269150227318,-18.3775796005477));
#90801=CARTESIAN_POINT('Ctrl Pts',(16.9368739857203,20.332314183374,-18.3819521531146));
#90802=CARTESIAN_POINT('Ctrl Pts',(16.9765908251609,20.3935881984058,-18.3863247056814));
#90803=CARTESIAN_POINT('Ctrl Pts',(17.019340565139,20.452624751059,-18.3906972582483));
#90804=CARTESIAN_POINT('Ctrl Pts',(17.0621346724099,20.5117225740734,-18.3950743488151));
#90805=CARTESIAN_POINT('Ctrl Pts',(17.10796768121,20.5685779068979,-18.399451439382));
#90806=CARTESIAN_POINT('Ctrl Pts',(17.156565568357,20.6228745035828,-18.4038285299488));
#90807=CARTESIAN_POINT('Ctrl Pts',(17.205189996614,20.6772007536545,-18.4082080110073));
#90808=CARTESIAN_POINT('Ctrl Pts',(17.2565819695238,20.7289651427766,-18.4125874920657));
#90809=CARTESIAN_POINT('Ctrl Pts',(17.3104308762819,20.7778886208013,-18.4169669731242));
#90810=CARTESIAN_POINT('Ctrl Pts',(17.364375229866,20.8268988153625,-18.4213542167834));
#90811=CARTESIAN_POINT('Ctrl Pts',(17.4207848402039,20.8730577373945,-18.4257414604427));
#90812=CARTESIAN_POINT('Ctrl Pts',(17.4793168103114,20.9161272953985,-18.430128704102));
#90813=CARTESIAN_POINT('Ctrl Pts',(17.5191129099216,20.9454104447157,-18.4331116070413));
#90814=CARTESIAN_POINT('Ctrl Pts',(17.5598894741973,20.9732663668681,-18.4360945099806));
#90815=CARTESIAN_POINT('Ctrl Pts',(17.6015321394767,20.9996323112596,-18.4390774129199));
#90816=CARTESIAN_POINT('Ctrl Pts',(17.6627935078072,21.0384197860744,-18.4434656218502));
#90817=CARTESIAN_POINT('Ctrl Pts',(17.7261694924202,21.0741319931223,-18.4478538307805));
#90818=CARTESIAN_POINT('Ctrl Pts',(17.791318615734,21.1065318007774,-18.4522420397107));
#90819=CARTESIAN_POINT('Ctrl Pts',(17.8563710469468,21.1388835217458,-18.4566237358114));
#90820=CARTESIAN_POINT('Ctrl Pts',(17.9231909643681,21.1679323895269,-18.461005431912));
#90821=CARTESIAN_POINT('Ctrl Pts',(17.9914091442161,21.1934852637299,-18.4653871280127));
#90822=CARTESIAN_POINT('Ctrl Pts',(18.0595471622737,21.2190081112721,-18.4697636752717));
#90823=CARTESIAN_POINT('Ctrl Pts',(18.1290797293043,21.2410429575788,-18.4741402225307));
#90824=CARTESIAN_POINT('Ctrl Pts',(18.1996158698647,21.2594439463797,-18.4785167697897));
#90825=CARTESIAN_POINT('Ctrl Pts',(18.2701072774298,21.2778332655408,-18.482890541506));
#90826=CARTESIAN_POINT('Ctrl Pts',(18.3416005301136,21.2925931782368,-18.4872643132223));
#90827=CARTESIAN_POINT('Ctrl Pts',(18.4136889989941,21.3036275021213,-18.4916380849387));
#90828=CARTESIAN_POINT('Ctrl Pts',(18.4857555311113,21.314658468224,-18.4960105257016));
#90829=CARTESIAN_POINT('Ctrl Pts',(18.558416443296,21.3219660233356,-18.5003829664645));
#90830=CARTESIAN_POINT('Ctrl Pts',(18.6312560654046,21.3255053047708,-18.5047554072274));
#90831=CARTESIAN_POINT('Ctrl Pts',(18.7040975500302,21.3290446767058,-18.5091279597941));
#90832=CARTESIAN_POINT('Ctrl Pts',(18.7771172717461,21.3288155622467,-18.5135005123608));
#90833=CARTESIAN_POINT('Ctrl Pts',(18.8498972932253,21.3248251624538,-18.5178730649275));
#90834=CARTESIAN_POINT('Ctrl Pts',(18.922752848556,21.3208306212736,-18.5222501554941));
#90835=CARTESIAN_POINT('Ctrl Pts',(18.9953677242794,21.3130670274164,-18.5266272460608));
#90836=CARTESIAN_POINT('Ctrl Pts',(19.0673276840476,21.3015936130792,-18.5310043366275));
#90837=CARTESIAN_POINT('Ctrl Pts',(19.1393269438205,21.2901139326845,-18.5353838176858));
#90838=CARTESIAN_POINT('Ctrl Pts',(19.2106701033884,21.274920498468,-18.5397632987441));
#90839=CARTESIAN_POINT('Ctrl Pts',(19.2809543980001,21.2561234404085,-18.5441427798024));
#90840=CARTESIAN_POINT('Ctrl Pts',(19.3513632710524,21.2372930646897,-18.5485300234614));
#90841=CARTESIAN_POINT('Ctrl Pts',(19.4207090718549,21.2148464584352,-18.5529172671205));
#90842=CARTESIAN_POINT('Ctrl Pts',(19.4886059995023,21.1889430693312,-18.5573045107796));
#90843=CARTESIAN_POINT('Ctrl Pts',(19.5347693678655,21.1713312607487,-18.5602874137202));
#90844=CARTESIAN_POINT('Ctrl Pts',(19.5802633709739,21.1521225055481,-18.5632703166607));
#90845=CARTESIAN_POINT('Ctrl Pts',(19.624973342625,21.1313789997632,-18.5662532196012));
#90846=CARTESIAN_POINT('Ctrl Pts',(19.690747087515,21.1008628082464,-18.5706414285353));
#90847=CARTESIAN_POINT('Ctrl Pts',(19.7550796205674,21.0669039749609,-18.5750296374695));
#90848=CARTESIAN_POINT('Ctrl Pts',(19.8175867162729,21.0296612736617,-18.5794178464036));
#90849=CARTESIAN_POINT('Ctrl Pts',(19.8800010410847,20.9924738467062,-18.583799542508));
#90850=CARTESIAN_POINT('Ctrl Pts',(19.9405948958109,20.9520124717685,-18.5881812386125));
#90851=CARTESIAN_POINT('Ctrl Pts',(19.9990060261175,20.9084830643887,-18.592562934717));
#90852=CARTESIAN_POINT('Ctrl Pts',(20.0573485186974,20.8650048075267,-18.5969394819799));
#90853=CARTESIAN_POINT('Ctrl Pts',(20.113512997131,20.818465966753,-18.6013160292427));
#90854=CARTESIAN_POINT('Ctrl Pts',(20.1671651917848,20.7691163413097,-18.6056925765056));
#90855=CARTESIAN_POINT('Ctrl Pts',(20.2207833609965,20.7197980126817,-18.6100663482258));
#90856=CARTESIAN_POINT('Ctrl Pts',(20.2718920534931,20.6676727619683,-18.6144401199459));
#90857=CARTESIAN_POINT('Ctrl Pts',(20.3201902946191,20.6130304380634,-18.6188138916661));
#90858=CARTESIAN_POINT('Ctrl Pts',(20.368473838428,20.5584047420012,-18.6231863324329));
#90859=CARTESIAN_POINT('Ctrl Pts',(20.4139483094877,20.5012638546127,-18.6275587731996));
#90860=CARTESIAN_POINT('Ctrl Pts',(20.4563509910144,20.4419330053873,-18.6319312139664));
#90861=CARTESIAN_POINT('Ctrl Pts',(20.4987547567822,20.3826006390657,-18.6363037665369));
#90862=CARTESIAN_POINT('Ctrl Pts',(20.5380862982191,20.3210785933454,-18.6406763191075));
#90863=CARTESIAN_POINT('Ctrl Pts',(20.574125448729,20.2577221851762,-18.645048871678));
#90864=CARTESIAN_POINT('Ctrl Pts',(20.6102020020282,20.1943000233375,-18.6494259622485));
#90865=CARTESIAN_POINT('Ctrl Pts',(20.6429791031792,20.1290401182302,-18.6538030528189));
#90866=CARTESIAN_POINT('Ctrl Pts',(20.6722823388071,20.0623228383337,-18.6581801433894));
#90867=CARTESIAN_POINT('Ctrl Pts',(20.7016015780193,19.9955691216548,-18.6625596244515));
#90868=CARTESIAN_POINT('Ctrl Pts',(20.7274430033785,19.9273568969102,-18.6669391055136));
#90869=CARTESIAN_POINT('Ctrl Pts',(20.7496812078475,19.858084436786,-18.6713185865756));
#90870=CARTESIAN_POINT('Ctrl Pts',(20.7719588293842,19.7886891916923,-18.6757058302384));
#90871=CARTESIAN_POINT('Ctrl Pts',(20.7906203524689,19.7182304251234,-18.6800930739012));
#90872=CARTESIAN_POINT('Ctrl Pts',(20.8055910206596,19.6471188405955,-18.684480317564));
#90873=CARTESIAN_POINT('Ctrl Pts',(20.8157696323546,19.5987698159095,-18.6874632204702));
#90874=CARTESIAN_POINT('Ctrl Pts',(20.8242431499881,19.5501192245651,-18.6904461233765));
#90875=CARTESIAN_POINT('Ctrl Pts',(20.8310018039417,19.501297148221,-18.6934290262827));
#90876=CARTESIAN_POINT('Ctrl Pts',(20.8409445967655,19.4294740021259,-18.6978172352092));
#90877=CARTESIAN_POINT('Ctrl Pts',(20.8472125720512,19.3569992504144,-18.7022054441356));
#90878=CARTESIAN_POINT('Ctrl Pts',(20.8497312594192,19.2842819071557,-18.7065936530621));
#90879=CARTESIAN_POINT('Ctrl Pts',(20.8522462086376,19.211672488491,-18.7109753491589));
#90880=CARTESIAN_POINT('Ctrl Pts',(20.8510228997993,19.1388216711234,-18.7153570452558));
#90881=CARTESIAN_POINT('Ctrl Pts',(20.8460383938856,19.0661455117948,-18.7197387413526));
#90882=CARTESIAN_POINT('Ctrl Pts',(20.841059745163,18.9935547527367,-18.7241152886079));
#90883=CARTESIAN_POINT('Ctrl Pts',(20.8323287119819,18.9211387228713,-18.7284918358632));
#90884=CARTESIAN_POINT('Ctrl Pts',(20.8198744021603,18.8493137016523,-18.7328683831184));
#90885=CARTESIAN_POINT('Ctrl Pts',(20.8074279906809,18.7775342308174,-18.7372421548311));
#90886=CARTESIAN_POINT('Ctrl Pts',(20.7912630697938,18.7063454990751,-18.7416159265437));
#90887=CARTESIAN_POINT('Ctrl Pts',(20.7714604446762,18.6361574681881,-18.7459896982563));
#90888=CARTESIAN_POINT('Ctrl Pts',(20.7516638455637,18.5659907957541,-18.7503621390155));
#90889=CARTESIAN_POINT('Ctrl Pts',(20.7282318707929,18.4968246835911,-18.7547345797748));
#90890=CARTESIAN_POINT('Ctrl Pts',(20.7012957832832,18.4290560754913,-18.759107020534));
#90891=CARTESIAN_POINT('Ctrl Pts',(20.6743590070145,18.3612857345401,-18.7634795730971));
#90892=CARTESIAN_POINT('Ctrl Pts',(20.6439181201446,18.2949134161269,-18.7678521256601));
#90893=CARTESIAN_POINT('Ctrl Pts',(20.6101527159951,18.2303165718418,-18.7722246782232));
#90894=CARTESIAN_POINT('Ctrl Pts',(20.5763522688349,18.1656526865138,-18.7766017687863));
#90895=CARTESIAN_POINT('Ctrl Pts',(20.5392206395554,18.1027683827099,-18.7809788593495));
#90896=CARTESIAN_POINT('Ctrl Pts',(20.4989832512009,18.0420162007194,-18.7853559499126));
#90897=CARTESIAN_POINT('Ctrl Pts',(20.4587238877147,17.9812308397069,-18.7897354309674));
#90898=CARTESIAN_POINT('Ctrl Pts',(20.4153556750912,17.9225803070075,-18.7941149120222));
#90899=CARTESIAN_POINT('Ctrl Pts',(20.3691456171801,17.8663856275434,-18.798494393077));
#90900=CARTESIAN_POINT('Ctrl Pts',(20.3228536522502,17.8100913433856,-18.8028816367327));
#90901=CARTESIAN_POINT('Ctrl Pts',(20.2737101085662,17.7562619617535,-18.8072688803884));
#90902=CARTESIAN_POINT('Ctrl Pts',(20.2220198585452,17.7051826470069,-18.8116561240441));
#90903=CARTESIAN_POINT('Ctrl Pts',(20.1868754689052,17.6704536344897,-18.8146390270175));
#90904=CARTESIAN_POINT('Ctrl Pts',(20.1505545743004,17.6369951039851,-18.8176219299908));
#90905=CARTESIAN_POINT('Ctrl Pts',(20.1131612647178,17.6048856809361,-18.8206048329642));
#90906=CARTESIAN_POINT('Ctrl Pts',(20.0581512102737,17.5576488589,-18.8249930418924));
#90907=CARTESIAN_POINT('Ctrl Pts',(20.0006041495888,17.5131492751,-18.8293812508206));
#90908=CARTESIAN_POINT('Ctrl Pts',(19.9408236893632,17.4716709388986,-18.8337694597489));
#90909=CARTESIAN_POINT('Ctrl Pts',(19.8811319532531,17.4302541634259,-18.8381511558474));
#90910=CARTESIAN_POINT('Ctrl Pts',(19.8192137908503,17.3918500068481,-18.842532851946));
#90911=CARTESIAN_POINT('Ctrl Pts',(19.7554066235765,17.3567029608733,-18.8469145480445));
#90912=CARTESIAN_POINT('Ctrl Pts',(19.6916744348034,17.3215972154753,-18.8512910953013));
#90913=CARTESIAN_POINT('Ctrl Pts',(19.6260580710909,17.2897412091782,-18.8556676425582));
#90914=CARTESIAN_POINT('Ctrl Pts',(19.5589233130916,17.2613357910866,-18.860044189815));
#90915=CARTESIAN_POINT('Ctrl Pts',(19.4918311309807,17.2329483872986,-18.8644179615291));
#90916=CARTESIAN_POINT('Ctrl Pts',(19.4232229083437,17.2080074173232,-18.8687917332433));
#90917=CARTESIAN_POINT('Ctrl Pts',(19.353487096455,17.1866668413214,-18.8731655049574));
#90918=CARTESIAN_POINT('Ctrl Pts',(19.2837725054087,17.1653327593287,-18.8775379457181));
#90919=CARTESIAN_POINT('Ctrl Pts',(19.2129314673135,17.1475970372528,-18.8819103864788));
#90920=CARTESIAN_POINT('Ctrl Pts',(19.1413687992098,17.1335641618981,-18.8862828272394));
#90921=CARTESIAN_POINT('Ctrl Pts',(19.0698043012414,17.1195309277212,-18.8906553798039));
#90922=CARTESIAN_POINT('Ctrl Pts',(18.9975186103768,17.1092008191083,-18.8950279323683));
#90923=CARTESIAN_POINT('Ctrl Pts',(18.9249263141292,17.1026271338843,-18.8994004849327));
#90924=CARTESIAN_POINT('Ctrl Pts',(18.8522586788588,17.0960466262418,-18.9037775754971));
#90925=CARTESIAN_POINT('Ctrl Pts',(18.7792842843242,17.093230369319,-18.9081546660615));
#90926=CARTESIAN_POINT('Ctrl Pts',(18.7064215783365,17.0941796413823,-18.9125317566259));
#90927=CARTESIAN_POINT('Ctrl Pts',(18.6335190793211,17.0951294318782,-18.9169112376818));
#90928=CARTESIAN_POINT('Ctrl Pts',(18.5607288719984,17.0998488145903,-18.9212907187378));
#90929=CARTESIAN_POINT('Ctrl Pts',(18.4884654116445,17.1082870462374,-18.9256701997938));
#90930=CARTESIAN_POINT('Ctrl Pts',(18.4160738647923,17.1167402345934,-18.9300574434505));
#90931=CARTESIAN_POINT('Ctrl Pts',(18.3442114053892,17.1289253543984,-18.9344446871073));
#90932=CARTESIAN_POINT('Ctrl Pts',(18.2732828331912,17.1447404102563,-18.938831930764));
#90933=CARTESIAN_POINT('Ctrl Pts',(18.2250582383096,17.1554931244045,-18.9418148337245));
#90934=CARTESIAN_POINT('Ctrl Pts',(18.1772650979153,17.1679227808449,-18.9447977366851));
#90935=CARTESIAN_POINT('Ctrl Pts',(18.1300258654972,17.1819844148327,-18.9477806396456));
#90936=CARTESIAN_POINT('Ctrl Pts',(18.0605280442512,17.2026717307626,-18.9521690525416));
#90937=CARTESIAN_POINT('Ctrl Pts',(17.9919586602192,17.2269742190354,-18.9565574654377));
#90938=CARTESIAN_POINT('Ctrl Pts',(17.9247209128519,17.2547903079923,-18.9609458783337));
#90939=CARTESIAN_POINT('Ctrl Pts',(17.8574469481214,17.2826213799824,-18.9653366550321));
#90940=CARTESIAN_POINT('Ctrl Pts',(17.7915065313946,17.3139697419478,-18.9697274317305));
#90941=CARTESIAN_POINT('Ctrl Pts',(17.7272902810914,17.3486830178901,-18.9741182084289));
#90942=CARTESIAN_POINT('Ctrl Pts',(17.6632831696942,17.3832832399478,-18.9784946852852));
#90943=CARTESIAN_POINT('Ctrl Pts',(17.6009894540069,17.4212262970143,-18.9828711621416));
#90944=CARTESIAN_POINT('Ctrl Pts',(17.5407759394806,17.4623132523526,-18.987247638998));
#90945=CARTESIAN_POINT('Ctrl Pts',(17.4806016975384,17.5033734098712,-18.9916212614194));
#90946=CARTESIAN_POINT('Ctrl Pts',(17.4225053615492,17.5475731249768,-18.9959948838409));
#90947=CARTESIAN_POINT('Ctrl Pts',(17.3668265524039,17.5946690424953,-19.0003685062624));
#90948=CARTESIAN_POINT('Ctrl Pts',(17.3111656907014,17.6417497791703,-19.0047407188955));
#90949=CARTESIAN_POINT('Ctrl Pts',(17.2579211760136,17.691724552697,-19.0091129315286));
#90950=CARTESIAN_POINT('Ctrl Pts',(17.2073998648577,17.7443094984342,-19.0134851441618));
#90951=CARTESIAN_POINT('Ctrl Pts',(17.1565195530969,17.7972681088071,-19.0178884254062));
#90952=CARTESIAN_POINT('Ctrl Pts',(17.1084016692992,17.8528738026132,-19.0222917066506));
#90953=CARTESIAN_POINT('Ctrl Pts',(17.0633209239241,17.9107998520373,-19.0266949878951));
#90954=CARTESIAN_POINT('Ctrl Pts',(17.0185206472328,17.9683655160528,-19.0310708742399));
#90955=CARTESIAN_POINT('Ctrl Pts',(16.9767200693617,18.0282223204899,-19.0354467605847));
#90956=CARTESIAN_POINT('Ctrl Pts',(16.9381461792585,18.0900191551467,-19.0398226469295));
#90957=CARTESIAN_POINT('Ctrl Pts',(16.8992100558504,18.1523963012936,-19.0442396256237));
#90958=CARTESIAN_POINT('Ctrl Pts',(16.8635617990236,18.2167496759085,-19.048656604318));
#90959=CARTESIAN_POINT('Ctrl Pts',(16.8313871440048,18.2826933048815,-19.0530735830123));
#90960=CARTESIAN_POINT('Ctrl Pts',(16.799212488986,18.3486369338544,-19.0574905617065));
#90961=CARTESIAN_POINT('Ctrl Pts',(16.7705115861154,18.4161703371716,-19.0619075404008));
#90962=CARTESIAN_POINT('Ctrl Pts',(16.7454194503191,18.4848895418526,-19.066324519095));
#90963=CARTESIAN_POINT('',(16.6170009086255,19.2090541496144,-18.089014757963));
#90964=CARTESIAN_POINT('Ctrl Pts',(16.7454194035981,18.4848896698064,-18.845275399947));
#90965=CARTESIAN_POINT('Ctrl Pts',(16.7566881830226,18.4540281392966,-18.8434820839473));
#90966=CARTESIAN_POINT('Ctrl Pts',(16.7686788833216,18.4234193640937,-18.8416796887102));
#90967=CARTESIAN_POINT('Ctrl Pts',(16.8104693873181,18.3236520192083,-18.8356907737385));
#90968=CARTESIAN_POINT('Ctrl Pts',(16.8432351033399,18.2558235694364,-18.8314361934986));
#90969=CARTESIAN_POINT('Ctrl Pts',(16.8841144410632,18.1815815125323,-18.826413132321));
#90970=CARTESIAN_POINT('Ctrl Pts',(16.8887460985814,18.1733020501008,-18.8258476348406));
#90971=CARTESIAN_POINT('Ctrl Pts',(16.8956954523512,18.1610731661099,-18.8250040399154));
#90972=CARTESIAN_POINT('Ctrl Pts',(16.8979706398703,18.1570995520131,-18.8247286083055));
#90973=CARTESIAN_POINT('Ctrl Pts',(16.9020434466171,18.1500396127087,-18.8242368429802));
#90974=CARTESIAN_POINT('Ctrl Pts',(16.9038360024033,18.1469504247672,-18.8240208375938));
#90975=CARTESIAN_POINT('Ctrl Pts',(16.9077088758036,18.1403148765687,-18.8235550653782));
#90976=CARTESIAN_POINT('Ctrl Pts',(16.9097916788551,18.136770087804,-18.823305142465));
#90977=CARTESIAN_POINT('Ctrl Pts',(16.9155744855488,18.1269934619521,-18.8226128477397));
#90978=CARTESIAN_POINT('Ctrl Pts',(16.919296144699,18.1207745920248,-18.8221691015424));
#90979=CARTESIAN_POINT('Ctrl Pts',(16.9399459720041,18.0866675486583,-18.8197172761966));
#90980=CARTESIAN_POINT('Ctrl Pts',(16.9574841398768,18.0591560678372,-18.8176726580399));
#90981=CARTESIAN_POINT('Ctrl Pts',(17.0662168418627,17.8969844598258,-18.8052647618544));
#90982=CARTESIAN_POINT('Ctrl Pts',(17.1720442315182,17.7727956955694,-18.7943129863953));
#90983=CARTESIAN_POINT('Ctrl Pts',(17.3764984354523,17.5823449080279,-18.7760619164364));
#90984=CARTESIAN_POINT('Ctrl Pts',(17.4684037333815,17.5099409776383,-18.7686228012944));
#90985=CARTESIAN_POINT('Ctrl Pts',(17.5777443465653,17.4375947898247,-18.7606173499102));
#90986=CARTESIAN_POINT('Ctrl Pts',(17.5897407310793,17.4298307444879,-18.7597493950153));
#90987=CARTESIAN_POINT('Ctrl Pts',(17.6089588054833,17.4176671285735,-18.7583751135059));
#90988=CARTESIAN_POINT('Ctrl Pts',(17.6161296709314,17.4131884393169,-18.7578658590025));
#90989=CARTESIAN_POINT('Ctrl Pts',(17.6288239835789,17.4053653022492,-18.7569704879953));
#90990=CARTESIAN_POINT('Ctrl Pts',(17.6343362262791,17.4020029642941,-18.756583715397));
#90991=CARTESIAN_POINT('Ctrl Pts',(17.6457691779616,17.39510070166,-18.7557856453885));
#90992=CARTESIAN_POINT('Ctrl Pts',(17.6516919855537,17.3915643876897,-18.755374483376));
#90993=CARTESIAN_POINT('Ctrl Pts',(17.6669394831441,17.3825614081306,-18.7543217606395));
#90994=CARTESIAN_POINT('Ctrl Pts',(17.6762890195859,17.3771370500115,-18.7536817412918));
#90995=CARTESIAN_POINT('Ctrl Pts',(17.7154849431519,17.3547960700698,-18.7510209731451));
#90996=CARTESIAN_POINT('Ctrl Pts',(17.7456997529865,17.338534040658,-18.7490237554065));
#90997=CARTESIAN_POINT('Ctrl Pts',(17.8254447535955,17.2980825135208,-18.7438793946618));
#90998=CARTESIAN_POINT('Ctrl Pts',(17.8755486541995,17.2750795785363,-18.7407716463391));
#90999=CARTESIAN_POINT('Ctrl Pts',(18.0275779364744,17.2123469195417,-18.7316269055718));
#91000=CARTESIAN_POINT('Ctrl Pts',(18.1317423635202,17.1785303469814,-18.725738641419));
#91001=CARTESIAN_POINT('Ctrl Pts',(18.2827853535169,17.1421327834214,-18.7172798205953));
#91002=CARTESIAN_POINT('Ctrl Pts',(18.3278564274958,17.1328148848208,-18.7147638427559));
#91003=CARTESIAN_POINT('Ctrl Pts',(18.3949976345574,17.1212019179944,-18.7109848787414));
#91004=CARTESIAN_POINT('Ctrl Pts',(18.4168586877139,17.1177728341217,-18.7097496032274));
#91005=CARTESIAN_POINT('Ctrl Pts',(18.4897488817082,17.1075074530004,-18.7056034016135));
#91006=CARTESIAN_POINT('Ctrl Pts',(18.540969426111,17.1021904362632,-18.7026453026566));
#91007=CARTESIAN_POINT('Ctrl Pts',(18.6009481557041,17.0981675772804,-18.6990774111751));
#91008=CARTESIAN_POINT('Ctrl Pts',(18.6095715108376,17.0976422013584,-18.6985619379131));
#91009=CARTESIAN_POINT('Ctrl Pts',(18.6226567822962,17.0969253487159,-18.6977756241765));
#91010=CARTESIAN_POINT('Ctrl Pts',(18.6271166064366,17.0966951774471,-18.6975069005307));
#91011=CARTESIAN_POINT('Ctrl Pts',(18.6351357887352,17.0963067452077,-18.6970223518697));
#91012=CARTESIAN_POINT('Ctrl Pts',(18.638694844033,17.0961433568516,-18.6968068170462));
#91013=CARTESIAN_POINT('Ctrl Pts',(18.6464438407427,17.095807218253,-18.6963364777056));
#91014=CARTESIAN_POINT('Ctrl Pts',(18.650633834557,17.0956379348362,-18.6960814870096));
#91015=CARTESIAN_POINT('Ctrl Pts',(18.6624421710708,17.0951959942018,-18.6953610274601));
#91016=CARTESIAN_POINT('Ctrl Pts',(18.6700614327788,17.094952039911,-18.6948939986445));
#91017=CARTESIAN_POINT('Ctrl Pts',(18.7164071794245,17.0937186732507,-18.6920407672182));
#91018=CARTESIAN_POINT('Ctrl Pts',(18.755150903648,17.093751331285,-18.6896028560475));
#91019=CARTESIAN_POINT('Ctrl Pts',(18.8845130638409,17.0974111677222,-18.6813339627653));
#91020=CARTESIAN_POINT('Ctrl Pts',(18.9748933270239,17.1057968420952,-18.67534911149));
#91021=CARTESIAN_POINT('Ctrl Pts',(19.1307468895404,17.1304265747517,-18.6649221045853));
#91022=CARTESIAN_POINT('Ctrl Pts',(19.1965088103256,17.1440505528089,-18.6604877009276));
#91023=CARTESIAN_POINT('Ctrl Pts',(19.3726486786,17.1893706001045,-18.6486167278986));
#91024=CARTESIAN_POINT('Ctrl Pts',(19.481287923539,17.2269572220288,-18.6413129003393));
#91025=CARTESIAN_POINT('Ctrl Pts',(19.5994120482589,17.2789145167974,-18.6334336657141));
#91026=CARTESIAN_POINT('Ctrl Pts',(19.6124064104446,17.2847875191501,-18.6325675392087));
#91027=CARTESIAN_POINT('Ctrl Pts',(19.6330013950945,17.2943474954566,-18.6311955965458));
#91028=CARTESIAN_POINT('Ctrl Pts',(19.640640830007,17.2979493628897,-18.6306868679841));
#91029=CARTESIAN_POINT('Ctrl Pts',(19.6540808673365,17.3043847088726,-18.6297921085585));
#91030=CARTESIAN_POINT('Ctrl Pts',(19.6598904095673,17.3071991643812,-18.6294054244209));
#91031=CARTESIAN_POINT('Ctrl Pts',(19.6718843364299,17.313077555936,-18.6286072367332));
#91032=CARTESIAN_POINT('Ctrl Pts',(19.678066800152,17.3161452533802,-18.6281958700613));
#91033=CARTESIAN_POINT('Ctrl Pts',(19.6939073006405,17.324101976521,-18.6271420010573));
#91034=CARTESIAN_POINT('Ctrl Pts',(19.7035431164003,17.3290349820306,-18.6265010466964));
#91035=CARTESIAN_POINT('Ctrl Pts',(19.7436812177253,17.3499735686956,-18.623831174993));
#91036=CARTESIAN_POINT('Ctrl Pts',(19.7738294074527,17.3666490188161,-18.6218259947229));
#91037=CARTESIAN_POINT('Ctrl Pts',(19.8513829707901,17.4120515948756,-18.6166564679669));
#91038=CARTESIAN_POINT('Ctrl Pts',(19.8980917604375,17.4419180076304,-18.6135320235719));
#91039=CARTESIAN_POINT('Ctrl Pts',(20.0335299735626,17.5362092235255,-18.6043581671796));
#91040=CARTESIAN_POINT('Ctrl Pts',(20.1184856894494,17.605726650619,-18.5984573831293));
#91041=CARTESIAN_POINT('Ctrl Pts',(20.2426990019465,17.724595024294,-18.5890955501464));
#91042=CARTESIAN_POINT('Ctrl Pts',(20.2857954782948,17.7696456064384,-18.5856824922175));
#91043=CARTESIAN_POINT('Ctrl Pts',(20.3639009019544,17.8588618271416,-18.5790298687353));
#91044=CARTESIAN_POINT('Ctrl Pts',(20.3992560780308,17.9026515729959,-18.575808071606));
#91045=CARTESIAN_POINT('Ctrl Pts',(20.4380924508417,17.9548806059924,-18.5719465658339));
#91046=CARTESIAN_POINT('Ctrl Pts',(20.4433182616942,17.962001166088,-18.5714197209636));
#91047=CARTESIAN_POINT('Ctrl Pts',(20.4511432900531,17.9728044429518,-18.570619458093));
#91048=CARTESIAN_POINT('Ctrl Pts',(20.4537756290325,17.9764632038733,-18.5703482711729));
#91049=CARTESIAN_POINT('Ctrl Pts',(20.4584693839771,17.9830313287334,-18.5698611007104));
#91050=CARTESIAN_POINT('Ctrl Pts',(20.4605351512207,17.9859375178354,-18.5696454213967));
#91051=CARTESIAN_POINT('Ctrl Pts',(20.4649961534025,17.9922470977984,-18.5691768874961));
#91052=CARTESIAN_POINT('Ctrl Pts',(20.4673886651485,17.9956522906735,-18.5689238582866));
#91053=CARTESIAN_POINT('Ctrl Pts',(20.4740515898102,18.0051951350547,-18.5682143419966));
#91054=CARTESIAN_POINT('Ctrl Pts',(20.4782995001,18.0113483182008,-18.5677563683124));
#91055=CARTESIAN_POINT('Ctrl Pts',(20.5029285736885,18.047431396272,-18.5650685681975));
#91056=CARTESIAN_POINT('Ctrl Pts',(20.522570426062,18.0778558510498,-18.5627936143927));
#91057=CARTESIAN_POINT('Ctrl Pts',(20.583496333549,18.1777609938561,-18.5553330598593));
#91058=CARTESIAN_POINT('Ctrl Pts',(20.6215838303243,18.2491033956708,-18.5500225781887));
#91059=CARTESIAN_POINT('Ctrl Pts',(20.7329514957758,18.4899350182144,-18.5325029595728));
#91060=CARTESIAN_POINT('Ctrl Pts',(20.7881899597197,18.6668744858624,-18.5203483062317));
#91061=CARTESIAN_POINT('Ctrl Pts',(20.8235784259158,18.8706410055578,-18.507628182563));
#91062=CARTESIAN_POINT('Ctrl Pts',(20.8270341684287,18.8925816086989,-18.5062730814037));
#91063=CARTESIAN_POINT('Ctrl Pts',(20.8313307834177,18.9229645714145,-18.5044159762503));
#91064=CARTESIAN_POINT('Ctrl Pts',(20.8324670642412,18.9313630804871,-18.5039046706352));
#91065=CARTESIAN_POINT('Ctrl Pts',(20.8343321484691,18.9458003411262,-18.5030291602133));
#91066=CARTESIAN_POINT('Ctrl Pts',(20.8350854099578,18.951835777502,-18.5026641865368));
#91067=CARTESIAN_POINT('Ctrl Pts',(20.8365834896951,18.9642749905758,-18.5019140543185));
#91068=CARTESIAN_POINT('Ctrl Pts',(20.8373250881334,18.9706790969109,-18.50152900107));
#91069=CARTESIAN_POINT('Ctrl Pts',(20.8389809017083,18.9855730402773,-18.5006360881155));
#91070=CARTESIAN_POINT('Ctrl Pts',(20.8398730331237,18.9940652578583,-18.5001289291483));
#91071=CARTESIAN_POINT('Ctrl Pts',(20.8425572315496,19.0211949452107,-18.4985148279229));
#91072=CARTESIAN_POINT('Ctrl Pts',(20.8441534739472,19.0398512130638,-18.4974140417935));
#91073=CARTESIAN_POINT('Ctrl Pts',(20.8472975665005,19.083391662572,-18.4948648992895));
#91074=CARTESIAN_POINT('Ctrl Pts',(20.8486537855435,19.1082871331505,-18.4934224851758));
#91075=CARTESIAN_POINT('Ctrl Pts',(20.8518757160796,19.1959009129661,-18.4883928072077));
#91076=CARTESIAN_POINT('Ctrl Pts',(20.8513931000354,19.2586747564463,-18.4848740335015));
#91077=CARTESIAN_POINT('Ctrl Pts',(20.8428731269474,19.4219205109642,-18.4758368461326));
#91078=CARTESIAN_POINT('Ctrl Pts',(20.8304524778499,19.5219996806492,-18.4704131036395));
#91079=CARTESIAN_POINT('Ctrl Pts',(20.7965173619992,19.6939835194408,-18.4608625762637));
#91080=CARTESIAN_POINT('Ctrl Pts',(20.7782248413561,19.7663325714297,-18.4567690575104));
#91081=CARTESIAN_POINT('Ctrl Pts',(20.7435199126226,19.8783389424115,-18.4501111135294));
#91082=CARTESIAN_POINT('Ctrl Pts',(20.7296550730301,19.9187229813976,-18.4476423442679));
#91083=CARTESIAN_POINT('Ctrl Pts',(20.7119408020859,19.9656489483421,-18.4446626154238));
#91084=CARTESIAN_POINT('Ctrl Pts',(20.7092644717072,19.9726266243162,-18.4442166127946));
#91085=CARTESIAN_POINT('Ctrl Pts',(20.7048766172369,19.9838878553132,-18.4434918385372));
#91086=CARTESIAN_POINT('Ctrl Pts',(20.7031879132138,19.9881803129204,-18.4432144014202));
#91087=CARTESIAN_POINT('Ctrl Pts',(20.7001655341565,19.9957896998859,-18.4427204347069));
#91088=CARTESIAN_POINT('Ctrl Pts',(20.6988374718782,19.9991088057131,-18.4425042448034));
#91089=CARTESIAN_POINT('Ctrl Pts',(20.6959721824199,20.0062175041717,-18.44203963896));
#91090=CARTESIAN_POINT('Ctrl Pts',(20.6944324032671,20.0100059543564,-18.4417910751516));
#91091=CARTESIAN_POINT('Ctrl Pts',(20.6901712154596,20.020403647306,-18.4411062777548));
#91092=CARTESIAN_POINT('Ctrl Pts',(20.6874273255032,20.0270035349698,-18.4406687174152));
#91093=CARTESIAN_POINT('Ctrl Pts',(20.6725294157162,20.0623317475899,-18.4383114919446));
#91094=CARTESIAN_POINT('Ctrl Pts',(20.6597756524679,20.0908010782994,-18.4363584675208));
#91095=CARTESIAN_POINT('Ctrl Pts',(20.5761200194105,20.266998272962,-18.4239802077525));
#91096=CARTESIAN_POINT('Ctrl Pts',(20.4888965915849,20.4063561070953,-18.4129429647892));
#91097=CARTESIAN_POINT('Ctrl Pts',(20.3132404425781,20.6257141076328,-18.3945844643212));
#91098=CARTESIAN_POINT('Ctrl Pts',(20.2325308660873,20.7109431651765,-18.3871201421978));
#91099=CARTESIAN_POINT('Ctrl Pts',(20.1345138028437,20.7985939041118,-18.379091234928));
#91100=CARTESIAN_POINT('Ctrl Pts',(20.1237623200426,20.808014096948,-18.3782229768817));
#91101=CARTESIAN_POINT('Ctrl Pts',(20.1064999679573,20.8228326027197,-18.3768483076294));
#91102=CARTESIAN_POINT('Ctrl Pts',(20.1000508823782,20.8283019171533,-18.3763389659636));
#91103=CARTESIAN_POINT('Ctrl Pts',(20.0886197264919,20.8378792483207,-18.3754434935676));
#91104=CARTESIAN_POINT('Ctrl Pts',(20.0836513391528,20.8420033587254,-18.3750567062754));
#91105=CARTESIAN_POINT('Ctrl Pts',(20.073336690675,20.8504858354867,-18.3742586555995));
#91106=CARTESIAN_POINT('Ctrl Pts',(20.0679878359118,20.8548409385097,-18.3738475273687));
#91107=CARTESIAN_POINT('Ctrl Pts',(20.054204685956,20.8659517699852,-18.3727949938832));
#91108=CARTESIAN_POINT('Ctrl Pts',(20.0457397103835,20.8726692548624,-18.3721551289169));
#91109=CARTESIAN_POINT('Ctrl Pts',(20.0102059305757,20.9004267658756,-18.3694958609134));
#91110=CARTESIAN_POINT('Ctrl Pts',(19.9826785877602,20.9208731985757,-18.3674999550833));
#91111=CARTESIAN_POINT('Ctrl Pts',(19.9096820194307,20.9723892641537,-18.3623597366743));
#91112=CARTESIAN_POINT('Ctrl Pts',(19.8634751073856,21.0023701394384,-18.359254735634));
#91113=CARTESIAN_POINT('Ctrl Pts',(19.7278399868876,21.0830384852254,-18.3504795520042));
#91114=CARTESIAN_POINT('Ctrl Pts',(19.6358217887229,21.129062674551,-18.3449342414303));
#91115=CARTESIAN_POINT('Ctrl Pts',(19.4803921384489,21.193135339703,-18.3357919712046));
#91116=CARTESIAN_POINT('Ctrl Pts',(19.4188406381593,21.2152340843411,-18.3322230005182));
#91117=CARTESIAN_POINT('Ctrl Pts',(19.2986467218889,21.2522031027207,-18.3251903183212));
#91118=CARTESIAN_POINT('Ctrl Pts',(19.2401969974864,21.2674773773786,-18.3217422066224));
#91119=CARTESIAN_POINT('Ctrl Pts',(19.1724050180915,21.2821278683357,-18.3176284693294));
#91120=CARTESIAN_POINT('Ctrl Pts',(19.1636176693573,21.283968465418,-18.3170930492486));
#91121=CARTESIAN_POINT('Ctrl Pts',(19.1503712301684,21.2866552208166,-18.3162822813292));
#91122=CARTESIAN_POINT('Ctrl Pts',(19.1459205631155,21.287543051761,-18.3160092525769));
#91123=CARTESIAN_POINT('Ctrl Pts',(19.137965754997,21.2891033179351,-18.3155200996695));
#91124=CARTESIAN_POINT('Ctrl Pts',(19.1344627376407,21.2897812118468,-18.3153042902113));
#91125=CARTESIAN_POINT('Ctrl Pts',(19.1268921650512,21.291226401109,-18.3148370061301));
#91126=CARTESIAN_POINT('Ctrl Pts',(19.1228241255658,21.2919906131287,-18.3145853651313));
#91127=CARTESIAN_POINT('Ctrl Pts',(19.1115024688403,21.2940831153999,-18.3138835608291));
#91128=CARTESIAN_POINT('Ctrl Pts',(19.1042441950608,21.2953854278869,-18.3134319616598));
#91129=CARTESIAN_POINT('Ctrl Pts',(19.0640941151047,21.3023730111874,-18.3109251948959));
#91130=CARTESIAN_POINT('Ctrl Pts',(19.0310801517453,21.3073173164746,-18.308831837261));
#91131=CARTESIAN_POINT('Ctrl Pts',(18.8373274374331,21.3316660523057,-18.2964121022734));
#91132=CARTESIAN_POINT('Ctrl Pts',(18.6749084259211,21.3333593728565,-18.2855110039595));
#91133=CARTESIAN_POINT('Ctrl Pts',(18.3979808907166,21.3044088446963,-18.2673255427473));
#91134=CARTESIAN_POINT('Ctrl Pts',(18.2832615100843,21.2827412966339,-18.2599031283738));
#91135=CARTESIAN_POINT('Ctrl Pts',(18.1571215317626,21.247935028918,-18.2519132285541));
#91136=CARTESIAN_POINT('Ctrl Pts',(18.1433891043865,21.24399578574,-18.2510454814046));
#91137=CARTESIAN_POINT('Ctrl Pts',(18.1215956219463,21.2375047096665,-18.2496714656165));
#91138=CARTESIAN_POINT('Ctrl Pts',(18.1135083461791,21.2350431248708,-18.2491622708503));
#91139=CARTESIAN_POINT('Ctrl Pts',(18.0992705579791,21.2306161076688,-18.2482669693244));
#91140=CARTESIAN_POINT('Ctrl Pts',(18.0931139268971,21.228670867525,-18.2478802067905));
#91141=CARTESIAN_POINT('Ctrl Pts',(18.0803978493686,21.2245890389854,-18.2470821235026));
#91142=CARTESIAN_POINT('Ctrl Pts',(18.0738397470212,21.2224484908521,-18.2466709383143));
#91143=CARTESIAN_POINT('Ctrl Pts',(18.0570316228513,21.2168713035411,-18.2456180857522));
#91144=CARTESIAN_POINT('Ctrl Pts',(18.046797169997,21.2133881109883,-18.2449779605012));
#91145=CARTESIAN_POINT('Ctrl Pts',(18.0047966138133,21.1987337032221,-18.2423544822049));
#91146=CARTESIAN_POINT('Ctrl Pts',(17.973271515087,21.1868834003443,-18.2403936947547));
#91147=CARTESIAN_POINT('Ctrl Pts',(17.8919727815959,21.1540887572778,-18.2353480330195));
#91148=CARTESIAN_POINT('Ctrl Pts',(17.8426930477131,21.1319831557131,-18.2323009089659));
#91149=CARTESIAN_POINT('Ctrl Pts',(17.6803078053599,21.0515453373463,-18.2222154748355));
#91150=CARTESIAN_POINT('Ctrl Pts',(17.5716302879619,20.9849141487426,-18.2154056689656));
#91151=CARTESIAN_POINT('Ctrl Pts',(17.3877165111387,20.8479577562523,-18.2028664177071));
#91152=CARTESIAN_POINT('Ctrl Pts',(17.3103691858698,20.7811527490037,-18.1971988929064));
#91153=CARTESIAN_POINT('Ctrl Pts',(17.2312944836335,20.7021938329868,-18.1905785134173));
#91154=CARTESIAN_POINT('Ctrl Pts',(17.2244841048952,20.6952993871924,-18.1900010124083));
#91155=CARTESIAN_POINT('Ctrl Pts',(17.2144982268534,20.6850504381913,-18.1891429160332));
#91156=CARTESIAN_POINT('Ctrl Pts',(17.2112858742539,20.6817317985459,-18.1888651213047));
#91157=CARTESIAN_POINT('Ctrl Pts',(17.205605977836,20.6758254156188,-18.1883707601584));
#91158=CARTESIAN_POINT('Ctrl Pts',(17.2031341027575,20.6732419053222,-18.188154535459));
#91159=CARTESIAN_POINT('Ctrl Pts',(17.1978517444917,20.6676929084314,-18.1876901289652));
#91160=CARTESIAN_POINT('Ctrl Pts',(17.1950433396301,20.6647255893828,-18.1874418007334));
#91161=CARTESIAN_POINT('Ctrl Pts',(17.1892976819905,20.6586195039357,-18.1869308575326));
#91162=CARTESIAN_POINT('Ctrl Pts',(17.1863613663141,20.6554798850187,-18.186668174419));
#91163=CARTESIAN_POINT('Ctrl Pts',(17.172907708721,20.641006617132,-18.1854574802763));
#91164=CARTESIAN_POINT('Ctrl Pts',(17.1625054852299,20.6295672437599,-18.1845012580124));
#91165=CARTESIAN_POINT('Ctrl Pts',(17.0941974973345,20.5527752339454,-18.1780928157282));
#91166=CARTESIAN_POINT('Ctrl Pts',(17.0402626618156,20.4840136367756,-18.1724082045646));
#91167=CARTESIAN_POINT('Ctrl Pts',(16.9494514375479,20.3522138990728,-18.161872553892));
#91168=CARTESIAN_POINT('Ctrl Pts',(16.9112865550028,20.2902120188646,-18.157046711364));
#91169=CARTESIAN_POINT('Ctrl Pts',(16.8741069813084,20.2221921702089,-18.1519487845772));
#91170=CARTESIAN_POINT('Ctrl Pts',(16.8718386237847,20.2180087662163,-18.1516360039948));
#91171=CARTESIAN_POINT('Ctrl Pts',(16.8058494071645,20.0953231363686,-18.1424856013833));
#91172=CARTESIAN_POINT('Ctrl Pts',(16.7535466359384,19.9710054393493,-18.133855260602));
#91173=CARTESIAN_POINT('Ctrl Pts',(16.708693751212,19.8274997919292,-18.1246738677132));
#91174=CARTESIAN_POINT('Ctrl Pts',(16.7041601068514,19.8124045427961,-18.123716947619));
#91175=CARTESIAN_POINT('Ctrl Pts',(16.697560032873,19.7895035996151,-18.1222782772424));
#91176=CARTESIAN_POINT('Ctrl Pts',(16.6953690586117,19.7817346512263,-18.121792479011));
#91177=CARTESIAN_POINT('Ctrl Pts',(16.6915244699324,19.7677975267565,-18.1209249599746));
#91178=CARTESIAN_POINT('Ctrl Pts',(16.6898542383331,19.7616340737468,-18.1205427029385));
#91179=CARTESIAN_POINT('Ctrl Pts',(16.6863713131476,19.7485471872113,-18.1197339567774));
#91180=CARTESIAN_POINT('Ctrl Pts',(16.6845657850353,19.7416219163989,-18.119307704042));
#91181=CARTESIAN_POINT('Ctrl Pts',(16.6809624106151,19.7275080461815,-18.1184424219227));
#91182=CARTESIAN_POINT('Ctrl Pts',(16.6791671181765,19.7203188933179,-18.1180034797745));
#91183=CARTESIAN_POINT('Ctrl Pts',(16.6747876919973,19.7023815898169,-18.1169127010839));
#91184=CARTESIAN_POINT('Ctrl Pts',(16.6722499088747,19.6916222683857,-18.1162623493033));
#91185=CARTESIAN_POINT('Ctrl Pts',(16.6345655716973,19.5260604238103,-18.1063131420913));
#91186=CARTESIAN_POINT('Ctrl Pts',(16.6168549651969,19.3678091385423,-18.0976369978758));
#91187=CARTESIAN_POINT('Ctrl Pts',(16.6170008943746,19.2090540346034,-18.089014728333));
#91188=CARTESIAN_POINT('Ctrl Pts',(16.6170008942678,19.2090541508675,-18.0890147346475));
#91189=CARTESIAN_POINT('Ctrl Pts',(16.6171322447143,19.0661505859132,-18.0812533901164));
#91190=CARTESIAN_POINT('Ctrl Pts',(16.6317328296694,18.9236421400003,-18.0735575474113));
#91191=CARTESIAN_POINT('Ctrl Pts',(16.66253979312,18.7741512307517,-18.0645864550536));
#91192=CARTESIAN_POINT('Ctrl Pts',(16.6645755328753,18.7646071203777,-18.0640096344675));
#91193=CARTESIAN_POINT('Ctrl Pts',(16.6678825024972,18.7496120812857,-18.0630964765093));
#91194=CARTESIAN_POINT('Ctrl Pts',(16.6691095143436,18.7441514103039,-18.0627624919851));
#91195=CARTESIAN_POINT('Ctrl Pts',(16.6714748390661,18.7338165827897,-18.0621275467242));
#91196=CARTESIAN_POINT('Ctrl Pts',(16.672608815234,18.7289414606676,-18.0618268279476));
#91197=CARTESIAN_POINT('Ctrl Pts',(16.6745951113992,18.7205372740482,-18.0613062705801));
#91198=CARTESIAN_POINT('Ctrl Pts',(16.6754392490442,18.7170062599395,-18.0610869016675));
#91199=CARTESIAN_POINT('Ctrl Pts',(16.6770954354609,18.7101564253846,-18.0606600439741));
#91200=CARTESIAN_POINT('Ctrl Pts',(16.6779064370994,18.7068373932249,-18.060452621718));
#91201=CARTESIAN_POINT('Ctrl Pts',(16.6801203219178,18.6978712381477,-18.0598907105575));
#91202=CARTESIAN_POINT('Ctrl Pts',(16.6815384465943,18.692227961207,-18.0595353560513));
#91203=CARTESIAN_POINT('Ctrl Pts',(16.6869129238201,18.6712078135313,-18.0582056095516));
#91204=CARTESIAN_POINT('Ctrl Pts',(16.6910188512614,18.6558702012061,-18.0572231157216));
#91205=CARTESIAN_POINT('Ctrl Pts',(16.7100001833739,18.5880300928202,-18.0528274467239));
#91206=CARTESIAN_POINT('Ctrl Pts',(16.7267222361259,18.5360951484225,-18.0493292904414));
#91207=CARTESIAN_POINT('Ctrl Pts',(16.7454193875989,18.4848897136231,-18.0457833433865));
#91208=CARTESIAN_POINT('Origin',(18.734,19.211,0.));
#91209=CARTESIAN_POINT('',(16.7454194502294,18.4848895420984,-17.2426989706651));
#91210=CARTESIAN_POINT('',(16.7454194505834,18.4848895411289,-17.4677764891862));
#91211=CARTESIAN_POINT('',(16.7454194503191,18.4848895418526,0.));
#91212=CARTESIAN_POINT('Ctrl Pts',(16.7454194505834,18.4848895411289,-17.4677764891862));
#91213=CARTESIAN_POINT('Ctrl Pts',(16.7278145381498,18.5331036744084,-17.471069432283));
#91214=CARTESIAN_POINT('Ctrl Pts',(16.7119674259087,18.5819461488812,-17.4743159633458));
#91215=CARTESIAN_POINT('Ctrl Pts',(16.6884846851829,18.6644279468596,-17.4796471179921));
#91216=CARTESIAN_POINT('Ctrl Pts',(16.6798675453392,18.6977612741547,-17.4817614577792));
#91217=CARTESIAN_POINT('Ctrl Pts',(16.6696144590733,18.741832165455,-17.4845061250789));
#91218=CARTESIAN_POINT('Ctrl Pts',(16.6672430098837,18.7523915949572,-17.485159967894));
#91219=CARTESIAN_POINT('Ctrl Pts',(16.6634921057334,18.7697136033824,-17.4862264849215));
#91220=CARTESIAN_POINT('Ctrl Pts',(16.6620645844282,18.7764654679844,-17.486640694217));
#91221=CARTESIAN_POINT('Ctrl Pts',(16.6593656416378,18.7895466182744,-17.4874403240723));
#91222=CARTESIAN_POINT('Ctrl Pts',(16.6580901071216,18.7958749683059,-17.4878258722433));
#91223=CARTESIAN_POINT('Ctrl Pts',(16.6552123719551,18.8104973739121,-17.4887137889343));
#91224=CARTESIAN_POINT('Ctrl Pts',(16.6536308200333,18.8187954179053,-17.4892154938139));
#91225=CARTESIAN_POINT('Ctrl Pts',(16.6495122698741,18.8411305999054,-17.4905601779181));
#91226=CARTESIAN_POINT('Ctrl Pts',(16.6470673782895,18.8551844333864,-17.4914002290407));
#91227=CARTESIAN_POINT('Ctrl Pts',(16.6261906875318,18.9828153699925,-17.4989768923311));
#91228=CARTESIAN_POINT('Ctrl Pts',(16.6169037092498,19.0977007839662,-17.5054070942451));
#91229=CARTESIAN_POINT('Ctrl Pts',(16.6171578063362,19.3990360603433,-17.5219135172291));
#91230=CARTESIAN_POINT('Ctrl Pts',(16.6418924522489,19.5844189884413,-17.5316811019748));
#91231=CARTESIAN_POINT('Ctrl Pts',(16.6942562458898,19.7778655756035,-17.5434580591134));
#91232=CARTESIAN_POINT('Ctrl Pts',(16.6981093688598,19.7915518726192,-17.5443004486877));
#91233=CARTESIAN_POINT('Ctrl Pts',(16.7036607297278,19.810535127945,-17.5454829879046));
#91234=CARTESIAN_POINT('Ctrl Pts',(16.7052425223367,19.8158661151707,-17.5458166329892));
#91235=CARTESIAN_POINT('Ctrl Pts',(16.70781564287,19.8244144478422,-17.5463542340038));
#91236=CARTESIAN_POINT('Ctrl Pts',(16.7087936869134,19.8276358106429,-17.546557417383));
#91237=CARTESIAN_POINT('Ctrl Pts',(16.7108530777658,19.8343610330275,-17.5469828690383));
#91238=CARTESIAN_POINT('Ctrl Pts',(16.7119358448849,19.8378644178034,-17.5472052228027));
#91239=CARTESIAN_POINT('Ctrl Pts',(16.7145777282274,19.8463343894496,-17.5477445178966));
#91240=CARTESIAN_POINT('Ctrl Pts',(16.7161460667055,19.8512980561515,-17.5480619953759));
#91241=CARTESIAN_POINT('Ctrl Pts',(16.7216994325126,19.868650971913,-17.5491767913443));
#91242=CARTESIAN_POINT('Ctrl Pts',(16.7257802914508,19.8810089235115,-17.5499794559409));
#91243=CARTESIAN_POINT('Ctrl Pts',(16.750571251162,19.9538209765807,-17.5547573412506));
#91244=CARTESIAN_POINT('Ctrl Pts',(16.7738944100975,20.0133447680255,-17.5588615547738));
#91245=CARTESIAN_POINT('Ctrl Pts',(16.8760923080288,20.2429951840857,-17.5752528654356));
#91246=CARTESIAN_POINT('Ctrl Pts',(16.974746264155,20.4034264307322,-17.5878515501128));
#91247=CARTESIAN_POINT('Ctrl Pts',(17.1286546429515,20.5921933516103,-17.6032548845364));
#91248=CARTESIAN_POINT('Ctrl Pts',(17.1657758433198,20.6342015705637,-17.6067354194405));
#91249=CARTESIAN_POINT('Ctrl Pts',(17.2128425227556,20.6833836833239,-17.6108793252361));
#91250=CARTESIAN_POINT('Ctrl Pts',(17.2212358818161,20.692005912753,-17.611608560134));
#91251=CARTESIAN_POINT('Ctrl Pts',(17.2352366845433,20.7061452736404,-17.6128091588313));
#91252=CARTESIAN_POINT('Ctrl Pts',(17.2408020960839,20.7117034641773,-17.6132823519281));
#91253=CARTESIAN_POINT('Ctrl Pts',(17.2509287741856,20.7217048960451,-17.614136123977));
#91254=CARTESIAN_POINT('Ctrl Pts',(17.2554793349983,20.7261587996999,-17.6145171714241));
#91255=CARTESIAN_POINT('Ctrl Pts',(17.2652853757592,20.7356703085867,-17.6153327649525));
#91256=CARTESIAN_POINT('Ctrl Pts',(17.2705470492769,20.7407214322899,-17.6157670254912));
#91257=CARTESIAN_POINT('Ctrl Pts',(17.2849677660904,20.7544225901594,-17.616948154851));
#91258=CARTESIAN_POINT('Ctrl Pts',(17.2941781765849,20.7630183097727,-17.6176926787737));
#91259=CARTESIAN_POINT('Ctrl Pts',(17.3433135806804,20.8080606057894,-17.6216137775313));
#91260=CARTESIAN_POINT('Ctrl Pts',(17.3845489113014,20.8430520145755,-17.6247285072309));
#91261=CARTESIAN_POINT('Ctrl Pts',(17.5775460280295,20.9945034180545,-17.6386250069292));
#91262=CARTESIAN_POINT('Ctrl Pts',(17.7433022263399,21.0916335286676,-17.6486492253669));
#91263=CARTESIAN_POINT('Ctrl Pts',(17.9351125746571,21.1715462468961,-17.6602003078369));
#91264=CARTESIAN_POINT('Ctrl Pts',(17.950457994147,21.1777294195228,-17.6611247770083));
#91265=CARTESIAN_POINT('Ctrl Pts',(18.0154375139924,21.2030306048585,-17.6650468978339));
#91266=CARTESIAN_POINT('Ctrl Pts',(18.0657063777173,21.2204528111761,-17.6680992472002));
#91267=CARTESIAN_POINT('Ctrl Pts',(18.1249049324642,21.2385029156948,-17.6717720071343));
#91268=CARTESIAN_POINT('Ctrl Pts',(18.1332522675775,21.2409918794265,-17.6722916723895));
#91269=CARTESIAN_POINT('Ctrl Pts',(18.1459167026367,21.2446831405404,-17.6730831307443));
#91270=CARTESIAN_POINT('Ctrl Pts',(18.1502227682919,21.2459233950315,-17.6733527652239));
#91271=CARTESIAN_POINT('Ctrl Pts',(18.1579604287672,21.24812545351,-17.6738382792656));
#91272=CARTESIAN_POINT('Ctrl Pts',(18.1613905405095,21.2490922716031,-17.6740538634403));
#91273=CARTESIAN_POINT('Ctrl Pts',(18.1688506234465,21.2511746657762,-17.6745235166991));
#91274=CARTESIAN_POINT('Ctrl Pts',(18.1728814107155,21.2522869501261,-17.674777767616));
#91275=CARTESIAN_POINT('Ctrl Pts',(18.1842167233877,21.2553787867753,-17.6754940931238));
#91276=CARTESIAN_POINT('Ctrl Pts',(18.191528521107,21.2573310987412,-17.6759576997751));
#91277=CARTESIAN_POINT('Ctrl Pts',(18.2353830048929,21.2687890615176,-17.6787468828349));
#91278=CARTESIAN_POINT('Ctrl Pts',(18.2721618032511,21.2773542294488,-17.6811215649766));
#91279=CARTESIAN_POINT('Ctrl Pts',(18.3941309889349,21.3023400940216,-17.6890700032577));
#91280=CARTESIAN_POINT('Ctrl Pts',(18.4800992851541,21.3145082245148,-17.6947858486727));
#91281=CARTESIAN_POINT('Ctrl Pts',(18.741827592304,21.3352735164521,-17.7121325352482));
#91282=CARTESIAN_POINT('Ctrl Pts',(18.9181763674323,21.3272943791837,-17.7236768236546));
#91283=CARTESIAN_POINT('Ctrl Pts',(19.1141646073011,21.2937124697931,-17.7359157476735));
#91284=CARTESIAN_POINT('Ctrl Pts',(19.1367351307694,21.2894659824281,-17.7373176168934));
#91285=CARTESIAN_POINT('Ctrl Pts',(19.1685800735477,21.2829363417795,-17.7392854326175));
#91286=CARTESIAN_POINT('Ctrl Pts',(19.1779143889847,21.2809565368931,-17.7398610030083));
#91287=CARTESIAN_POINT('Ctrl Pts',(19.1930627928452,21.2776363844247,-17.7407931594251));
#91288=CARTESIAN_POINT('Ctrl Pts',(19.1988850849014,21.2763344649648,-17.741150971393));
#91289=CARTESIAN_POINT('Ctrl Pts',(19.211063708426,21.2735571013614,-17.7418984756122));
#91290=CARTESIAN_POINT('Ctrl Pts',(19.2174188868234,21.272076844663,-17.7422880089456));
#91291=CARTESIAN_POINT('Ctrl Pts',(19.232526428858,21.2684842558276,-17.7432127775852));
#91292=CARTESIAN_POINT('Ctrl Pts',(19.2412724063549,21.2663454144774,-17.743747153775));
#91293=CARTESIAN_POINT('Ctrl Pts',(19.2707149375798,21.2589458212547,-17.7455429570136));
#91294=CARTESIAN_POINT('Ctrl Pts',(19.2913458872534,21.2534276295855,-17.7467960732497));
#91295=CARTESIAN_POINT('Ctrl Pts',(19.4033557192912,21.2216445272356,-17.753576137664));
#91296=CARTESIAN_POINT('Ctrl Pts',(19.492974382584,21.1895574117104,-17.7589087810605));
#91297=CARTESIAN_POINT('Ctrl Pts',(19.7363095986762,21.0834556104271,-17.7735133182203));
#91298=CARTESIAN_POINT('Ctrl Pts',(19.8836685566068,20.9967672952764,-17.7824758109733));
#91299=CARTESIAN_POINT('Ctrl Pts',(20.0485503306469,20.8708271237563,-17.7943218991438));
#91300=CARTESIAN_POINT('Ctrl Pts',(20.0774678139186,20.8475092448898,-17.7964788729866));
#91301=CARTESIAN_POINT('Ctrl Pts',(20.1112112788538,20.8188026655144,-17.7991125988913));
#91302=CARTESIAN_POINT('Ctrl Pts',(20.1166438930873,20.8141332382076,-17.7995403465985));
#91303=CARTESIAN_POINT('Ctrl Pts',(20.1254646639922,20.8064734438604,-17.8002411667417));
#91304=CARTESIAN_POINT('Ctrl Pts',(20.1288671799788,20.8034995982892,-17.8005130443811));
#91305=CARTESIAN_POINT('Ctrl Pts',(20.1349379838007,20.7981592502612,-17.8010009562064));
#91306=CARTESIAN_POINT('Ctrl Pts',(20.1376098358062,20.7957968793201,-17.8012166822356));
#91307=CARTESIAN_POINT('Ctrl Pts',(20.1433801608473,20.7906688927959,-17.8016847379081));
#91308=CARTESIAN_POINT('Ctrl Pts',(20.1464764263562,20.7879009458304,-17.8019372390437));
#91309=CARTESIAN_POINT('Ctrl Pts',(20.1550950819255,20.780150436122,-17.8026438184658));
#91310=CARTESIAN_POINT('Ctrl Pts',(20.160599324441,20.7751479107757,-17.8030993639404));
#91311=CARTESIAN_POINT('Ctrl Pts',(20.1922708963681,20.7460569945044,-17.8057449268417));
#91312=CARTESIAN_POINT('Ctrl Pts',(20.2178525815749,20.7213427274424,-17.8079784654129));
#91313=CARTESIAN_POINT('Ctrl Pts',(20.2978171774206,20.6400965326136,-17.8152423233763));
#91314=CARTESIAN_POINT('Ctrl Pts',(20.3496837032355,20.5811845037461,-17.8203908452554));
#91315=CARTESIAN_POINT('Ctrl Pts',(20.514464659045,20.3716207401282,-17.8379867275695));
#91316=CARTESIAN_POINT('Ctrl Pts',(20.6105582562123,20.2088240356525,-17.8503962460361));
#91317=CARTESIAN_POINT('Ctrl Pts',(20.6923702539724,20.015333087509,-17.8633119731376));
#91318=CARTESIAN_POINT('Ctrl Pts',(20.7005622604193,19.9950910018949,-17.8646439180138));
#91319=CARTESIAN_POINT('Ctrl Pts',(20.7114759711671,19.9668760547626,-17.8664746012221));
#91320=CARTESIAN_POINT('Ctrl Pts',(20.7144652639641,19.9590088021795,-17.8669823003044));
#91321=CARTESIAN_POINT('Ctrl Pts',(20.7195285507188,19.9454400440436,-17.8678532649114));
#91322=CARTESIAN_POINT('Ctrl Pts',(20.7216250794035,19.9397471090383,-17.8682172814285));
#91323=CARTESIAN_POINT('Ctrl Pts',(20.7259018044506,19.9279782907146,-17.8689669318332));
#91324=CARTESIAN_POINT('Ctrl Pts',(20.7280787429726,19.921901284412,-17.869352453872));
#91325=CARTESIAN_POINT('Ctrl Pts',(20.733088397827,19.9077125658525,-17.8702489681924));
#91326=CARTESIAN_POINT('Ctrl Pts',(20.7358996073823,19.8995933393707,-17.8707592418767));
#91327=CARTESIAN_POINT('Ctrl Pts',(20.7447725785032,19.8734531148339,-17.872393474927));
#91328=CARTESIAN_POINT('Ctrl Pts',(20.7506411364583,19.8553671728449,-17.8735110562459));
#91329=CARTESIAN_POINT('Ctrl Pts',(20.7789116014426,19.7640704598513,-17.8790902698697));
#91330=CARTESIAN_POINT('Ctrl Pts',(20.7975753557142,19.6897577025538,-17.8834287521325));
#91331=CARTESIAN_POINT('Ctrl Pts',(20.8331254686511,19.5067026779437,-17.8937918397514));
#91332=CARTESIAN_POINT('Ctrl Pts',(20.8456447165604,19.397347030519,-17.8997070761613));
#91333=CARTESIAN_POINT('Ctrl Pts',(20.852163677474,19.2170914331259,-17.90953068319));
#91334=CARTESIAN_POINT('Ctrl Pts',(20.8511926986483,19.1465921290349,-17.9133941242643));
#91335=CARTESIAN_POINT('Ctrl Pts',(20.8436648199995,19.0285407420244,-17.9200783564362));
#91336=CARTESIAN_POINT('Ctrl Pts',(20.8390039902355,18.9809250615126,-17.9228339540835));
#91337=CARTESIAN_POINT('Ctrl Pts',(20.8317210118101,18.9258414011549,-17.9261328082676));
#91338=CARTESIAN_POINT('Ctrl Pts',(20.8306647736406,18.9181763453397,-17.9265943689256));
#91339=CARTESIAN_POINT('Ctrl Pts',(20.8289077477013,18.9059228417631,-17.9273365017912));
#91340=CARTESIAN_POINT('Ctrl Pts',(20.82823383626,18.9013305278501,-17.9276155970307));
#91341=CARTESIAN_POINT('Ctrl Pts',(20.8270122832189,18.8931927429871,-17.9281119314208));
#91342=CARTESIAN_POINT('Ctrl Pts',(20.8264707254483,18.8896464045768,-17.9283288240676));
#91343=CARTESIAN_POINT('Ctrl Pts',(20.8253023152921,18.8821233780297,-17.9287902170686));
#91344=CARTESIAN_POINT('Ctrl Pts',(20.8246731432062,18.8781471585274,-17.9290348410504));
#91345=CARTESIAN_POINT('Ctrl Pts',(20.8229412017746,18.8674003599248,-17.9296980122098));
#91346=CARTESIAN_POINT('Ctrl Pts',(20.8218168699204,18.8606333751208,-17.9301177528161));
#91347=CARTESIAN_POINT('Ctrl Pts',(20.8160296030717,18.8268190026475,-17.9322255765431));
#91348=CARTESIAN_POINT('Ctrl Pts',(20.8108741000732,18.7998599839208,-17.9339393555694));
#91349=CARTESIAN_POINT('Ctrl Pts',(20.7943756947817,18.7218411635685,-17.938981270215));
#91350=CARTESIAN_POINT('Ctrl Pts',(20.7816632939064,18.6710938347364,-17.9423637066549));
#91351=CARTESIAN_POINT('Ctrl Pts',(20.7281508699135,18.4867346121005,-17.9549159520242));
#91352=CARTESIAN_POINT('Ctrl Pts',(20.676031861902,18.3567665953127,-17.9642561577558));
#91353=CARTESIAN_POINT('Ctrl Pts',(20.568025803529,18.1494501516391,-17.9793774121036));
#91354=CARTESIAN_POINT('Ctrl Pts',(20.5190441747391,18.0690016554109,-17.9853157197031));
#91355=CARTESIAN_POINT('Ctrl Pts',(20.4569072706104,17.9807680760621,-17.9919011250461));
#91356=CARTESIAN_POINT('Ctrl Pts',(20.4488381347374,17.9695451133157,-17.9927403433996));
#91357=CARTESIAN_POINT('Ctrl Pts',(20.4357377078108,17.9516958399824,-17.9940778131357));
#91358=CARTESIAN_POINT('Ctrl Pts',(20.4307763725365,17.9450189028627,-17.9945787533409));
#91359=CARTESIAN_POINT('Ctrl Pts',(20.4219072802446,17.9332287276212,-17.9954644985758));
#91360=CARTESIAN_POINT('Ctrl Pts',(20.4180153438979,17.9281037710892,-17.9958499152712));
#91361=CARTESIAN_POINT('Ctrl Pts',(20.4098676450413,17.9174757328825,-17.996650060495));
#91362=CARTESIAN_POINT('Ctrl Pts',(20.4056079990364,17.9119757151419,-17.9970646294719));
#91363=CARTESIAN_POINT('Ctrl Pts',(20.3944973180197,17.8977748499481,-17.998136383414));
#91364=CARTESIAN_POINT('Ctrl Pts',(20.3876049277941,17.8891065142371,-17.9987919162296));
#91365=CARTESIAN_POINT('Ctrl Pts',(20.3575847336181,17.8519533257188,-18.0016078413936));
#91366=CARTESIAN_POINT('Ctrl Pts',(20.3337857501951,17.8240172883197,-18.0037410557394));
#91367=CARTESIAN_POINT('Ctrl Pts',(20.2688577207695,17.7516986906226,-18.0093211374301));
#91368=CARTESIAN_POINT('Ctrl Pts',(20.2265311953206,17.7084355318785,-18.0127192631978));
#91369=CARTESIAN_POINT('Ctrl Pts',(20.0626353976562,17.5546827378792,-18.0251630816708));
#91370=CARTESIAN_POINT('Ctrl Pts',(19.9302075613234,17.4566512418382,-18.0338183669568));
#91371=CARTESIAN_POINT('Ctrl Pts',(19.7389938622242,17.3469071906713,-18.0461877225001));
#91372=CARTESIAN_POINT('Ctrl Pts',(19.6891028610983,17.3208592611254,-18.0494095568747));
#91373=CARTESIAN_POINT('Ctrl Pts',(19.6302525253493,17.2930588058304,-18.053271104193));
#91374=CARTESIAN_POINT('Ctrl Pts',(19.6222428771549,17.2893362420735,-18.0537979506305));
#91375=CARTESIAN_POINT('Ctrl Pts',(19.6101110613525,17.2837899117377,-18.054598215452));
#91376=CARTESIAN_POINT('Ctrl Pts',(19.6060058641526,17.2819289572066,-18.05486940274));
#91377=CARTESIAN_POINT('Ctrl Pts',(19.5986425598896,17.2786193549091,-18.0553565736344));
#91378=CARTESIAN_POINT('Ctrl Pts',(19.5953867094193,17.2771658161954,-18.0555722530103));
#91379=CARTESIAN_POINT('Ctrl Pts',(19.5883227022054,17.2740335469633,-18.0560407867821));
#91380=CARTESIAN_POINT('Ctrl Pts',(19.5845133145256,17.2723578409569,-18.056293815799));
#91381=CARTESIAN_POINT('Ctrl Pts',(19.5738460019558,17.2677029047829,-18.0570033308837));
#91382=CARTESIAN_POINT('Ctrl Pts',(19.5669772769126,17.2647487932967,-18.057461303547));
#91383=CARTESIAN_POINT('Ctrl Pts',(19.5267536975942,17.2477013094374,-18.0601490847304));
#91384=CARTESIAN_POINT('Ctrl Pts',(19.4930594299405,17.2344300942969,-18.0624240198908));
#91385=CARTESIAN_POINT('Ctrl Pts',(19.3831204868046,17.1943537867052,-18.0698844847535));
#91386=CARTESIAN_POINT('Ctrl Pts',(19.3056795058767,17.1710489807659,-18.0751948922975));
#91387=CARTESIAN_POINT('Ctrl Pts',(19.047642151826,17.1092457342018,-18.0927145441974));
#91388=CARTESIAN_POINT('Ctrl Pts',(18.8632910545939,17.089902785717,-18.1048693120295));
#91389=CARTESIAN_POINT('Ctrl Pts',(18.6565433610784,17.0953008944633,-18.1175895244022));
#91390=CARTESIAN_POINT('Ctrl Pts',(18.6343518742613,17.0962299070359,-18.1189446157085));
#91391=CARTESIAN_POINT('Ctrl Pts',(18.6037176416392,17.0979956625955,-18.1208017097063));
#91392=CARTESIAN_POINT('Ctrl Pts',(18.5952597625058,17.098534148783,-18.121313013871));
#91393=CARTESIAN_POINT('Ctrl Pts',(18.5807377890449,17.0995463093912,-18.1221885225074));
#91394=CARTESIAN_POINT('Ctrl Pts',(18.5746721325546,17.0999953517938,-18.1225534958415));
#91395=CARTESIAN_POINT('Ctrl Pts',(18.5621813314149,17.1009741929067,-18.1233036279888));
#91396=CARTESIAN_POINT('Ctrl Pts',(18.5557564971343,17.1015072134328,-18.1236886815058));
#91397=CARTESIAN_POINT('Ctrl Pts',(18.5408278888795,17.1028144183628,-18.1245815961476));
#91398=CARTESIAN_POINT('Ctrl Pts',(18.5323261262762,17.1036107234177,-18.1250887565259));
#91399=CARTESIAN_POINT('Ctrl Pts',(18.5051985080918,17.1063172591723,-18.1267028665239));
#91400=CARTESIAN_POINT('Ctrl Pts',(18.4865927541825,17.108423188016,-18.1278036599205));
#91401=CARTESIAN_POINT('Ctrl Pts',(18.443284526461,17.1139079618984,-18.1303528216572));
#91402=CARTESIAN_POINT('Ctrl Pts',(18.4186086918266,17.1174769170304,-18.1317952476117));
#91403=CARTESIAN_POINT('Ctrl Pts',(18.332072820792,17.1315577262709,-18.1368249801372));
#91404=CARTESIAN_POINT('Ctrl Pts',(18.2706204225959,17.1443829852342,-18.1403437948504));
#91405=CARTESIAN_POINT('Ctrl Pts',(18.0890101236765,17.1907954277338,-18.1507066446127));
#91406=CARTESIAN_POINT('Ctrl Pts',(17.9711630272875,17.2322838473503,-18.1573707516173));
#91407=CARTESIAN_POINT('Ctrl Pts',(17.7746724313688,17.3216378176537,-18.1692247103236));
#91408=CARTESIAN_POINT('Ctrl Pts',(17.694225304787,17.3646892892378,-18.1743222554369));
#91409=CARTESIAN_POINT('Ctrl Pts',(17.6087795695628,17.4177745718916,-18.1802822045596));
#91410=CARTESIAN_POINT('Ctrl Pts',(17.6007795166221,17.4228194214088,-18.1808457704524));
#91411=CARTESIAN_POINT('Ctrl Pts',(17.5889454065238,17.4303933418688,-18.18168812737));
#91412=CARTESIAN_POINT('Ctrl Pts',(17.58508521665,17.4328816370354,-18.1819642842158));
#91413=CARTESIAN_POINT('Ctrl Pts',(17.5782984602636,17.437287736454,-18.1824523120774));
#91414=CARTESIAN_POINT('Ctrl Pts',(17.5753685121989,17.4392002601475,-18.1826638296609));
#91415=CARTESIAN_POINT('Ctrl Pts',(17.5724154762232,17.4411383118368,-18.1828778616448));
#91416=CARTESIAN_POINT('Ctrl Pts',(17.5723876768811,17.4411565572391,-18.1828798765785));
#91417=CARTESIAN_POINT('Ctrl Pts',(17.5723329295829,17.4411924911032,-18.1828838448852));
#91418=CARTESIAN_POINT('Ctrl Pts',(17.5723059815571,17.4412101795543,-18.1828857982588));
#91419=CARTESIAN_POINT('Ctrl Pts',(17.5722528731422,17.4412450411944,-18.1828896480527));
#91420=CARTESIAN_POINT('Ctrl Pts',(17.5722267126976,17.4412622143691,-18.182891544473));
#91421=CARTESIAN_POINT('Ctrl Pts',(17.572175122085,17.441296082961,-18.1828952845066));
#91422=CARTESIAN_POINT('Ctrl Pts',(17.5721496918833,17.4413127783547,-18.1828971281186));
#91423=CARTESIAN_POINT('Ctrl Pts',(17.5720995102198,17.4413457250849,-18.1829007662609));
#91424=CARTESIAN_POINT('Ctrl Pts',(17.5720747586255,17.4413619764671,-18.1829025607975));
#91425=CARTESIAN_POINT('Ctrl Pts',(17.5720258872356,17.4413940658728,-18.1829061041825));
#91426=CARTESIAN_POINT('Ctrl Pts',(17.5720017674302,17.4414099038655,-18.1829078530285));
#91427=CARTESIAN_POINT('Ctrl Pts',(17.5719541167089,17.4414411945576,-18.1829113081347));
#91428=CARTESIAN_POINT('Ctrl Pts',(17.571930585955,17.4414566471167,-18.1829130143804));
#91429=CARTESIAN_POINT('Ctrl Pts',(17.5718840751017,17.4414871919498,-18.18291638705));
#91430=CARTESIAN_POINT('Ctrl Pts',(17.5718610948154,17.4415022843157,-18.1829180534851));
#91431=CARTESIAN_POINT('Ctrl Pts',(17.571815648977,17.4415321322613,-18.1829213491311));
#91432=CARTESIAN_POINT('Ctrl Pts',(17.5717931835544,17.4415468877278,-18.1829229783303));
#91433=CARTESIAN_POINT('Ctrl Pts',(17.5717487348362,17.4415760832076,-18.1829262018624));
#91434=CARTESIAN_POINT('Ctrl Pts',(17.5717267516314,17.4415905231353,-18.1829277961867));
#91435=CARTESIAN_POINT('Ctrl Pts',(17.5716832380417,17.4416191067115,-18.1829309520881));
#91436=CARTESIAN_POINT('Ctrl Pts',(17.5716617073941,17.4416332505086,-18.1829325136824));
#91437=CARTESIAN_POINT('Ctrl Pts',(17.5716190706881,17.4416612602982,-18.1829356061659));
#91438=CARTESIAN_POINT('Ctrl Pts',(17.5715979647949,17.44167512616,-18.1829371370414));
#91439=CARTESIAN_POINT('Ctrl Pts',(17.5715561524305,17.4417025965481,-18.1829401699072));
#91440=CARTESIAN_POINT('Ctrl Pts',(17.57153544589,17.4417162010995,-18.182941671901));
#91441=CARTESIAN_POINT('Ctrl Pts',(17.5714944086082,17.4417431643273,-18.1829446487124));
#91442=CARTESIAN_POINT('Ctrl Pts',(17.5714740778194,17.4417565230162,-18.1829461235319));
#91443=CARTESIAN_POINT('Ctrl Pts',(17.5714337701556,17.4417830088435,-18.1829490475778));
#91444=CARTESIAN_POINT('Ctrl Pts',(17.5714137932678,17.4417961359732,-18.1829504968036));
#91445=CARTESIAN_POINT('Ctrl Pts',(17.5713741726683,17.441822172258,-18.1829533711625));
#91446=CARTESIAN_POINT('Ctrl Pts',(17.5713545291607,17.4418350812631,-18.1829547962794));
#91447=CARTESIAN_POINT('Ctrl Pts',(17.5713155565373,17.4418606935957,-18.1829576237793));
#91448=CARTESIAN_POINT('Ctrl Pts',(17.5712962274227,17.4418733969075,-18.182959026161));
#91449=CARTESIAN_POINT('Ctrl Pts',(17.5712578661399,17.441898609275,-18.1829618094526));
#91450=CARTESIAN_POINT('Ctrl Pts',(17.5712388337983,17.4419111184308,-18.182963190374));
#91451=CARTESIAN_POINT('Ctrl Pts',(17.5712010491702,17.441935953547,-18.1829659319673));
#91452=CARTESIAN_POINT('Ctrl Pts',(17.5711822968948,17.4419482794874,-18.1829672926374));
#91453=CARTESIAN_POINT('Ctrl Pts',(17.5711450571503,17.4419727581579,-18.1829699948314));
#91454=CARTESIAN_POINT('Ctrl Pts',(17.5711265695495,17.4419849109626,-18.1829713363639));
#91455=CARTESIAN_POINT('Ctrl Pts',(17.5710898439478,17.4420090533225,-18.1829740013835));
#91456=CARTESIAN_POINT('Ctrl Pts',(17.5710716061683,17.4420210427209,-18.1829753248536));
#91457=CARTESIAN_POINT('Ctrl Pts',(17.5710353669697,17.4420448669384,-18.1829779547063));
#91458=CARTESIAN_POINT('Ctrl Pts',(17.5710173653863,17.4420567018553,-18.1829792611));
#91459=CARTESIAN_POINT('Ctrl Pts',(17.5709815858628,17.4420802254397,-18.1829818577204));
#91460=CARTESIAN_POINT('Ctrl Pts',(17.5709638077115,17.4420919142364,-18.1829831479616));
#91461=CARTESIAN_POINT('Ctrl Pts',(17.5709284620844,17.4421151540779,-18.1829857132159));
#91462=CARTESIAN_POINT('Ctrl Pts',(17.5709108948849,17.442126704932,-18.1829869882081));
#91463=CARTESIAN_POINT('Ctrl Pts',(17.5708759600353,17.4421496761772,-18.1829895237697));
#91464=CARTESIAN_POINT('Ctrl Pts',(17.5708585923436,17.4421610965871,-18.1829907843414));
#91465=CARTESIAN_POINT('Ctrl Pts',(17.5708240457307,17.4421838140066,-18.1829932918422));
#91466=CARTESIAN_POINT('Ctrl Pts',(17.5708068667396,17.4421951110542,-18.1829945387758));
#91467=CARTESIAN_POINT('Ctrl Pts',(17.5707726865593,17.4422175889388,-18.1829970197947));
#91468=CARTESIAN_POINT('Ctrl Pts',(17.5707556856181,17.4422287696052,-18.1829982538614));
#91469=CARTESIAN_POINT('Ctrl Pts',(17.5707218526017,17.4422510205822,-18.1830007097934));
#91470=CARTESIAN_POINT('Ctrl Pts',(17.5707050202001,17.4422620911005,-18.1830019316819));
#91471=CARTESIAN_POINT('Ctrl Pts',(17.5706715144529,17.4422841282125,-18.1830043639678));
#91472=CARTESIAN_POINT('Ctrl Pts',(17.5706548411569,17.4422950947672,-18.1830055743611));
#91473=CARTESIAN_POINT('Ctrl Pts',(17.5706216444584,17.4423169299593,-18.1830079843205));
#91474=CARTESIAN_POINT('Ctrl Pts',(17.570605121206,17.4423277984921,-18.1830091838751));
#91475=CARTESIAN_POINT('Ctrl Pts',(17.570572216745,17.4423494427856,-18.1830115727255));
#91476=CARTESIAN_POINT('Ctrl Pts',(17.5705558352775,17.4423602187111,-18.1830127620395));
#91477=CARTESIAN_POINT('Ctrl Pts',(17.5705232060589,17.4423816832514,-18.183015131012));
#91478=CARTESIAN_POINT('Ctrl Pts',(17.5705069582918,17.4423923718713,-18.183016310671));
#91479=CARTESIAN_POINT('Ctrl Pts',(17.566982828392,17.4447107960331,-18.1832721835445));
#91480=CARTESIAN_POINT('Ctrl Pts',(17.56348185495,17.4470289395001,-18.183527578501));
#91481=CARTESIAN_POINT('Ctrl Pts',(17.5533919580001,17.45375315368,-18.1842670607959));
#91482=CARTESIAN_POINT('Ctrl Pts',(17.5468209376607,17.4581857779186,-18.1847528846693));
#91483=CARTESIAN_POINT('Ctrl Pts',(17.5033266597986,17.4878825520949,-18.1879960317687));
#91484=CARTESIAN_POINT('Ctrl Pts',(17.467190127829,17.5142729428558,-18.190822405644));
#91485=CARTESIAN_POINT('Ctrl Pts',(17.3385925468834,17.6145862361737,-18.2012934831911));
#91486=CARTESIAN_POINT('Ctrl Pts',(17.251538945909,17.6950823624554,-18.2091816948777));
#91487=CARTESIAN_POINT('Ctrl Pts',(17.0719302031485,17.8915077774818,-18.2267169967406));
#91488=CARTESIAN_POINT('Ctrl Pts',(16.983870581663,18.0107508526359,-18.2362464651292));
#91489=CARTESIAN_POINT('Ctrl Pts',(16.9017321928617,18.1504877523761,-18.2461429233346));
#91490=CARTESIAN_POINT('Ctrl Pts',(16.8946440500213,18.1628295705175,-18.2470073575586));
#91491=CARTESIAN_POINT('Ctrl Pts',(16.8835524970935,18.1826011299718,-18.2483771351266));
#91492=CARTESIAN_POINT('Ctrl Pts',(16.8794682167216,18.1899847871268,-18.2488853765757));
#91493=CARTESIAN_POINT('Ctrl Pts',(16.8723380095826,18.2030588869045,-18.2497795699371));
#91494=CARTESIAN_POINT('Ctrl Pts',(16.8692737762323,18.2087391727414,-18.2501661725114));
#91495=CARTESIAN_POINT('Ctrl Pts',(16.8629851028918,18.2205254005149,-18.2509644709339));
#91496=CARTESIAN_POINT('Ctrl Pts',(16.8597644601158,18.2266332897756,-18.251376028527));
#91497=CARTESIAN_POINT('Ctrl Pts',(16.8515648039321,18.2423699197297,-18.252430966219));
#91498=CARTESIAN_POINT('Ctrl Pts',(16.846629717173,18.2520214173842,-18.2530727921898));
#91499=CARTESIAN_POINT('Ctrl Pts',(16.826264297891,18.2926160735764,-18.2557511773201));
#91500=CARTESIAN_POINT('Ctrl Pts',(16.8115185774839,18.3238980178994,-18.2577638058596));
#91501=CARTESIAN_POINT('Ctrl Pts',(16.7787536063524,18.3980651762211,-18.2624275038487));
#91502=CARTESIAN_POINT('Ctrl Pts',(16.7613690522028,18.4412087662872,-18.2650577862056));
#91503=CARTESIAN_POINT('Ctrl Pts',(16.7454194512262,18.4848895393686,-18.2676549287063));
#91504=CARTESIAN_POINT('Ctrl Pts',(16.7454193875989,18.4848897136231,-18.0457833433865));
#91505=CARTESIAN_POINT('Ctrl Pts',(16.7694007750431,18.4192124700628,-18.0412352318572));
#91506=CARTESIAN_POINT('Ctrl Pts',(16.7966314900153,18.3547353160456,-18.0366093750544));
#91507=CARTESIAN_POINT('Ctrl Pts',(16.8579483854115,18.2275406538387,-18.0272786197108));
#91508=CARTESIAN_POINT('Ctrl Pts',(16.892096831064,18.1649811270577,-18.0225819649794));
#91509=CARTESIAN_POINT('Ctrl Pts',(16.978591243529,18.0239422161366,-18.011832929093));
#91510=CARTESIAN_POINT('Ctrl Pts',(17.0331590482315,17.9469943678683,-18.0058472848897));
#91511=CARTESIAN_POINT('Ctrl Pts',(17.1062782688705,17.8572369002143,-17.9987333372101));
#91512=CARTESIAN_POINT('Ctrl Pts',(17.120130926287,17.8407521278998,-17.9974205295563));
#91513=CARTESIAN_POINT('Ctrl Pts',(17.1388605828479,17.8191418315462,-17.9956905478605));
#91514=CARTESIAN_POINT('Ctrl Pts',(17.1435148395733,17.8138257525991,-17.9952642363448));
#91515=CARTESIAN_POINT('Ctrl Pts',(17.1527788562823,17.8033506982318,-17.9944226994679));
#91516=CARTESIAN_POINT('Ctrl Pts',(17.1573874620078,17.7981908235994,-17.9940074335443));
#91517=CARTESIAN_POINT('Ctrl Pts',(17.1663406818436,17.7882650107935,-17.9932071352293));
#91518=CARTESIAN_POINT('Ctrl Pts',(17.1706819361164,17.7834961576686,-17.992821968023));
#91519=CARTESIAN_POINT('Ctrl Pts',(17.1807318671667,17.7725571736575,-17.9919368744562));
#91520=CARTESIAN_POINT('Ctrl Pts',(17.1864556614052,17.7664010313155,-17.9914375981433));
#91521=CARTESIAN_POINT('Ctrl Pts',(17.2018931563937,17.7499945110545,-17.9901037071673));
#91522=CARTESIAN_POINT('Ctrl Pts',(17.2116731110691,17.7398068527246,-17.9892719465976));
#91523=CARTESIAN_POINT('Ctrl Pts',(17.2964936087109,17.6532019038836,-17.9821687483938));
#91524=CARTESIAN_POINT('Ctrl Pts',(17.3771357592124,17.5824781851315,-17.9761599972751));
#91525=CARTESIAN_POINT('Ctrl Pts',(17.557081758988,17.4473515974383,-17.9637965954818));
#91526=CARTESIAN_POINT('Ctrl Pts',(17.6571165237939,17.3845518013112,-17.9574902290854));
#91527=CARTESIAN_POINT('Ctrl Pts',(17.8135386826446,17.3036917516068,-17.9477841101837));
#91528=CARTESIAN_POINT('Ctrl Pts',(17.8662965452217,17.279119169192,-17.9445320299065));
#91529=CARTESIAN_POINT('Ctrl Pts',(17.9471276805199,17.2454504963471,-17.9394869599092));
#91530=CARTESIAN_POINT('Ctrl Pts',(17.974491093388,17.2347158800626,-17.9377685758654));
#91531=CARTESIAN_POINT('Ctrl Pts',(18.0086259090111,17.2221384461147,-17.9356016719268));
#91532=CARTESIAN_POINT('Ctrl Pts',(18.0151961434791,17.2197544437846,-17.9351835322876));
#91533=CARTESIAN_POINT('Ctrl Pts',(18.025625938475,17.2160283496411,-17.9345179139001));
#91534=CARTESIAN_POINT('Ctrl Pts',(18.02947785329,17.2146647974544,-17.9342716903632));
#91535=CARTESIAN_POINT('Ctrl Pts',(18.0367077138852,17.2121290055456,-17.9338087516652));
#91536=CARTESIAN_POINT('Ctrl Pts',(18.0400846899702,17.2109541688816,-17.9335921930797));
#91537=CARTESIAN_POINT('Ctrl Pts',(18.047829942678,17.208281603055,-17.9330947703364));
#91538=CARTESIAN_POINT('Ctrl Pts',(18.0522001418168,17.2067896124719,-17.9328135718565));
#91539=CARTESIAN_POINT('Ctrl Pts',(18.0657524619673,17.2022122911968,-17.9319399868914));
#91540=CARTESIAN_POINT('Ctrl Pts',(18.0749507521021,17.1991757254206,-17.9313448401075));
#91541=CARTESIAN_POINT('Ctrl Pts',(18.1838239490618,17.164060961566,-17.9242770427483));
#91542=CARTESIAN_POINT('Ctrl Pts',(18.2857145920554,17.1393610118921,-17.9174370809357));
#91543=CARTESIAN_POINT('Ctrl Pts',(18.5556538025838,17.0947739039101,-17.8993941173019));
#91544=CARTESIAN_POINT('Ctrl Pts',(18.725034735708,17.0872867813506,-17.888201308236));
#91545=CARTESIAN_POINT('Ctrl Pts',(18.9210776613035,17.1021010602245,-17.8759055917875));
#91546=CARTESIAN_POINT('Ctrl Pts',(18.9485933595457,17.1047230497041,-17.8741931402574));
#91547=CARTESIAN_POINT('Ctrl Pts',(18.9960376606,17.1101834854926,-17.8712628653616));
#91548=CARTESIAN_POINT('Ctrl Pts',(19.015991160724,17.1127686513795,-17.8700373715249));
#91549=CARTESIAN_POINT('Ctrl Pts',(19.0447123268009,17.1169068732953,-17.8682828198744));
#91550=CARTESIAN_POINT('Ctrl Pts',(19.0535113359188,17.1182313354469,-17.8677465748083));
#91551=CARTESIAN_POINT('Ctrl Pts',(19.0687294139861,17.1206202375685,-17.8668212701996));
#91552=CARTESIAN_POINT('Ctrl Pts',(19.0751523578311,17.1216588593569,-17.8664313983205));
#91553=CARTESIAN_POINT('Ctrl Pts',(19.0874780352979,17.1237103352193,-17.8656844677823));
#91554=CARTESIAN_POINT('Ctrl Pts',(19.0933814501789,17.1247186573857,-17.8653272693811));
#91555=CARTESIAN_POINT('Ctrl Pts',(19.1088023277615,17.1274199892045,-17.864395582684));
#91556=CARTESIAN_POINT('Ctrl Pts',(19.1183126826966,17.1291531725628,-17.8638223758359));
#91557=CARTESIAN_POINT('Ctrl Pts',(19.1511148014039,17.1353635245841,-17.86184984785));
#91558=CARTESIAN_POINT('Ctrl Pts',(19.1743435098283,17.1401670285286,-17.8604609163047));
#91559=CARTESIAN_POINT('Ctrl Pts',(19.3559695113042,17.1809201832999,-17.8496523143701));
#91560=CARTESIAN_POINT('Ctrl Pts',(19.5098343618125,17.2345996954044,-17.84086054137));
#91561=CARTESIAN_POINT('Ctrl Pts',(19.7732432839508,17.3620519303113,-17.8249632570808));
#91562=CARTESIAN_POINT('Ctrl Pts',(19.8849297401308,17.4294314593247,-17.8178826643024));
#91563=CARTESIAN_POINT('Ctrl Pts',(19.9992785490981,17.5136784059995,-17.8095008712134));
#91564=CARTESIAN_POINT('Ctrl Pts',(20.0087921745942,17.5208120526872,-17.8087942035455));
#91565=CARTESIAN_POINT('Ctrl Pts',(20.0222355116379,17.5310703991321,-17.8077815124583));
#91566=CARTESIAN_POINT('Ctrl Pts',(20.0262151820152,17.5341296652678,-17.807479940922));
#91567=CARTESIAN_POINT('Ctrl Pts',(20.0330563060198,17.5394274133314,-17.8069583822628));
#91568=CARTESIAN_POINT('Ctrl Pts',(20.0359229770487,17.5416591838708,-17.8067388697597));
#91569=CARTESIAN_POINT('Ctrl Pts',(20.0414713245671,17.5460016871227,-17.8063121160466));
#91570=CARTESIAN_POINT('Ctrl Pts',(20.0441536477917,17.548111529523,-17.8061049430936));
#91571=CARTESIAN_POINT('Ctrl Pts',(20.0513796124041,17.553823612937,-17.8055445352819));
#91572=CARTESIAN_POINT('Ctrl Pts',(20.0559135357071,17.5574380195127,-17.8051904428509));
#91573=CARTESIAN_POINT('Ctrl Pts',(20.0727024771639,17.5709352044647,-17.8038702478292));
#91574=CARTESIAN_POINT('Ctrl Pts',(20.0848616347388,17.5809356865076,-17.8028961890968));
#91575=CARTESIAN_POINT('Ctrl Pts',(20.1982165645823,17.6763054588638,-17.7936543924056));
#91576=CARTESIAN_POINT('Ctrl Pts',(20.2912971904285,17.7708483397255,-17.7848626578304));
#91577=CARTESIAN_POINT('Ctrl Pts',(20.4751312135868,17.9963798255623,-17.7656435836203));
#91578=CARTESIAN_POINT('Ctrl Pts',(20.5612183200509,18.1301987969987,-17.7553219516416));
#91579=CARTESIAN_POINT('Ctrl Pts',(20.6409909805632,18.291474473976,-17.7442711325658));
#91580=CARTESIAN_POINT('Ctrl Pts',(20.6501374156965,18.3106893597136,-17.7429741982922));
#91581=CARTESIAN_POINT('Ctrl Pts',(20.6627342311604,18.3382147464022,-17.7411435616999));
#91582=CARTESIAN_POINT('Ctrl Pts',(20.6664235295409,18.3464138910887,-17.7406016492379));
#91583=CARTESIAN_POINT('Ctrl Pts',(20.6726991486793,18.360601764511,-17.7396696763341));
#91584=CARTESIAN_POINT('Ctrl Pts',(20.6753102072901,18.3665793533067,-17.7392787715828));
#91585=CARTESIAN_POINT('Ctrl Pts',(20.680257491221,18.3780495795848,-17.7385319856521));
#91586=CARTESIAN_POINT('Ctrl Pts',(20.6825981929262,18.3835402072292,-17.7381759545686));
#91587=CARTESIAN_POINT('Ctrl Pts',(20.6886261004958,18.3978474111791,-17.7372519347542));
#91588=CARTESIAN_POINT('Ctrl Pts',(20.6922769106077,18.4066792484475,-17.7366851858077));
#91589=CARTESIAN_POINT('Ctrl Pts',(20.7045303054971,18.4369000123294,-17.7347580499153));
#91590=CARTESIAN_POINT('Ctrl Pts',(20.7128434507132,18.4584050659376,-17.7334074117917));
#91591=CARTESIAN_POINT('Ctrl Pts',(20.7810962753581,18.6439219186914,-17.7219216025564));
#91592=CARTESIAN_POINT('Ctrl Pts',(20.8208822866533,18.8146292509893,-17.7125287212828));
#91593=CARTESIAN_POINT('Ctrl Pts',(20.8484696836762,19.0754196754077,-17.6982616249294));
#91594=CARTESIAN_POINT('Ctrl Pts',(20.8522681123727,19.1630224933138,-17.6934673595822));
#91595=CARTESIAN_POINT('Ctrl Pts',(20.8499192066847,19.2885696708907,-17.6862991722787));
#91596=CARTESIAN_POINT('Ctrl Pts',(20.8481873581345,19.3265099738846,-17.6840935315199));
#91597=CARTESIAN_POINT('Ctrl Pts',(20.8448871336712,19.3719408934137,-17.681383442228));
#91598=CARTESIAN_POINT('Ctrl Pts',(20.8442973265724,19.3794982249009,-17.6809303278143));
#91599=CARTESIAN_POINT('Ctrl Pts',(20.8433189958267,19.3912217550084,-17.6802236297753));
#91600=CARTESIAN_POINT('Ctrl Pts',(20.8429586795066,19.3953903321004,-17.6799716020201));
#91601=CARTESIAN_POINT('Ctrl Pts',(20.8422686044159,19.4031072385222,-17.6795036217923));
#91602=CARTESIAN_POINT('Ctrl Pts',(20.8419422433812,19.4066558137334,-17.6792878618748));
#91603=CARTESIAN_POINT('Ctrl Pts',(20.8411855869811,19.4146613651401,-17.6787998455118));
#91604=CARTESIAN_POINT('Ctrl Pts',(20.8407501125497,19.4191177840819,-17.6785273028526));
#91605=CARTESIAN_POINT('Ctrl Pts',(20.8394274758862,19.4322232757449,-17.6777232822785));
#91606=CARTESIAN_POINT('Ctrl Pts',(20.8385011777521,19.4408681814495,-17.6771896825332));
#91607=CARTESIAN_POINT('Ctrl Pts',(20.8315687415822,19.5020090784442,-17.6733940694801));
#91608=CARTESIAN_POINT('Ctrl Pts',(20.8236527906456,19.5542653691349,-17.6700368099673));
#91609=CARTESIAN_POINT('Ctrl Pts',(20.8085615198715,19.6336920229547,-17.6648134546291));
#91610=CARTESIAN_POINT('Ctrl Pts',(20.8027856594876,19.6611109320709,-17.6629879272846));
#91611=CARTESIAN_POINT('Ctrl Pts',(20.7654794458532,19.8222794246022,-17.6521522063743));
#91612=CARTESIAN_POINT('Ctrl Pts',(20.721527248678,19.9528296853035,-17.6429724273416));
#91613=CARTESIAN_POINT('Ctrl Pts',(20.6398198646363,20.1347899396232,-17.6300832910823));
#91614=CARTESIAN_POINT('Ctrl Pts',(20.6119317713591,20.1902398138991,-17.6261368762026));
#91615=CARTESIAN_POINT('Ctrl Pts',(20.56341174853,20.2769911100224,-17.6199428209381));
#91616=CARTESIAN_POINT('Ctrl Pts',(20.544316817235,20.3091064121426,-17.6176448544003));
#91617=CARTESIAN_POINT('Ctrl Pts',(20.5184335733051,20.3501268746623,-17.6147012688758));
#91618=CARTESIAN_POINT('Ctrl Pts',(20.5124117314167,20.3595055224583,-17.61402766517));
#91619=CARTESIAN_POINT('Ctrl Pts',(20.5025027569214,20.3746733262951,-17.6129371575771));
#91620=CARTESIAN_POINT('Ctrl Pts',(20.4986606520937,20.380491511868,-17.6125185834845));
#91621=CARTESIAN_POINT('Ctrl Pts',(20.491220098872,20.3916387547516,-17.6117160633738));
#91622=CARTESIAN_POINT('Ctrl Pts',(20.4876259826827,20.3969705980208,-17.6113319605348));
#91623=CARTESIAN_POINT('Ctrl Pts',(20.4793459026301,20.4091340941558,-17.6104550931246));
#91624=CARTESIAN_POINT('Ctrl Pts',(20.4746440004502,20.4159548099744,-17.6099629389182));
#91625=CARTESIAN_POINT('Ctrl Pts',(20.4620569814684,20.4339864768083,-17.6086605316839));
#91626=CARTESIAN_POINT('Ctrl Pts',(20.4541027413163,20.4451488670963,-17.6078529222034));
#91627=CARTESIAN_POINT('Ctrl Pts',(20.3933247531992,20.5287110139857,-17.601794959091));
#91628=CARTESIAN_POINT('Ctrl Pts',(20.3360564619037,20.5977728215801,-17.5967243210894));
#91629=CARTESIAN_POINT('Ctrl Pts',(20.1788940193098,20.7645223122779,-17.5840353610477));
#91630=CARTESIAN_POINT('Ctrl Pts',(20.0734157494003,20.8563309625267,-17.5766145748611));
#91631=CARTESIAN_POINT('Ctrl Pts',(19.9142050327264,20.969384287177,-17.5658324970017));
#91632=CARTESIAN_POINT('Ctrl Pts',(19.8674784146453,20.9998613797976,-17.5627088847467));
#91633=CARTESIAN_POINT('Ctrl Pts',(19.7950134452223,21.0431463104387,-17.5578409965815));
#91634=CARTESIAN_POINT('Ctrl Pts',(19.7701258074578,21.0573349539123,-17.5561650477678));
#91635=CARTESIAN_POINT('Ctrl Pts',(19.7388474017694,21.0743354746634,-17.5540440287497));
#91636=CARTESIAN_POINT('Ctrl Pts',(19.7327191813931,21.0776272754986,-17.5536277773761));
#91637=CARTESIAN_POINT('Ctrl Pts',(19.7230001955002,21.0827863106764,-17.5529663610738));
#91638=CARTESIAN_POINT('Ctrl Pts',(19.7194200456824,21.0846735874935,-17.5527224470012));
#91639=CARTESIAN_POINT('Ctrl Pts',(19.7126603391451,21.0882122355443,-17.5522613605475));
#91640=CARTESIAN_POINT('Ctrl Pts',(19.7094819942835,21.0898658054284,-17.5520443299069));
#91641=CARTESIAN_POINT('Ctrl Pts',(19.7022091732893,21.0936261445186,-17.5515471936676));
#91642=CARTESIAN_POINT('Ctrl Pts',(19.6981120162057,21.0957276255603,-17.5512667602578));
#91643=CARTESIAN_POINT('Ctrl Pts',(19.6872234748587,21.101267693771,-17.5505205684744));
#91644=CARTESIAN_POINT('Ctrl Pts',(19.6804204159355,21.104683009228,-17.5500534125796));
#91645=CARTESIAN_POINT('Ctrl Pts',(19.6328499252083,21.1282442881864,-17.5467810402348));
#91646=CARTESIAN_POINT('Ctrl Pts',(19.5914641285686,21.1471072908906,-17.5439048049551));
#91647=CARTESIAN_POINT('Ctrl Pts',(19.5442245208114,21.1668266768969,-17.5406145969368));
#91648=CARTESIAN_POINT('Ctrl Pts',(19.5389333864481,21.1690102161501,-17.540245970546));
#91649=CARTESIAN_POINT('Ctrl Pts',(19.3878102258,21.2306594626412,-17.5297157049605));
#91650=CARTESIAN_POINT('Ctrl Pts',(19.2358040147326,21.2736896493362,-17.5191256584674));
#91651=CARTESIAN_POINT('Ctrl Pts',(18.9788178326079,21.3163173978165,-17.5022143764419));
#91652=CARTESIAN_POINT('Ctrl Pts',(18.8761048670814,21.3257361038233,-17.4956952021538));
#91653=CARTESIAN_POINT('Ctrl Pts',(18.7582952652666,21.327912374419,-17.4885096331805));
#91654=CARTESIAN_POINT('Ctrl Pts',(18.7434875837209,21.3280305298032,-17.4876115088568));
#91655=CARTESIAN_POINT('Ctrl Pts',(18.7209109523997,21.3279737902928,-17.4862496142555));
#91656=CARTESIAN_POINT('Ctrl Pts',(18.7131424119755,21.3279115039332,-17.4857823326196));
#91657=CARTESIAN_POINT('Ctrl Pts',(18.6990135014297,21.3277204378913,-17.4849348580076));
#91658=CARTESIAN_POINT('Ctrl Pts',(18.6926530611768,21.327605749611,-17.4845542283781));
#91659=CARTESIAN_POINT('Ctrl Pts',(18.6789274053218,21.3272963619309,-17.4837346994523));
#91660=CARTESIAN_POINT('Ctrl Pts',(18.6715624771499,21.3270918789247,-17.4832961114984));
#91661=CARTESIAN_POINT('Ctrl Pts',(18.6516067753745,21.3264335455224,-17.4821107794829));
#91662=CARTESIAN_POINT('Ctrl Pts',(18.6390186167652,21.3259057369416,-17.4813663563354));
#91663=CARTESIAN_POINT('Ctrl Pts',(18.5779499495872,21.3227988388268,-17.4777700569275));
#91664=CARTESIAN_POINT('Ctrl Pts',(18.5295609840548,21.3186648628839,-17.4749671559836));
#91665=CARTESIAN_POINT('Ctrl Pts',(18.4408402631761,21.3080005841054,-17.4698882905772));
#91666=CARTESIAN_POINT('Ctrl Pts',(18.4004744140076,21.3019603081542,-17.46760061205));
#91667=CARTESIAN_POINT('Ctrl Pts',(18.2279671705293,21.2710235012372,-17.4578738607842));
#91668=CARTESIAN_POINT('Ctrl Pts',(18.0981936382654,21.234738032034,-17.4507040386991));
#91669=CARTESIAN_POINT('Ctrl Pts',(17.914208005236,21.1638350443407,-17.4398677489502));
#91670=CARTESIAN_POINT('Ctrl Pts',(17.8567128101947,21.1386902401825,-17.4363742131181));
#91671=CARTESIAN_POINT('Ctrl Pts',(17.7726606707444,21.0973914040426,-17.4309874992658));
#91672=CARTESIAN_POINT('Ctrl Pts',(17.7452021041984,21.0831443131641,-17.4291811176432));
#91673=CARTESIAN_POINT('Ctrl Pts',(17.711812846052,21.0648805902241,-17.4269145474043));
#91674=CARTESIAN_POINT('Ctrl Pts',(17.7055759333888,21.0614279927707,-17.4264881055031));
#91675=CARTESIAN_POINT('Ctrl Pts',(17.6957925211661,21.0559474032014,-17.4258141591422));
#91676=CARTESIAN_POINT('Ctrl Pts',(17.6922341846518,21.0539404968716,-17.4255679869908));
#91677=CARTESIAN_POINT('Ctrl Pts',(17.6855723010471,21.0501577272888,-17.4251050905651));
#91678=CARTESIAN_POINT('Ctrl Pts',(17.682467436557,21.0483842965251,-17.4248885225401));
#91679=CARTESIAN_POINT('Ctrl Pts',(17.6753618172859,21.0443018125396,-17.424391005736));
#91680=CARTESIAN_POINT('Ctrl Pts',(17.6713641286261,21.0419875318245,-17.4241097221638));
#91681=CARTESIAN_POINT('Ctrl Pts',(17.6590006518283,21.0347761293966,-17.423235615169));
#91682=CARTESIAN_POINT('Ctrl Pts',(17.650661039943,21.0298346978623,-17.4226400267852));
#91683=CARTESIAN_POINT('Ctrl Pts',(17.560183280674,20.9753813171494,-17.4161155796273));
#91684=CARTESIAN_POINT('Ctrl Pts',(17.4814756293523,20.9204050057408,-17.4098775552118));
#91685=CARTESIAN_POINT('Ctrl Pts',(17.3080590803382,20.7808525208292,-17.3952245813983));
#91686=CARTESIAN_POINT('Ctrl Pts',(17.2166658943002,20.6927037832022,-17.3867948010584));
#91687=CARTESIAN_POINT('Ctrl Pts',(17.0955502260439,20.5528523659937,-17.3748732452443));
#91688=CARTESIAN_POINT('Ctrl Pts',(17.0592305770765,20.5072383169643,-17.371174862511));
#91689=CARTESIAN_POINT('Ctrl Pts',(17.0037578839691,20.4313390331937,-17.3653244384609));
#91690=CARTESIAN_POINT('Ctrl Pts',(16.983411210312,20.4019677869511,-17.3631287167273));
#91691=CARTESIAN_POINT('Ctrl Pts',(16.9578008007423,20.3629226155869,-17.3602956491267));
#91692=CARTESIAN_POINT('Ctrl Pts',(16.9518562841104,20.3537042884106,-17.3596328533288));
#91693=CARTESIAN_POINT('Ctrl Pts',(16.9422715539011,20.3385842517995,-17.3585554693151));
#91694=CARTESIAN_POINT('Ctrl Pts',(16.9385882718256,20.3327102110524,-17.3581392853156));
#91695=CARTESIAN_POINT('Ctrl Pts',(16.9315377850271,20.3213425054804,-17.3573383893286));
#91696=CARTESIAN_POINT('Ctrl Pts',(16.9281666786304,20.315851362279,-17.3569535363394));
#91697=CARTESIAN_POINT('Ctrl Pts',(16.9204737488977,20.3031911953769,-17.356070815532));
#91698=CARTESIAN_POINT('Ctrl Pts',(16.9161692532598,20.2960117280348,-17.3555735863286));
#91699=CARTESIAN_POINT('Ctrl Pts',(16.9047788758154,20.2767556594777,-17.3542487703178));
#91700=CARTESIAN_POINT('Ctrl Pts',(16.8977699551827,20.264633846942,-17.3534239761013));
#91701=CARTESIAN_POINT('Ctrl Pts',(16.8410121010338,20.164185311981,-17.3466623641973));
#91702=CARTESIAN_POINT('Ctrl Pts',(16.7975427766105,20.0724538047347,-17.3409591108816));
#91703=CARTESIAN_POINT('Ctrl Pts',(16.7062965716862,19.8376978734538,-17.3270884795012));
#91704=CARTESIAN_POINT('Ctrl Pts',(16.6668952196633,19.6920445464143,-17.319119822132));
#91705=CARTESIAN_POINT('Ctrl Pts',(16.6370543890959,19.5043826523554,-17.3084710835149));
#91706=CARTESIAN_POINT('Ctrl Pts',(16.631938189477,19.4651457325877,-17.3062221137651));
#91707=CARTESIAN_POINT('Ctrl Pts',(16.626393979092,19.4107834529683,-17.3030474656015));
#91708=CARTESIAN_POINT('Ctrl Pts',(16.6250239190745,19.3957604686448,-17.3021639816366));
#91709=CARTESIAN_POINT('Ctrl Pts',(16.6229323250509,19.3697556824083,-17.3006220422313));
#91710=CARTESIAN_POINT('Ctrl Pts',(16.6221356451447,19.3587803435252,-17.2999673827355));
#91711=CARTESIAN_POINT('Ctrl Pts',(16.6211102618364,19.3429455002856,-17.2990166282724));
#91712=CARTESIAN_POINT('Ctrl Pts',(16.6208126721346,19.3380904282536,-17.2987242760423));
#91713=CARTESIAN_POINT('Ctrl Pts',(16.6203235173845,19.3296328029661,-17.2982134561621));
#91714=CARTESIAN_POINT('Ctrl Pts',(16.6201244222716,19.3260306778541,-17.2979954101872));
#91715=CARTESIAN_POINT('Ctrl Pts',(16.6197264097696,19.3184793973308,-17.2975372671188));
#91716=CARTESIAN_POINT('Ctrl Pts',(16.6195293495772,19.3145302038257,-17.2972970719183));
#91717=CARTESIAN_POINT('Ctrl Pts',(16.6190357980324,19.3040493179722,-17.2966580762555));
#91718=CARTESIAN_POINT('Ctrl Pts',(16.6187585037377,19.2975168254328,-17.2962582243825));
#91719=CARTESIAN_POINT('Ctrl Pts',(16.6177066689143,19.2696966953738,-17.2945489348637));
#91720=CARTESIAN_POINT('Ctrl Pts',(16.6172232249825,19.2484001290508,-17.2932244436307));
#91721=CARTESIAN_POINT('Ctrl Pts',(16.6170218768569,19.2219269139405,-17.2915610829938));
#91722=CARTESIAN_POINT('Ctrl Pts',(16.6170014935719,19.216752887994,-17.2912351857526));
#91723=CARTESIAN_POINT('Ctrl Pts',(16.6169868170217,19.1630721342973,-17.2878459976942));
#91724=CARTESIAN_POINT('Ctrl Pts',(16.618640710772,19.1145823861424,-17.2847171541311));
#91725=CARTESIAN_POINT('Ctrl Pts',(16.6353861374769,18.8703421461503,-17.2687464404757));
#91726=CARTESIAN_POINT('Ctrl Pts',(16.6759975325268,18.6772599417279,-17.2555537971222));
#91727=CARTESIAN_POINT('Ctrl Pts',(16.7435636729826,18.4899871113246,-17.2430395181198));
#91728=CARTESIAN_POINT('Ctrl Pts',(16.7444891184151,18.4874374185689,-17.2428691684334));
#91729=CARTESIAN_POINT('Ctrl Pts',(16.7454194502294,18.4848895420984,-17.2426989706651));
#91730=CARTESIAN_POINT('Origin',(18.734,19.211,0.));
#91731=CARTESIAN_POINT('',(16.7454194446555,18.4848895573634,-16.4437313838642));
#91732=CARTESIAN_POINT('',(16.7454194503294,18.4848895418246,-16.6645989754405));
#91733=CARTESIAN_POINT('',(16.7454194503191,18.4848895418526,0.));
#91734=CARTESIAN_POINT('',(16.6170007987606,19.2099039755699,-16.7126929344973));
#91735=CARTESIAN_POINT('Ctrl Pts',(16.7454194503294,18.4848895418246,-16.6645989754405));
#91736=CARTESIAN_POINT('Ctrl Pts',(16.7447285761329,18.4867816217058,-16.6647267315824));
#91737=CARTESIAN_POINT('Ctrl Pts',(16.7440404001695,18.4886746935246,-16.664854598572));
#91738=CARTESIAN_POINT('Ctrl Pts',(16.6879393884391,18.6436890726986,-16.6753284307576));
#91739=CARTESIAN_POINT('Ctrl Pts',(16.650376635932,18.8026872523377,-16.6862947866301));
#91740=CARTESIAN_POINT('Ctrl Pts',(16.621854709062,19.0458921890449,-16.7022898980983));
#91741=CARTESIAN_POINT('Ctrl Pts',(16.6170428510048,19.1278576474473,-16.7075611564714));
#91742=CARTESIAN_POINT('Ctrl Pts',(16.617000284921,19.2099016579427,-16.7126936831171));
#91743=CARTESIAN_POINT('Ctrl Pts',(16.6170002837488,19.2099039196303,-16.7126938246042));
#91744=CARTESIAN_POINT('Ctrl Pts',(16.6169868619687,19.2358271140463,-16.7143155325004));
#91745=CARTESIAN_POINT('Ctrl Pts',(16.6174495936211,19.2617494353718,-16.7159232237688));
#91746=CARTESIAN_POINT('Ctrl Pts',(16.6190263313245,19.3052644054436,-16.7185989970965));
#91747=CARTESIAN_POINT('Ctrl Pts',(16.6198840704897,19.3228626987045,-16.7196748128033));
#91748=CARTESIAN_POINT('Ctrl Pts',(16.6214584272066,19.3485615081172,-16.7212369082377));
#91749=CARTESIAN_POINT('Ctrl Pts',(16.6220021593856,19.3566715120544,-16.7217285743142));
#91750=CARTESIAN_POINT('Ctrl Pts',(16.6230473344705,19.3710219815548,-16.722596318813));
#91751=CARTESIAN_POINT('Ctrl Pts',(16.6235297736961,19.3772636938281,-16.7229729894496));
#91752=CARTESIAN_POINT('Ctrl Pts',(16.6245388660994,19.3896063308187,-16.7237163741477));
#91753=CARTESIAN_POINT('Ctrl Pts',(16.6250643169823,19.3957072899552,-16.7240831222323));
#91754=CARTESIAN_POINT('Ctrl Pts',(16.6261638663541,19.4078571848804,-16.7248121146517));
#91755=CARTESIAN_POINT('Ctrl Pts',(16.6267375498195,19.4139060984439,-16.7251743683558));
#91756=CARTESIAN_POINT('Ctrl Pts',(16.6281714408722,19.4283626123967,-16.7260385446406));
#91757=CARTESIAN_POINT('Ctrl Pts',(16.6290559728491,19.4367677377642,-16.7265396984872));
#91758=CARTESIAN_POINT('Ctrl Pts',(16.6319011461661,19.4623317995503,-16.7280601928522));
#91759=CARTESIAN_POINT('Ctrl Pts',(16.6340214751808,19.4794725053514,-16.7290745195657));
#91760=CARTESIAN_POINT('Ctrl Pts',(16.6419661856781,19.5378270006969,-16.7325118270954));
#91761=CARTESIAN_POINT('Ctrl Pts',(16.6487962625818,19.5788954588415,-16.734903562638));
#91762=CARTESIAN_POINT('Ctrl Pts',(16.6900265287536,19.7884237302569,-16.7470133525422));
#91763=CARTESIAN_POINT('Ctrl Pts',(16.7436413625375,19.9524297308197,-16.7561209159006));
#91764=CARTESIAN_POINT('Ctrl Pts',(16.8430671529535,20.1649353143168,-16.769015070992));
#91765=CARTESIAN_POINT('Ctrl Pts',(16.8721436922977,20.2205095627063,-16.772506914072));
#91766=CARTESIAN_POINT('Ctrl Pts',(16.9191779867286,20.3014431519003,-16.7778912675595));
#91767=CARTESIAN_POINT('Ctrl Pts',(16.9352983589405,20.3278336433306,-16.7796970709735));
#91768=CARTESIAN_POINT('Ctrl Pts',(16.955838015451,20.3598602033141,-16.781962996951));
#91769=CARTESIAN_POINT('Ctrl Pts',(16.9597163391459,20.3658408104971,-16.7823893955291));
#91770=CARTESIAN_POINT('Ctrl Pts',(16.9658647090614,20.3752178839487,-16.7830632886657));
#91771=CARTESIAN_POINT('Ctrl Pts',(16.9681145507912,20.3786276238563,-16.7833094512671));
#91772=CARTESIAN_POINT('Ctrl Pts',(16.9723521715327,20.3850096739091,-16.7837723398921));
#91773=CARTESIAN_POINT('Ctrl Pts',(16.9743376166432,20.387983467129,-16.7839889097274));
#91774=CARTESIAN_POINT('Ctrl Pts',(16.978905371257,20.3947876432489,-16.7844864442225));
#91775=CARTESIAN_POINT('Ctrl Pts',(16.9814926832449,20.3986146024436,-16.7847677437638));
#91776=CARTESIAN_POINT('Ctrl Pts',(16.9895487942547,20.4104469497606,-16.7856419485841));
#91777=CARTESIAN_POINT('Ctrl Pts',(16.9950599854416,20.4184231288489,-16.7862376196978));
#91778=CARTESIAN_POINT('Ctrl Pts',(17.0573284912404,20.507231829616,-16.7929389979651));
#91779=CARTESIAN_POINT('Ctrl Pts',(17.1196150372987,20.5840261716636,-16.799372258923));
#91780=CARTESIAN_POINT('Ctrl Pts',(17.3015406323331,20.7787657961343,-16.8169267070101));
#91781=CARTESIAN_POINT('Ctrl Pts',(17.4302425856269,20.8873241182522,-16.8280724108276));
#91782=CARTESIAN_POINT('Ctrl Pts',(17.5967906256836,20.9969003267764,-16.8405985654122));
#91783=CARTESIAN_POINT('Ctrl Pts',(17.6235430601663,21.0136565641113,-16.8425611858813));
#91784=CARTESIAN_POINT('Ctrl Pts',(17.6638282719996,21.0376516766322,-16.8454447101559));
#91785=CARTESIAN_POINT('Ctrl Pts',(17.6770802466514,21.04535125576,-16.8463820183829));
#91786=CARTESIAN_POINT('Ctrl Pts',(17.7013526714543,21.0591034961797,-16.8480787183859));
#91787=CARTESIAN_POINT('Ctrl Pts',(17.7123455617898,21.0652031327013,-16.8488397721356));
#91788=CARTESIAN_POINT('Ctrl Pts',(17.7297375496511,21.0746518119148,-16.8500324566828));
#91789=CARTESIAN_POINT('Ctrl Pts',(17.7361004331576,21.0780665766759,-16.8504664276954));
#91790=CARTESIAN_POINT('Ctrl Pts',(17.7425268566749,21.0814732045099,-16.8509023717785));
#91791=CARTESIAN_POINT('Ctrl Pts',(17.742572988694,21.0814976567688,-16.8509055010767));
#91792=CARTESIAN_POINT('Ctrl Pts',(17.7426668788075,21.0815474187379,-16.850911869727));
#91793=CARTESIAN_POINT('Ctrl Pts',(17.7427146380403,21.0815727288948,-16.8509151091475));
#91794=CARTESIAN_POINT('Ctrl Pts',(17.7428118417404,21.0816242375357,-16.8509217020285));
#91795=CARTESIAN_POINT('Ctrl Pts',(17.7428612873874,21.0816504364768,-16.8509250555596));
#91796=CARTESIAN_POINT('Ctrl Pts',(17.7429619255951,21.0817037548567,-16.8509318808163));
#91797=CARTESIAN_POINT('Ctrl Pts',(17.7430131189639,21.0817308745433,-16.8509353525868));
#91798=CARTESIAN_POINT('Ctrl Pts',(17.743117316422,21.0817860676683,-16.850942418619));
#91799=CARTESIAN_POINT('Ctrl Pts',(17.7431703213666,21.0818141413663,-16.850946012928));
#91800=CARTESIAN_POINT('Ctrl Pts',(17.7432782080578,21.081871276926,-16.8509533284854));
#91801=CARTESIAN_POINT('Ctrl Pts',(17.7433330906024,21.0819003390028,-16.8509570497764));
#91802=CARTESIAN_POINT('Ctrl Pts',(17.7434448009888,21.0819594869601,-16.8509646239069));
#91803=CARTESIAN_POINT('Ctrl Pts',(17.743501629632,21.0819895730421,-16.8509684767885));
#91804=CARTESIAN_POINT('Ctrl Pts',(17.7436173033879,21.0820508060135,-16.8509763188877));
#91805=CARTESIAN_POINT('Ctrl Pts',(17.7436761490008,21.0820819529285,-16.850980308126));
#91806=CARTESIAN_POINT('Ctrl Pts',(17.743795930242,21.0821453457674,-16.8509884278842));
#91807=CARTESIAN_POINT('Ctrl Pts',(17.7438568665135,21.0821775917753,-16.8509925584333));
#91808=CARTESIAN_POINT('Ctrl Pts',(17.7439809051875,21.0822432222997,-16.8510009659292));
#91809=CARTESIAN_POINT('Ctrl Pts',(17.7440440082634,21.0822766068973,-16.8510052429061));
#91810=CARTESIAN_POINT('Ctrl Pts',(17.7441724595007,21.0823445555359,-16.8510139485624));
#91811=CARTESIAN_POINT('Ctrl Pts',(17.7442378082344,21.0823791195843,-16.8510183772639));
#91812=CARTESIAN_POINT('Ctrl Pts',(17.7443708346786,21.0824494705992,-16.8510273920047));
#91813=CARTESIAN_POINT('Ctrl Pts',(17.7444385097022,21.0824852558274,-16.851031977844));
#91814=CARTESIAN_POINT('Ctrl Pts',(17.7445651187777,21.082552195442,-16.8510405567208));
#91815=CARTESIAN_POINT('Ctrl Pts',(17.7446240535157,21.0825833513263,-16.8510445498681));
#91816=CARTESIAN_POINT('Ctrl Pts',(17.7447516740642,21.0826508102924,-16.8510531964201));
#91817=CARTESIAN_POINT('Ctrl Pts',(17.7448203614933,21.0826871129543,-16.8510578498634));
#91818=CARTESIAN_POINT('Ctrl Pts',(17.7449690837388,21.0827657051226,-16.8510679249293));
#91819=CARTESIAN_POINT('Ctrl Pts',(17.745049120253,21.0828079937968,-16.8510733465706));
#91820=CARTESIAN_POINT('Ctrl Pts',(17.7452223905787,21.0828995299494,-16.8510850830394));
#91821=CARTESIAN_POINT('Ctrl Pts',(17.7453156261222,21.082948776,-16.8510913978537));
#91822=CARTESIAN_POINT('Ctrl Pts',(17.7455174346605,21.0830553499014,-16.8511050652072));
#91823=CARTESIAN_POINT('Ctrl Pts',(17.7456260093849,21.0831126754954,-16.8511124176867));
#91824=CARTESIAN_POINT('Ctrl Pts',(17.7458609668928,21.0832367028962,-16.8511283271168));
#91825=CARTESIAN_POINT('Ctrl Pts',(17.7459873511926,21.0833034012196,-16.851136883931));
#91826=CARTESIAN_POINT('Ctrl Pts',(17.7462732744956,21.0834542579886,-16.8511562402255));
#91827=CARTESIAN_POINT('Ctrl Pts',(17.7464328175309,21.0835384088572,-16.8511670394376));
#91828=CARTESIAN_POINT('Ctrl Pts',(17.7523042755597,21.0866343464138,-16.851564415543));
#91829=CARTESIAN_POINT('Ctrl Pts',(17.7580299779621,21.089620029261,-16.8519500648428));
#91830=CARTESIAN_POINT('Ctrl Pts',(17.7712868246782,21.0964558816396,-16.8528387220066));
#91831=CARTESIAN_POINT('Ctrl Pts',(17.7788275936084,21.1002872245328,-16.8533410626657));
#91832=CARTESIAN_POINT('Ctrl Pts',(17.7991801790671,21.1104750438881,-16.8546885773145));
#91833=CARTESIAN_POINT('Ctrl Pts',(17.8120339211277,21.1167471249668,-16.855530803637));
#91834=CARTESIAN_POINT('Ctrl Pts',(17.9304938537348,21.17307150822,-16.8632149735147));
#91835=CARTESIAN_POINT('Ctrl Pts',(18.0400176401703,21.2144321750125,-16.869740077917));
#91836=CARTESIAN_POINT('Ctrl Pts',(18.3090793521164,21.2913078700916,-16.8850589020573));
#91837=CARTESIAN_POINT('Ctrl Pts',(18.4703742342261,21.3178288746519,-16.893668925298));
#91838=CARTESIAN_POINT('Ctrl Pts',(18.6653332390215,21.3271322556068,-16.9048787602948));
#91839=CARTESIAN_POINT('Ctrl Pts',(18.6976032181876,21.3279331273018,-16.9067616839022));
#91840=CARTESIAN_POINT('Ctrl Pts',(18.7371006182579,21.3280100541111,-16.9091134837565));
#91841=CARTESIAN_POINT('Ctrl Pts',(18.744324293872,21.3279871488925,-16.9095455352233));
#91842=CARTESIAN_POINT('Ctrl Pts',(18.7556536680013,21.3278932376672,-16.9102263756007));
#91843=CARTESIAN_POINT('Ctrl Pts',(18.7597595962524,21.3278472556048,-16.9104737864354));
#91844=CARTESIAN_POINT('Ctrl Pts',(18.7674374186014,21.3277389308635,-16.9109377144555));
#91845=CARTESIAN_POINT('Ctrl Pts',(18.7710092974935,21.3276794924209,-16.9111540675673));
#91846=CARTESIAN_POINT('Ctrl Pts',(18.7791669391463,21.3275230889816,-16.9116493745664));
#91847=CARTESIAN_POINT('Ctrl Pts',(18.7837525324062,21.3274202614765,-16.9119286521317));
#91848=CARTESIAN_POINT('Ctrl Pts',(18.7978617023467,21.3270579976204,-16.9127905002145));
#91849=CARTESIAN_POINT('Ctrl Pts',(18.8073837372242,21.3267491783374,-16.9133757272426));
#91850=CARTESIAN_POINT('Ctrl Pts',(18.9364229332486,21.3216920366697,-16.9213521058086));
#91851=CARTESIAN_POINT('Ctrl Pts',(19.0553172939337,21.3068875165682,-16.9292201784027));
#91852=CARTESIAN_POINT('Ctrl Pts',(19.278917930622,21.2595672372516,-16.944319034537));
#91853=CARTESIAN_POINT('Ctrl Pts',(19.3836331873354,21.2288065999973,-16.9515219245795));
#91854=CARTESIAN_POINT('Ctrl Pts',(19.5556696800508,21.1634800837495,-16.9633456297866));
#91855=CARTESIAN_POINT('Ctrl Pts',(19.624359334101,21.1331295334193,-16.9680666263175));
#91856=CARTESIAN_POINT('Ctrl Pts',(19.708074147434,21.0906867550345,-16.9738164859375));
#91857=CARTESIAN_POINT('Ctrl Pts',(19.7247356953516,21.0819584601334,-16.9749608455561));
#91858=CARTESIAN_POINT('Ctrl Pts',(19.7488031797864,21.0689388268045,-16.9766142756146));
#91859=CARTESIAN_POINT('Ctrl Pts',(19.7563025588582,21.0648229849044,-16.9771295418241));
#91860=CARTESIAN_POINT('Ctrl Pts',(19.7694116718697,21.0575246443458,-16.9780304146364));
#91861=CARTESIAN_POINT('Ctrl Pts',(19.7750321554186,21.0543617781739,-16.9784167171584));
#91862=CARTESIAN_POINT('Ctrl Pts',(19.7859209692477,21.0481685309219,-16.9791652647264));
#91863=CARTESIAN_POINT('Ctrl Pts',(19.7911908701844,21.0451410528464,-16.9795276092995));
#91864=CARTESIAN_POINT('Ctrl Pts',(19.8037628120906,21.0378464773464,-16.9803922250094));
#91865=CARTESIAN_POINT('Ctrl Pts',(19.8110524998835,21.0335582134938,-16.9808937256131));
#91866=CARTESIAN_POINT('Ctrl Pts',(19.837294313774,21.0179086609543,-16.9826998326179));
#91867=CARTESIAN_POINT('Ctrl Pts',(19.8560943942174,21.0062942590332,-16.9839952146785));
#91868=CARTESIAN_POINT('Ctrl Pts',(20.0311361676866,20.8943321224197,-16.9960802195306));
#91869=CARTESIAN_POINT('Ctrl Pts',(20.1737155331028,20.7741360980852,-17.0060121270811));
#91870=CARTESIAN_POINT('Ctrl Pts',(20.3527273144784,20.5776831764974,-17.0205012281641));
#91871=CARTESIAN_POINT('Ctrl Pts',(20.4032549682087,20.5154872064165,-17.024905025784));
#91872=CARTESIAN_POINT('Ctrl Pts',(20.4712211668354,20.4213918739281,-17.0315447344727));
#91873=CARTESIAN_POINT('Ctrl Pts',(20.4915579013346,20.3916675003225,-17.0336394527146));
#91874=CARTESIAN_POINT('Ctrl Pts',(20.5151821105899,20.3551743824452,-17.0362265466963));
#91875=CARTESIAN_POINT('Ctrl Pts',(20.5192056544858,20.3488864161047,-17.0366728563519));
#91876=CARTESIAN_POINT('Ctrl Pts',(20.5254189006928,20.3390623299429,-17.037371205983));
#91877=CARTESIAN_POINT('Ctrl Pts',(20.5276316270342,20.3355407435103,-17.0376217485581));
#91878=CARTESIAN_POINT('Ctrl Pts',(20.5317222036078,20.3289877434587,-17.0380883923686));
#91879=CARTESIAN_POINT('Ctrl Pts',(20.533602777282,20.325958097536,-17.0383043101056));
#91880=CARTESIAN_POINT('Ctrl Pts',(20.5378449576885,20.3190851576459,-17.0387945218359));
#91881=CARTESIAN_POINT('Ctrl Pts',(20.5402019285213,20.3152390776044,-17.0390691134711));
#91882=CARTESIAN_POINT('Ctrl Pts',(20.546256291654,20.305288385517,-17.0397801815962));
#91883=CARTESIAN_POINT('Ctrl Pts',(20.5499351028077,20.2991726133277,-17.0402178254077));
#91884=CARTESIAN_POINT('Ctrl Pts',(20.5723467300015,20.2614846619987,-17.0429179787807));
#91885=CARTESIAN_POINT('Ctrl Pts',(20.5902853875496,20.2294502491368,-17.0452267902693));
#91886=CARTESIAN_POINT('Ctrl Pts',(20.6867169475803,20.0462262154028,-17.0584408035116));
#91887=CARTESIAN_POINT('Ctrl Pts',(20.7475691642428,19.8864617645616,-17.0699344876168));
#91888=CARTESIAN_POINT('Ctrl Pts',(20.8116284924949,19.6284529161769,-17.0872115337993));
#91889=CARTESIAN_POINT('Ctrl Pts',(20.8283440005247,19.5343180509846,-17.093278696753));
#91890=CARTESIAN_POINT('Ctrl Pts',(20.8409558166998,19.4180852872211,-17.1004603553849));
#91891=CARTESIAN_POINT('Ctrl Pts',(20.8429419159826,19.3967718426598,-17.1017650198563));
#91892=CARTESIAN_POINT('Ctrl Pts',(20.8453044674437,19.3664466464373,-17.1036045693131));
#91893=CARTESIAN_POINT('Ctrl Pts',(20.8459470682652,19.3574574986415,-17.1041477736253));
#91894=CARTESIAN_POINT('Ctrl Pts',(20.8469560605195,19.3419514584894,-17.1050812699915));
#91895=CARTESIAN_POINT('Ctrl Pts',(20.8473497464858,19.3354365246846,-17.1054724136768));
#91896=CARTESIAN_POINT('Ctrl Pts',(20.8480455185504,19.3229648070265,-17.1062191818024));
#91897=CARTESIAN_POINT('Ctrl Pts',(20.8483525719362,19.3170083731765,-17.1065749584272));
#91898=CARTESIAN_POINT('Ctrl Pts',(20.849084946768,19.3015291665882,-17.1074972936121));
#91899=CARTESIAN_POINT('Ctrl Pts',(20.8494711342402,19.2920046095096,-17.1080626214963));
#91900=CARTESIAN_POINT('Ctrl Pts',(20.8505663755161,19.2595846314874,-17.1099796755452));
#91901=CARTESIAN_POINT('Ctrl Pts',(20.8509681832544,19.2366799480955,-17.1113217929126));
#91902=CARTESIAN_POINT('Ctrl Pts',(20.8512294839296,19.0371639492722,-17.1229163549525));
#91903=CARTESIAN_POINT('Ctrl Pts',(20.8293620856766,18.8612228780746,-17.1324065973639));
#91904=CARTESIAN_POINT('Ctrl Pts',(20.7646788927514,18.6064626451888,-17.1467107748272));
#91905=CARTESIAN_POINT('Ctrl Pts',(20.7383786067801,18.5242786371518,-17.1514330993186));
#91906=CARTESIAN_POINT('Ctrl Pts',(20.6935122575157,18.4088677197828,-17.1585042895766));
#91907=CARTESIAN_POINT('Ctrl Pts',(20.678948685082,18.374173434108,-17.1606900291397));
#91908=CARTESIAN_POINT('Ctrl Pts',(20.6603586941051,18.3329975291665,-17.163378060292));
#91909=CARTESIAN_POINT('Ctrl Pts',(20.6572109417736,18.326123835399,-17.1638299847379));
#91910=CARTESIAN_POINT('Ctrl Pts',(20.6522658673023,18.3154763917768,-17.1645352232892));
#91911=CARTESIAN_POINT('Ctrl Pts',(20.6504940359422,18.3116907761807,-17.1647869918207));
#91912=CARTESIAN_POINT('Ctrl Pts',(20.647190659324,18.3046870280305,-17.1652547367467));
#91913=CARTESIAN_POINT('Ctrl Pts',(20.6456621941976,18.3014675064759,-17.1654705221608));
#91914=CARTESIAN_POINT('Ctrl Pts',(20.6421925989564,18.2942066177321,-17.1659589123766));
#91915=CARTESIAN_POINT('Ctrl Pts',(20.6402467672974,18.2901675712732,-17.1662318053479));
#91916=CARTESIAN_POINT('Ctrl Pts',(20.6344782328566,18.2782902171649,-17.1670377967522));
#91917=CARTESIAN_POINT('Ctrl Pts',(20.6306199633149,18.2704694256415,-17.1675730322893));
#91918=CARTESIAN_POINT('Ctrl Pts',(20.6028094843568,18.2149640330731,-17.171402770531));
#91919=CARTESIAN_POINT('Ctrl Pts',(20.5771121655385,18.1681802435231,-17.1747943985693));
#91920=CARTESIAN_POINT('Ctrl Pts',(20.5406293835266,18.1073293425063,-17.1793798479116));
#91921=CARTESIAN_POINT('Ctrl Pts',(20.5313932850883,18.0923508127367,-17.1805231535638));
#91922=CARTESIAN_POINT('Ctrl Pts',(20.4960017766648,18.0365251151155,-17.18483514981));
#91923=CARTESIAN_POINT('Ctrl Pts',(20.4686323362891,17.9964663709702,-17.1880325966352));
#91924=CARTESIAN_POINT('Ctrl Pts',(20.3751392973078,17.8692416741765,-17.19846191336));
#91925=CARTESIAN_POINT('Ctrl Pts',(20.3036275044895,17.7862450873941,-17.2056947123692));
#91926=CARTESIAN_POINT('Ctrl Pts',(20.1869266995004,17.6703088638426,-17.2162683604883));
#91927=CARTESIAN_POINT('Ctrl Pts',(20.1463326070025,17.6330131181074,-17.2197575867501));
#91928=CARTESIAN_POINT('Ctrl Pts',(20.0781788366405,17.5751366184986,-17.2253152820729));
#91929=CARTESIAN_POINT('Ctrl Pts',(20.0514942437143,17.5535697957619,-17.2274221920438));
#91930=CARTESIAN_POINT('Ctrl Pts',(20.0157271157714,17.5260722791464,-17.2301587689651));
#91931=CARTESIAN_POINT('Ctrl Pts',(20.0071077751816,17.519550200756,-17.230811778265));
#91932=CARTESIAN_POINT('Ctrl Pts',(19.992906284514,17.5089742805748,-17.2318772838336));
#91933=CARTESIAN_POINT('Ctrl Pts',(19.9873536792914,17.5048812646441,-17.2322913095779));
#91934=CARTESIAN_POINT('Ctrl Pts',(19.9765651487209,17.4970097606554,-17.2330908254781));
#91935=CARTESIAN_POINT('Ctrl Pts',(19.971331754115,17.4932279484552,-17.2334764419846));
#91936=CARTESIAN_POINT('Ctrl Pts',(19.9592058782948,17.4845495848669,-17.2343648594301));
#91937=CARTESIAN_POINT('Ctrl Pts',(19.9523011729783,17.4796702407674,-17.2348669943182));
#91938=CARTESIAN_POINT('Ctrl Pts',(19.9336483181675,17.466655680199,-17.2362135926313));
#91939=CARTESIAN_POINT('Ctrl Pts',(19.9218465970028,17.4585977430387,-17.23705511473));
#91940=CARTESIAN_POINT('Ctrl Pts',(19.8128219796707,17.3857657871692,-17.244736205846));
#91941=CARTESIAN_POINT('Ctrl Pts',(19.7104693969057,17.329019773098,-17.2512591646177));
#91942=CARTESIAN_POINT('Ctrl Pts',(19.4555750118391,17.2141262805561,-17.2665653516512));
#91943=CARTESIAN_POINT('Ctrl Pts',(19.300007055965,17.1645886759212,-17.2751654880419));
#91944=CARTESIAN_POINT('Ctrl Pts',(19.1084203759755,17.1271201854677,-17.2863745074836));
#91945=CARTESIAN_POINT('Ctrl Pts',(19.0763803121059,17.1216170384523,-17.2882704642959));
#91946=CARTESIAN_POINT('Ctrl Pts',(19.0370669393538,17.1157931269504,-17.2906367648735));
#91947=CARTESIAN_POINT('Ctrl Pts',(19.0299002993836,17.1147689965118,-17.2910697459533));
#91948=CARTESIAN_POINT('Ctrl Pts',(19.0186573899362,17.113221160417,-17.2917517285284));
#91949=CARTESIAN_POINT('Ctrl Pts',(19.014584530552,17.1126725207913,-17.2919993442989));
#91950=CARTESIAN_POINT('Ctrl Pts',(19.0069687910067,17.1116692023527,-17.2924634454415));
#91951=CARTESIAN_POINT('Ctrl Pts',(19.0034263488704,17.1112116295464,-17.2926797654534));
#91952=CARTESIAN_POINT('Ctrl Pts',(18.9953375040211,17.1101876096167,-17.2931747180546));
#91953=CARTESIAN_POINT('Ctrl Pts',(18.990790425775,17.109626956746,-17.2934536725306));
#91954=CARTESIAN_POINT('Ctrl Pts',(18.9768088411896,17.1079490911507,-17.2943135554647));
#91955=CARTESIAN_POINT('Ctrl Pts',(18.9673687567909,17.1068806416475,-17.2948971232507));
#91956=CARTESIAN_POINT('Ctrl Pts',(18.8825088768579,17.0978540985116,-17.3001679133913));
#91957=CARTESIAN_POINT('Ctrl Pts',(18.8067270609206,17.0938914242035,-17.3050498675469));
#91958=CARTESIAN_POINT('Ctrl Pts',(18.5459833782494,17.0942725845345,-17.3221028197883));
#91959=CARTESIAN_POINT('Ctrl Pts',(18.3618541881496,17.1187733034733,-17.3344995710412));
#91960=CARTESIAN_POINT('Ctrl Pts',(18.1318211789033,17.1807521451726,-17.3495264498624));
#91961=CARTESIAN_POINT('Ctrl Pts',(18.0809325868206,17.1965448783824,-17.3528279687531));
#91962=CARTESIAN_POINT('Ctrl Pts',(18.0188618052271,17.2184078119572,-17.3568295781235));
#91963=CARTESIAN_POINT('Ctrl Pts',(18.0070705909193,17.222679122904,-17.3575886262899));
#91964=CARTESIAN_POINT('Ctrl Pts',(17.9884944114631,17.2295955912846,-17.3587828512243));
#91965=CARTESIAN_POINT('Ctrl Pts',(17.9816840852419,17.2321713616683,-17.3592203317231));
#91966=CARTESIAN_POINT('Ctrl Pts',(17.9689419667816,17.2370659165558,-17.3600382628031));
#91967=CARTESIAN_POINT('Ctrl Pts',(17.9630071032306,17.2393764267801,-17.3604189852731));
#91968=CARTESIAN_POINT('Ctrl Pts',(17.9497498540491,17.244606639461,-17.3612689366474));
#91969=CARTESIAN_POINT('Ctrl Pts',(17.9424331431518,17.2475405393779,-17.3617376817351));
#91970=CARTESIAN_POINT('Ctrl Pts',(17.9239377700824,17.2550771167157,-17.3629218105322));
#91971=CARTESIAN_POINT('Ctrl Pts',(17.9127817374088,17.2597348422183,-17.3636353286591));
#91972=CARTESIAN_POINT('Ctrl Pts',(17.8493600421741,17.2868541353214,-17.3676884300711));
#91973=CARTESIAN_POINT('Ctrl Pts',(17.797973941112,17.3113207609099,-17.3709589032607));
#91974=CARTESIAN_POINT('Ctrl Pts',(17.7238750783338,17.3503394861406,-17.3756896543121));
#91975=CARTESIAN_POINT('Ctrl Pts',(17.7003574662086,17.3633005961775,-17.3771935453424));
#91976=CARTESIAN_POINT('Ctrl Pts',(17.5767175020271,17.4345411033099,-17.3851308845967));
#91977=CARTESIAN_POINT('Ctrl Pts',(17.481259711552,17.500517160423,-17.3913557726303));
#91978=CARTESIAN_POINT('Ctrl Pts',(17.3297861141352,17.6247218640124,-17.4020346734756));
#91979=CARTESIAN_POINT('Ctrl Pts',(17.2708275916785,17.6789362073988,-17.4064365018023));
#91980=CARTESIAN_POINT('Ctrl Pts',(17.1900064510278,17.7621835671349,-17.4130735323533));
#91981=CARTESIAN_POINT('Ctrl Pts',(17.165593140646,17.7886481760463,-17.4151676727849));
#91982=CARTESIAN_POINT('Ctrl Pts',(17.1369483323212,17.8213343243613,-17.4177541257169));
#91983=CARTESIAN_POINT('Ctrl Pts',(17.1320583903991,17.8269740627617,-17.4182003988007));
#91984=CARTESIAN_POINT('Ctrl Pts',(17.1244906025232,17.8357960891903,-17.4188987035491));
#91985=CARTESIAN_POINT('Ctrl Pts',(17.1217920799543,17.8389606715801,-17.4191492381247));
#91986=CARTESIAN_POINT('Ctrl Pts',(17.1167971617542,17.8448533402538,-17.4196158748166));
#91987=CARTESIAN_POINT('Ctrl Pts',(17.1144983275154,17.8475792842341,-17.4198317934835));
#91988=CARTESIAN_POINT('Ctrl Pts',(17.1093069381485,17.8537668570215,-17.4203220174013));
#91989=CARTESIAN_POINT('Ctrl Pts',(17.1064185682556,17.8572319135843,-17.420596620357));
#91990=CARTESIAN_POINT('Ctrl Pts',(17.0978965703123,17.8675220925263,-17.4214122651026));
#91991=CARTESIAN_POINT('Ctrl Pts',(17.0922947221149,17.8743732402815,-17.4219555195858));
#91992=CARTESIAN_POINT('Ctrl Pts',(17.0511032547075,17.9254006400831,-17.4260018821648));
#91993=CARTESIAN_POINT('Ctrl Pts',(17.0172623091447,17.9709525606907,-17.4296146850004));
#91994=CARTESIAN_POINT('Ctrl Pts',(16.9504046662844,18.0689366960563,-17.4372973740587));
#91995=CARTESIAN_POINT('Ctrl Pts',(16.9177757210432,18.121573692312,-17.4413750532935));
#91996=CARTESIAN_POINT('Ctrl Pts',(16.8338946484414,18.2711590250988,-17.4527032244226));
#91997=CARTESIAN_POINT('Ctrl Pts',(16.7877887173321,18.3707818688211,-17.4599518050173));
#91998=CARTESIAN_POINT('Ctrl Pts',(16.7481977230133,18.4773143771053,-17.4672585705686));
#91999=CARTESIAN_POINT('Ctrl Pts',(16.7468031572123,18.4811000183989,-17.467517671245));
#92000=CARTESIAN_POINT('Ctrl Pts',(16.7454194505834,18.4848895411289,-17.4677764891862));
#92001=CARTESIAN_POINT('',(16.6170006442198,19.2126515526684,-16.4878149140766));
#92002=CARTESIAN_POINT('Ctrl Pts',(16.7454194502294,18.4848895420984,-17.2426989706651));
#92003=CARTESIAN_POINT('Ctrl Pts',(16.7608133382974,18.4427306858745,-17.2398827653555));
#92004=CARTESIAN_POINT('Ctrl Pts',(16.7775450772477,18.4010690881806,-17.2371085333092));
#92005=CARTESIAN_POINT('Ctrl Pts',(16.8006203765564,18.348510109161,-17.2336175690097));
#92006=CARTESIAN_POINT('Ctrl Pts',(16.8057522413298,18.3370971610802,-17.2328600437446));
#92007=CARTESIAN_POINT('Ctrl Pts',(16.8140577699586,18.3190555931353,-17.2316632154219));
#92008=CARTESIAN_POINT('Ctrl Pts',(16.8171652140291,18.3123969747177,-17.231221645671));
#92009=CARTESIAN_POINT('Ctrl Pts',(16.8230280590362,18.300002894862,-17.2303999489647));
#92010=CARTESIAN_POINT('Ctrl Pts',(16.8257747635082,18.2942634332026,-17.2300195267569));
#92011=CARTESIAN_POINT('Ctrl Pts',(16.8319433148342,18.2815215943543,-17.2291751329545));
#92012=CARTESIAN_POINT('Ctrl Pts',(16.8353780490106,18.2745255316601,-17.2287116157621));
#92013=CARTESIAN_POINT('Ctrl Pts',(16.8455036916209,18.2541857493234,-17.2273642277309));
#92014=CARTESIAN_POINT('Ctrl Pts',(16.8522972775032,18.2408934603478,-17.2264839544724));
#92015=CARTESIAN_POINT('Ctrl Pts',(16.9092402982048,18.1323282483482,-17.2192939179738));
#92016=CARTESIAN_POINT('Ctrl Pts',(16.9664531679667,18.0409301958476,-17.2132499565895));
#92017=CARTESIAN_POINT('Ctrl Pts',(17.1097520567792,17.8466741581555,-17.1999842903702));
#92018=CARTESIAN_POINT('Ctrl Pts',(17.1991353481694,17.7468436069552,-17.1928656003642));
#92019=CARTESIAN_POINT('Ctrl Pts',(17.3093863068514,17.6449750294365,-17.1845197252994));
#92020=CARTESIAN_POINT('Ctrl Pts',(17.3215700997975,17.6339774445076,-17.1836024509762));
#92021=CARTESIAN_POINT('Ctrl Pts',(17.373685192635,17.5880246656061,-17.1796940129411));
#92022=CARTESIAN_POINT('Ctrl Pts',(17.4147922967863,17.5544386995924,-17.1766482377681));
#92023=CARTESIAN_POINT('Ctrl Pts',(17.4640563103417,17.5171854327889,-17.1729828821949));
#92024=CARTESIAN_POINT('Ctrl Pts',(17.4710311400996,17.5119783944767,-17.1724635938947));
#92025=CARTESIAN_POINT('Ctrl Pts',(17.4816439665743,17.5041568806896,-17.1716725980688));
#92026=CARTESIAN_POINT('Ctrl Pts',(17.4852585760779,17.5015106248567,-17.1714030453901));
#92027=CARTESIAN_POINT('Ctrl Pts',(17.491763703779,17.4967798610813,-17.1709176182842));
#92028=CARTESIAN_POINT('Ctrl Pts',(17.4946511079854,17.4946911630227,-17.1707020387784));
#92029=CARTESIAN_POINT('Ctrl Pts',(17.5009388108367,17.49016688858,-17.1702323249346));
#92030=CARTESIAN_POINT('Ctrl Pts',(17.5043410130771,17.4877341270827,-17.1699780083776));
#92031=CARTESIAN_POINT('Ctrl Pts',(17.5139234946811,17.4809249523921,-17.1692613162666));
#92032=CARTESIAN_POINT('Ctrl Pts',(17.5201200075639,17.4765716477264,-17.1687974061867));
#92033=CARTESIAN_POINT('Ctrl Pts',(17.5574223496223,17.4506630320028,-17.1660026203623));
#92034=CARTESIAN_POINT('Ctrl Pts',(17.5890762148143,17.4299131621867,-17.1636224139565));
#92035=CARTESIAN_POINT('Ctrl Pts',(17.6953532907791,17.3642498466803,-17.1556463338188));
#92036=CARTESIAN_POINT('Ctrl Pts',(17.7721892209598,17.3230934286936,-17.1499073692223));
#92037=CARTESIAN_POINT('Ctrl Pts',(18.0106984254139,17.2136857130653,-17.132569870025));
#92038=CARTESIAN_POINT('Ctrl Pts',(18.1785591328292,17.1606492070527,-17.1210593283118));
#92039=CARTESIAN_POINT('Ctrl Pts',(18.3736830972609,17.1247618207071,-17.1088475343449));
#92040=CARTESIAN_POINT('Ctrl Pts',(18.3963708884204,17.1209701773303,-17.107443440555));
#92041=CARTESIAN_POINT('Ctrl Pts',(18.4285581222713,17.1161287827881,-17.1054730735289));
#92042=CARTESIAN_POINT('Ctrl Pts',(18.4380091714817,17.1147725334597,-17.1048971425516));
#92043=CARTESIAN_POINT('Ctrl Pts',(18.4533813600868,17.1126726220892,-17.1039645617273));
#92044=CARTESIAN_POINT('Ctrl Pts',(18.4592969594628,17.1118899870161,-17.1036066837254));
#92045=CARTESIAN_POINT('Ctrl Pts',(18.4716873046522,17.1103040163012,-17.1028591677689));
#92046=CARTESIAN_POINT('Ctrl Pts',(18.4781626227438,17.1095055784187,-17.1024696881781));
#92047=CARTESIAN_POINT('Ctrl Pts',(18.49357731391,17.1076771758321,-17.1015452762753));
#92048=CARTESIAN_POINT('Ctrl Pts',(18.5025198127061,17.1066742416274,-17.101011201296));
#92049=CARTESIAN_POINT('Ctrl Pts',(18.5326744199962,17.1034868388343,-17.099217483476));
#92050=CARTESIAN_POINT('Ctrl Pts',(18.5539134972714,17.1015658071187,-17.0979661247632));
#92051=CARTESIAN_POINT('Ctrl Pts',(18.6697332462445,17.0928522295383,-17.091202430274));
#92052=CARTESIAN_POINT('Ctrl Pts',(18.7646647782039,17.0920986580974,-17.0858833027061));
#92053=CARTESIAN_POINT('Ctrl Pts',(19.0285280222344,17.1077480484148,-17.0713394145862));
#92054=CARTESIAN_POINT('Ctrl Pts',(19.195882176884,17.1380627443865,-17.0624207447181));
#92055=CARTESIAN_POINT('Ctrl Pts',(19.3943158318376,17.199251722985,-17.0505775159879));
#92056=CARTESIAN_POINT('Ctrl Pts',(19.4305044825888,17.2114927541701,-17.0483610744069));
#92057=CARTESIAN_POINT('Ctrl Pts',(19.473120199167,17.2272050112181,-17.0456612971868));
#92058=CARTESIAN_POINT('Ctrl Pts',(19.4798878362058,17.2297396539709,-17.0452298279612));
#92059=CARTESIAN_POINT('Ctrl Pts',(19.4908839492304,17.2339222871765,-17.0445241194717));
#92060=CARTESIAN_POINT('Ctrl Pts',(19.495120401348,17.2355493352358,-17.0442511029315));
#92061=CARTESIAN_POINT('Ctrl Pts',(19.5026782732002,17.2384799257266,-17.0437619632272));
#92062=CARTESIAN_POINT('Ctrl Pts',(19.5060016587068,17.239778254534,-17.0435461546909));
#92063=CARTESIAN_POINT('Ctrl Pts',(19.5131735701707,17.2426009850688,-17.0430788625902));
#92064=CARTESIAN_POINT('Ctrl Pts',(19.517020857971,17.2441282528494,-17.0428272125963));
#92065=CARTESIAN_POINT('Ctrl Pts',(19.5277101679921,17.2484079489913,-17.042125358408));
#92066=CARTESIAN_POINT('Ctrl Pts',(19.5345422464008,17.2511848307807,-17.0416737180217));
#92067=CARTESIAN_POINT('Ctrl Pts',(19.5733072090948,17.2671772784661,-17.0390943254087));
#92068=CARTESIAN_POINT('Ctrl Pts',(19.6049252570322,17.2811367297378,-17.0369255078848));
#92069=CARTESIAN_POINT('Ctrl Pts',(19.7038701346755,17.3277478083891,-17.0299625078815));
#92070=CARTESIAN_POINT('Ctrl Pts',(19.769812612359,17.3631965499211,-17.0250600376702));
#92071=CARTESIAN_POINT('Ctrl Pts',(19.999415570089,17.5027823087797,-17.0073370682358));
#92072=CARTESIAN_POINT('Ctrl Pts',(20.1505137405041,17.6258171798855,-16.9945246047959));
#92073=CARTESIAN_POINT('Ctrl Pts',(20.297180975354,17.7832038609921,-16.9813072130045));
#92074=CARTESIAN_POINT('Ctrl Pts',(20.3113717392771,17.7988969501502,-16.9800172853959));
#92075=CARTESIAN_POINT('Ctrl Pts',(20.3308021890409,17.8210429028221,-16.978234831391));
#92076=CARTESIAN_POINT('Ctrl Pts',(20.3362423662733,17.8273174620911,-16.9777339460917));
#92077=CARTESIAN_POINT('Ctrl Pts',(20.3455737304454,17.838208842062,-16.9768715528553));
#92078=CARTESIAN_POINT('Ctrl Pts',(20.3494823173193,17.8428105629785,-16.9765093273947));
#92079=CARTESIAN_POINT('Ctrl Pts',(20.3575399292169,17.8523797489023,-16.9757604838787));
#92080=CARTESIAN_POINT('Ctrl Pts',(20.3616859720391,17.8573496513807,-16.975373990376));
#92081=CARTESIAN_POINT('Ctrl Pts',(20.3713503100389,17.8690429902778,-16.974470263144));
#92082=CARTESIAN_POINT('Ctrl Pts',(20.3768501164111,17.8757816088079,-16.9739537837821));
#92083=CARTESIAN_POINT('Ctrl Pts',(20.394606741979,17.8978136624232,-16.9722789481775));
#92084=CARTESIAN_POINT('Ctrl Pts',(20.4066929776906,17.9132437250251,-16.9711274301937));
#92085=CARTESIAN_POINT('Ctrl Pts',(20.4676175746711,17.9932893794753,-16.9652588531404));
#92086=CARTESIAN_POINT('Ctrl Pts',(20.5129356569166,18.0605048674188,-16.9606804075939));
#92087=CARTESIAN_POINT('Ctrl Pts',(20.6403814937926,18.2751421311587,-16.9468447557961));
#92088=CARTESIAN_POINT('Ctrl Pts',(20.7088316391719,18.4298773210331,-16.9379726523065));
#92089=CARTESIAN_POINT('Ctrl Pts',(20.7740144561736,18.6427162789224,-16.9254609686511));
#92090=CARTESIAN_POINT('Ctrl Pts',(20.787845243202,18.6949340812579,-16.9223636359522));
#92091=CARTESIAN_POINT('Ctrl Pts',(20.8015778125553,18.7561511672814,-16.9186407333664));
#92092=CARTESIAN_POINT('Ctrl Pts',(20.8034390016764,18.7646955254871,-16.9181190531254));
#92093=CARTESIAN_POINT('Ctrl Pts',(20.8061752909591,18.7776425143841,-16.9173251229311));
#92094=CARTESIAN_POINT('Ctrl Pts',(20.8070894391582,18.7820369209381,-16.9170550518218));
#92095=CARTESIAN_POINT('Ctrl Pts',(20.8087044242035,18.7899260675077,-16.9165690733248));
#92096=CARTESIAN_POINT('Ctrl Pts',(20.8094104160417,18.793419697391,-16.9163534638132));
#92097=CARTESIAN_POINT('Ctrl Pts',(20.8109243812277,18.8010103023265,-16.9158841317804));
#92098=CARTESIAN_POINT('Ctrl Pts',(20.8117290458402,18.8051078358564,-16.9156302294797));
#92099=CARTESIAN_POINT('Ctrl Pts',(20.8139530056626,18.8166126562977,-16.9149158490997));
#92100=CARTESIAN_POINT('Ctrl Pts',(20.8153448309229,18.824025099657,-16.9144538520078));
#92101=CARTESIAN_POINT('Ctrl Pts',(20.8233859748052,18.8681484879154,-16.9116941377102));
#92102=CARTESIAN_POINT('Ctrl Pts',(20.8291030668226,18.9050201708442,-16.909348489043));
#92103=CARTESIAN_POINT('Ctrl Pts',(20.8446409571895,19.0263200153417,-16.9015442361564));
#92104=CARTESIAN_POINT('Ctrl Pts',(20.8503524223027,19.111187630202,-16.8959487214791));
#92105=CARTESIAN_POINT('Ctrl Pts',(20.8521980299003,19.3745107904806,-16.8785530615524));
#92106=CARTESIAN_POINT('Ctrl Pts',(20.8309048315297,19.5523405823664,-16.866831316198));
#92107=CARTESIAN_POINT('Ctrl Pts',(20.7820180809691,19.7474971384358,-16.8544506656616));
#92108=CARTESIAN_POINT('Ctrl Pts',(20.7761303999908,19.7694896887762,-16.8530611502229));
#92109=CARTESIAN_POINT('Ctrl Pts',(20.7672820275648,19.8005282998256,-16.8511075050183));
#92110=CARTESIAN_POINT('Ctrl Pts',(20.7646135002302,19.8096553576232,-16.8505339383858));
#92111=CARTESIAN_POINT('Ctrl Pts',(20.7601724701446,19.8244734254388,-16.8496041398287));
#92112=CARTESIAN_POINT('Ctrl Pts',(20.7584372914539,19.8301754005053,-16.8492466942338));
#92113=CARTESIAN_POINT('Ctrl Pts',(20.7547504591449,19.84210952208,-16.8484992507435));
#92114=CARTESIAN_POINT('Ctrl Pts',(20.7527939990759,19.8483401272186,-16.8481094148603));
#92115=CARTESIAN_POINT('Ctrl Pts',(20.7480629092415,19.8631665288297,-16.8471826438304));
#92116=CARTESIAN_POINT('Ctrl Pts',(20.74526202201,19.8717538621746,-16.8466465778249));
#92117=CARTESIAN_POINT('Ctrl Pts',(20.7356005815914,19.9007444899207,-16.8448390400018));
#92118=CARTESIAN_POINT('Ctrl Pts',(20.72848369125,19.9210614094748,-16.8435760300224));
#92119=CARTESIAN_POINT('Ctrl Pts',(20.65877648858,20.1107348947486,-16.8318107390562));
#92120=CARTESIAN_POINT('Ctrl Pts',(20.5750744889951,20.2715371396014,-16.8221162571427));
#92121=CARTESIAN_POINT('Ctrl Pts',(20.4038334576143,20.5177463402424,-16.8057909893335));
#92122=CARTESIAN_POINT('Ctrl Pts',(20.3275426677446,20.6097649082873,-16.7992390617861));
#92123=CARTESIAN_POINT('Ctrl Pts',(20.2372569729471,20.7016367454378,-16.7916051806598));
#92124=CARTESIAN_POINT('Ctrl Pts',(20.230545949909,20.7083742503944,-16.7910383510971));
#92125=CARTESIAN_POINT('Ctrl Pts',(20.2205335648251,20.718291600122,-16.7901931457129));
#92126=CARTESIAN_POINT('Ctrl Pts',(20.2172667945473,20.7215064125772,-16.7899174505304));
#92127=CARTESIAN_POINT('Ctrl Pts',(20.2114355004931,20.7272078029677,-16.7894253969436));
#92128=CARTESIAN_POINT('Ctrl Pts',(20.2088750976532,20.7296985237336,-16.7892093683627));
#92129=CARTESIAN_POINT('Ctrl Pts',(20.2033561957336,20.7350401076278,-16.7887437542423));
#92130=CARTESIAN_POINT('Ctrl Pts',(20.2003957414283,20.7378888002918,-16.7884940137176));
#92131=CARTESIAN_POINT('Ctrl Pts',(20.1921997568507,20.7457295530085,-16.7878027263656));
#92132=CARTESIAN_POINT('Ctrl Pts',(20.1869469595464,20.7507033678675,-16.7873598115959));
#92133=CARTESIAN_POINT('Ctrl Pts',(20.1580085252817,20.7778248957362,-16.7849209651063));
#92134=CARTESIAN_POINT('Ctrl Pts',(20.1338432734866,20.799451786185,-16.7828889395332));
#92135=CARTESIAN_POINT('Ctrl Pts',(19.9854221093857,20.9262650367634,-16.7704852827918));
#92136=CARTESIAN_POINT('Ctrl Pts',(19.8498706098471,21.0173842724899,-16.7595219761107));
#92137=CARTESIAN_POINT('Ctrl Pts',(19.6013597780351,21.1456932529202,-16.7412532752891));
#92138=CARTESIAN_POINT('Ctrl Pts',(19.4932263134805,21.1906298122628,-16.733807804058));
#92139=CARTESIAN_POINT('Ctrl Pts',(19.368338526942,21.2307789780287,-16.7257980463268));
#92140=CARTESIAN_POINT('Ctrl Pts',(19.3547141305646,21.2350075273089,-16.7249315762956));
#92141=CARTESIAN_POINT('Ctrl Pts',(19.3329550908196,21.2415204155779,-16.7235591941654));
#92142=CARTESIAN_POINT('Ctrl Pts',(19.3248478987339,21.2438942723837,-16.7230503667555));
#92143=CARTESIAN_POINT('Ctrl Pts',(19.3105204456,21.2479965267566,-16.7221554924122));
#92144=CARTESIAN_POINT('Ctrl Pts',(19.3043061211828,21.2497451051533,-16.7217687916749));
#92145=CARTESIAN_POINT('Ctrl Pts',(19.2914323810326,21.2533040331069,-16.7209706262376));
#92146=CARTESIAN_POINT('Ctrl Pts',(19.2847719094458,21.2551103024464,-16.7205592981371));
#92147=CARTESIAN_POINT('Ctrl Pts',(19.2676443872167,21.2596653654501,-16.7195056451325));
#92148=CARTESIAN_POINT('Ctrl Pts',(19.2571647944896,21.2623665484237,-16.718864866956));
#92149=CARTESIAN_POINT('Ctrl Pts',(19.2132694495572,21.2733226036583,-16.7161967129957));
#92150=CARTESIAN_POINT('Ctrl Pts',(19.179674500919,21.2808425458438,-16.7141930353365));
#92151=CARTESIAN_POINT('Ctrl Pts',(19.0916087532639,21.2983115691613,-16.7090282608772));
#92152=CARTESIAN_POINT('Ctrl Pts',(19.0369038015083,21.3069493188486,-16.7059069700503));
#92153=CARTESIAN_POINT('Ctrl Pts',(18.8731169370877,21.3262631490915,-16.6967386112696));
#92154=CARTESIAN_POINT('Ctrl Pts',(18.7634791437289,21.3306281634368,-16.6908401907265));
#92155=CARTESIAN_POINT('Ctrl Pts',(18.5938540381529,21.3242132902009,-16.6815973286925));
#92156=CARTESIAN_POINT('Ctrl Pts',(18.533838412007,21.3193752020727,-16.6783017826909));
#92157=CARTESIAN_POINT('Ctrl Pts',(18.4161480307497,21.3048172135664,-16.6716596722049));
#92158=CARTESIAN_POINT('Ctrl Pts',(18.3585095813221,21.2952519143196,-16.6683201738073));
#92159=CARTESIAN_POINT('Ctrl Pts',(18.292623443894,21.2814963502925,-16.6643275082868));
#92160=CARTESIAN_POINT('Ctrl Pts',(18.2839125603699,21.2796202385259,-16.6637960575681));
#92161=CARTESIAN_POINT('Ctrl Pts',(18.2707974233826,21.2767087984518,-16.6629901508239));
#92162=CARTESIAN_POINT('Ctrl Pts',(18.2663840937811,21.2757142248661,-16.6627179729499));
#92163=CARTESIAN_POINT('Ctrl Pts',(18.2584969040207,21.2739102085808,-16.662229738127));
#92164=CARTESIAN_POINT('Ctrl Pts',(18.2550218717433,21.2731061261093,-16.6620139910414));
#92165=CARTESIAN_POINT('Ctrl Pts',(18.2475085531926,21.2713476139634,-16.6615461397746));
#92166=CARTESIAN_POINT('Ctrl Pts',(18.2434710919051,21.2703901057891,-16.661293865448));
#92167=CARTESIAN_POINT('Ctrl Pts',(18.2322207231911,21.2676870521928,-16.6605885460473));
#92168=CARTESIAN_POINT('Ctrl Pts',(18.2250142226527,21.2659154600617,-16.6601340420788));
#92169=CARTESIAN_POINT('Ctrl Pts',(18.1835878735642,21.2555002336375,-16.6575063345529));
#92170=CARTESIAN_POINT('Ctrl Pts',(18.1495812600686,21.2460403221128,-16.6552902798065));
#92171=CARTESIAN_POINT('Ctrl Pts',(18.0417580379232,21.213120889428,-16.648108466777));
#92172=CARTESIAN_POINT('Ctrl Pts',(17.9689882853298,21.1864600574827,-16.6430272461827));
#92173=CARTESIAN_POINT('Ctrl Pts',(17.7276375597699,21.0826971669278,-16.6256903976212));
#92174=CARTESIAN_POINT('Ctrl Pts',(17.5677309391923,20.9874737591486,-16.6134585182406));
#92175=CARTESIAN_POINT('Ctrl Pts',(17.4027595268346,20.8572395274554,-16.6004980487838));
#92176=CARTESIAN_POINT('Ctrl Pts',(17.3835382494091,20.8415087922951,-16.5989801576873));
#92177=CARTESIAN_POINT('Ctrl Pts',(17.3570805703094,20.8190668653724,-16.5968788920727));
#92178=CARTESIAN_POINT('Ctrl Pts',(17.3496081024696,20.8126382982942,-16.5962840607804));
#92179=CARTESIAN_POINT('Ctrl Pts',(17.3376414850434,20.8021970929332,-16.5953291730991));
#92180=CARTESIAN_POINT('Ctrl Pts',(17.3331191541901,20.7982171079787,-16.5949677708059));
#92181=CARTESIAN_POINT('Ctrl Pts',(17.3240601040195,20.7901755969321,-16.5942426998683));
#92182=CARTESIAN_POINT('Ctrl Pts',(17.3195237958012,20.7861136927771,-16.5938790520863));
#92183=CARTESIAN_POINT('Ctrl Pts',(17.308815303024,20.7764415187106,-16.5930192243498));
#92184=CARTESIAN_POINT('Ctrl Pts',(17.3026585954686,20.7708142055097,-16.5925237697993));
#92185=CARTESIAN_POINT('Ctrl Pts',(17.2835087793866,20.7531021601161,-16.5909790765961));
#92186=CARTESIAN_POINT('Ctrl Pts',(17.2706340332799,20.7408901689957,-16.589935275857));
#92187=CARTESIAN_POINT('Ctrl Pts',(17.2410163613195,20.7120811236827,-16.587520381117));
#92188=CARTESIAN_POINT('Ctrl Pts',(17.2243939338661,20.6953632550145,-16.5861545741598));
#92189=CARTESIAN_POINT('Ctrl Pts',(17.1679487870902,20.636664891547,-16.5814744621242));
#92190=CARTESIAN_POINT('Ctrl Pts',(17.1295686553656,20.5933304868224,-16.5782181253249));
#92191=CARTESIAN_POINT('Ctrl Pts',(16.9902367712116,20.4223798814947,-16.5659819735331));
#92192=CARTESIAN_POINT('Ctrl Pts',(16.9023477456282,20.2848695605904,-16.5574009865093));
#92193=CARTESIAN_POINT('Ctrl Pts',(16.8040977614397,20.0833278367252,-16.5448725997813));
#92194=CARTESIAN_POINT('Ctrl Pts',(16.779551817381,20.0268488270614,-16.541360640526));
#92195=CARTESIAN_POINT('Ctrl Pts',(16.754233554344,19.9608647474203,-16.5371690538814));
#92196=CARTESIAN_POINT('Ctrl Pts',(16.7510188204722,19.9523217612051,-16.5366246936974));
#92197=CARTESIAN_POINT('Ctrl Pts',(16.7462992686397,19.9395294237985,-16.5358066925635));
#92198=CARTESIAN_POINT('Ctrl Pts',(16.7447525651962,19.9352954929125,-16.5355354877355));
#92199=CARTESIAN_POINT('Ctrl Pts',(16.7420066161964,19.9277036158188,-16.5350482980861));
#92200=CARTESIAN_POINT('Ctrl Pts',(16.7408023220002,19.9243475521669,-16.5348326175953));
#92201=CARTESIAN_POINT('Ctrl Pts',(16.7382108441443,19.9170679593546,-16.5343640962465));
#92202=CARTESIAN_POINT('Ctrl Pts',(16.7368267677674,19.9131434309484,-16.5341110808477));
#92203=CARTESIAN_POINT('Ctrl Pts',(16.7329885652896,19.9021570952751,-16.5334016414113));
#92204=CARTESIAN_POINT('Ctrl Pts',(16.7305602908146,19.8950864126831,-16.5329437312795));
#92205=CARTESIAN_POINT('Ctrl Pts',(16.7165951444969,19.8537103629048,-16.5302570475579));
#92206=CARTESIAN_POINT('Ctrl Pts',(16.7059028430342,19.8191287041954,-16.5279831894366));
#92207=CARTESIAN_POINT('Ctrl Pts',(16.6742359297377,19.7065615433117,-16.5205278820005));
#92208=CARTESIAN_POINT('Ctrl Pts',(16.6568356156139,19.6276481163896,-16.5152217318738));
#92209=CARTESIAN_POINT('Ctrl Pts',(16.62611250444,19.4370747924495,-16.502476141204));
#92210=CARTESIAN_POINT('Ctrl Pts',(16.6170882586042,19.3249577472053,-16.4950407472082));
#92211=CARTESIAN_POINT('Ctrl Pts',(16.6170006442198,19.2126515526684,-16.4878149140766));
#92212=CARTESIAN_POINT('Ctrl Pts',(16.6170006421843,19.2126489414195,-16.4878147460677));
#92213=CARTESIAN_POINT('Ctrl Pts',(16.6169350225893,19.1284029889612,-16.4823943244624));
#92214=CARTESIAN_POINT('Ctrl Pts',(16.6218981987403,19.0442181697761,-16.4770994291474));
#92215=CARTESIAN_POINT('Ctrl Pts',(16.633098807133,18.950209986943,-16.471327040016));
#92216=CARTESIAN_POINT('Ctrl Pts',(16.6344059066889,18.9398876570459,-16.4706950623719));
#92217=CARTESIAN_POINT('Ctrl Pts',(16.6367383501716,18.9224977218493,-16.4696333979581));
#92218=CARTESIAN_POINT('Ctrl Pts',(16.6377234420822,18.9154249891837,-16.4692024488237));
#92219=CARTESIAN_POINT('Ctrl Pts',(16.6396009380811,18.9024267101138,-16.468411965802));
#92220=CARTESIAN_POINT('Ctrl Pts',(16.6404827474481,18.8964997293883,-16.4680521005657));
#92221=CARTESIAN_POINT('Ctrl Pts',(16.6423536700329,18.8842811744395,-16.467311403041));
#92222=CARTESIAN_POINT('Ctrl Pts',(16.6433460343017,18.8779901537177,-16.4669306778651));
#92223=CARTESIAN_POINT('Ctrl Pts',(16.6456303028101,18.8639219699515,-16.4660806816276));
#92224=CARTESIAN_POINT('Ctrl Pts',(16.6469372952589,18.8561473261561,-16.4656118946186));
#92225=CARTESIAN_POINT('Ctrl Pts',(16.6503588008126,18.836467557097,-16.4644275879081));
#92226=CARTESIAN_POINT('Ctrl Pts',(16.6525319517277,18.8245728129953,-16.4637139347788));
#92227=CARTESIAN_POINT('Ctrl Pts',(16.6655166178299,18.7567911540029,-16.4596586380029));
#92228=CARTESIAN_POINT('Ctrl Pts',(16.6784773403236,18.701336772074,-16.456386194377));
#92229=CARTESIAN_POINT('Ctrl Pts',(16.7044778881151,18.6073650743949,-16.4508783799238));
#92230=CARTESIAN_POINT('Ctrl Pts',(16.7164194104933,18.568579643663,-16.4486161308946));
#92231=CARTESIAN_POINT('Ctrl Pts',(16.7346150747456,18.5150079072523,-16.4454901792472));
#92232=CARTESIAN_POINT('Ctrl Pts',(16.7399323961956,18.4999168000981,-16.4446094297424));
#92233=CARTESIAN_POINT('Ctrl Pts',(16.7454194446555,18.4848895573635,-16.4437313838642));
#92234=CARTESIAN_POINT('Origin',(18.734,19.211,0.));
#92235=CARTESIAN_POINT('',(16.7454194503191,18.4848895418527,-15.6464962064494));
#92236=CARTESIAN_POINT('',(16.7454194505387,18.4848895412514,-15.8662164192772));
#92237=CARTESIAN_POINT('',(16.7454194503191,18.4848895418526,0.));
#92238=CARTESIAN_POINT('Ctrl Pts',(16.7454194505387,18.4848895412513,-15.8662164192772));
#92239=CARTESIAN_POINT('Ctrl Pts',(16.7372703379848,18.5072073119498,-15.8675066544822));
#92240=CARTESIAN_POINT('Ctrl Pts',(16.7294937210257,18.5296710612778,-15.8687971937546));
#92241=CARTESIAN_POINT('Ctrl Pts',(16.6950140122692,18.6349799328782,-15.8748264215078));
#92242=CARTESIAN_POINT('Ctrl Pts',(16.6730620585041,18.7192730630267,-15.879590771347));
#92243=CARTESIAN_POINT('Ctrl Pts',(16.6490998728355,18.8417960952826,-15.8867186438287));
#92244=CARTESIAN_POINT('Ctrl Pts',(16.6428359561586,18.8791075386946,-15.8889160378287));
#92245=CARTESIAN_POINT('Ctrl Pts',(16.6365221776738,18.9240625137794,-15.8916169870224));
#92246=CARTESIAN_POINT('Ctrl Pts',(16.6355092984658,18.9315664519105,-15.8920696099598));
#92247=CARTESIAN_POINT('Ctrl Pts',(16.6339995009993,18.9432232343556,-15.8927757052441));
#92248=CARTESIAN_POINT('Ctrl Pts',(16.6334745846743,18.9473724769717,-15.8930276259775));
#92249=CARTESIAN_POINT('Ctrl Pts',(16.6325251662833,18.955060116845,-15.8934955089828));
#92250=CARTESIAN_POINT('Ctrl Pts',(16.6320973022233,18.9585980407536,-15.8937112793496));
#92251=CARTESIAN_POINT('Ctrl Pts',(16.6311517265414,18.9665859877452,-15.8941994496842));
#92252=CARTESIAN_POINT('Ctrl Pts',(16.6306392092088,18.9710365580287,-15.8944721366715));
#92253=CARTESIAN_POINT('Ctrl Pts',(16.6291723812532,18.9841399594694,-15.8952769688769));
#92254=CARTESIAN_POINT('Ctrl Pts',(16.6282573251072,18.992796966599,-15.8958112422079));
#92255=CARTESIAN_POINT('Ctrl Pts',(16.6221408152905,19.0542888849057,-15.8996231389614));
#92256=CARTESIAN_POINT('Ctrl Pts',(16.6188755553195,19.1072929604781,-15.9029969137695));
#92257=CARTESIAN_POINT('Ctrl Pts',(16.6172125016239,19.1767948315625,-15.9074892765317));
#92258=CARTESIAN_POINT('Ctrl Pts',(16.6170107019972,19.1932348624198,-15.9085569473233));
#92259=CARTESIAN_POINT('Ctrl Pts',(16.6169886661989,19.2284497820847,-15.9108526786612));
#92260=CARTESIAN_POINT('Ctrl Pts',(16.6172266699904,19.2472233291539,-15.9120818925368));
#92261=CARTESIAN_POINT('Ctrl Pts',(16.6217705396517,19.4220908626881,-15.9235687497658));
#92262=CARTESIAN_POINT('Ctrl Pts',(16.6430867859052,19.5772852807938,-15.9339905157257));
#92263=CARTESIAN_POINT('Ctrl Pts',(16.6824567722274,19.7333814825322,-15.9442508721972));
#92264=CARTESIAN_POINT('Ctrl Pts',(16.6836461856932,19.7380306114362,-15.9445563049051));
#92265=CARTESIAN_POINT('Ctrl Pts',(16.700756637075,19.8039765604478,-15.9488864316136));
#92266=CARTESIAN_POINT('Ctrl Pts',(16.7194057233029,19.8645372993343,-15.9528331057524));
#92267=CARTESIAN_POINT('Ctrl Pts',(16.744959207958,19.935956743936,-15.9574536552498));
#92268=CARTESIAN_POINT('Ctrl Pts',(16.7492787226897,19.9477000847883,-15.958212341309));
#92269=CARTESIAN_POINT('Ctrl Pts',(16.756535005512,19.966900394793,-15.9594512072949));
#92270=CARTESIAN_POINT('Ctrl Pts',(16.7594104063373,19.974380082677,-15.9599334245396));
#92271=CARTESIAN_POINT('Ctrl Pts',(16.7646512558223,19.9877851863247,-15.9607969988478));
#92272=CARTESIAN_POINT('Ctrl Pts',(16.7670011407485,19.9937165457377,-15.9611788728995));
#92273=CARTESIAN_POINT('Ctrl Pts',(16.7720573989489,20.0063124979173,-15.9619893728709));
#92274=CARTESIAN_POINT('Ctrl Pts',(16.7747710038254,20.0129741153373,-15.9624177491541));
#92275=CARTESIAN_POINT('Ctrl Pts',(16.7821562834052,20.0308429904551,-15.9635661535161));
#92276=CARTESIAN_POINT('Ctrl Pts',(16.7868905535818,20.042024208996,-15.9642840543624));
#92277=CARTESIAN_POINT('Ctrl Pts',(16.8108460052971,20.0972725461428,-15.9678286378448));
#92278=CARTESIAN_POINT('Ctrl Pts',(16.8314690797192,20.1407187370143,-15.9706070439605));
#92279=CARTESIAN_POINT('Ctrl Pts',(16.9305671038933,20.3323508844003,-15.9828817081904));
#92280=CARTESIAN_POINT('Ctrl Pts',(17.0249934829181,20.4715936178588,-15.9917999865555));
#92281=CARTESIAN_POINT('Ctrl Pts',(17.1995485361948,20.6728115048001,-16.0063839212129));
#92282=CARTESIAN_POINT('Ctrl Pts',(17.2693654620147,20.7427554364548,-16.0118766883602));
#92283=CARTESIAN_POINT('Ctrl Pts',(17.3511068413779,20.8139315351939,-16.0182979628849));
#92284=CARTESIAN_POINT('Ctrl Pts',(17.3584620166462,20.8202477257904,-16.0188757012464));
#92285=CARTESIAN_POINT('Ctrl Pts',(17.3693853964042,20.829498478165,-16.0197340841584));
#92286=CARTESIAN_POINT('Ctrl Pts',(17.3729203592993,20.8324723404708,-16.0200119253745));
#92287=CARTESIAN_POINT('Ctrl Pts',(17.379208746065,20.8377275260725,-16.0205063378721));
#92288=CARTESIAN_POINT('Ctrl Pts',(17.3819582459753,20.8400134686323,-16.0207225671721));
#92289=CARTESIAN_POINT('Ctrl Pts',(17.3878614411671,20.8448961621785,-16.0211869480593));
#92290=CARTESIAN_POINT('Ctrl Pts',(17.3910168175665,20.847490714733,-16.0214352458989));
#92291=CARTESIAN_POINT('Ctrl Pts',(17.399698556077,20.8545873772714,-16.0221185784219));
#92292=CARTESIAN_POINT('Ctrl Pts',(17.405240118824,20.8590706856279,-16.0225549306345));
#92293=CARTESIAN_POINT('Ctrl Pts',(17.4349422088294,20.8828534803047,-16.0248941948067));
#92294=CARTESIAN_POINT('Ctrl Pts',(17.4594994325259,20.9016487733083,-16.0268298793207));
#92295=CARTESIAN_POINT('Ctrl Pts',(17.5350662576103,20.9569030432717,-16.032769249948));
#92296=CARTESIAN_POINT('Ctrl Pts',(17.5872901051328,20.991638894754,-16.0368503662621));
#92297=CARTESIAN_POINT('Ctrl Pts',(17.7561738807176,21.0934557490769,-16.0498093867847));
#92298=CARTESIAN_POINT('Ctrl Pts',(17.8777424423705,21.1517760712222,-16.0587750403475));
#92299=CARTESIAN_POINT('Ctrl Pts',(18.0423576948902,21.2122464713815,-16.0700684915993));
#92300=CARTESIAN_POINT('Ctrl Pts',(18.0810896173937,21.2252156957783,-16.0726704383924));
#92301=CARTESIAN_POINT('Ctrl Pts',(18.1665838700041,21.2511175143233,-16.0782894123099));
#92302=CARTESIAN_POINT('Ctrl Pts',(18.2134654325085,21.26358006063,-16.0812910215525));
#92303=CARTESIAN_POINT('Ctrl Pts',(18.2730119900446,21.2772375612181,-16.0850068878458));
#92304=CARTESIAN_POINT('Ctrl Pts',(18.2853121770729,21.2799434146481,-16.0857693559484));
#92305=CARTESIAN_POINT('Ctrl Pts',(18.3048443108914,21.2840578043013,-16.0869722262839));
#92306=CARTESIAN_POINT('Ctrl Pts',(18.3120605779536,21.28553859731,-16.0874149339052));
#92307=CARTESIAN_POINT('Ctrl Pts',(18.3255227062038,21.2882279048498,-16.0882376989306));
#92308=CARTESIAN_POINT('Ctrl Pts',(18.3317665506242,21.2894459872229,-16.0886180580254));
#92309=CARTESIAN_POINT('Ctrl Pts',(18.3456487794615,21.2920893069624,-16.0894610037054));
#92310=CARTESIAN_POINT('Ctrl Pts',(18.3532897352393,21.2935006772667,-16.0899231436532));
#92311=CARTESIAN_POINT('Ctrl Pts',(18.3755207990142,21.2974805594587,-16.09126252262));
#92312=CARTESIAN_POINT('Ctrl Pts',(18.390130499251,21.2999380665025,-16.0921362302239));
#92313=CARTESIAN_POINT('Ctrl Pts',(18.5067618485589,21.3182999358133,-16.0990618573236));
#92314=CARTESIAN_POINT('Ctrl Pts',(18.6098034071758,21.32687556893,-16.1048707490221));
#92315=CARTESIAN_POINT('Ctrl Pts',(18.8727090876753,21.3294748362667,-16.1193461025518));
#92316=CARTESIAN_POINT('Ctrl Pts',(19.0319979647193,21.3129907613249,-16.1277744772072));
#92317=CARTESIAN_POINT('Ctrl Pts',(19.2353151291203,21.2683594659664,-16.1395295669706));
#92318=CARTESIAN_POINT('Ctrl Pts',(19.2823474315499,21.2563261688315,-16.142324317089));
#92319=CARTESIAN_POINT('Ctrl Pts',(19.3363663344937,21.2405083128188,-16.1456660095503));
#92320=CARTESIAN_POINT('Ctrl Pts',(19.3437999112581,21.2382871668293,-16.1461287968799));
#92321=CARTESIAN_POINT('Ctrl Pts',(19.3556667038689,21.2346702077863,-16.1468725286104));
#92322=CARTESIAN_POINT('Ctrl Pts',(19.3601079030015,21.2333005447848,-16.1471519859625));
#92323=CARTESIAN_POINT('Ctrl Pts',(19.3679699771556,21.2308475051833,-16.1476487304446));
#92324=CARTESIAN_POINT('Ctrl Pts',(19.3713926503351,21.2297700426906,-16.1478656690635));
#92325=CARTESIAN_POINT('Ctrl Pts',(19.3786461899969,21.2274663320713,-16.1483268959632));
#92326=CARTESIAN_POINT('Ctrl Pts',(19.3824762460304,21.2262378858005,-16.1485713065385));
#92327=CARTESIAN_POINT('Ctrl Pts',(19.3928140280941,21.2228896393008,-16.1492333101437));
#92328=CARTESIAN_POINT('Ctrl Pts',(19.3993149475863,21.2207492037316,-16.1496520895752));
#92329=CARTESIAN_POINT('Ctrl Pts',(19.4316549186143,21.2099271234083,-16.1517473445269));
#92330=CARTESIAN_POINT('Ctrl Pts',(19.4573336978648,21.200778939605,-16.1534491572841));
#92331=CARTESIAN_POINT('Ctrl Pts',(19.5312492754909,21.1728263444362,-16.158444594095));
#92332=CARTESIAN_POINT('Ctrl Pts',(19.5789802184669,21.1527457923717,-16.1617914264722));
#92333=CARTESIAN_POINT('Ctrl Pts',(19.7513291389154,21.0726795994349,-16.1742136793461));
#92334=CARTESIAN_POINT('Ctrl Pts',(19.8707357306342,21.0022692271514,-16.183460321891));
#92335=CARTESIAN_POINT('Ctrl Pts',(20.0600503310996,20.8640331959325,-16.1986385612822));
#92336=CARTESIAN_POINT('Ctrl Pts',(20.1337362630978,20.802122586771,-16.204711127236));
#92337=CARTESIAN_POINT('Ctrl Pts',(20.2129594146628,20.7257807064029,-16.2114253132841));
#92338=CARTESIAN_POINT('Ctrl Pts',(20.2228563979325,20.716054211461,-16.2122678391311));
#92339=CARTESIAN_POINT('Ctrl Pts',(20.2385435219477,20.7003311406643,-16.2136095515018));
#92340=CARTESIAN_POINT('Ctrl Pts',(20.2443949946132,20.6943965819486,-16.2141114538958));
#92341=CARTESIAN_POINT('Ctrl Pts',(20.2547040314954,20.6838169237359,-16.2149983082703));
#92342=CARTESIAN_POINT('Ctrl Pts',(20.259175711001,20.6791857832855,-16.2153838770409));
#92343=CARTESIAN_POINT('Ctrl Pts',(20.2684305518141,20.6695130017695,-16.2161837577181));
#92344=CARTESIAN_POINT('Ctrl Pts',(20.2732101580416,20.6644680546276,-16.2165979129536));
#92345=CARTESIAN_POINT('Ctrl Pts',(20.2855195851536,20.6513464527358,-16.2176673607829));
#92346=CARTESIAN_POINT('Ctrl Pts',(20.2930112736187,20.6432341927009,-16.2183210147964));
#92347=CARTESIAN_POINT('Ctrl Pts',(20.3249209678904,20.608134216241,-16.221117670866));
#92348=CARTESIAN_POINT('Ctrl Pts',(20.3487051625018,20.5805769477522,-16.2232339635939));
#92349=CARTESIAN_POINT('Ctrl Pts',(20.4096666454325,20.5061477177143,-16.2287591338815));
#92350=CARTESIAN_POINT('Ctrl Pts',(20.4455890093664,20.4582891297163,-16.2321205143551));
#92351=CARTESIAN_POINT('Ctrl Pts',(20.5743805507534,20.2706403478866,-16.2447295331557));
#92352=CARTESIAN_POINT('Ctrl Pts',(20.6525332045611,20.1215278360038,-16.2535600900867));
#92353=CARTESIAN_POINT('Ctrl Pts',(20.7314606050521,19.9143827251244,-16.2660207074756));
#92354=CARTESIAN_POINT('Ctrl Pts',(20.748724706781,19.8632878456706,-16.2691133167137));
#92355=CARTESIAN_POINT('Ctrl Pts',(20.7664984018001,19.803212511083,-16.2728309609752));
#92356=CARTESIAN_POINT('Ctrl Pts',(20.768926347849,19.7948151800642,-16.273352439142));
#92357=CARTESIAN_POINT('Ctrl Pts',(20.772521955724,19.7820843862449,-16.2741461215025));
#92358=CARTESIAN_POINT('Ctrl Pts',(20.7737279911564,19.7777617324963,-16.2744161488845));
#92359=CARTESIAN_POINT('Ctrl Pts',(20.7758672021795,19.7699991348371,-16.2749020808522));
#92360=CARTESIAN_POINT('Ctrl Pts',(20.7768054426064,19.7665606424587,-16.2751176878113));
#92361=CARTESIAN_POINT('Ctrl Pts',(20.7788242211849,19.7590879005226,-16.2755870519059));
#92362=CARTESIAN_POINT('Ctrl Pts',(20.7799014919576,19.7550528712854,-16.275840989026));
#92363=CARTESIAN_POINT('Ctrl Pts',(20.782891330925,19.7437196596552,-16.2765555634833));
#92364=CARTESIAN_POINT('Ctrl Pts',(20.7847768123271,19.7364144876266,-16.277017721132));
#92365=CARTESIAN_POINT('Ctrl Pts',(20.7957646678839,19.6928824517357,-16.2797803557153));
#92366=CARTESIAN_POINT('Ctrl Pts',(20.8039453947512,19.656432273043,-16.2821288798174));
#92367=CARTESIAN_POINT('Ctrl Pts',(20.8276015321951,19.5362292035531,-16.2899473316017));
#92368=CARTESIAN_POINT('Ctrl Pts',(20.8389879282697,19.4517599740834,-16.2955546762976));
#92369=CARTESIAN_POINT('Ctrl Pts',(20.8583669163958,19.1892229037362,-16.3129454354005));
#92370=CARTESIAN_POINT('Ctrl Pts',(20.8490135372426,19.0106221892133,-16.3246495988053));
#92371=CARTESIAN_POINT('Ctrl Pts',(20.8133485376991,18.8128570185984,-16.3370162763271));
#92372=CARTESIAN_POINT('Ctrl Pts',(20.8089427716754,18.7904994258932,-16.3384070634925));
#92373=CARTESIAN_POINT('Ctrl Pts',(20.802187213201,18.7589146812718,-16.3403621679231));
#92374=CARTESIAN_POINT('Ctrl Pts',(20.8001349567033,18.7496261498893,-16.3409359412275));
#92375=CARTESIAN_POINT('Ctrl Pts',(20.7966949663175,18.7345401321159,-16.3418659829541));
#92376=CARTESIAN_POINT('Ctrl Pts',(20.7953452462647,18.7287341950681,-16.3422234663102));
#92377=CARTESIAN_POINT('Ctrl Pts',(20.7924655646804,18.7165799772789,-16.3429709157617));
#92378=CARTESIAN_POINT('Ctrl Pts',(20.790930714254,18.7102329103519,-16.3433607201655));
#92379=CARTESIAN_POINT('Ctrl Pts',(20.7872036082603,18.6951264955355,-16.3442872831915));
#92380=CARTESIAN_POINT('Ctrl Pts',(20.7849846198863,18.6863738260265,-16.3448231737148));
#92381=CARTESIAN_POINT('Ctrl Pts',(20.7772909391374,18.6568215804738,-16.3466294900107));
#92382=CARTESIAN_POINT('Ctrl Pts',(20.7715551903311,18.6360908948829,-16.3478914697358));
#92383=CARTESIAN_POINT('Ctrl Pts',(20.7148905508003,18.4427996760088,-16.3596190630719));
#92384=CARTESIAN_POINT('Ctrl Pts',(20.6424768867629,18.2773073149672,-16.3692832525787));
#92385=CARTESIAN_POINT('Ctrl Pts',(20.4883295364103,18.0200282347763,-16.3856074761936));
#92386=CARTESIAN_POINT('Ctrl Pts',(20.4180311589327,17.9225449017254,-16.3921923595659));
#92387=CARTESIAN_POINT('Ctrl Pts',(20.3336713427506,17.8243381489574,-16.3998650207705));
#92388=CARTESIAN_POINT('Ctrl Pts',(20.3274243060859,17.8171641175908,-16.4004320371321));
#92389=CARTESIAN_POINT('Ctrl Pts',(20.3180957235876,17.8065959444037,-16.4012774683594));
#92390=CARTESIAN_POINT('Ctrl Pts',(20.3150510616812,17.8031692032372,-16.4015532005077));
#92391=CARTESIAN_POINT('Ctrl Pts',(20.3096140319301,17.7970897543647,-16.4020452945855));
#92392=CARTESIAN_POINT('Ctrl Pts',(20.3072260558671,17.7944331864542,-16.4022613264826));
#92393=CARTESIAN_POINT('Ctrl Pts',(20.3020773230243,17.7887344181768,-16.4027269186725));
#92394=CARTESIAN_POINT('Ctrl Pts',(20.2993144721353,17.7856942507366,-16.4029766337973));
#92395=CARTESIAN_POINT('Ctrl Pts',(20.2916632600421,17.7773241394906,-16.4036677807611));
#92396=CARTESIAN_POINT('Ctrl Pts',(20.2867564615553,17.7720112327354,-16.4041105796447));
#92397=CARTESIAN_POINT('Ctrl Pts',(20.2597183887548,17.7430346861219,-16.406547622935));
#92398=CARTESIAN_POINT('Ctrl Pts',(20.2370746040844,17.719857742163,-16.4085778995664));
#92399=CARTESIAN_POINT('Ctrl Pts',(20.097483666602,17.5833909361846,-16.4209809736149));
#92400=CARTESIAN_POINT('Ctrl Pts',(19.9683196361249,17.483384903518,-16.431945889431));
#92401=CARTESIAN_POINT('Ctrl Pts',(19.7289717787905,17.3387359982418,-16.4502134574942));
#92402=CARTESIAN_POINT('Ctrl Pts',(19.6241279329738,17.2866763765054,-16.4576564236641));
#92403=CARTESIAN_POINT('Ctrl Pts',(19.502224009768,17.2382544165585,-16.4656656123793));
#92404=CARTESIAN_POINT('Ctrl Pts',(19.4888880039725,17.233112899239,-16.4665337624093));
#92405=CARTESIAN_POINT('Ctrl Pts',(19.4675809827548,17.2251451628107,-16.4679082935556));
#92406=CARTESIAN_POINT('Ctrl Pts',(19.4596435150015,17.2222310377965,-16.4684176042152));
#92407=CARTESIAN_POINT('Ctrl Pts',(19.4456142188266,17.2171755607581,-16.4693130406014));
#92408=CARTESIAN_POINT('Ctrl Pts',(19.4395296934197,17.2150143928148,-16.4696998227235));
#92409=CARTESIAN_POINT('Ctrl Pts',(19.4269249419875,17.2106021387253,-16.4704978804469));
#92410=CARTESIAN_POINT('Ctrl Pts',(19.420403403652,17.2083550120386,-16.470909020808));
#92411=CARTESIAN_POINT('Ctrl Pts',(19.4036362681259,17.2026690853815,-16.4719616220111));
#92412=CARTESIAN_POINT('Ctrl Pts',(19.3933750308138,17.1992767661786,-16.472601542176));
#92413=CARTESIAN_POINT('Ctrl Pts',(19.3504478183054,17.1854489578652,-16.4752613457933));
#92414=CARTESIAN_POINT('Ctrl Pts',(19.3175556178848,17.1757290170095,-16.4772577199586));
#92415=CARTESIAN_POINT('Ctrl Pts',(19.2312587993225,17.1524917941883,-16.4823994168371));
#92416=CARTESIAN_POINT('Ctrl Pts',(19.1775362635816,17.1402516873574,-16.4855053983549));
#92417=CARTESIAN_POINT('Ctrl Pts',(19.0159374463888,17.1100117523139,-16.4946470567729));
#92418=CARTESIAN_POINT('Ctrl Pts',(18.9070813659006,17.0982567435247,-16.5005339951662));
#92419=CARTESIAN_POINT('Ctrl Pts',(18.7545609007622,17.0936578019592,-16.5088415043364));
#92420=CARTESIAN_POINT('Ctrl Pts',(18.7112882878485,17.0936798263302,-16.511206511981));
#92421=CARTESIAN_POINT('Ctrl Pts',(18.5928088297098,17.0973726713773,-16.5177696490504));
#92422=CARTESIAN_POINT('Ctrl Pts',(18.5177564429834,17.1037288720893,-16.5220238639938));
#92423=CARTESIAN_POINT('Ctrl Pts',(18.4338140958387,17.1153694449363,-16.527046513207));
#92424=CARTESIAN_POINT('Ctrl Pts',(18.4244262290748,17.1167356725686,-16.5276120009833));
#92425=CARTESIAN_POINT('Ctrl Pts',(18.410521447902,17.1188547869544,-16.5284555842056));
#92426=CARTESIAN_POINT('Ctrl Pts',(18.4059971338908,17.1195593278658,-16.5287310139246));
#92427=CARTESIAN_POINT('Ctrl Pts',(18.3979478499815,17.1208395493804,-16.5292227772194));
#92428=CARTESIAN_POINT('Ctrl Pts',(18.3944220163879,17.1214094779884,-16.529438782477));
#92429=CARTESIAN_POINT('Ctrl Pts',(18.3868404970197,17.1226546780927,-16.5299045559549));
#92430=CARTESIAN_POINT('Ctrl Pts',(18.3827853905457,17.1233328326854,-16.5301544802672));
#92431=CARTESIAN_POINT('Ctrl Pts',(18.371587516295,17.1252390551038,-16.5308467825892));
#92432=CARTESIAN_POINT('Ctrl Pts',(18.3644491185967,17.1264919836675,-16.5312905350325));
#92433=CARTESIAN_POINT('Ctrl Pts',(18.3252126943376,17.1335866200963,-16.5337424573576));
#92434=CARTESIAN_POINT('Ctrl Pts',(18.2932484482161,17.140132739488,-16.5357871695786));
#92435=CARTESIAN_POINT('Ctrl Pts',(18.1029248986742,17.1837157752577,-16.5481950996584));
#92436=CARTESIAN_POINT('Ctrl Pts',(17.9491147409275,17.2381613894483,-16.5591467914266));
#92437=CARTESIAN_POINT('Ctrl Pts',(17.6981779518302,17.3610276539101,-16.5773969661328));
#92438=CARTESIAN_POINT('Ctrl Pts',(17.5977168659777,17.4209739011093,-16.5848353107958));
#92439=CARTESIAN_POINT('Ctrl Pts',(17.4910707273739,17.4972263303822,-16.5928404804345));
#92440=CARTESIAN_POINT('Ctrl Pts',(17.4795260830902,17.5056588098105,-16.5937088485083));
#92441=CARTESIAN_POINT('Ctrl Pts',(17.4612896757661,17.5192645181367,-16.5950836585368));
#92442=CARTESIAN_POINT('Ctrl Pts',(17.4545421215723,17.5243619088323,-16.5955930318842));
#92443=CARTESIAN_POINT('Ctrl Pts',(17.4426965018002,17.5334225893669,-16.596488541193));
#92444=CARTESIAN_POINT('Ctrl Pts',(17.4375857206993,17.5373690039356,-16.5968753338861));
#92445=CARTESIAN_POINT('Ctrl Pts',(17.4272245941441,17.5454455395872,-16.5976603896072));
#92446=CARTESIAN_POINT('Ctrl Pts',(17.4219755787544,17.5495772538036,-16.5980585832868));
#92447=CARTESIAN_POINT('Ctrl Pts',(17.4086671173706,17.5601552898741,-16.5990694540297));
#92448=CARTESIAN_POINT('Ctrl Pts',(17.4006350326858,17.5666358747579,-16.5996807535804));
#92449=CARTESIAN_POINT('Ctrl Pts',(17.3833150855723,17.5808206026031,-16.601001764251));
#92450=CARTESIAN_POINT('Ctrl Pts',(17.3740450221823,17.5885459719998,-16.6017106003301));
#92451=CARTESIAN_POINT('Ctrl Pts',(17.3475939486691,17.6109754286509,-16.6037388864044));
#92452=CARTESIAN_POINT('Ctrl Pts',(17.3305815226943,17.6258763451671,-16.6050504124132));
#92453=CARTESIAN_POINT('Ctrl Pts',(17.2733864286901,17.6776154003413,-16.6094885510654));
#92454=CARTESIAN_POINT('Ctrl Pts',(17.234387828678,17.7157326999588,-16.6125639121214));
#92455=CARTESIAN_POINT('Ctrl Pts',(17.1220538387575,17.8343492803952,-16.6216520988581));
#92456=CARTESIAN_POINT('Ctrl Pts',(17.0534108180664,17.9190408009899,-16.6275160212359));
#92457=CARTESIAN_POINT('Ctrl Pts',(16.9234840446183,18.1073250390856,-16.6399672490605));
#92458=CARTESIAN_POINT('Ctrl Pts',(16.8638998449213,18.2116084425544,-16.6465480196933));
#92459=CARTESIAN_POINT('Ctrl Pts',(16.8094654166003,18.3289874233287,-16.6542160118183));
#92460=CARTESIAN_POINT('Ctrl Pts',(16.8055204004251,18.337646706947,-16.65478319563));
#92461=CARTESIAN_POINT('Ctrl Pts',(16.7997614702753,18.3505168054459,-16.6556288292752));
#92462=CARTESIAN_POINT('Ctrl Pts',(16.797902579604,18.3547075290473,-16.6559045945268));
#92463=CARTESIAN_POINT('Ctrl Pts',(16.7946195145981,18.3621742855265,-16.6563967248373));
#92464=CARTESIAN_POINT('Ctrl Pts',(16.7931900050555,18.3654479176277,-16.6566127596762));
#92465=CARTESIAN_POINT('Ctrl Pts',(16.7901344690081,18.3724937861814,-16.6570783321415));
#92466=CARTESIAN_POINT('Ctrl Pts',(16.7885111578161,18.3762670861491,-16.6573280244621));
#92467=CARTESIAN_POINT('Ctrl Pts',(16.7840607644922,18.3866952879818,-16.6580190455068));
#92468=CARTESIAN_POINT('Ctrl Pts',(16.7812568102554,18.3933599130058,-16.6584617404719));
#92469=CARTESIAN_POINT('Ctrl Pts',(16.7668566453678,18.4280837731999,-16.6607732919043));
#92470=CARTESIAN_POINT('Ctrl Pts',(16.7558316159281,18.4563740043379,-16.6626735625179));
#92471=CARTESIAN_POINT('Ctrl Pts',(16.7454194503294,18.4848895418246,-16.6645989754405));
#92472=CARTESIAN_POINT('Ctrl Pts',(16.7454194446555,18.4848895573635,-16.4437313838642));
#92473=CARTESIAN_POINT('Ctrl Pts',(16.7704615306514,18.4163074211586,-16.4397241110012));
#92474=CARTESIAN_POINT('Ctrl Pts',(16.7990388766678,18.349055408265,-16.4357751040702));
#92475=CARTESIAN_POINT('Ctrl Pts',(16.8846074405981,18.1735115759695,-16.4251562043927));
#92476=CARTESIAN_POINT('Ctrl Pts',(16.9475863594341,18.0684795667363,-16.4184725391856));
#92477=CARTESIAN_POINT('Ctrl Pts',(17.0262143222114,17.9598814560045,-16.4105598910851));
#92478=CARTESIAN_POINT('Ctrl Pts',(17.0332468354988,17.950338193115,-16.4098553651788));
#92479=CARTESIAN_POINT('Ctrl Pts',(17.0433668792879,17.936843892707,-16.4088452168993));
#92480=CARTESIAN_POINT('Ctrl Pts',(17.0463890177702,17.9328437865109,-16.4085440160231));
#92481=CARTESIAN_POINT('Ctrl Pts',(17.0516249495664,17.9259644438552,-16.4080228927674));
#92482=CARTESIAN_POINT('Ctrl Pts',(17.0538320188974,17.9230800700326,-16.4078034428587));
#92483=CARTESIAN_POINT('Ctrl Pts',(17.0581283780679,17.9174950850107,-16.4073766446614));
#92484=CARTESIAN_POINT('Ctrl Pts',(17.0602167830424,17.9147938433464,-16.4071693638787));
#92485=CARTESIAN_POINT('Ctrl Pts',(17.0658747510241,17.9075120340758,-16.4066083056037));
#92486=CARTESIAN_POINT('Ctrl Pts',(17.0694566109586,17.9029411222151,-16.4062536670681));
#92487=CARTESIAN_POINT('Ctrl Pts',(17.0828547584918,17.8859875158255,-16.4049293334138));
#92488=CARTESIAN_POINT('Ctrl Pts',(17.0927905037472,17.873700464655,-16.4039516191479));
#92489=CARTESIAN_POINT('Ctrl Pts',(17.1850072210732,17.7622361696263,-16.3949256851549));
#92490=CARTESIAN_POINT('Ctrl Pts',(17.2760386713513,17.6706630134185,-16.3863804075939));
#92491=CARTESIAN_POINT('Ctrl Pts',(17.4471373716444,17.5273815367175,-16.3716359364207));
#92492=CARTESIAN_POINT('Ctrl Pts',(17.5234275556216,17.4717175414131,-16.3654339514517));
#92493=CARTESIAN_POINT('Ctrl Pts',(17.6472805455279,17.3934601810411,-16.3560397924745));
#92494=CARTESIAN_POINT('Ctrl Pts',(17.6923971686405,17.3672336341904,-16.3527432610836));
#92495=CARTESIAN_POINT('Ctrl Pts',(17.7577913354779,17.3323870910632,-16.348142686415));
#92496=CARTESIAN_POINT('Ctrl Pts',(17.7773025027236,17.3223762223864,-16.3467915879511));
#92497=CARTESIAN_POINT('Ctrl Pts',(17.8120124089517,17.3052430828614,-16.3444252533818));
#92498=CARTESIAN_POINT('Ctrl Pts',(17.8271466380412,17.2979951514389,-16.3434057332562));
#92499=CARTESIAN_POINT('Ctrl Pts',(17.8497424354057,17.28750222027,-16.3419013132079));
#92500=CARTESIAN_POINT('Ctrl Pts',(17.8571388390056,17.2841191898847,-16.3414116549642));
#92501=CARTESIAN_POINT('Ctrl Pts',(17.8704014009748,17.2781452252445,-16.3405385643761));
#92502=CARTESIAN_POINT('Ctrl Pts',(17.876260150255,17.275538176017,-16.3401545813735));
#92503=CARTESIAN_POINT('Ctrl Pts',(17.8877713728649,17.2704784013072,-16.3394034363394));
#92504=CARTESIAN_POINT('Ctrl Pts',(17.8934228831066,17.2680236552739,-16.3390362081115));
#92505=CARTESIAN_POINT('Ctrl Pts',(17.9087987350939,17.2614247624792,-16.3380412601121));
#92506=CARTESIAN_POINT('Ctrl Pts',(17.9185436111592,17.2573286820976,-16.3374151805354));
#92507=CARTESIAN_POINT('Ctrl Pts',(17.9556042876434,17.2420765117757,-16.3350507499504));
#92508=CARTESIAN_POINT('Ctrl Pts',(17.9831223803184,17.2314186012617,-16.3333292111239));
#92509=CARTESIAN_POINT('Ctrl Pts',(18.0171056445599,17.2190673429564,-16.331241227544));
#92510=CARTESIAN_POINT('Ctrl Pts',(18.0233666816409,17.2168251041448,-16.3308581002547));
#92511=CARTESIAN_POINT('Ctrl Pts',(18.2107989234549,17.1506956085706,-16.3194341215848));
#92512=CARTESIAN_POINT('Ctrl Pts',(18.3998039003853,17.1117365839016,-16.3092858481144));
#92513=CARTESIAN_POINT('Ctrl Pts',(18.6540373129886,17.0945815900907,-16.2952817936928));
#92514=CARTESIAN_POINT('Ctrl Pts',(18.7167523310306,17.0931420523626,-16.2917894011348));
#92515=CARTESIAN_POINT('Ctrl Pts',(18.8103525060619,17.0951513036267,-16.2864042814848));
#92516=CARTESIAN_POINT('Ctrl Pts',(18.8412512065431,17.0964924065404,-16.2845982904104));
#92517=CARTESIAN_POINT('Ctrl Pts',(18.8792207313226,17.0989747272743,-16.2823321553682));
#92518=CARTESIAN_POINT('Ctrl Pts',(18.8863313914775,17.0994756792029,-16.2819057427643));
#92519=CARTESIAN_POINT('Ctrl Pts',(18.8975128599053,17.1003201963732,-16.2812318324158));
#92520=CARTESIAN_POINT('Ctrl Pts',(18.9015855106454,17.1006396552329,-16.2809856667422));
#92521=CARTESIAN_POINT('Ctrl Pts',(18.9092211361267,17.1012608361784,-16.2805227756422));
#92522=CARTESIAN_POINT('Ctrl Pts',(18.9127842797583,17.1015597978279,-16.2803062064237));
#92523=CARTESIAN_POINT('Ctrl Pts',(18.9209489220383,17.1022656782048,-16.2798086777473));
#92524=CARTESIAN_POINT('Ctrl Pts',(18.9255498444668,17.1026786308726,-16.2795273834362));
#92525=CARTESIAN_POINT('Ctrl Pts',(18.9398022677399,17.1040048854598,-16.2786532105473));
#92526=CARTESIAN_POINT('Ctrl Pts',(18.9494487144043,17.104969413954,-16.2780575664193));
#92527=CARTESIAN_POINT('Ctrl Pts',(19.0583922718588,17.1166187665741,-16.2712881671043));
#92528=CARTESIAN_POINT('Ctrl Pts',(19.1568094795274,17.1342500138841,-16.2647796484082));
#92529=CARTESIAN_POINT('Ctrl Pts',(19.4189277760569,17.200615039463,-16.2469646156926));
#92530=CARTESIAN_POINT('Ctrl Pts',(19.5786209928436,17.262306328343,-16.2356403865543));
#92531=CARTESIAN_POINT('Ctrl Pts',(19.7551327423921,17.3563192144771,-16.2231066089301));
#92532=CARTESIAN_POINT('Ctrl Pts',(19.780785029331,17.370675536726,-16.2212824452972));
#92533=CARTESIAN_POINT('Ctrl Pts',(19.8245078514859,17.3963551793112,-16.2181680336639));
#92534=CARTESIAN_POINT('Ctrl Pts',(19.842721106416,17.4074255602496,-16.2168690578628));
#92535=CARTESIAN_POINT('Ctrl Pts',(19.8683808270902,17.4235576727887,-16.215036066827));
#92536=CARTESIAN_POINT('Ctrl Pts',(19.8759665198765,17.4283944896968,-16.2144938126804));
#92537=CARTESIAN_POINT('Ctrl Pts',(19.8889995923516,17.4368220205085,-16.2135614369659));
#92538=CARTESIAN_POINT('Ctrl Pts',(19.8944615848521,17.4403898021285,-16.213170469153));
#92539=CARTESIAN_POINT('Ctrl Pts',(19.9048879955412,17.447269319616,-16.2124236884958));
#92540=CARTESIAN_POINT('Ctrl Pts',(19.9098550657846,17.4505769041444,-16.2120677251431));
#92541=CARTESIAN_POINT('Ctrl Pts',(19.922734539108,17.4592322078263,-16.2111441531797));
#92542=CARTESIAN_POINT('Ctrl Pts',(19.930624916454,17.464612581347,-16.2105777819303));
#92543=CARTESIAN_POINT('Ctrl Pts',(19.9574051396603,17.4831404764714,-16.2086533239791));
#92544=CARTESIAN_POINT('Ctrl Pts',(19.9761172950283,17.4965428394698,-16.207304948819));
#92545=CARTESIAN_POINT('Ctrl Pts',(20.1353166627209,17.6145423851928,-16.1957903035545));
#92546=CARTESIAN_POINT('Ctrl Pts',(20.2625385652158,17.7358925886438,-16.1863715732034));
#92547=CARTESIAN_POINT('Ctrl Pts',(20.4285658908881,17.9390935895098,-16.1720947011483));
#92548=CARTESIAN_POINT('Ctrl Pts',(20.4795301237799,18.0099914014938,-16.1673195255445));
#92549=CARTESIAN_POINT('Ctrl Pts',(20.5461419212577,18.1158900825681,-16.1601770607969));
#92550=CARTESIAN_POINT('Ctrl Pts',(20.5654462905767,18.1484896904844,-16.1579766778086));
#92551=CARTESIAN_POINT('Ctrl Pts',(20.5875478672095,18.1882064304733,-16.1552724158058));
#92552=CARTESIAN_POINT('Ctrl Pts',(20.591195711937,18.1948452551236,-16.154819614514));
#92553=CARTESIAN_POINT('Ctrl Pts',(20.5968024601485,18.2051801891155,-16.154113300508));
#92554=CARTESIAN_POINT('Ctrl Pts',(20.5987862129881,18.208862845386,-16.1538613409515));
#92555=CARTESIAN_POINT('Ctrl Pts',(20.6024397918604,18.2156937936839,-16.1533934227245));
#92556=CARTESIAN_POINT('Ctrl Pts',(20.6041125877399,18.2188404318184,-16.1531776561949));
#92557=CARTESIAN_POINT('Ctrl Pts',(20.6078699860158,18.2259516060288,-16.1526895418979));
#92558=CARTESIAN_POINT('Ctrl Pts',(20.6099499438573,18.2299185200787,-16.1524169074041));
#92559=CARTESIAN_POINT('Ctrl Pts',(20.6160334232944,18.2416110648502,-16.1516123703569));
#92560=CARTESIAN_POINT('Ctrl Pts',(20.6200018641408,18.2493547033928,-16.1510783419754));
#92561=CARTESIAN_POINT('Ctrl Pts',(20.647809630442,18.3044503692619,-16.1472713998582));
#92562=CARTESIAN_POINT('Ctrl Pts',(20.6699085752681,18.3526547876637,-16.1439026066277));
#92563=CARTESIAN_POINT('Ctrl Pts',(20.6974105989166,18.419124903479,-16.1392545425674));
#92564=CARTESIAN_POINT('Ctrl Pts',(20.7044128210968,18.4367128227123,-16.1380243728112));
#92565=CARTESIAN_POINT('Ctrl Pts',(20.7281825343384,18.498828144907,-16.1336838334092));
#92566=CARTESIAN_POINT('Ctrl Pts',(20.7436837153178,18.5438239556507,-16.130547154643));
#92567=CARTESIAN_POINT('Ctrl Pts',(20.7897747142654,18.6938523942022,-16.1201795341099));
#92568=CARTESIAN_POINT('Ctrl Pts',(20.8137460009862,18.8007423255791,-16.1129474872608));
#92569=CARTESIAN_POINT('Ctrl Pts',(20.8372085215249,18.9635374632004,-16.1023754190192));
#92570=CARTESIAN_POINT('Ctrl Pts',(20.8429361007121,19.018352301346,-16.0988870151962));
#92571=CARTESIAN_POINT('Ctrl Pts',(20.8487493996785,19.1075575720974,-16.0933304765121));
#92572=CARTESIAN_POINT('Ctrl Pts',(20.8501478196467,19.1418336717667,-16.091223920679));
#92573=CARTESIAN_POINT('Ctrl Pts',(20.8508908250243,19.1869366535892,-16.0884877295449));
#92574=CARTESIAN_POINT('Ctrl Pts',(20.8509860900701,19.1977443994115,-16.0878347601204));
#92575=CARTESIAN_POINT('Ctrl Pts',(20.8510065598351,19.2154504384766,-16.0867693029909));
#92576=CARTESIAN_POINT('Ctrl Pts',(20.850980821094,19.2223483769558,-16.086355286078));
#92577=CARTESIAN_POINT('Ctrl Pts',(20.850865717936,19.2357026787889,-16.0855557757483));
#92578=CARTESIAN_POINT('Ctrl Pts',(20.8507805291747,19.2421589929963,-16.0851701560413));
#92579=CARTESIAN_POINT('Ctrl Pts',(20.8505155754932,19.2570684786624,-16.0842817148123));
#92580=CARTESIAN_POINT('Ctrl Pts',(20.850314704346,19.2655212010512,-16.0837795594562));
#92581=CARTESIAN_POINT('Ctrl Pts',(20.8496380997534,19.2882570949629,-16.0824328698369));
#92582=CARTESIAN_POINT('Ctrl Pts',(20.8490683645714,19.3025371834458,-16.0815912775324));
#92583=CARTESIAN_POINT('Ctrl Pts',(20.8425104361114,19.4335805095935,-16.0739047273808));
#92584=CARTESIAN_POINT('Ctrl Pts',(20.8270036818209,19.5496727052252,-16.0673769189932));
#92585=CARTESIAN_POINT('Ctrl Pts',(20.7671076590146,19.8231615861361,-16.0520504590556));
#92586=CARTESIAN_POINT('Ctrl Pts',(20.7139537705473,19.977837431565,-16.0434357244137));
#92587=CARTESIAN_POINT('Ctrl Pts',(20.6297053860372,20.1538811836281,-16.0322254754236));
#92588=CARTESIAN_POINT('Ctrl Pts',(20.6151600109521,20.1825763462623,-16.0303487372091));
#92589=CARTESIAN_POINT('Ctrl Pts',(20.5965589974672,20.2172877598065,-16.0280038204065));
#92590=CARTESIAN_POINT('Ctrl Pts',(20.5931180759991,20.2236307573174,-16.0275722127252));
#92591=CARTESIAN_POINT('Ctrl Pts',(20.5876692368418,20.2335537676982,-16.0268919176751));
#92592=CARTESIAN_POINT('Ctrl Pts',(20.5856831850314,20.2371458127681,-16.0266446047377));
#92593=CARTESIAN_POINT('Ctrl Pts',(20.5819489223078,20.2438535930472,-16.0261807592261));
#92594=CARTESIAN_POINT('Ctrl Pts',(20.5802032662988,20.2469706863496,-16.0259643901107));
#92595=CARTESIAN_POINT('Ctrl Pts',(20.5761971777473,20.2540817896673,-16.0254689128982));
#92596=CARTESIAN_POINT('Ctrl Pts',(20.5739316503172,20.2580728641697,-16.0251894802629));
#92597=CARTESIAN_POINT('Ctrl Pts',(20.5679813929563,20.2684762149334,-16.0244576327782));
#92598=CARTESIAN_POINT('Ctrl Pts',(20.5642760439421,20.2748765408433,-16.0240039368438));
#92599=CARTESIAN_POINT('Ctrl Pts',(20.5397023474197,20.3168148457175,-16.0210090073442));
#92600=CARTESIAN_POINT('Ctrl Pts',(20.5178350509524,20.3517538891273,-16.0184094103354));
#92601=CARTESIAN_POINT('Ctrl Pts',(20.4893125920036,20.3944992071165,-16.01511743289));
#92602=CARTESIAN_POINT('Ctrl Pts',(20.483600294008,20.4029276295792,-16.014462753299));
#92603=CARTESIAN_POINT('Ctrl Pts',(20.4774536526555,20.4118575251865,-16.0137634109665));
#92604=CARTESIAN_POINT('Ctrl Pts',(20.4770795501952,20.4124004812903,-16.0137208668999));
#92605=CARTESIAN_POINT('Ctrl Pts',(20.4637375587464,20.431745119707,-16.0122042876288));
#92606=CARTESIAN_POINT('Ctrl Pts',(20.4504668125158,20.4503354261383,-16.0107197946073));
#92607=CARTESIAN_POINT('Ctrl Pts',(20.4097658760076,20.5054433002699,-16.0062448422303));
#92608=CARTESIAN_POINT('Ctrl Pts',(20.3814524633525,20.5412912911306,-16.0032337198904));
#92609=CARTESIAN_POINT('Ctrl Pts',(20.2814844904335,20.6597714222965,-15.9929934764379));
#92610=CARTESIAN_POINT('Ctrl Pts',(20.2045911633877,20.7377652009908,-15.985762897092));
#92611=CARTESIAN_POINT('Ctrl Pts',(20.0804339735937,20.8455753752534,-15.9751939111193));
#92612=CARTESIAN_POINT('Ctrl Pts',(20.0374614049651,20.8800447231658,-15.9717071118169));
#92613=CARTESIAN_POINT('Ctrl Pts',(19.9656280011274,20.9331954211171,-15.9661528296056));
#92614=CARTESIAN_POINT('Ctrl Pts',(19.9375729784018,20.952917593733,-15.9640469646169));
#92615=CARTESIAN_POINT('Ctrl Pts',(19.9000608371231,20.9779487560198,-15.9613115259344));
#92616=CARTESIAN_POINT('Ctrl Pts',(19.8910258432682,20.9838781647546,-15.9606586341646));
#92617=CARTESIAN_POINT('Ctrl Pts',(19.8761502290105,20.9934784518513,-15.9595932712653));
#92618=CARTESIAN_POINT('Ctrl Pts',(19.8703364510601,20.9971903730249,-15.9591792714499));
#92619=CARTESIAN_POINT('Ctrl Pts',(19.8590454231376,21.0043219140586,-15.9583797716986));
#92620=CARTESIAN_POINT('Ctrl Pts',(19.8535704726723,21.0077450152183,-15.9579941455898));
#92621=CARTESIAN_POINT('Ctrl Pts',(19.8408898479131,21.0155928522036,-15.957105657542));
#92622=CARTESIAN_POINT('Ctrl Pts',(19.8336731230668,21.0199995918204,-15.9566034619942));
#92623=CARTESIAN_POINT('Ctrl Pts',(19.8141869538748,21.0317387072876,-15.9552565934069));
#92624=CARTESIAN_POINT('Ctrl Pts',(19.8018692003457,21.0389903395289,-15.9544148635639));
#92625=CARTESIAN_POINT('Ctrl Pts',(19.687971681656,21.1044991982377,-15.9467174738565));
#92626=CARTESIAN_POINT('Ctrl Pts',(19.5817897004939,21.1543628316632,-15.9401800358359));
#92627=CARTESIAN_POINT('Ctrl Pts',(19.3186486453608,21.2522374761913,-15.9248116575232));
#92628=CARTESIAN_POINT('Ctrl Pts',(19.1592046940596,21.2913012269958,-15.9161664072812));
#92629=CARTESIAN_POINT('Ctrl Pts',(18.9656472654506,21.3155234756884,-15.9049530471375));
#92630=CARTESIAN_POINT('Ctrl Pts',(18.9343369906131,21.3187344156688,-15.9031159327262));
#92631=CARTESIAN_POINT('Ctrl Pts',(18.8958240931573,21.3218181674089,-15.9008151267591));
#92632=CARTESIAN_POINT('Ctrl Pts',(18.8886767214384,21.3223539451003,-15.900386401206));
#92633=CARTESIAN_POINT('Ctrl Pts',(18.8774430127991,21.32313869371,-15.8997096479797));
#92634=CARTESIAN_POINT('Ctrl Pts',(18.8733583629199,21.3234121296327,-15.8994629711669));
#92635=CARTESIAN_POINT('Ctrl Pts',(18.8657059533733,21.3239021079378,-15.898999657603));
#92636=CARTESIAN_POINT('Ctrl Pts',(18.8621384297138,21.3241214631538,-15.8987831802999));
#92637=CARTESIAN_POINT('Ctrl Pts',(18.8539725030067,21.324602803852,-15.8982865782145));
#92638=CARTESIAN_POINT('Ctrl Pts',(18.8493738034868,21.3248588170622,-15.8980061232282));
#92639=CARTESIAN_POINT('Ctrl Pts',(18.8351628067134,21.3256034432128,-15.8971370918124));
#92640=CARTESIAN_POINT('Ctrl Pts',(18.8255481419381,21.3260415043647,-15.8965457955876));
#92641=CARTESIAN_POINT('Ctrl Pts',(18.7294004275695,21.3297653531511,-15.8906016342087));
#92642=CARTESIAN_POINT('Ctrl Pts',(18.6427551834193,21.3278038852054,-15.8849957737045));
#92643=CARTESIAN_POINT('Ctrl Pts',(18.4300104794483,21.3099017019319,-15.8709781227803));
#92644=CARTESIAN_POINT('Ctrl Pts',(18.304739685429,21.287905664406,-15.8625167854829));
#92645=CARTESIAN_POINT('Ctrl Pts',(18.0889889683362,21.2296554581317,-15.8480526034237));
#92646=CARTESIAN_POINT('Ctrl Pts',(17.9976063531014,21.1981431813898,-15.8419579312411));
#92647=CARTESIAN_POINT('Ctrl Pts',(17.8952172026777,21.1547968602301,-15.8351790078744));
#92648=CARTESIAN_POINT('Ctrl Pts',(17.8818109215526,21.148956812298,-15.8342922488543));
#92649=CARTESIAN_POINT('Ctrl Pts',(17.8614116482803,21.1398178554646,-15.832943980679));
#92650=CARTESIAN_POINT('Ctrl Pts',(17.8543746314943,21.1366188523872,-15.8324790671705));
#92651=CARTESIAN_POINT('Ctrl Pts',(17.8415803413249,21.1307178428823,-15.8316340838682));
#92652=CARTESIAN_POINT('Ctrl Pts',(17.8358174453569,21.1280283105296,-15.8312535902115));
#92653=CARTESIAN_POINT('Ctrl Pts',(17.8233758133189,21.1221534058359,-15.8304323332899));
#92654=CARTESIAN_POINT('Ctrl Pts',(17.8167014656391,21.1189588965691,-15.8299918922878));
#92655=CARTESIAN_POINT('Ctrl Pts',(17.7985847175492,21.1101707301395,-15.8287966188649));
#92656=CARTESIAN_POINT('Ctrl Pts',(17.7871757109797,21.1045086451464,-15.8280441741482));
#92657=CARTESIAN_POINT('Ctrl Pts',(17.7311353452366,21.0760636563785,-15.8243486701561));
#92658=CARTESIAN_POINT('Ctrl Pts',(17.6872694614211,21.051803009335,-15.8214579772666));
#92659=CARTESIAN_POINT('Ctrl Pts',(17.4954797346555,20.9366559798244,-15.8087586078297));
#92660=CARTESIAN_POINT('Ctrl Pts',(17.3582177129612,20.8293460645849,-15.7995651219046));
#92661=CARTESIAN_POINT('Ctrl Pts',(17.19129710037,20.6620992066969,-15.786578876898));
#92662=CARTESIAN_POINT('Ctrl Pts',(17.1489969925824,20.615772387948,-15.7830863884505));
#92663=CARTESIAN_POINT('Ctrl Pts',(17.0889996927197,20.5438988842907,-15.7777011350884));
#92664=CARTESIAN_POINT('Ctrl Pts',(17.0697048264685,20.5197271659977,-15.7758951112547));
#92665=CARTESIAN_POINT('Ctrl Pts',(17.0466234949472,20.4894757894566,-15.773628939708));
#92666=CARTESIAN_POINT('Ctrl Pts',(17.0423282298531,20.4837868764361,-15.7732025246463));
#92667=CARTESIAN_POINT('Ctrl Pts',(17.0356167548365,20.4748037986237,-15.7725286112769));
#92668=CARTESIAN_POINT('Ctrl Pts',(17.0331811635899,20.4715240870096,-15.7722824450599));
#92669=CARTESIAN_POINT('Ctrl Pts',(17.0286315565118,20.4653604975651,-15.7718195535131));
#92670=CARTESIAN_POINT('Ctrl Pts',(17.0265153489592,20.4624783065149,-15.7716029843948));
#92671=CARTESIAN_POINT('Ctrl Pts',(17.0216819502108,20.4558603277475,-15.7711054567143));
#92672=CARTESIAN_POINT('Ctrl Pts',(17.0189696857099,20.4521210091549,-15.7708241633042));
#92673=CARTESIAN_POINT('Ctrl Pts',(17.0106032987982,20.4405067282988,-15.769949995944));
#92674=CARTESIAN_POINT('Ctrl Pts',(17.0049911091582,20.432601912176,-15.7693543564931));
#92675=CARTESIAN_POINT('Ctrl Pts',(16.942141667551,20.3427772303528,-15.762580978144));
#92676=CARTESIAN_POINT('Ctrl Pts',(16.8907261578416,20.2569506599535,-15.7560680511294));
#92677=CARTESIAN_POINT('Ctrl Pts',(16.768406338946,20.0155354424814,-15.738236566643));
#92678=CARTESIAN_POINT('Ctrl Pts',(16.7099350762936,19.8544398915282,-15.7269007125148));
#92679=CARTESIAN_POINT('Ctrl Pts',(16.6614520672809,19.6448237544999,-15.7134187937563));
#92680=CARTESIAN_POINT('Ctrl Pts',(16.6528139418684,19.6012858439423,-15.7106795639875));
#92681=CARTESIAN_POINT('Ctrl Pts',(16.6436144406144,19.5458388846826,-15.7072652732538));
#92682=CARTESIAN_POINT('Ctrl Pts',(16.6417764781134,19.5341557038691,-15.706549965101));
#92683=CARTESIAN_POINT('Ctrl Pts',(16.6389885125918,19.51541190343,-15.7054088058363));
#92684=CARTESIAN_POINT('Ctrl Pts',(16.6379760960099,19.5083609509589,-15.7049809854188));
#92685=CARTESIAN_POINT('Ctrl Pts',(16.6361227657874,19.4949735293922,-15.7041714108607));
#92686=CARTESIAN_POINT('Ctrl Pts',(16.635274926426,19.4886381136652,-15.7037894418225));
#92687=CARTESIAN_POINT('Ctrl Pts',(16.6334140698746,19.4742372053294,-15.702923765898));
#92688=CARTESIAN_POINT('Ctrl Pts',(16.6324187836035,19.4661694923306,-15.7024406236861));
#92689=CARTESIAN_POINT('Ctrl Pts',(16.6299653959363,19.4452937279088,-15.701195073411));
#92690=CARTESIAN_POINT('Ctrl Pts',(16.6285777518862,19.4324776155075,-15.7004348865106));
#92691=CARTESIAN_POINT('Ctrl Pts',(16.6203967177256,19.3498752954838,-15.6955629102487));
#92692=CARTESIAN_POINT('Ctrl Pts',(16.616956381725,19.2797966609927,-15.691558250133));
#92693=CARTESIAN_POINT('Ctrl Pts',(16.6171212268841,19.0172834136081,-15.676859263182));
#92694=CARTESIAN_POINT('Ctrl Pts',(16.6434647892515,18.8258343582239,-15.6668249337217));
#92695=CARTESIAN_POINT('Ctrl Pts',(16.7087052425926,18.5926572672549,-15.6531662107904));
#92696=CARTESIAN_POINT('Ctrl Pts',(16.723802096131,18.5452146498781,-15.6503027130819));
#92697=CARTESIAN_POINT('Ctrl Pts',(16.742161444939,18.4938591918365,-15.6470652126431));
#92698=CARTESIAN_POINT('Ctrl Pts',(16.7437828789803,18.489371578843,-15.6467811375154));
#92699=CARTESIAN_POINT('Ctrl Pts',(16.7454194503191,18.4848895418528,-15.6464962064494));
#92700=CARTESIAN_POINT('Origin',(18.734,19.211,0.));
#92701=CARTESIAN_POINT('',(16.7454194448477,18.4848895568371,-14.8438385225655));
#92702=CARTESIAN_POINT('',(16.7486736478041,18.4860706551708,-15.066381399058));
#92703=CARTESIAN_POINT('',(16.7454194503191,18.4848895418526,0.));
#92704=CARTESIAN_POINT('',(16.6156459487826,19.212740575031,-15.1109429532718));
#92705=CARTESIAN_POINT('Ctrl Pts',(16.7486736478041,18.4860706551708,-15.066381399058));
#92706=CARTESIAN_POINT('Ctrl Pts',(16.6638907080669,18.7190472863516,-15.0812352504626));
#92707=CARTESIAN_POINT('Ctrl Pts',(16.6178442115102,18.9662441554235,-15.0960891018672));
#92708=CARTESIAN_POINT('Ctrl Pts',(16.6156459487826,19.212740575031,-15.1109429532718));
#92709=CARTESIAN_POINT('Ctrl Pts',(16.6170007608289,19.212794811659,-15.1101643053096));
#92710=CARTESIAN_POINT('Ctrl Pts',(16.6170691197604,19.2934248907551,-15.1145731285289));
#92711=CARTESIAN_POINT('Ctrl Pts',(16.6217438740534,19.3739800238093,-15.1190366797522));
#92712=CARTESIAN_POINT('Ctrl Pts',(16.6337248047666,19.4776387155272,-15.1250697176005));
#92713=CARTESIAN_POINT('Ctrl Pts',(16.6368453917013,19.5011629633464,-15.1264584526702));
#92714=CARTESIAN_POINT('Ctrl Pts',(16.6412432748791,19.5305211890863,-15.1282216951713));
#92715=CARTESIAN_POINT('Ctrl Pts',(16.6421508377164,19.5364098664599,-15.1285768878127));
#92716=CARTESIAN_POINT('Ctrl Pts',(16.643715780129,19.5462867698596,-15.1291753145913));
#92717=CARTESIAN_POINT('Ctrl Pts',(16.6443597513821,19.5502771265929,-15.1294178177132));
#92718=CARTESIAN_POINT('Ctrl Pts',(16.6455594680068,19.5575781495653,-15.1298629008675));
#92719=CARTESIAN_POINT('Ctrl Pts',(16.6461116697319,19.5608893959485,-15.1300652817493));
#92720=CARTESIAN_POINT('Ctrl Pts',(16.6472681665132,19.567724031502,-15.130484112733));
#92721=CARTESIAN_POINT('Ctrl Pts',(16.6478735058963,19.5712471782848,-15.1307006235895));
#92722=CARTESIAN_POINT('Ctrl Pts',(16.64928005852,19.5793110447164,-15.1311975665018));
#92723=CARTESIAN_POINT('Ctrl Pts',(16.6500871823861,19.5838506775108,-15.1314783304732));
#92724=CARTESIAN_POINT('Ctrl Pts',(16.6526294587065,19.5978834459161,-15.1323492524446));
#92725=CARTESIAN_POINT('Ctrl Pts',(16.6544146697914,19.6073672251524,-15.1329421470191));
#92726=CARTESIAN_POINT('Ctrl Pts',(16.673431573657,19.7047264393825,-15.139070638307));
#92727=CARTESIAN_POINT('Ctrl Pts',(16.6961558788501,19.7914271088415,-15.1448764765017));
#92728=CARTESIAN_POINT('Ctrl Pts',(16.738599780215,19.9196167563596,-15.1537504328869));
#92729=CARTESIAN_POINT('Ctrl Pts',(16.7542920844716,19.9623429485463,-15.1567594503444));
#92730=CARTESIAN_POINT('Ctrl Pts',(16.7857100315866,20.0400495149138,-15.1622978990167));
#92731=CARTESIAN_POINT('Ctrl Pts',(16.8010330167755,20.0751733743205,-15.1648270609592));
#92732=CARTESIAN_POINT('Ctrl Pts',(16.8576523026906,20.1959061170435,-15.1735859373226));
#92733=CARTESIAN_POINT('Ctrl Pts',(16.9037553976654,20.279142813405,-15.1797350589487));
#92734=CARTESIAN_POINT('Ctrl Pts',(16.98037113813,20.3978496151008,-15.1886008559529));
#92735=CARTESIAN_POINT('Ctrl Pts',(17.0067076175732,20.4358623371365,-15.1914572270433));
#92736=CARTESIAN_POINT('Ctrl Pts',(17.0414157633168,20.4826097334158,-15.194994936695));
#92737=CARTESIAN_POINT('Ctrl Pts',(17.0486437876414,20.4921741330187,-15.1957201364725));
#92738=CARTESIAN_POINT('Ctrl Pts',(17.0603173995666,20.5073513426466,-15.1968733046793));
#92739=CARTESIAN_POINT('Ctrl Pts',(17.0647108123106,20.51300378663,-15.1973033161713));
#92740=CARTESIAN_POINT('Ctrl Pts',(17.0730769268785,20.5236554448443,-15.1981147104128));
#92741=CARTESIAN_POINT('Ctrl Pts',(17.0770437298117,20.5286591713228,-15.198496321254));
#92742=CARTESIAN_POINT('Ctrl Pts',(17.0860738393375,20.5399444917881,-15.1993580650651));
#92743=CARTESIAN_POINT('Ctrl Pts',(17.0911505572635,20.5462152652305,-15.1998376533312));
#92744=CARTESIAN_POINT('Ctrl Pts',(17.1062386171615,20.5646357397032,-15.2012488100003));
#92745=CARTESIAN_POINT('Ctrl Pts',(17.1163499124345,20.5767031337094,-15.2021763243838));
#92746=CARTESIAN_POINT('Ctrl Pts',(17.2076552505965,20.6832352123291,-15.2103952542774));
#92747=CARTESIAN_POINT('Ctrl Pts',(17.2969087698296,20.7704805616849,-15.2173237787246));
#92748=CARTESIAN_POINT('Ctrl Pts',(17.5230057614327,20.9554937227271,-15.2332793356579));
#92749=CARTESIAN_POINT('Ctrl Pts',(17.6648036943985,21.0458212970044,-15.2421392555806));
#92750=CARTESIAN_POINT('Ctrl Pts',(17.8351453836605,21.1278237449123,-15.2531373168278));
#92751=CARTESIAN_POINT('Ctrl Pts',(17.8546924769311,21.1368689179489,-15.2544048484744));
#92752=CARTESIAN_POINT('Ctrl Pts',(17.8801232774212,21.1481688446537,-15.2560652200103));
#92753=CARTESIAN_POINT('Ctrl Pts',(17.8858845389524,21.1506981086003,-15.2564421137673));
#92754=CARTESIAN_POINT('Ctrl Pts',(17.8947422388003,21.1545397397834,-15.257022836009));
#92755=CARTESIAN_POINT('Ctrl Pts',(17.8978307301784,21.1558704999805,-15.2572255563272));
#92756=CARTESIAN_POINT('Ctrl Pts',(17.9042045086151,21.1585988264718,-15.2576444238103));
#92757=CARTESIAN_POINT('Ctrl Pts',(17.9074901355794,21.1599954309256,-15.2578606286241));
#92758=CARTESIAN_POINT('Ctrl Pts',(17.9149829265378,21.1631579987719,-15.2583543127009));
#92759=CARTESIAN_POINT('Ctrl Pts',(17.9191922603767,21.1649186690701,-15.2586321074155));
#92760=CARTESIAN_POINT('Ctrl Pts',(17.9301580868714,21.1694638323502,-15.2593569044156));
#92761=CARTESIAN_POINT('Ctrl Pts',(17.9369232980745,21.1722269454673,-15.2598051486424));
#92762=CARTESIAN_POINT('Ctrl Pts',(17.9802281062826,21.1896528437242,-15.2626807311095));
#92763=CARTESIAN_POINT('Ctrl Pts',(18.017153974243,21.2033279007886,-15.2651613189248));
#92764=CARTESIAN_POINT('Ctrl Pts',(18.2352196800195,21.2772391545958,-15.279889625781));
#92765=CARTESIAN_POINT('Ctrl Pts',(18.4234627722836,21.3137848053859,-15.292819965755));
#92766=CARTESIAN_POINT('Ctrl Pts',(18.6690771857391,21.3277214028344,-15.3086327479154));
#92767=CARTESIAN_POINT('Ctrl Pts',(18.7241880123992,21.3286942684755,-15.3121215554525));
#92768=CARTESIAN_POINT('Ctrl Pts',(18.8135709767503,21.3267821271883,-15.3176786619517));
#92769=CARTESIAN_POINT('Ctrl Pts',(18.8478425684395,21.3252151347389,-15.3197853916697));
#92770=CARTESIAN_POINT('Ctrl Pts',(18.8928443013813,21.3220599954916,-15.3225217722703));
#92771=CARTESIAN_POINT('Ctrl Pts',(18.903620215058,21.3212215064005,-15.3231747613143));
#92772=CARTESIAN_POINT('Ctrl Pts',(18.921262260065,21.3197127418703,-15.3242402423033));
#92773=CARTESIAN_POINT('Ctrl Pts',(18.9281322748977,21.3190913745296,-15.3246542635876));
#92774=CARTESIAN_POINT('Ctrl Pts',(18.941426786433,21.3178233950745,-15.3254537767271));
#92775=CARTESIAN_POINT('Ctrl Pts',(18.94785159488,21.3171809481989,-15.3258393949022));
#92776=CARTESIAN_POINT('Ctrl Pts',(18.9626822979287,21.3156293948725,-15.3267278245541));
#92777=CARTESIAN_POINT('Ctrl Pts',(18.971085922556,21.31469930162,-15.3272299699215));
#92778=CARTESIAN_POINT('Ctrl Pts',(18.9936776825545,21.3120618058809,-15.3285766148951));
#92779=CARTESIAN_POINT('Ctrl Pts',(19.0078546294512,21.3102610289786,-15.3294181728522));
#92780=CARTESIAN_POINT('Ctrl Pts',(19.1377965712587,21.2924168454141,-15.337102041364));
#92781=CARTESIAN_POINT('Ctrl Pts',(19.2520722511782,21.2669557788185,-15.3436274674306));
#92782=CARTESIAN_POINT('Ctrl Pts',(19.5191932517011,21.1837376537684,-15.3589439081253));
#92783=CARTESIAN_POINT('Ctrl Pts',(19.6685807115964,21.1175070858719,-15.3675514160382));
#92784=CARTESIAN_POINT('Ctrl Pts',(19.8367388909741,21.0184018770823,-15.3787610362288));
#92785=CARTESIAN_POINT('Ctrl Pts',(19.8642150773718,21.0013486332106,-15.3806472681951));
#92786=CARTESIAN_POINT('Ctrl Pts',(19.8973404289251,20.9797227842018,-15.3830027492314));
#92787=CARTESIAN_POINT('Ctrl Pts',(19.9033722574255,20.9757407064675,-15.3834350373594));
#92788=CARTESIAN_POINT('Ctrl Pts',(19.9127993871593,20.9694475747342,-15.3841161685256));
#92789=CARTESIAN_POINT('Ctrl Pts',(19.916208621062,20.9671573516867,-15.3843636315422));
#92790=CARTESIAN_POINT('Ctrl Pts',(19.9225706730188,20.9628565913669,-15.3848276035793));
#92791=CARTESIAN_POINT('Ctrl Pts',(19.9255250739641,20.960848495994,-15.3850439481982));
#92792=CARTESIAN_POINT('Ctrl Pts',(19.9322601965055,20.9562456926736,-15.3855391646632));
#92793=CARTESIAN_POINT('Ctrl Pts',(19.9360375663805,20.9536461816506,-15.38581835973));
#92794=CARTESIAN_POINT('Ctrl Pts',(19.9476314937909,20.9456118395016,-15.3866797057842));
#92795=CARTESIAN_POINT('Ctrl Pts',(19.9554197332402,20.940136623848,-15.3872645088872));
#92796=CARTESIAN_POINT('Ctrl Pts',(20.0608327242514,20.8649626507338,-15.3952614107075));
#92797=CARTESIAN_POINT('Ctrl Pts',(20.1523877659229,20.7871494252094,-15.4031531095498));
#92798=CARTESIAN_POINT('Ctrl Pts',(20.3135179904146,20.6247401417072,-15.4182672139133));
#92799=CARTESIAN_POINT('Ctrl Pts',(20.3841163943823,20.5416606007797,-15.4254618019288));
#92800=CARTESIAN_POINT('Ctrl Pts',(20.4919507452078,20.3929060549428,-15.4372653250561));
#92801=CARTESIAN_POINT('Ctrl Pts',(20.5326447102117,20.3300049524239,-15.4419746596193));
#92802=CARTESIAN_POINT('Ctrl Pts',(20.5792769856146,20.2487835409625,-15.4477119319991));
#92803=CARTESIAN_POINT('Ctrl Pts',(20.5884126207073,20.2323695214722,-15.4488547983053));
#92804=CARTESIAN_POINT('Ctrl Pts',(20.6013870623139,20.208310213105,-15.4505064814297));
#92805=CARTESIAN_POINT('Ctrl Pts',(20.6053997217216,20.2007601661773,-15.4510214756272));
#92806=CARTESIAN_POINT('Ctrl Pts',(20.6123583853641,20.1874734301005,-15.4519220347232));
#92807=CARTESIAN_POINT('Ctrl Pts',(20.6153241017789,20.1817472426193,-15.4523082940495));
#92808=CARTESIAN_POINT('Ctrl Pts',(20.6210346052342,20.1705969733215,-15.4530568754688));
#92809=CARTESIAN_POINT('Ctrl Pts',(20.623782281851,20.165174449955,-15.453419296536));
#92810=CARTESIAN_POINT('Ctrl Pts',(20.6302989861685,20.1521752043832,-15.4542842819653));
#92811=CARTESIAN_POINT('Ctrl Pts',(20.6340460340923,20.1445875330033,-15.4547860742798));
#92812=CARTESIAN_POINT('Ctrl Pts',(20.6474264613079,20.1170782740257,-15.4565943426743));
#92813=CARTESIAN_POINT('Ctrl Pts',(20.6567930564118,20.0970279782003,-15.4578915650937));
#92814=CARTESIAN_POINT('Ctrl Pts',(20.7416650400087,19.9076620830962,-15.4699604304115));
#92815=CARTESIAN_POINT('Ctrl Pts',(20.7949366097104,19.7292695186358,-15.4798776729096));
#92816=CARTESIAN_POINT('Ctrl Pts',(20.8370036304495,19.466946153904,-15.4943601181923));
#92817=CARTESIAN_POINT('Ctrl Pts',(20.8451946785674,19.3870332888556,-15.4987741917299));
#92818=CARTESIAN_POINT('Ctrl Pts',(20.850461770287,19.2708271156551,-15.5054278730004));
#92819=CARTESIAN_POINT('Ctrl Pts',(20.8511737220716,19.2347653081696,-15.5075256032415));
#92820=CARTESIAN_POINT('Ctrl Pts',(20.8509209260533,19.1912371681383,-15.5101160388122));
#92821=CARTESIAN_POINT('Ctrl Pts',(20.8508380342263,19.1837693230324,-15.5105625389141));
#92822=CARTESIAN_POINT('Ctrl Pts',(20.8506474517536,19.1721429693674,-15.5112611222685));
#92823=CARTESIAN_POINT('Ctrl Pts',(20.85056701431,19.1679839902409,-15.5115117064976));
#92824=CARTESIAN_POINT('Ctrl Pts',(20.8503948597539,19.1602603412614,-15.5119783873891));
#92825=CARTESIAN_POINT('Ctrl Pts',(20.8503063939365,19.1566956563464,-15.512194300298));
#92826=CARTESIAN_POINT('Ctrl Pts',(20.8500856425717,19.1486229796412,-15.512684448632));
#92827=CARTESIAN_POINT('Ctrl Pts',(20.8499479582416,19.144115199711,-15.512958981371));
#92828=CARTESIAN_POINT('Ctrl Pts',(20.849497605133,19.1307684033944,-15.5137742286541));
#92829=CARTESIAN_POINT('Ctrl Pts',(20.8491439508148,19.1219309959322,-15.5143171527537));
#92830=CARTESIAN_POINT('Ctrl Pts',(20.8461180363622,19.0565708177643,-15.5183543269264));
#92831=CARTESIAN_POINT('Ctrl Pts',(20.8412360822994,19.0001781445165,-15.5219577233054));
#92832=CARTESIAN_POINT('Ctrl Pts',(20.8130482446981,18.7784200373076,-15.5364346135072));
#92833=CARTESIAN_POINT('Ctrl Pts',(20.7724738455468,18.6158537801209,-15.5476702297927));
#92834=CARTESIAN_POINT('Ctrl Pts',(20.6924624647145,18.4050638743508,-15.5622010112452));
#92835=CARTESIAN_POINT('Ctrl Pts',(20.6694539963057,18.3512750079729,-15.565912287619));
#92836=CARTESIAN_POINT('Ctrl Pts',(20.6288110695379,18.2661919181628,-15.5717806675225));
#92837=CARTESIAN_POINT('Ctrl Pts',(20.6125580912548,18.2342753487285,-15.5739817853825));
#92838=CARTESIAN_POINT('Ctrl Pts',(20.5902741696631,18.193131774859,-15.5768207007394));
#92839=CARTESIAN_POINT('Ctrl Pts',(20.5849708416758,18.1835193592641,-15.5774840790439));
#92840=CARTESIAN_POINT('Ctrl Pts',(20.5761955106883,18.1679023061202,-15.5785621703011));
#92841=CARTESIAN_POINT('Ctrl Pts',(20.5727683978061,18.1618728010446,-15.5789784830163));
#92842=CARTESIAN_POINT('Ctrl Pts',(20.5661006471687,18.1502749061132,-15.579779464103));
#92843=CARTESIAN_POINT('Ctrl Pts',(20.5628641031591,18.1447042625287,-15.5801642743378));
#92844=CARTESIAN_POINT('Ctrl Pts',(20.5553663865783,18.1319339798337,-15.5810466685782));
#92845=CARTESIAN_POINT('Ctrl Pts',(20.5510878476226,18.1247446215906,-15.5815436155439));
#92846=CARTESIAN_POINT('Ctrl Pts',(20.5395434907498,18.1056053700408,-15.5828671818466));
#92847=CARTESIAN_POINT('Ctrl Pts',(20.5322016118998,18.0937016683609,-15.5836910170113));
#92848=CARTESIAN_POINT('Ctrl Pts',(20.4710613330323,17.9967362084341,-15.590409223576));
#92849=CARTESIAN_POINT('Ctrl Pts',(20.4113743223814,17.9155318379454,-15.5960735879851));
#92850=CARTESIAN_POINT('Ctrl Pts',(20.2350899268049,17.7084129682052,-15.6110568404912));
#92851=CARTESIAN_POINT('Ctrl Pts',(20.1086392270318,17.5919279864943,-15.6200635473757));
#92852=CARTESIAN_POINT('Ctrl Pts',(19.9371702672619,17.468685230952,-15.632094787001));
#92853=CARTESIAN_POINT('Ctrl Pts',(19.9041378002494,17.446331047384,-15.6344077557125));
#92854=CARTESIAN_POINT('Ctrl Pts',(19.8640122976131,17.4207988179777,-15.6372367510775));
#92855=CARTESIAN_POINT('Ctrl Pts',(19.8575059829887,17.416708394112,-15.6376960635362));
#92856=CARTESIAN_POINT('Ctrl Pts',(19.8474039941651,17.4104339102215,-15.6384103607666));
#92857=CARTESIAN_POINT('Ctrl Pts',(19.8438237620606,17.4082249407255,-15.6386637355539));
#92858=CARTESIAN_POINT('Ctrl Pts',(19.8372000634862,17.4041653901539,-15.6391329522938));
#92859=CARTESIAN_POINT('Ctrl Pts',(19.8341585013622,17.4023118127388,-15.6393485935521));
#92860=CARTESIAN_POINT('Ctrl Pts',(19.8273073388361,17.3981602783709,-15.6398347296075));
#92861=CARTESIAN_POINT('Ctrl Pts',(19.8234951890574,17.3958666644972,-15.6401055007096));
#92862=CARTESIAN_POINT('Ctrl Pts',(19.8137223624237,17.3900286347835,-15.6408002905011));
#92863=CARTESIAN_POINT('Ctrl Pts',(19.8077515007968,17.3865014923688,-15.6412253907565));
#92864=CARTESIAN_POINT('Ctrl Pts',(19.7727681064537,17.3660670996981,-15.6437191087663));
#92865=CARTESIAN_POINT('Ctrl Pts',(19.743375659397,17.3498237397996,-15.6458264339797));
#92866=CARTESIAN_POINT('Ctrl Pts',(19.6974282277872,17.3258399798626,-15.6491249626217));
#92867=CARTESIAN_POINT('Ctrl Pts',(19.6811369202531,17.3176025589441,-15.6502953209886));
#92868=CARTESIAN_POINT('Ctrl Pts',(19.6425584282783,17.2987184873438,-15.6530654176598));
#92869=CARTESIAN_POINT('Ctrl Pts',(19.6201875387926,17.2882492150893,-15.6546706773384));
#92870=CARTESIAN_POINT('Ctrl Pts',(19.5566270888549,17.2598486761793,-15.6592195096192));
#92871=CARTESIAN_POINT('Ctrl Pts',(19.5150429438074,17.2428337071169,-15.6621813147283));
#92872=CARTESIAN_POINT('Ctrl Pts',(19.3704830907159,17.188987511668,-15.6723715592087));
#92873=CARTESIAN_POINT('Ctrl Pts',(19.2652050271064,17.1588133823372,-15.6796015915757));
#92874=CARTESIAN_POINT('Ctrl Pts',(19.1041215716146,17.125878870974,-15.6901694287262));
#92875=CARTESIAN_POINT('Ctrl Pts',(19.0497690519771,17.1169582560398,-15.6936556299833));
#92876=CARTESIAN_POINT('Ctrl Pts',(18.961105536361,17.1059376743791,-15.699209071197));
#92877=CARTESIAN_POINT('Ctrl Pts',(18.9269852600988,17.1025358137451,-15.7013146787371));
#92878=CARTESIAN_POINT('Ctrl Pts',(18.882020100502,17.0991534568251,-15.7040498370852));
#92879=CARTESIAN_POINT('Ctrl Pts',(18.8712382299633,17.0984253984557,-15.7047026999878));
#92880=CARTESIAN_POINT('Ctrl Pts',(18.8535659125318,17.0973679203593,-15.7057680279105));
#92881=CARTESIAN_POINT('Ctrl Pts',(18.8466786918907,17.0969895720051,-15.7061820214219));
#92882=CARTESIAN_POINT('Ctrl Pts',(18.833340804196,17.0963222238964,-15.706981517379));
#92883=CARTESIAN_POINT('Ctrl Pts',(18.8268904305305,17.0960290636828,-15.7073671459535));
#92884=CARTESIAN_POINT('Ctrl Pts',(18.811989926927,17.0954201567187,-15.70825565166));
#92885=CARTESIAN_POINT('Ctrl Pts',(18.8035390085454,17.0951255161387,-15.7087578623163));
#92886=CARTESIAN_POINT('Ctrl Pts',(18.7807983227276,17.0944690557678,-15.7101047980134));
#92887=CARTESIAN_POINT('Ctrl Pts',(18.7665061253851,17.0942013114992,-15.7109465793941));
#92888=CARTESIAN_POINT('Ctrl Pts',(18.6350479161247,17.0930703660303,-15.718648079815));
#92889=CARTESIAN_POINT('Ctrl Pts',(18.5179952210324,17.1017905082359,-15.7251891697428));
#92890=CARTESIAN_POINT('Ctrl Pts',(18.2404051691153,17.145834873476,-15.7405740963719));
#92891=CARTESIAN_POINT('Ctrl Pts',(18.08210787952,17.1902161995463,-15.7492315175644));
#92892=CARTESIAN_POINT('Ctrl Pts',(17.901668165526,17.264237029948,-15.760446319959));
#92893=CARTESIAN_POINT('Ctrl Pts',(17.8730709881215,17.2767137367901,-15.7622678352236));
#92894=CARTESIAN_POINT('Ctrl Pts',(17.8382748814437,17.2928194544098,-15.764551266668));
#92895=CARTESIAN_POINT('Ctrl Pts',(17.8318034323742,17.2958547199911,-15.7649788385074));
#92896=CARTESIAN_POINT('Ctrl Pts',(17.8216539246104,17.3006779426256,-15.7656541737725));
#92897=CARTESIAN_POINT('Ctrl Pts',(17.8179653947633,17.3024439160643,-15.7659005957242));
#92898=CARTESIAN_POINT('Ctrl Pts',(17.8110620178731,17.3057736979643,-15.7663636981294));
#92899=CARTESIAN_POINT('Ctrl Pts',(17.8078460072386,17.3073349659571,-15.7665802207487));
#92900=CARTESIAN_POINT('Ctrl Pts',(17.800489613972,17.3109293078088,-15.7670772824539));
#92901=CARTESIAN_POINT('Ctrl Pts',(17.7963519234447,17.3129677664095,-15.7673581540515));
#92902=CARTESIAN_POINT('Ctrl Pts',(17.7855281696195,17.3183441853468,-15.768096212688));
#92903=CARTESIAN_POINT('Ctrl Pts',(17.7788531288448,17.321704020938,-15.7685547157601));
#92904=CARTESIAN_POINT('Ctrl Pts',(17.7341721533976,17.3444911856123,-15.77164558563));
#92905=CARTESIAN_POINT('Ctrl Pts',(17.696746216713,17.3650273842549,-15.7743405504313));
#92906=CARTESIAN_POINT('Ctrl Pts',(17.6537624983241,17.3903331382943,-15.7775396677328));
#92907=CARTESIAN_POINT('Ctrl Pts',(17.6475741898257,17.3940190319585,-15.7780028227472));
#92908=CARTESIAN_POINT('Ctrl Pts',(17.506733216783,17.4788837808983,-15.788601064497));
#92909=CARTESIAN_POINT('Ctrl Pts',(17.3815204068972,17.5747809998755,-15.7991743180983));
#92910=CARTESIAN_POINT('Ctrl Pts',(17.1996368765667,17.7493510037903,-15.8155534463536));
#92911=CARTESIAN_POINT('Ctrl Pts',(17.1356824256298,17.819571561161,-15.8215790722409));
#92912=CARTESIAN_POINT('Ctrl Pts',(17.063376756453,17.9105531859024,-15.8287171504957));
#92913=CARTESIAN_POINT('Ctrl Pts',(17.0503589587253,17.9274514677791,-15.8300171974182));
#92914=CARTESIAN_POINT('Ctrl Pts',(17.0322147377083,17.9517554217632,-15.8318514236441));
#92915=CARTESIAN_POINT('Ctrl Pts',(17.0268770682142,17.9590010836857,-15.8323938569715));
#92916=CARTESIAN_POINT('Ctrl Pts',(17.0177495690614,17.9715581794582,-15.833326444012));
#92917=CARTESIAN_POINT('Ctrl Pts',(17.013937824724,17.9768534597266,-15.833717444985));
#92918=CARTESIAN_POINT('Ctrl Pts',(17.0066870488709,17.9870250931465,-15.8344642231734));
#92919=CARTESIAN_POINT('Ctrl Pts',(17.003244040454,17.9918985221222,-15.8348201512138));
#92920=CARTESIAN_POINT('Ctrl Pts',(16.9943461593564,18.0046067587536,-15.8357434892715));
#92921=CARTESIAN_POINT('Ctrl Pts',(16.9889235577931,18.0124640793104,-15.8363096631929));
#92922=CARTESIAN_POINT('Ctrl Pts',(16.9706219355146,18.0393705675953,-15.8382327210528));
#92923=CARTESIAN_POINT('Ctrl Pts',(16.9579999147849,18.0585931779762,-15.839579912918));
#92924=CARTESIAN_POINT('Ctrl Pts',(16.8645247598485,18.2061350475879,-15.8497291248369));
#92925=CARTESIAN_POINT('Ctrl Pts',(16.7973961927158,18.3425421376678,-15.857987029616));
#92926=CARTESIAN_POINT('Ctrl Pts',(16.7454194505387,18.4848895412513,-15.8662164192772));
#92927=CARTESIAN_POINT('',(16.6170002518853,19.2099672937205,-14.8907771687908));
#92928=CARTESIAN_POINT('Ctrl Pts',(16.7454194503191,18.4848895418528,-15.6464962064494));
#92929=CARTESIAN_POINT('Ctrl Pts',(16.7464618212973,18.4820348265275,-15.646314727117));
#92930=CARTESIAN_POINT('Ctrl Pts',(16.7475103330494,18.4791823732292,-15.6461329005545));
#92931=CARTESIAN_POINT('Ctrl Pts',(16.7501831765914,18.4719590306671,-15.6456711873015));
#92932=CARTESIAN_POINT('Ctrl Pts',(16.7518158016389,18.4675912658523,-15.645390821652));
#92933=CARTESIAN_POINT('Ctrl Pts',(16.7547310336454,18.4598700180448,-15.6448930464087));
#92934=CARTESIAN_POINT('Ctrl Pts',(16.7560077574923,18.4565143610466,-15.6446759903617));
#92935=CARTESIAN_POINT('Ctrl Pts',(16.7587298590392,18.4494141674561,-15.6442151703432));
#92936=CARTESIAN_POINT('Ctrl Pts',(16.760177328531,18.4456705473598,-15.6439712873832));
#92937=CARTESIAN_POINT('Ctrl Pts',(16.7641078952561,18.4355901623563,-15.6433121688402));
#92938=CARTESIAN_POINT('Ctrl Pts',(16.7666108942137,18.429261281392,-15.6428957641459));
#92939=CARTESIAN_POINT('Ctrl Pts',(16.7791207398447,18.398070525457,-15.640831204365));
#92940=CARTESIAN_POINT('Ctrl Pts',(16.7895680677611,18.373389375823,-15.6391585768968));
#92941=CARTESIAN_POINT('Ctrl Pts',(16.8210382189566,18.3028068679415,-15.6342757171667));
#92942=CARTESIAN_POINT('Ctrl Pts',(16.8432373330588,18.2574522047139,-15.6310148787141));
#92943=CARTESIAN_POINT('Ctrl Pts',(16.9295816583965,18.0959373868848,-15.6190523488454));
#92944=CARTESIAN_POINT('Ctrl Pts',(17.002989257499,17.9850738644353,-15.6101841461185));
#92945=CARTESIAN_POINT('Ctrl Pts',(17.1511162430004,17.801451616154,-15.5948582198333));
#92946=CARTESIAN_POINT('Ctrl Pts',(17.2217357581854,17.7259377182922,-15.5883172744764));
#92947=CARTESIAN_POINT('Ctrl Pts',(17.3079107837369,17.6463416503839,-15.5811566207662));
#92948=CARTESIAN_POINT('Ctrl Pts',(17.3183213375557,17.6369160939192,-15.5803038124706));
#92949=CARTESIAN_POINT('Ctrl Pts',(17.3350950535145,17.6220304524294,-15.5789489199586));
#92950=CARTESIAN_POINT('Ctrl Pts',(17.3413980608891,17.6165034917723,-15.5784440350067));
#92951=CARTESIAN_POINT('Ctrl Pts',(17.3526049390447,17.6067935837632,-15.5775537343629));
#92952=CARTESIAN_POINT('Ctrl Pts',(17.3574953646643,17.6025953461111,-15.5771676859683));
#92953=CARTESIAN_POINT('Ctrl Pts',(17.3676821966819,17.5939308432624,-15.5763685838711));
#92954=CARTESIAN_POINT('Ctrl Pts',(17.3729815139306,17.5894681071075,-15.575955678056));
#92955=CARTESIAN_POINT('Ctrl Pts',(17.3867089330075,17.5780224830243,-15.5748932018281));
#92956=CARTESIAN_POINT('Ctrl Pts',(17.3951695181801,17.5710787403345,-15.5742452292214));
#92957=CARTESIAN_POINT('Ctrl Pts',(17.4313068150247,17.5418863312755,-15.5715060262037));
#92958=CARTESIAN_POINT('Ctrl Pts',(17.4594880963102,17.520269507589,-15.5694401343146));
#92959=CARTESIAN_POINT('Ctrl Pts',(17.5349316129331,17.4653584015064,-15.5640773301655));
#92960=CARTESIAN_POINT('Ctrl Pts',(17.5830375239335,17.4332723228912,-15.5608243484111));
#92961=CARTESIAN_POINT('Ctrl Pts',(17.770793085422,17.318862031781,-15.5486248546165));
#92962=CARTESIAN_POINT('Ctrl Pts',(17.918401471303,17.25070735247,-15.5400738399266));
#92963=CARTESIAN_POINT('Ctrl Pts',(18.0929193608975,17.1932848495841,-15.5298130893036));
#92964=CARTESIAN_POINT('Ctrl Pts',(18.113610929582,17.1868270419296,-15.5285934990093));
#92965=CARTESIAN_POINT('Ctrl Pts',(18.1746753193025,17.1687931780516,-15.5249758283697));
#92966=CARTESIAN_POINT('Ctrl Pts',(18.215295288226,17.1581001743488,-15.5225459138842));
#92967=CARTESIAN_POINT('Ctrl Pts',(18.2634485671725,17.1469443654395,-15.5196092826258));
#92968=CARTESIAN_POINT('Ctrl Pts',(18.2707026486073,17.1453040218832,-15.519165406912));
#92969=CARTESIAN_POINT('Ctrl Pts',(18.2824589271604,17.1427106496649,-15.5184434203876));
#92970=CARTESIAN_POINT('Ctrl Pts',(18.2869559243674,17.1417340019477,-15.5181666274569));
#92971=CARTESIAN_POINT('Ctrl Pts',(18.2949509737732,17.1400249336552,-15.5176733698364));
#92972=CARTESIAN_POINT('Ctrl Pts',(18.2984477327466,17.1392867005484,-15.5174572411903));
#92973=CARTESIAN_POINT('Ctrl Pts',(18.3059565647136,17.1377212927563,-15.5169922697591));
#92974=CARTESIAN_POINT('Ctrl Pts',(18.3099691142896,17.1368969197004,-15.5167432765022));
#92975=CARTESIAN_POINT('Ctrl Pts',(18.3210204168516,17.1346598535017,-15.5160561123951));
#92976=CARTESIAN_POINT('Ctrl Pts',(18.3280639262587,17.1332713264984,-15.5156165998363));
#92977=CARTESIAN_POINT('Ctrl Pts',(18.3661847547162,17.1259575888047,-15.5132300022163));
#92978=CARTESIAN_POINT('Ctrl Pts',(18.39738310792,17.1206941060276,-15.5112485866999));
#92979=CARTESIAN_POINT('Ctrl Pts',(18.5904484628164,17.0925559980764,-15.498861442055));
#92980=CARTESIAN_POINT('Ctrl Pts',(18.7543927490247,17.0877958224382,-15.487851091797));
#92981=CARTESIAN_POINT('Ctrl Pts',(19.0338618281357,17.1120781888918,-15.4695259696804));
#92982=CARTESIAN_POINT('Ctrl Pts',(19.1494465050029,17.1318650985331,-15.4620691886714));
#92983=CARTESIAN_POINT('Ctrl Pts',(19.2766584375527,17.1646825527341,-15.4540472965382));
#92984=CARTESIAN_POINT('Ctrl Pts',(19.2904615651038,17.1683928872342,-15.4531791278567));
#92985=CARTESIAN_POINT('Ctrl Pts',(19.3123692432902,17.1745203137437,-15.4518045729043));
#92986=CARTESIAN_POINT('Ctrl Pts',(19.3204985291414,17.17684662017,-15.4512952569314));
#92987=CARTESIAN_POINT('Ctrl Pts',(19.3348106926231,17.1810351720397,-15.4503998144226));
#92988=CARTESIAN_POINT('Ctrl Pts',(19.3409993555557,17.1828771055693,-15.4500130314626));
#92989=CARTESIAN_POINT('Ctrl Pts',(19.3537815603101,17.1867452246307,-15.4492149750924));
#92990=CARTESIAN_POINT('Ctrl Pts',(19.3603738276835,17.1887753814597,-15.4488038369074));
#92991=CARTESIAN_POINT('Ctrl Pts',(19.3772687438688,17.1940688872014,-15.447751247656));
#92992=CARTESIAN_POINT('Ctrl Pts',(19.3875566202858,17.1973789976141,-15.4471113371985));
#92993=CARTESIAN_POINT('Ctrl Pts',(19.4303799581408,17.2115201194859,-15.4444516272409));
#92994=CARTESIAN_POINT('Ctrl Pts',(19.462676268386,17.2230623925964,-15.4424553349185));
#92995=CARTESIAN_POINT('Ctrl Pts',(19.5460739539732,17.2551733482917,-15.4373138962826));
#92996=CARTESIAN_POINT('Ctrl Pts',(19.5966791462783,17.2769608759741,-15.434208085989));
#92997=CARTESIAN_POINT('Ctrl Pts',(19.7450258090312,17.3478127900661,-15.4250667264352));
#92998=CARTESIAN_POINT('Ctrl Pts',(19.8398767814879,17.4024986323835,-15.4191799166778));
#92999=CARTESIAN_POINT('Ctrl Pts',(19.9655432814717,17.4885489782426,-15.4108879396568));
#93000=CARTESIAN_POINT('Ctrl Pts',(20.0002583105075,17.513906579616,-15.4085384339124));
#93001=CARTESIAN_POINT('Ctrl Pts',(20.0938032272092,17.5867054555196,-15.4019765558035));
#93002=CARTESIAN_POINT('Ctrl Pts',(20.1508965821154,17.6362622166131,-15.3977073634541));
#93003=CARTESIAN_POINT('Ctrl Pts',(20.2120392756548,17.6953552427986,-15.3926678160888));
#93004=CARTESIAN_POINT('Ctrl Pts',(20.2188211823139,17.7019986151866,-15.3921019251866));
#93005=CARTESIAN_POINT('Ctrl Pts',(20.2288083534064,17.7119142902945,-15.3912578545929));
#93006=CARTESIAN_POINT('Ctrl Pts',(20.2320481580851,17.7151518480775,-15.3909823451046));
#93007=CARTESIAN_POINT('Ctrl Pts',(20.2377957106074,17.7209328140889,-15.3904904946403));
#93008=CARTESIAN_POINT('Ctrl Pts',(20.2403075532293,17.7234720800524,-15.390274482435));
#93009=CARTESIAN_POINT('Ctrl Pts',(20.2456963664194,17.7289473719113,-15.3898087570877));
#93010=CARTESIAN_POINT('Ctrl Pts',(20.248571173344,17.7318853807491,-15.3895588881872));
#93011=CARTESIAN_POINT('Ctrl Pts',(20.2564882266924,17.7400237703792,-15.3888668918282));
#93012=CARTESIAN_POINT('Ctrl Pts',(20.2615123118425,17.7452416289841,-15.388423391894));
#93013=CARTESIAN_POINT('Ctrl Pts',(20.2889763366229,17.7740594634095,-15.3859754195532));
#93014=CARTESIAN_POINT('Ctrl Pts',(20.3108948923896,17.7981476575058,-15.3839345405864));
#93015=CARTESIAN_POINT('Ctrl Pts',(20.4389281604584,17.9455461493966,-15.3715279086093));
#93016=CARTESIAN_POINT('Ctrl Pts',(20.5310941831851,18.0802454240744,-15.3605727162411));
#93017=CARTESIAN_POINT('Ctrl Pts',(20.6613730595803,18.3275042306929,-15.3423172746963));
#93018=CARTESIAN_POINT('Ctrl Pts',(20.7071813425255,18.4351811557761,-15.3348770814132));
#93019=CARTESIAN_POINT('Ctrl Pts',(20.7483642049038,18.5596705659051,-15.326870626374));
#93020=CARTESIAN_POINT('Ctrl Pts',(20.7527146990851,18.5732820677364,-15.326002658254));
#93021=CARTESIAN_POINT('Ctrl Pts',(20.75941939604,18.595015626581,-15.3246283598287));
#93022=CARTESIAN_POINT('Ctrl Pts',(20.7618632718003,18.6031093582938,-15.3241191015222));
#93023=CARTESIAN_POINT('Ctrl Pts',(20.7660879209759,18.6174097620832,-15.3232237260909));
#93024=CARTESIAN_POINT('Ctrl Pts',(20.7678888955056,18.623610307123,-15.3228369528513));
#93025=CARTESIAN_POINT('Ctrl Pts',(20.771555220673,18.6364520854575,-15.3220388836862));
#93026=CARTESIAN_POINT('Ctrl Pts',(20.7734165372754,18.6430943981465,-15.3216277231476));
#93027=CARTESIAN_POINT('Ctrl Pts',(20.7781109545724,18.6601676899669,-15.3205750086698));
#93028=CARTESIAN_POINT('Ctrl Pts',(20.7808967179971,18.6706115648992,-15.3199349960594));
#93029=CARTESIAN_POINT('Ctrl Pts',(20.7921897540702,18.714290006212,-15.3172742934018));
#93030=CARTESIAN_POINT('Ctrl Pts',(20.7999688282541,18.7477086456871,-15.3152771329364));
#93031=CARTESIAN_POINT('Ctrl Pts',(20.8181177594599,18.8352622375545,-15.3101329530553));
#93032=CARTESIAN_POINT('Ctrl Pts',(20.8271923252784,18.8896400207663,-15.3070253246903));
#93033=CARTESIAN_POINT('Ctrl Pts',(20.847909952043,19.0527894438711,-15.2978807931925));
#93034=CARTESIAN_POINT('Ctrl Pts',(20.8532599351002,19.1621729953013,-15.291992619048));
#93035=CARTESIAN_POINT('Ctrl Pts',(20.8488264518945,19.3172966006862,-15.2835435861459));
#93036=CARTESIAN_POINT('Ctrl Pts',(20.846029397009,19.3630574755655,-15.2810373712711));
#93037=CARTESIAN_POINT('Ctrl Pts',(20.8396445266059,19.4311322580234,-15.2772457677915));
#93038=CARTESIAN_POINT('Ctrl Pts',(20.837181382164,19.4535388773749,-15.2759874359774));
#93039=CARTESIAN_POINT('Ctrl Pts',(20.8335686285498,19.4821838340803,-15.2743608706973));
#93040=CARTESIAN_POINT('Ctrl Pts',(20.8327480887147,19.4884627121551,-15.2740032275575));
#93041=CARTESIAN_POINT('Ctrl Pts',(20.8258132327739,19.5397376289191,-15.2710729163464));
#93042=CARTESIAN_POINT('Ctrl Pts',(20.8182812484857,19.5845265046774,-15.2684522282174));
#93043=CARTESIAN_POINT('Ctrl Pts',(20.8078132896979,19.6364942294351,-15.2653039568065));
#93044=CARTESIAN_POINT('Ctrl Pts',(20.8062705546122,19.6439453133609,-15.264849955684));
#93045=CARTESIAN_POINT('Ctrl Pts',(20.8037300105769,19.6558908609339,-15.2641176824912));
#93046=CARTESIAN_POINT('Ctrl Pts',(20.8027576347759,19.6603907458598,-15.2638408259588));
#93047=CARTESIAN_POINT('Ctrl Pts',(20.8010024651387,19.6683867562725,-15.2633470156382));
#93048=CARTESIAN_POINT('Ctrl Pts',(20.8002254661125,19.6718841055093,-15.2631303959459));
#93049=CARTESIAN_POINT('Ctrl Pts',(20.7985516858265,19.679328645847,-15.2626679244081));
#93050=CARTESIAN_POINT('Ctrl Pts',(20.7976524747891,19.6832751810458,-15.2624219404899));
#93051=CARTESIAN_POINT('Ctrl Pts',(20.7951765541253,19.6939996263973,-15.2617513204872));
#93052=CARTESIAN_POINT('Ctrl Pts',(20.7935777498196,19.7007723100772,-15.2613254457314));
#93053=CARTESIAN_POINT('Ctrl Pts',(20.7852192197669,19.7354150545794,-15.259135373659));
#93054=CARTESIAN_POINT('Ctrl Pts',(20.7779274186208,19.7631521130403,-15.2573430682459));
#93055=CARTESIAN_POINT('Ctrl Pts',(20.7547774541449,19.8444571910483,-15.251991425533));
#93056=CARTESIAN_POINT('Ctrl Pts',(20.7373604286853,19.8975534703494,-15.248370238316));
#93057=CARTESIAN_POINT('Ctrl Pts',(20.6691425351427,20.0807123067221,-15.2355657320242));
#93058=CARTESIAN_POINT('Ctrl Pts',(20.6075942740134,20.2064022750081,-15.2262394981157));
#93059=CARTESIAN_POINT('Ctrl Pts',(20.4870741947634,20.4011306239625,-15.2114604455813));
#93060=CARTESIAN_POINT('Ctrl Pts',(20.4352576128017,20.4740938961757,-15.2058281269232));
#93061=CARTESIAN_POINT('Ctrl Pts',(20.3703515631348,20.5542163906147,-15.1995368715949));
#93062=CARTESIAN_POINT('Ctrl Pts',(20.3616241760003,20.5647785142856,-15.1987051182947));
#93063=CARTESIAN_POINT('Ctrl Pts',(20.3474571411605,20.5815887988599,-15.1973772297129));
#93064=CARTESIAN_POINT('Ctrl Pts',(20.3420823980459,20.5878909201756,-15.1968784662085));
#93065=CARTESIAN_POINT('Ctrl Pts',(20.3324697868567,20.5990290640551,-15.1959952251807));
#93066=CARTESIAN_POINT('Ctrl Pts',(20.3282466369264,20.6038775984337,-15.1956101475697));
#93067=CARTESIAN_POINT('Ctrl Pts',(20.3193976977879,20.6139439623226,-15.1948093789898));
#93068=CARTESIAN_POINT('Ctrl Pts',(20.3147680808237,20.6191583355595,-15.1943938541769));
#93069=CARTESIAN_POINT('Ctrl Pts',(20.3026698665308,20.6326497938427,-15.1933167766899));
#93070=CARTESIAN_POINT('Ctrl Pts',(20.2951614388007,20.6408909943367,-15.1926569076469));
#93071=CARTESIAN_POINT('Ctrl Pts',(20.2621921186869,20.676508628919,-15.1897959849049));
#93072=CARTESIAN_POINT('Ctrl Pts',(20.2360727348287,20.7032682213898,-15.1876232211937));
#93073=CARTESIAN_POINT('Ctrl Pts',(20.1647139335123,20.772602979298,-15.1819140029514));
#93074=CARTESIAN_POINT('Ctrl Pts',(20.1182857599495,20.8139036243126,-15.1784292939751));
#93075=CARTESIAN_POINT('Ctrl Pts',(19.9653800727645,20.9383159583459,-15.1675264745593));
#93076=CARTESIAN_POINT('Ctrl Pts',(19.8527475927383,21.0133095243525,-15.1603353968679));
#93077=CARTESIAN_POINT('Ctrl Pts',(19.6615335535597,21.1157523342815,-15.1483693533313));
#93078=CARTESIAN_POINT('Ctrl Pts',(19.5871469487989,21.150210420812,-15.1437602921818));
#93079=CARTESIAN_POINT('Ctrl Pts',(19.5020345749563,21.1837909118349,-15.1383386088654));
#93080=CARTESIAN_POINT('Ctrl Pts',(19.4930842240697,21.1872520646618,-15.1377666780148));
#93081=CARTESIAN_POINT('Ctrl Pts',(19.4798089805932,21.1922821927852,-15.1369153079885));
#93082=CARTESIAN_POINT('Ctrl Pts',(19.4755018636163,21.1938981689231,-15.1366386065038));
#93083=CARTESIAN_POINT('Ctrl Pts',(19.4678394783845,21.1967445434177,-15.1361454493929));
#93084=CARTESIAN_POINT('Ctrl Pts',(19.4644863269233,21.197980497566,-15.1359293292924));
#93085=CARTESIAN_POINT('Ctrl Pts',(19.4572819031519,21.2006153088292,-15.1354643052791));
#93086=CARTESIAN_POINT('Ctrl Pts',(19.453429751928,21.2020114565059,-15.1352152505222));
#93087=CARTESIAN_POINT('Ctrl Pts',(19.442812772387,21.2058245683849,-15.134527747316));
#93088=CARTESIAN_POINT('Ctrl Pts',(19.4360397305469,21.2082182700584,-15.134087955009));
#93089=CARTESIAN_POINT('Ctrl Pts',(19.3993117870122,21.2209886069406,-15.1316971125447));
#93090=CARTESIAN_POINT('Ctrl Pts',(19.3691405599911,21.2307252765818,-15.1297115903816));
#93091=CARTESIAN_POINT('Ctrl Pts',(19.1821576219572,21.2864634780219,-15.1173231378092));
#93092=CARTESIAN_POINT('Ctrl Pts',(19.020677317936,21.3148559450112,-15.1063166472014));
#93093=CARTESIAN_POINT('Ctrl Pts',(18.7407053511653,21.3312219271883,-15.0879963471976));
#93094=CARTESIAN_POINT('Ctrl Pts',(18.6234911258319,21.3283525024668,-15.0805406775329));
#93095=CARTESIAN_POINT('Ctrl Pts',(18.4928879276334,21.3142732198246,-15.0725198193826));
#93096=CARTESIAN_POINT('Ctrl Pts',(18.4786936111983,21.3125974715049,-15.0716516639673));
#93097=CARTESIAN_POINT('Ctrl Pts',(18.4561305025961,21.3097017500052,-15.0702771259826));
#93098=CARTESIAN_POINT('Ctrl Pts',(18.4477503608139,21.3085751811004,-15.0697678138239));
#93099=CARTESIAN_POINT('Ctrl Pts',(18.4329830758618,21.306499821612,-15.0688723757521));
#93100=CARTESIAN_POINT('Ctrl Pts',(18.4265931448461,21.3055719653025,-15.0684855934351));
#93101=CARTESIAN_POINT('Ctrl Pts',(18.4133859842095,21.3035924666151,-15.0676875362193));
#93102=CARTESIAN_POINT('Ctrl Pts',(18.4065694415479,21.302536710072,-15.0672763965563));
#93103=CARTESIAN_POINT('Ctrl Pts',(18.3890865791447,21.299741373465,-15.0662237990248));
#93104=CARTESIAN_POINT('Ctrl Pts',(18.3784281163115,21.2979533859664,-15.0655838818129));
#93105=CARTESIAN_POINT('Ctrl Pts',(18.3340091343197,21.2901518018149,-15.0629241062285));
#93106=CARTESIAN_POINT('Ctrl Pts',(18.3003824320171,21.2833997946169,-15.0609277565146));
#93107=CARTESIAN_POINT('Ctrl Pts',(18.213215384097,21.2636825440875,-15.0557861366747));
#93108=CARTESIAN_POINT('Ctrl Pts',(18.1599898267852,21.2494394051595,-15.0526802062049));
#93109=CARTESIAN_POINT('Ctrl Pts',(18.0045375861835,21.2012676129357,-15.0436307844694));
#93110=CARTESIAN_POINT('Ctrl Pts',(17.9042759436445,21.1615997755708,-15.0378298283945));
#93111=CARTESIAN_POINT('Ctrl Pts',(17.6993597569857,21.0618551640889,-15.0254260779334));
#93112=CARTESIAN_POINT('Ctrl Pts',(17.5959470071513,21.0001261074266,-15.018828609812));
#93113=CARTESIAN_POINT('Ctrl Pts',(17.4906331647077,20.9244229396325,-15.0111418568529));
#93114=CARTESIAN_POINT('Ctrl Pts',(17.4829565968111,20.9188260019371,-15.0105755732857));
#93115=CARTESIAN_POINT('Ctrl Pts',(17.4716343320212,20.9104537095105,-15.0097310279634));
#93116=CARTESIAN_POINT('Ctrl Pts',(17.4679594328788,20.9077177938474,-15.0094554407745));
#93117=CARTESIAN_POINT('Ctrl Pts',(17.4615604000717,20.9029214316605,-15.0089729368512));
#93118=CARTESIAN_POINT('Ctrl Pts',(17.4588323369226,20.9008662956718,-15.0087663928243));
#93119=CARTESIAN_POINT('Ctrl Pts',(17.4529434263976,20.8964076132299,-15.0083187005526));
#93120=CARTESIAN_POINT('Ctrl Pts',(17.4497844117452,20.894001809205,-15.0080773970113));
#93121=CARTESIAN_POINT('Ctrl Pts',(17.4413944510692,20.8875749094958,-15.0074335099071));
#93122=CARTESIAN_POINT('Ctrl Pts',(17.4361755526817,20.8835382607191,-15.0070298524683));
#93123=CARTESIAN_POINT('Ctrl Pts',(17.4245779490864,20.8744809250067,-15.0061259807316));
#93124=CARTESIAN_POINT('Ctrl Pts',(17.4182091124819,20.8694478378671,-15.0056249515416));
#93125=CARTESIAN_POINT('Ctrl Pts',(17.398985283648,20.8540754273455,-15.0040988253626));
#93126=CARTESIAN_POINT('Ctrl Pts',(17.3862223578311,20.8436225971152,-15.0030667181486));
#93127=CARTESIAN_POINT('Ctrl Pts',(17.3390418057299,20.8040514883759,-14.9991842510155));
#93128=CARTESIAN_POINT('Ctrl Pts',(17.3054366293051,20.7739867513939,-14.9962835432857));
#93129=CARTESIAN_POINT('Ctrl Pts',(17.2178827406146,20.6904733250081,-14.9884085533946));
#93130=CARTESIAN_POINT('Ctrl Pts',(17.1658065505382,20.6351564430838,-14.9833805822346));
#93131=CARTESIAN_POINT('Ctrl Pts',(17.0169228477852,20.4589166570284,-14.9681407804334));
#93132=CARTESIAN_POINT('Ctrl Pts',(16.9302834974346,20.3300500983987,-14.9580559665156));
#93133=CARTESIAN_POINT('Ctrl Pts',(16.8473598005248,20.1716514176227,-14.9470407174499));
#93134=CARTESIAN_POINT('Ctrl Pts',(16.8366142451859,20.150249572677,-14.9455780297531));
#93135=CARTESIAN_POINT('Ctrl Pts',(16.8220268810556,20.1199235275425,-14.9435403653674));
#93136=CARTESIAN_POINT('Ctrl Pts',(16.8178801418033,20.1111488101519,-14.9429548210001));
#93137=CARTESIAN_POINT('Ctrl Pts',(16.8112693178155,20.0969072605944,-14.9420109076378));
#93138=CARTESIAN_POINT('Ctrl Pts',(16.8087678968943,20.0914580063287,-14.9416512510367));
#93139=CARTESIAN_POINT('Ctrl Pts',(16.8036027081718,20.0800785676884,-14.9409033144092));
#93140=CARTESIAN_POINT('Ctrl Pts',(16.800943033911,20.0741465857094,-14.9405151783309));
#93141=CARTESIAN_POINT('Ctrl Pts',(16.7947203277592,20.0600947984488,-14.9395998476362));
#93142=CARTESIAN_POINT('Ctrl Pts',(16.7911808847732,20.0519646324747,-14.9390734650396));
#93143=CARTESIAN_POINT('Ctrl Pts',(16.7796053595027,20.0249122838459,-14.9373324251423));
#93144=CARTESIAN_POINT('Ctrl Pts',(16.7717936629083,20.0058949309126,-14.9361253930586));
#93145=CARTESIAN_POINT('Ctrl Pts',(16.7318169225117,19.9043904128562,-14.9297674203842));
#93146=CARTESIAN_POINT('Ctrl Pts',(16.7045711712959,19.8200554557607,-14.9247836505034));
#93147=CARTESIAN_POINT('Ctrl Pts',(16.6389736836006,19.5628932602865,-14.9101349610871));
#93148=CARTESIAN_POINT('Ctrl Pts',(16.6169140089545,19.3867612829644,-14.9008598344646));
#93149=CARTESIAN_POINT('Ctrl Pts',(16.6170002518853,19.2099672937205,-14.8907771687908));
#93150=CARTESIAN_POINT('Ctrl Pts',(16.6170002532686,19.2099644618986,-14.8907770072903));
#93151=CARTESIAN_POINT('Ctrl Pts',(16.6170133611387,19.1831674202198,-14.8892487548365));
#93152=CARTESIAN_POINT('Ctrl Pts',(16.6175352642807,19.1563740130565,-14.8877018056538));
#93153=CARTESIAN_POINT('Ctrl Pts',(16.6191227654004,19.1151184461241,-14.8852809873123));
#93154=CARTESIAN_POINT('Ctrl Pts',(16.6198286097268,19.1006446791055,-14.8844242999335));
#93155=CARTESIAN_POINT('Ctrl Pts',(16.6209600190457,19.0814889215016,-14.8832793662802));
#93156=CARTESIAN_POINT('Ctrl Pts',(16.6212526903932,19.076799085809,-14.8829981723266));
#93157=CARTESIAN_POINT('Ctrl Pts',(16.6217938179286,19.068568820797,-14.8825030883143));
#93158=CARTESIAN_POINT('Ctrl Pts',(16.6220355693794,19.0650279486961,-14.8822895662434));
#93159=CARTESIAN_POINT('Ctrl Pts',(16.6225281743401,19.0580703880282,-14.8818689511269));
#93160=CARTESIAN_POINT('Ctrl Pts',(16.6227784202666,19.0546536603399,-14.8816618916634));
#93161=CARTESIAN_POINT('Ctrl Pts',(16.6233330673747,19.0473250324884,-14.8812166617965));
#93162=CARTESIAN_POINT('Ctrl Pts',(16.6236400494779,19.0434133832307,-14.8809783504605));
#93163=CARTESIAN_POINT('Ctrl Pts',(16.6244765273423,19.0331216587381,-14.8803496189784));
#93164=CARTESIAN_POINT('Ctrl Pts',(16.6250240881385,19.0267431500854,-14.8799582055379));
#93165=CARTESIAN_POINT('Ctrl Pts',(16.6274167961225,19.0002797749452,-14.8783273302293));
#93166=CARTESIAN_POINT('Ctrl Pts',(16.629519932923,18.9802200469978,-14.8770744361996));
#93167=CARTESIAN_POINT('Ctrl Pts',(16.6324142606819,18.9559616685905,-14.8755415586506));
#93168=CARTESIAN_POINT('Ctrl Pts',(16.6329320450474,18.9517306067433,-14.8752735437659));
#93169=CARTESIAN_POINT('Ctrl Pts',(16.6366907711341,18.9217671159181,-14.8733710044627));
#93170=CARTESIAN_POINT('Ctrl Pts',(16.6403914470368,18.8960956066903,-14.8717174084526));
#93171=CARTESIAN_POINT('Ctrl Pts',(16.665994580413,18.7389851978773,-14.8614773061057));
#93172=CARTESIAN_POINT('Ctrl Pts',(16.6997789097244,18.6098841517055,-14.8525677443131));
#93173=CARTESIAN_POINT('Ctrl Pts',(16.7454194448477,18.4848895568371,-14.8438385225655));
#93174=CARTESIAN_POINT('Origin',(18.734,19.211,0.));
#93175=CARTESIAN_POINT('',(16.7454194461219,18.4848895533475,-14.0426552599844));
#93176=CARTESIAN_POINT('',(16.7454194503191,18.4848895418526,-14.2664527091109));
#93177=CARTESIAN_POINT('',(16.7454194503191,18.4848895418526,0.));
#93178=CARTESIAN_POINT('',(16.6195738484597,19.2114672066323,-14.3109440134334));
#93179=CARTESIAN_POINT('Ctrl Pts',(16.7454194503191,18.4848895418526,-14.2664527091109));
#93180=CARTESIAN_POINT('Ctrl Pts',(16.7196506946332,18.5554617885013,-14.270975824323));
#93181=CARTESIAN_POINT('Ctrl Pts',(16.6976093487813,18.627498828733,-14.2754989395351));
#93182=CARTESIAN_POINT('Ctrl Pts',(16.6794520907032,18.7005865515055,-14.2800220547472));
#93183=CARTESIAN_POINT('Ctrl Pts',(16.6613181210866,18.7735805321165,-14.2845393686211));
#93184=CARTESIAN_POINT('Ctrl Pts',(16.6470584426659,18.8476220952149,-14.289056682495));
#93185=CARTESIAN_POINT('Ctrl Pts',(16.6367803549673,18.922280827639,-14.2935739963689));
#93186=CARTESIAN_POINT('Ctrl Pts',(16.6265157659132,18.9968415076116,-14.2980853774646));
#93187=CARTESIAN_POINT('Ctrl Pts',(16.6202224201554,19.072017312509,-14.3025967585603));
#93188=CARTESIAN_POINT('Ctrl Pts',(16.6179565327787,19.1473678946593,-14.3071081396561));
#93189=CARTESIAN_POINT('Ctrl Pts',(16.61731437944,19.1687222781118,-14.3083866667632));
#93190=CARTESIAN_POINT('Ctrl Pts',(16.6169953775011,19.1900906491545,-14.3096651938704));
#93191=CARTESIAN_POINT('Ctrl Pts',(16.617000050606,19.2114628884564,-14.3109437209775));
#93192=CARTESIAN_POINT('Ctrl Pts',(16.6203928462353,19.2114685807016,-14.3109441064946));
#93193=CARTESIAN_POINT('Ctrl Pts',(16.6197599964399,19.5369558005646,-14.3304466040344));
#93194=CARTESIAN_POINT('Ctrl Pts',(16.8436652507848,20.5691167836237,-14.3923410371346));
#93195=CARTESIAN_POINT('Ctrl Pts',(18.453125516026,21.6984565773647,-14.4966274057954));
#93196=CARTESIAN_POINT('Ctrl Pts',(20.6735253020556,20.7935840586526,-14.6238032124768));
#93197=CARTESIAN_POINT('Ctrl Pts',(21.114531003966,18.4367888923735,-14.7509790191583));
#93198=CARTESIAN_POINT('Ctrl Pts',(19.3715472621554,16.7902843643798,-14.8781548258396));
#93199=CARTESIAN_POINT('Ctrl Pts',(17.4471161436709,17.2650914732991,-14.9832889524729));
#93200=CARTESIAN_POINT('Ctrl Pts',(16.8648290097867,18.166885156152,-15.0460311435457));
#93201=CARTESIAN_POINT('Ctrl Pts',(16.7486736478041,18.4860706551708,-15.066381399058));
#93202=CARTESIAN_POINT('Ctrl Pts',(16.7454194448477,18.484889556837,-14.8438385225655));
#93203=CARTESIAN_POINT('Ctrl Pts',(16.760364385294,18.4439602212943,-14.840980148999));
#93204=CARTESIAN_POINT('Ctrl Pts',(16.7765805848748,18.4034713560533,-14.838138763469));
#93205=CARTESIAN_POINT('Ctrl Pts',(16.8176683039001,18.3094224023408,-14.8315216662765));
#93206=CARTESIAN_POINT('Ctrl Pts',(16.8435369451236,18.2563693039662,-14.8277760980566));
#93207=CARTESIAN_POINT('Ctrl Pts',(16.8887243955929,18.1727583809304,-14.8218600131763));
#93208=CARTESIAN_POINT('Ctrl Pts',(16.9066661974489,18.1414958436656,-14.8196445879183));
#93209=CARTESIAN_POINT('Ctrl Pts',(16.9311171312812,18.1013048027343,-14.8167901761693));
#93210=CARTESIAN_POINT('Ctrl Pts',(16.9369092150479,18.0919491580119,-14.8161252602874));
#93211=CARTESIAN_POINT('Ctrl Pts',(16.9464735387144,18.0767661944531,-14.8150453023116));
#93212=CARTESIAN_POINT('Ctrl Pts',(16.9502019067965,18.0709116087291,-14.8146286499345));
#93213=CARTESIAN_POINT('Ctrl Pts',(16.957445284155,18.05965998839,-14.8138274432605));
#93214=CARTESIAN_POINT('Ctrl Pts',(16.9609562569011,18.054260458358,-14.8134427448301));
#93215=CARTESIAN_POINT('Ctrl Pts',(16.9690774063331,18.0418947793422,-14.8125612071051));
#93216=CARTESIAN_POINT('Ctrl Pts',(16.9737043014657,18.0349396973884,-14.8120650007214));
#93217=CARTESIAN_POINT('Ctrl Pts',(16.9861630821549,18.0164500909454,-14.8107447111344));
#93218=CARTESIAN_POINT('Ctrl Pts',(16.9940680310008,18.0049651191932,-14.8099233900928));
#93219=CARTESIAN_POINT('Ctrl Pts',(17.0584934135661,17.9133145097415,-14.8033573529328));
#93220=CARTESIAN_POINT('Ctrl Pts',(17.1204130387034,17.8370820292176,-14.7978303323002));
#93221=CARTESIAN_POINT('Ctrl Pts',(17.2808171221161,17.6654700582512,-14.7848750373219));
#93222=CARTESIAN_POINT('Ctrl Pts',(17.3836930602115,17.5748239666527,-14.7775970535287));
#93223=CARTESIAN_POINT('Ctrl Pts',(17.5362188245962,17.464676453206,-14.7671723063572));
#93224=CARTESIAN_POINT('Ctrl Pts',(17.57892459575,17.4361406322258,-14.764285394078));
#93225=CARTESIAN_POINT('Ctrl Pts',(17.6379507252786,17.3997326701052,-14.7602785698418));
#93226=CARTESIAN_POINT('Ctrl Pts',(17.6533986661325,17.3904742335635,-14.7592284235887));
#93227=CARTESIAN_POINT('Ctrl Pts',(17.6764327302698,17.3770656532769,-14.7576575044492));
#93228=CARTESIAN_POINT('Ctrl Pts',(17.6839295734656,17.3727628520983,-14.7571454373302));
#93229=CARTESIAN_POINT('Ctrl Pts',(17.6975506155132,17.3650555891748,-14.7562132581507));
#93230=CARTESIAN_POINT('Ctrl Pts',(17.7036658083792,17.361635367238,-14.7557941025942));
#93231=CARTESIAN_POINT('Ctrl Pts',(17.7133275446521,17.3562943614642,-14.7551306506557));
#93232=CARTESIAN_POINT('Ctrl Pts',(17.7168628546947,17.354353212445,-14.7548876354203));
#93233=CARTESIAN_POINT('Ctrl Pts',(17.7204127490508,17.352417237565,-14.7546433429248));
#93234=CARTESIAN_POINT('Ctrl Pts',(17.7204218420691,17.3524122786716,-14.7546427171702));
#93235=CARTESIAN_POINT('Ctrl Pts',(17.7204400832236,17.3524023309998,-14.7546414618645));
#93236=CARTESIAN_POINT('Ctrl Pts',(17.7204492316218,17.3523973420797,-14.7546408322952));
#93237=CARTESIAN_POINT('Ctrl Pts',(17.7204675838462,17.3523873341884,-14.7546395693386));
#93238=CARTESIAN_POINT('Ctrl Pts',(17.7204767880041,17.3523823150375,-14.7546389359284));
#93239=CARTESIAN_POINT('Ctrl Pts',(17.7204952526121,17.3523722462167,-14.7546376652303));
#93240=CARTESIAN_POINT('Ctrl Pts',(17.7205045126594,17.3523671967676,-14.7546370279702));
#93241=CARTESIAN_POINT('Ctrl Pts',(17.7205230894845,17.3523570671147,-14.7546357495421));
#93242=CARTESIAN_POINT('Ctrl Pts',(17.7205324061711,17.3523519869617,-14.7546351083804));
#93243=CARTESIAN_POINT('Ctrl Pts',(17.7205510966092,17.352341795722,-14.7546338221261));
#93244=CARTESIAN_POINT('Ctrl Pts',(17.7205604702178,17.3523366847143,-14.7546331770432));
#93245=CARTESIAN_POINT('Ctrl Pts',(17.7205792745839,17.3523264317228,-14.7546318829408));
#93246=CARTESIAN_POINT('Ctrl Pts',(17.7205887057091,17.3523212895395,-14.7546312338958));
#93247=CARTESIAN_POINT('Ctrl Pts',(17.7206076260477,17.3523109736881,-14.7546299318044));
#93248=CARTESIAN_POINT('Ctrl Pts',(17.7206171145797,17.3523058003926,-14.7546292788048));
#93249=CARTESIAN_POINT('Ctrl Pts',(17.7206361498426,17.3522954222598,-14.7546279687965));
#93250=CARTESIAN_POINT('Ctrl Pts',(17.720645696871,17.3522902172614,-14.7546273117672));
#93251=CARTESIAN_POINT('Ctrl Pts',(17.7206648494162,17.3522797755684,-14.7546259936795));
#93252=CARTESIAN_POINT('Ctrl Pts',(17.7206744549312,17.352274538876,-14.7546253326212));
#93253=CARTESIAN_POINT('Ctrl Pts',(17.7206937248093,17.3522640336023,-14.7546240064504));
#93254=CARTESIAN_POINT('Ctrl Pts',(17.7207033894106,17.3522587648924,-14.7546233413217));
#93255=CARTESIAN_POINT('Ctrl Pts',(17.7207227775041,17.3522481955641,-14.7546220070071));
#93256=CARTESIAN_POINT('Ctrl Pts',(17.7207325016844,17.3522428945718,-14.7546213377739));
#93257=CARTESIAN_POINT('Ctrl Pts',(17.7207519723628,17.3522322806191,-14.7546199977674));
#93258=CARTESIAN_POINT('Ctrl Pts',(17.720761774882,17.3522269371207,-14.7546193231384));
#93259=CARTESIAN_POINT('Ctrl Pts',(17.7207814225257,17.3522162271022,-14.7546179709444));
#93260=CARTESIAN_POINT('Ctrl Pts',(17.7207912660535,17.3522108614526,-14.7546172934891));
#93261=CARTESIAN_POINT('Ctrl Pts',(17.7208110155964,17.3522000962955,-14.7546159342737));
#93262=CARTESIAN_POINT('Ctrl Pts',(17.7208209197984,17.3521946977775,-14.7546152526384));
#93263=CARTESIAN_POINT('Ctrl Pts',(17.7208408246989,17.3521838483502,-14.7546138827223));
#93264=CARTESIAN_POINT('Ctrl Pts',(17.7208507733133,17.352178425832,-14.7546131980262));
#93265=CARTESIAN_POINT('Ctrl Pts',(17.7238601058545,17.3505382124049,-14.7544060852418));
#93266=CARTESIAN_POINT('Ctrl Pts',(17.7268633780036,17.348910718339,-14.7541991891587));
#93267=CARTESIAN_POINT('Ctrl Pts',(17.7339045057823,17.3451170993749,-14.7537136658549));
#93268=CARTESIAN_POINT('Ctrl Pts',(17.7379454510664,17.3429568176735,-14.7534346722837));
#93269=CARTESIAN_POINT('Ctrl Pts',(17.7503890311355,17.3363563586983,-14.7525745515342));
#93270=CARTESIAN_POINT('Ctrl Pts',(17.7588144426734,17.331959702139,-14.7519907829509));
#93271=CARTESIAN_POINT('Ctrl Pts',(17.8740984783587,17.2727848922271,-14.7439871942518));
#93272=CARTESIAN_POINT('Ctrl Pts',(17.9853878363025,17.2271447679186,-14.7360866505523));
#93273=CARTESIAN_POINT('Ctrl Pts',(18.2037525158422,17.1585945596431,-14.720966304644));
#93274=CARTESIAN_POINT('Ctrl Pts',(18.3099420885646,17.1340529968721,-14.7137743028233));
#93275=CARTESIAN_POINT('Ctrl Pts',(18.4915160222587,17.1066031891036,-14.701977063376));
#93276=CARTESIAN_POINT('Ctrl Pts',(18.5660248641103,17.0993487744956,-14.6972713587155));
#93277=CARTESIAN_POINT('Ctrl Pts',(18.6595270652887,17.0952270135606,-14.691538005017));
#93278=CARTESIAN_POINT('Ctrl Pts',(18.6782957390707,17.0946496936655,-14.690395604011));
#93279=CARTESIAN_POINT('Ctrl Pts',(18.7056173573618,17.0941730104952,-14.6887444653229));
#93280=CARTESIAN_POINT('Ctrl Pts',(18.7141655386271,17.0940756566685,-14.6882295559854));
#93281=CARTESIAN_POINT('Ctrl Pts',(18.72916239922,17.0939957065688,-14.6873290948004));
#93282=CARTESIAN_POINT('Ctrl Pts',(18.7356108021183,17.0939907918172,-14.6869428489901));
#93283=CARTESIAN_POINT('Ctrl Pts',(18.7481384103832,17.0940384833689,-14.686194257091));
#93284=CARTESIAN_POINT('Ctrl Pts',(18.7542175582907,17.0940878126224,-14.6858318122002));
#93285=CARTESIAN_POINT('Ctrl Pts',(18.7687596470708,17.0942684620982,-14.6849667114913));
#93286=CARTESIAN_POINT('Ctrl Pts',(18.7772222205011,17.0944243506482,-14.6844648281934));
#93287=CARTESIAN_POINT('Ctrl Pts',(18.8078153918785,17.0951714647278,-14.6826558841119));
#93288=CARTESIAN_POINT('Ctrl Pts',(18.8299378014056,17.0960590798965,-14.6813580861697));
#93289=CARTESIAN_POINT('Ctrl Pts',(19.0370407923683,17.1076250322666,-14.6692945679292));
#93290=CARTESIAN_POINT('Ctrl Pts',(19.2198767734016,17.1421960510957,-14.6593821587678));
#93291=CARTESIAN_POINT('Ctrl Pts',(19.4722003392099,17.2252498830168,-14.6449018754311));
#93292=CARTESIAN_POINT('Ctrl Pts',(19.5470137817247,17.2546897379911,-14.640484381163));
#93293=CARTESIAN_POINT('Ctrl Pts',(19.6527382783776,17.3034070240085,-14.6338260494439));
#93294=CARTESIAN_POINT('Ctrl Pts',(19.6851158769681,17.3193422019941,-14.6317273177624));
#93295=CARTESIAN_POINT('Ctrl Pts',(19.7236835019477,17.3395643589369,-14.6291357712455));
#93296=CARTESIAN_POINT('Ctrl Pts',(19.7302802445997,17.3430678644241,-14.6286892079536));
#93297=CARTESIAN_POINT('Ctrl Pts',(19.7405218332053,17.3485768190172,-14.6279905470797));
#93298=CARTESIAN_POINT('Ctrl Pts',(19.7441796170762,17.3505582658033,-14.6277399490601));
#93299=CARTESIAN_POINT('Ctrl Pts',(19.7509618393948,17.354258140612,-14.627273255934));
#93300=CARTESIAN_POINT('Ctrl Pts',(19.7540877849913,17.355973686037,-14.6270573446658));
#93301=CARTESIAN_POINT('Ctrl Pts',(19.7611572579809,17.3598767453571,-14.6265672174679));
#93302=CARTESIAN_POINT('Ctrl Pts',(19.7650981188443,17.3620689561403,-14.6262927043333));
#93303=CARTESIAN_POINT('Ctrl Pts',(19.7752541316709,17.3677610813809,-14.6255819716341));
#93304=CARTESIAN_POINT('Ctrl Pts',(19.7814585950792,17.3712798130904,-14.6251445865443));
#93305=CARTESIAN_POINT('Ctrl Pts',(19.8194282038753,17.3930678205638,-14.6224488534005));
#93306=CARTESIAN_POINT('Ctrl Pts',(19.8507303166432,17.4121267910756,-14.6201443732444));
#93307=CARTESIAN_POINT('Ctrl Pts',(20.0248080780698,17.5244124701656,-14.6069248120852));
#93308=CARTESIAN_POINT('Ctrl Pts',(20.1564044248614,17.6338089110355,-14.5954194463102));
#93309=CARTESIAN_POINT('Ctrl Pts',(20.3389498886409,17.8271907158452,-14.5781372887802));
#93310=CARTESIAN_POINT('Ctrl Pts',(20.3996851144032,17.9009276224433,-14.5720752770046));
#93311=CARTESIAN_POINT('Ctrl Pts',(20.4677003530977,17.9959157150026,-14.5648990210767));
#93312=CARTESIAN_POINT('Ctrl Pts',(20.4798919036987,18.0134991660483,-14.5635949282936));
#93313=CARTESIAN_POINT('Ctrl Pts',(20.4968363305516,18.0387465045181,-14.5617560378387));
#93314=CARTESIAN_POINT('Ctrl Pts',(20.5018097355606,18.046260145456,-14.5612129289374));
#93315=CARTESIAN_POINT('Ctrl Pts',(20.5103025631564,18.0592705184964,-14.5602795451815));
#93316=CARTESIAN_POINT('Ctrl Pts',(20.51384478594,18.0647521498893,-14.5598884192364));
#93317=CARTESIAN_POINT('Ctrl Pts',(20.520575666109,18.0752746962347,-14.559141650114));
#93318=CARTESIAN_POINT('Ctrl Pts',(20.5237684741472,18.0803128697931,-14.55878585492));
#93319=CARTESIAN_POINT('Ctrl Pts',(20.5320092863036,18.0934390386526,-14.5578633963749));
#93320=CARTESIAN_POINT('Ctrl Pts',(20.5370240587277,18.1015478180062,-14.5572979643667));
#93321=CARTESIAN_POINT('Ctrl Pts',(20.5539058222054,18.1292620543609,-14.5553801709333));
#93322=CARTESIAN_POINT('Ctrl Pts',(20.565509436491,18.1490266344562,-14.5540374285452));
#93323=CARTESIAN_POINT('Ctrl Pts',(20.663650729255,18.3225868076299,-14.5424505459645));
#93324=CARTESIAN_POINT('Ctrl Pts',(20.7309644217023,18.486452080381,-14.5329671870379));
#93325=CARTESIAN_POINT('Ctrl Pts',(20.7997638421875,18.7400872461869,-14.5186656755487));
#93326=CARTESIAN_POINT('Ctrl Pts',(20.8172426869461,18.8246884344534,-14.513938285898));
#93327=CARTESIAN_POINT('Ctrl Pts',(20.8348593197461,18.9473781500297,-14.5068602610292));
#93328=CARTESIAN_POINT('Ctrl Pts',(20.839214783305,18.9847773591439,-14.5046731125794));
#93329=CARTESIAN_POINT('Ctrl Pts',(20.8432447319754,19.0298016571566,-14.501983519773));
#93330=CARTESIAN_POINT('Ctrl Pts',(20.8438784832334,19.0373366449291,-14.5015315107062));
#93331=CARTESIAN_POINT('Ctrl Pts',(20.844799862241,19.0490419353556,-14.5008261683893));
#93332=CARTESIAN_POINT('Ctrl Pts',(20.8451155358369,19.0532100548362,-14.5005743814444));
#93333=CARTESIAN_POINT('Ctrl Pts',(20.8456774806304,19.0609336157271,-14.5001066198758));
#93334=CARTESIAN_POINT('Ctrl Pts',(20.8459271190536,19.0644887543152,-14.4998908363447));
#93335=CARTESIAN_POINT('Ctrl Pts',(20.8464705010979,19.0725172255188,-14.4994024729696));
#93336=CARTESIAN_POINT('Ctrl Pts',(20.8467590119133,19.0769908452358,-14.4991296050961));
#93337=CARTESIAN_POINT('Ctrl Pts',(20.847566800596,19.0901678888321,-14.4983237548342));
#93338=CARTESIAN_POINT('Ctrl Pts',(20.8480465146547,19.098873519893,-14.497788636437));
#93339=CARTESIAN_POINT('Ctrl Pts',(20.8510777739034,19.1608501102201,-14.4939608922289));
#93340=CARTESIAN_POINT('Ctrl Pts',(20.8516690202901,19.2141933166927,-14.4905712491947));
#93341=CARTESIAN_POINT('Ctrl Pts',(20.849771296706,19.2852779855699,-14.4859755175017));
#93342=CARTESIAN_POINT('Ctrl Pts',(20.8490725191469,19.3030522291724,-14.4848197735307));
#93343=CARTESIAN_POINT('Ctrl Pts',(20.8456417841853,19.3691003570406,-14.4805049749309));
#93344=CARTESIAN_POINT('Ctrl Pts',(20.8414803257243,19.4172842432429,-14.4773175553088));
#93345=CARTESIAN_POINT('Ctrl Pts',(20.8225348262352,19.5738711838925,-14.466898421102));
#93346=CARTESIAN_POINT('Ctrl Pts',(20.8009994148964,19.681287253838,-14.4596657481459));
#93347=CARTESIAN_POINT('Ctrl Pts',(20.7562766792513,19.8395872832691,-14.4490923647354));
#93348=CARTESIAN_POINT('Ctrl Pts',(20.7392311683564,19.8920093410287,-14.4456032762369));
#93349=CARTESIAN_POINT('Ctrl Pts',(20.7082857979193,19.97589297996,-14.4400457747291));
#93350=CARTESIAN_POINT('Ctrl Pts',(20.6956323716152,20.0077837458202,-14.4379389241457));
#93351=CARTESIAN_POINT('Ctrl Pts',(20.6779797130102,20.0493010776704,-14.4352024119854));
#93352=CARTESIAN_POINT('Ctrl Pts',(20.673674356959,20.0592153129718,-14.4345494094366));
#93353=CARTESIAN_POINT('Ctrl Pts',(20.6664971896164,20.0754022180398,-14.4334839121122));
#93354=CARTESIAN_POINT('Ctrl Pts',(20.6636703519265,20.0816945027249,-14.4330698879061));
#93355=CARTESIAN_POINT('Ctrl Pts',(20.6581380617941,20.0938495957112,-14.4322703730626));
#93356=CARTESIAN_POINT('Ctrl Pts',(20.6554364460723,20.0997140567263,-14.4318847560845));
#93357=CARTESIAN_POINT('Ctrl Pts',(20.6491353965626,20.1132288478629,-14.4309963348185));
#93358=CARTESIAN_POINT('Ctrl Pts',(20.6455168633236,20.1208701915526,-14.4304941966003));
#93359=CARTESIAN_POINT('Ctrl Pts',(20.6356595230338,20.1413678076158,-14.4291475832915));
#93360=CARTESIAN_POINT('Ctrl Pts',(20.6293360948846,20.1541830688318,-14.4283060496316));
#93361=CARTESIAN_POINT('Ctrl Pts',(20.5701244976835,20.2711826181164,-14.4206240565047));
#93362=CARTESIAN_POINT('Ctrl Pts',(20.5088231053038,20.370891616978,-14.4141002963679));
#93363=CARTESIAN_POINT('Ctrl Pts',(20.3431651249008,20.5961995976273,-14.3987908013014));
#93364=CARTESIAN_POINT('Ctrl Pts',(20.2319380122963,20.7157791069975,-14.3901882912071));
#93365=CARTESIAN_POINT('Ctrl Pts',(20.0834417584139,20.8424867616726,-14.378979084769));
#93366=CARTESIAN_POINT('Ctrl Pts',(20.0582758625374,20.8629792047038,-14.3770862664228));
#93367=CARTESIAN_POINT('Ctrl Pts',(20.0269361876511,20.8873225735431,-14.3747234574541));
#93368=CARTESIAN_POINT('Ctrl Pts',(20.0211991957322,20.8917318593329,-14.3742906996231));
#93369=CARTESIAN_POINT('Ctrl Pts',(20.0121692051913,20.8985986980074,-14.3736089913711));
#93370=CARTESIAN_POINT('Ctrl Pts',(20.0088914014812,20.9010762693989,-14.3733614248366));
#93371=CARTESIAN_POINT('Ctrl Pts',(20.0027505658338,20.9056898717341,-14.3728973653981));
#93372=CARTESIAN_POINT('Ctrl Pts',(19.999889333394,20.9078282042104,-14.3726810375456));
#93373=CARTESIAN_POINT('Ctrl Pts',(19.9933448682973,20.9126934226707,-14.372186000265));
#93374=CARTESIAN_POINT('Ctrl Pts',(19.9896581970831,20.9154155870131,-14.3719069685211));
#93375=CARTESIAN_POINT('Ctrl Pts',(19.978296550821,20.9237479305096,-14.3710466156867));
#93376=CARTESIAN_POINT('Ctrl Pts',(19.9705927238708,20.9293183079316,-14.3704626511641));
#93377=CARTESIAN_POINT('Ctrl Pts',(19.8655500875889,21.0041988632052,-14.3624950877892));
#93378=CARTESIAN_POINT('Ctrl Pts',(19.7625612688421,21.0651906197424,-14.3546353179602));
#93379=CARTESIAN_POINT('Ctrl Pts',(19.5568295753698,21.164593123943,-14.3395409607983));
#93380=CARTESIAN_POINT('Ctrl Pts',(19.4551412751722,21.2043723536813,-14.3323343131133));
#93381=CARTESIAN_POINT('Ctrl Pts',(19.2789768596638,21.2580300245103,-14.3205014679587));
#93382=CARTESIAN_POINT('Ctrl Pts',(19.205998412301,21.2760790180474,-14.3157751883983));
#93383=CARTESIAN_POINT('Ctrl Pts',(19.1137242387055,21.2937512229167,-14.3100196277815));
#93384=CARTESIAN_POINT('Ctrl Pts',(19.0951943511194,21.2970445418641,-14.30887459241));
#93385=CARTESIAN_POINT('Ctrl Pts',(19.0681789154828,21.3014752246207,-14.3072203719711));
#93386=CARTESIAN_POINT('Ctrl Pts',(19.0597268875907,21.3028088369554,-14.3067049828028));
#93387=CARTESIAN_POINT('Ctrl Pts',(19.0448902189832,21.3050577518684,-14.3058039682094));
#93388=CARTESIAN_POINT('Ctrl Pts',(19.0385090919058,21.3059951815683,-14.3054176461905));
#93389=CARTESIAN_POINT('Ctrl Pts',(19.026107334211,21.3077592218988,-14.3046691139596));
#93390=CARTESIAN_POINT('Ctrl Pts',(19.0200872387001,21.3085890975963,-14.3043068039707));
#93391=CARTESIAN_POINT('Ctrl Pts',(19.0056828708493,21.3105115873742,-14.3034423553043));
#93392=CARTESIAN_POINT('Ctrl Pts',(18.9972954208162,21.311579922869,-14.3029409864763));
#93393=CARTESIAN_POINT('Ctrl Pts',(18.9669802968281,21.3152568281218,-14.3011358535905));
#93394=CARTESIAN_POINT('Ctrl Pts',(18.9450180565557,21.3175725839205,-14.2998413006809));
#93395=CARTESIAN_POINT('Ctrl Pts',(18.7379199827263,21.336138137842,-14.2877478434002));
#93396=CARTESIAN_POINT('Ctrl Pts',(18.5514434170283,21.3282875468118,-14.2778083650023));
#93397=CARTESIAN_POINT('Ctrl Pts',(18.2608025090816,21.2773254224045,-14.2617216768859));
#93398=CARTESIAN_POINT('Ctrl Pts',(18.1548646586907,21.2501695597091,-14.2557003810084));
#93399=CARTESIAN_POINT('Ctrl Pts',(18.040343472846,21.2111671856347,-14.248559775022));
#93400=CARTESIAN_POINT('Ctrl Pts',(18.0292094441632,21.207271125442,-14.2478586791554));
#93401=CARTESIAN_POINT('Ctrl Pts',(18.0134002024229,21.2015903560976,-14.2468526045614));
#93402=CARTESIAN_POINT('Ctrl Pts',(18.0086976288879,21.199881721809,-14.2465519988798));
#93403=CARTESIAN_POINT('Ctrl Pts',(18.0005936629115,21.1969046611281,-14.2460315741936));
#93404=CARTESIAN_POINT('Ctrl Pts',(17.9971893597688,21.1956441138572,-14.2458122242128));
#93405=CARTESIAN_POINT('Ctrl Pts',(17.9905867710304,21.193179973797,-14.2453853522918));
#93406=CARTESIAN_POINT('Ctrl Pts',(17.987388151527,21.1919773913057,-14.2451778966455));
#93407=CARTESIAN_POINT('Ctrl Pts',(17.9787483398747,21.1887051903587,-14.2446157842747));
#93408=CARTESIAN_POINT('Ctrl Pts',(17.9733127973195,21.1866208816299,-14.2442602608719));
#93409=CARTESIAN_POINT('Ctrl Pts',(17.9530677564887,21.1787617999759,-14.24292924112));
#93410=CARTESIAN_POINT('Ctrl Pts',(17.9383152763305,21.1728428725006,-14.2419456234424));
#93411=CARTESIAN_POINT('Ctrl Pts',(17.8094129752262,21.1194321996078,-14.2332390236098));
#93412=CARTESIAN_POINT('Ctrl Pts',(17.6995707159296,21.0621955459608,-14.2250578474201));
#93413=CARTESIAN_POINT('Ctrl Pts',(17.4544611345086,20.9058165199231,-14.2058447694268));
#93414=CARTESIAN_POINT('Ctrl Pts',(17.3246749611485,20.7995359555036,-14.1949287920433));
#93415=CARTESIAN_POINT('Ctrl Pts',(17.1939622374886,20.6637305902117,-14.1833517514888));
#93416=CARTESIAN_POINT('Ctrl Pts',(17.1794267472057,20.6481654502522,-14.1820538228942));
#93417=CARTESIAN_POINT('Ctrl Pts',(17.1590898228379,20.6257182815798,-14.1802220395227));
#93418=CARTESIAN_POINT('Ctrl Pts',(17.1530939482356,20.6190148940125,-14.1796799605968));
#93419=CARTESIAN_POINT('Ctrl Pts',(17.1428229801553,20.6073836313759,-14.1787477914602));
#93420=CARTESIAN_POINT('Ctrl Pts',(17.1385276479695,20.6024738696221,-14.178356855997));
#93421=CARTESIAN_POINT('Ctrl Pts',(17.1303461927102,20.5930344006403,-14.1776100726829));
#93422=CARTESIAN_POINT('Ctrl Pts',(17.1264564025671,20.5885079679131,-14.1772540746334));
#93423=CARTESIAN_POINT('Ctrl Pts',(17.1163900583104,20.5766933557242,-14.1763302732042));
#93424=CARTESIAN_POINT('Ctrl Pts',(17.1102435596605,20.5693796569169,-14.1757637084269));
#93425=CARTESIAN_POINT('Ctrl Pts',(17.089446485294,20.5442904153736,-14.1738378781157));
#93426=CARTESIAN_POINT('Ctrl Pts',(17.0750362878584,20.5263170939052,-14.1724883432209));
#93427=CARTESIAN_POINT('Ctrl Pts',(16.953766337136,20.3698971700147,-14.1609878265011));
#93428=CARTESIAN_POINT('Ctrl Pts',(16.864150154017,20.2189398915557,-14.1515817994359));
#93429=CARTESIAN_POINT('Ctrl Pts',(16.7591127275801,19.9785619014972,-14.1373097817773));
#93430=CARTESIAN_POINT('Ctrl Pts',(16.7291075080056,19.8963719336705,-14.1325252751382));
#93431=CARTESIAN_POINT('Ctrl Pts',(16.6934927506757,19.7762058875582,-14.125370235814));
#93432=CARTESIAN_POINT('Ctrl Pts',(16.6836950214513,19.7395608976502,-14.1231672807582));
#93433=CARTESIAN_POINT('Ctrl Pts',(16.6731275270582,19.6953047300112,-14.1204601680526));
#93434=CARTESIAN_POINT('Ctrl Pts',(16.6714072198997,19.6879249844417,-14.1200072134695));
#93435=CARTESIAN_POINT('Ctrl Pts',(16.6687987127009,19.6764569208378,-14.1193007114558));
#93436=CARTESIAN_POINT('Ctrl Pts',(16.6678829298,19.6723748516669,-14.1190487185104));
#93437=CARTESIAN_POINT('Ctrl Pts',(16.6662094767309,19.6648105900958,-14.1185807699362));
#93438=CARTESIAN_POINT('Ctrl Pts',(16.6654484969531,19.6613291890014,-14.1183650066512));
#93439=CARTESIAN_POINT('Ctrl Pts',(16.6637510234887,19.6534683397513,-14.1178769403347));
#93440=CARTESIAN_POINT('Ctrl Pts',(16.6628196396638,19.6490878570938,-14.117604350828));
#93441=CARTESIAN_POINT('Ctrl Pts',(16.6601202351964,19.6361909880336,-14.1168000668043));
#93442=CARTESIAN_POINT('Ctrl Pts',(16.6583908184045,19.6276667427219,-14.1162662484183));
#93443=CARTESIAN_POINT('Ctrl Pts',(16.6465063451288,19.5671778946155,-14.11246366245));
#93444=CARTESIAN_POINT('Ctrl Pts',(16.6382522854133,19.5148633783206,-14.1090992546497));
#93445=CARTESIAN_POINT('Ctrl Pts',(16.6301911557542,19.4474349068513,-14.1047115460807));
#93446=CARTESIAN_POINT('Ctrl Pts',(16.6285718207931,19.4325519920709,-14.1037398732529));
#93447=CARTESIAN_POINT('Ctrl Pts',(16.6204362485765,19.3496075534794,-14.0983107806219));
#93448=CARTESIAN_POINT('Ctrl Pts',(16.6170625895926,19.281280122789,-14.0937881882882));
#93449=CARTESIAN_POINT('Ctrl Pts',(16.6168557116705,19.0521414080326,-14.0786472548159));
#93450=CARTESIAN_POINT('Ctrl Pts',(16.6350247738266,18.8918491647295,-14.0681492543664));
#93451=CARTESIAN_POINT('Ctrl Pts',(16.6765204048253,18.7119688441873,-14.0567777517569));
#93452=CARTESIAN_POINT('Ctrl Pts',(16.6822553156487,18.6888906229362,-14.0553254722581));
#93453=CARTESIAN_POINT('Ctrl Pts',(16.6908695980434,18.6565626266136,-14.053299773467));
#93454=CARTESIAN_POINT('Ctrl Pts',(16.6934253016897,18.6472291725468,-14.0527159507125));
#93455=CARTESIAN_POINT('Ctrl Pts',(16.6976666649288,18.632146446195,-14.0517740690389));
#93456=CARTESIAN_POINT('Ctrl Pts',(16.6993128687432,18.6263863093291,-14.051414733227));
#93457=CARTESIAN_POINT('Ctrl Pts',(16.7027975173184,18.6143864002933,-14.0506668861545));
#93458=CARTESIAN_POINT('Ctrl Pts',(16.7046403176352,18.6081479501106,-14.0502785213764));
#93459=CARTESIAN_POINT('Ctrl Pts',(16.7090695304346,18.5934041602845,-14.0493616221231));
#93460=CARTESIAN_POINT('Ctrl Pts',(16.7116808336732,18.5849063800131,-14.0488339074799));
#93461=CARTESIAN_POINT('Ctrl Pts',(16.7205471773943,18.5566875633133,-14.0470838258043));
#93462=CARTESIAN_POINT('Ctrl Pts',(16.7270378948414,18.5370414056753,-14.0458691950132));
#93463=CARTESIAN_POINT('Ctrl Pts',(16.7375951451554,18.5065926190859,-14.0439912513117));
#93464=CARTESIAN_POINT('Ctrl Pts',(16.7414631935575,18.4957244434831,-14.0433218631904));
#93465=CARTESIAN_POINT('Ctrl Pts',(16.7454194461219,18.4848895533475,-14.0426552599844));
#93466=CARTESIAN_POINT('Origin',(18.734,19.211,0.));
#93467=CARTESIAN_POINT('',(16.7454194503191,18.4848895418526,-13.2445592875761));
#93468=CARTESIAN_POINT('',(16.7454194857027,18.4848894449486,-13.4647888259555));
#93469=CARTESIAN_POINT('',(16.7454194503191,18.4848895418526,0.));
#93470=CARTESIAN_POINT('',(16.6170008950802,19.2090532671895,-13.5109437209775));
#93471=CARTESIAN_POINT('Ctrl Pts',(16.7454194857027,18.4848894449486,-13.4647888259555));
#93472=CARTESIAN_POINT('Ctrl Pts',(16.729766689791,18.5277573591082,-13.4673502383313));
#93473=CARTESIAN_POINT('Ctrl Pts',(16.7154972638857,18.5711390561076,-13.4699562830825));
#93474=CARTESIAN_POINT('Ctrl Pts',(16.6982006737283,18.6300882848655,-13.4735579023356));
#93475=CARTESIAN_POINT('Ctrl Pts',(16.6939331614507,18.6452574976678,-13.4744899974107));
#93476=CARTESIAN_POINT('Ctrl Pts',(16.688327079247,18.666073447028,-13.4757780725209));
#93477=CARTESIAN_POINT('Ctrl Pts',(16.6868416780844,18.6716805677099,-13.4761259264936));
#93478=CARTESIAN_POINT('Ctrl Pts',(16.6845188929975,18.68059652954,-13.4766805685755));
#93479=CARTESIAN_POINT('Ctrl Pts',(16.6836664223905,18.6839014612219,-13.4768864907921));
#93480=CARTESIAN_POINT('Ctrl Pts',(16.6819231277774,18.6907282368419,-13.4773125581594));
#93481=CARTESIAN_POINT('Ctrl Pts',(16.6810333782027,18.6942503061859,-13.4775327661828));
#93482=CARTESIAN_POINT('Ctrl Pts',(16.6789361643699,18.702643026039,-13.478058406022));
#93483=CARTESIAN_POINT('Ctrl Pts',(16.6777369481559,18.7075156984371,-13.4783643090191));
#93484=CARTESIAN_POINT('Ctrl Pts',(16.6752325955531,18.7178496140955,-13.4790145326324));
#93485=CARTESIAN_POINT('Ctrl Pts',(16.6739318425285,18.7233118684068,-13.4793590913189));
#93486=CARTESIAN_POINT('Ctrl Pts',(16.6704195232459,18.7383259631485,-13.480308434029));
#93487=CARTESIAN_POINT('Ctrl Pts',(16.6682525895442,18.7478879646503,-13.4809155409754));
#93488=CARTESIAN_POINT('Ctrl Pts',(16.633616461448,18.9058077670562,-13.4909794231096));
#93489=CARTESIAN_POINT('Ctrl Pts',(16.6171414693839,19.0572035914288,-13.5011355845678));
#93490=CARTESIAN_POINT('Ctrl Pts',(16.6170009071414,19.2090401949666,-13.5111420663959));
#93491=CARTESIAN_POINT('Ctrl Pts',(16.6170008950802,19.2090532671895,-13.5109437209775));
#93492=CARTESIAN_POINT('Ctrl Pts',(16.6169347298129,19.2810055201563,-13.5152699622426));
#93493=CARTESIAN_POINT('Ctrl Pts',(16.62054107027,19.3530526998715,-13.5195962035077));
#93494=CARTESIAN_POINT('Ctrl Pts',(16.6278222442379,19.4247855494018,-13.5239224447728));
#93495=CARTESIAN_POINT('Ctrl Pts',(16.6350987839402,19.4964727429596,-13.5282459325052));
#93496=CARTESIAN_POINT('Ctrl Pts',(16.6460454699347,19.5678455121798,-13.5325694202375));
#93497=CARTESIAN_POINT('Ctrl Pts',(16.6606126061973,19.6384970353346,-13.5368929079699));
#93498=CARTESIAN_POINT('Ctrl Pts',(16.6751755434729,19.70912819314,-13.5412151494539));
#93499=CARTESIAN_POINT('Ctrl Pts',(16.6933567603002,19.7790380332547,-13.545537390938));
#93500=CARTESIAN_POINT('Ctrl Pts',(16.7150553040206,19.8478291093979,-13.5498596324221));
#93501=CARTESIAN_POINT('Ctrl Pts',(16.7367551488124,19.9166243103389,-13.5541821330731));
#93502=CARTESIAN_POINT('Ctrl Pts',(16.7619725873318,19.9843001434081,-13.5585046337241));
#93503=CARTESIAN_POINT('Ctrl Pts',(16.7905571249898,20.0504753073033,-13.5628271343751));
#93504=CARTESIAN_POINT('Ctrl Pts',(16.8191715095119,20.1167195687348,-13.5671541484134));
#93505=CARTESIAN_POINT('Ctrl Pts',(16.851159810165,20.1814595804034,-13.5714811624517));
#93506=CARTESIAN_POINT('Ctrl Pts',(16.8863242283784,20.2443359777741,-13.57580817649));
#93507=CARTESIAN_POINT('Ctrl Pts',(16.9215100988957,20.3072507333393,-13.580137830254));
#93508=CARTESIAN_POINT('Ctrl Pts',(16.9598756760648,20.3682991960106,-13.5844674840181));
#93509=CARTESIAN_POINT('Ctrl Pts',(17.0011797410095,20.4271508746994,-13.5887971377822));
#93510=CARTESIAN_POINT('Ctrl Pts',(17.0425525940393,20.4861005653946,-13.5931340021826));
#93511=CARTESIAN_POINT('Ctrl Pts',(17.0868733907403,20.5428457872301,-13.597470866583));
#93512=CARTESIAN_POINT('Ctrl Pts',(17.1338612235974,20.5970897865047,-13.6018077309834));
#93513=CARTESIAN_POINT('Ctrl Pts',(17.1504345250049,20.6162224447881,-13.6033374069974));
#93514=CARTESIAN_POINT('Ctrl Pts',(17.167339302115,20.6350442778642,-13.6048670830114));
#93515=CARTESIAN_POINT('Ctrl Pts',(17.1845622179522,20.6535434342032,-13.6063967590254));
#93516=CARTESIAN_POINT('Ctrl Pts',(17.2339699045479,20.7066122947449,-13.6107849679563));
#93517=CARTESIAN_POINT('Ctrl Pts',(17.2862036327226,20.7572434590661,-13.6151731768872));
#93518=CARTESIAN_POINT('Ctrl Pts',(17.3409933109756,20.8051208750698,-13.6195613858181));
#93519=CARTESIAN_POINT('Ctrl Pts',(17.3957016722616,20.8529272330498,-13.6239430819193));
#93520=CARTESIAN_POINT('Ctrl Pts',(17.45295809287,20.8979876412173,-13.6283247780206));
#93521=CARTESIAN_POINT('Ctrl Pts',(17.5124544762692,20.9400215537851,-13.6327064741219));
#93522=CARTESIAN_POINT('Ctrl Pts',(17.5718809466832,20.9820060731604,-13.6370830213815));
#93523=CARTESIAN_POINT('Ctrl Pts',(17.6335417591178,21.0209708847354,-13.6414595686412));
#93524=CARTESIAN_POINT('Ctrl Pts',(17.6970957742218,21.0566756558408,-13.6458361159008));
#93525=CARTESIAN_POINT('Ctrl Pts',(17.760609484293,21.0923577834992,-13.6502098876178));
#93526=CARTESIAN_POINT('Ctrl Pts',(17.8260135952856,21.1247837371303,-13.6545836593348));
#93527=CARTESIAN_POINT('Ctrl Pts',(17.8929392167481,21.1537572568069,-13.6589574310518));
#93528=CARTESIAN_POINT('Ctrl Pts',(17.9598444725194,21.1827219597441,-13.6633298718153));
#93529=CARTESIAN_POINT('Ctrl Pts',(18.0282698771526,21.2082361229382,-13.6677023125789));
#93530=CARTESIAN_POINT('Ctrl Pts',(18.0978247669417,21.2301508296418,-13.6720747533424));
#93531=CARTESIAN_POINT('Ctrl Pts',(18.1673814352569,21.2520660967068,-13.6764473059098));
#93532=CARTESIAN_POINT('Ctrl Pts',(18.2380671853858,21.2703815814966,-13.6808198584771));
#93533=CARTESIAN_POINT('Ctrl Pts',(18.3094759435911,21.2849981498377,-13.6851924110445));
#93534=CARTESIAN_POINT('Ctrl Pts',(18.3809588124992,21.2996298878047,-13.6895695016118));
#93535=CARTESIAN_POINT('Ctrl Pts',(18.4531657140476,21.3105549478119,-13.6939465921792));
#93536=CARTESIAN_POINT('Ctrl Pts',(18.5256809453904,21.3177254618214,-13.6983236827465));
#93537=CARTESIAN_POINT('Ctrl Pts',(18.5982357799925,21.3248998919147,-13.7027031638054));
#93538=CARTESIAN_POINT('Ctrl Pts',(18.6710987974701,21.3283156708867,-13.7070826448644));
#93539=CARTESIAN_POINT('Ctrl Pts',(18.7438524696382,21.3279770732915,-13.7114621259233));
#93540=CARTESIAN_POINT('Ctrl Pts',(18.8167350972017,21.3276378755344,-13.7158493695831));
#93541=CARTESIAN_POINT('Ctrl Pts',(18.8895075103818,21.3235310394329,-13.7202366132428));
#93542=CARTESIAN_POINT('Ctrl Pts',(18.9617560691006,21.3157128481073,-13.7246238569025));
#93543=CARTESIAN_POINT('Ctrl Pts',(19.0108781271737,21.3103972313651,-13.7276067598373));
#93544=CARTESIAN_POINT('Ctrl Pts',(19.0597581560651,21.3033670563132,-13.730589662772));
#93545=CARTESIAN_POINT('Ctrl Pts',(19.1082694567066,21.2946533717911,-13.7335725657068));
#93546=CARTESIAN_POINT('Ctrl Pts',(19.1796354137561,21.2818344939807,-13.7379607746377));
#93547=CARTESIAN_POINT('Ctrl Pts',(19.2504813367646,21.2653198837036,-13.7423489835686));
#93548=CARTESIAN_POINT('Ctrl Pts',(19.3203952805281,21.2451655721633,-13.7467371924995));
#93549=CARTESIAN_POINT('Ctrl Pts',(19.3902054604073,21.2250411729629,-13.7511188886007));
#93550=CARTESIAN_POINT('Ctrl Pts',(19.4590859472337,21.201287928559,-13.755500584702));
#93551=CARTESIAN_POINT('Ctrl Pts',(19.5266340795883,21.1740130452636,-13.7598822808033));
#93552=CARTESIAN_POINT('Ctrl Pts',(19.5941028375116,21.1467702121268,-13.7642588280629));
#93553=CARTESIAN_POINT('Ctrl Pts',(19.660241906012,21.116014140384,-13.7686353753226));
#93554=CARTESIAN_POINT('Ctrl Pts',(19.7246645510875,21.0819015867273,-13.7730119225822));
#93555=CARTESIAN_POINT('Ctrl Pts',(19.7890463402578,21.0478106667563,-13.7773856942992));
#93556=CARTESIAN_POINT('Ctrl Pts',(19.8517134405363,21.0103677135302,-13.7817594660162));
#93557=CARTESIAN_POINT('Ctrl Pts',(19.9123011549783,20.9697766737641,-13.7861332377331));
#93558=CARTESIAN_POINT('Ctrl Pts',(19.9728704323752,20.9291979859878,-13.7905056784967));
#93559=CARTESIAN_POINT('Ctrl Pts',(20.031361179655,20.885473381869,-13.7948781192602));
#93560=CARTESIAN_POINT('Ctrl Pts',(20.087436722545,20.8388507419498,-13.7992505600238));
#93561=CARTESIAN_POINT('Ctrl Pts',(20.1435136992929,20.7922269098846,-13.8036231125911));
#93562=CARTESIAN_POINT('Ctrl Pts',(20.1971749793962,20.7427052048248,-13.8079956651585));
#93563=CARTESIAN_POINT('Ctrl Pts',(20.2481174066912,20.6905734110732,-13.8123682177258));
#93564=CARTESIAN_POINT('Ctrl Pts',(20.2991127039588,20.6383875129796,-13.8167453082932));
#93565=CARTESIAN_POINT('Ctrl Pts',(20.3473831767925,20.5835864635391,-13.8211223988605));
#93566=CARTESIAN_POINT('Ctrl Pts',(20.3926635636817,20.5264938929979,-13.8254994894278));
#93567=CARTESIAN_POINT('Ctrl Pts',(20.4379686798708,20.4693701420848,-13.8298789704868));
#93568=CARTESIAN_POINT('Ctrl Pts',(20.4802801788317,20.409952771581,-13.8342584515457));
#93569=CARTESIAN_POINT('Ctrl Pts',(20.5193756547004,20.3485951703498,-13.8386379326046));
#93570=CARTESIAN_POINT('Ctrl Pts',(20.5585404270376,20.2871288131823,-13.8430251762644));
#93571=CARTESIAN_POINT('Ctrl Pts',(20.5944775548135,20.2237157776927,-13.8474124199241));
#93572=CARTESIAN_POINT('Ctrl Pts',(20.6270104676965,20.1587343347117,-13.8517996635838));
#93573=CARTESIAN_POINT('Ctrl Pts',(20.6491297135927,20.114553215082,-13.8547825665186));
#93574=CARTESIAN_POINT('Ctrl Pts',(20.6696762814796,20.0696475457982,-13.8577654694534));
#93575=CARTESIAN_POINT('Ctrl Pts',(20.6886076987149,20.0241406668741,-13.8607483723882));
#93576=CARTESIAN_POINT('Ctrl Pts',(20.7164580900962,19.9571945754736,-13.8651365813191));
#93577=CARTESIAN_POINT('Ctrl Pts',(20.7409194707721,19.8886853205153,-13.86952479025));
#93578=CARTESIAN_POINT('Ctrl Pts',(20.761815975992,19.8189896113518,-13.8739129991809));
#93579=CARTESIAN_POINT('Ctrl Pts',(20.7826814673334,19.7493973421763,-13.8782946952822));
#93580=CARTESIAN_POINT('Ctrl Pts',(20.7999924489195,19.678622572649,-13.8826763913834));
#93581=CARTESIAN_POINT('Ctrl Pts',(20.8136211113039,19.607061906044,-13.8870580874847));
#93582=CARTESIAN_POINT('Ctrl Pts',(20.8272337589253,19.5355853289173,-13.8914346347443));
#93583=CARTESIAN_POINT('Ctrl Pts',(20.8371725931961,19.4633251607436,-13.895811182004));
#93584=CARTESIAN_POINT('Ctrl Pts',(20.8433600899068,19.3906914330412,-13.9001877292636));
#93585=CARTESIAN_POINT('Ctrl Pts',(20.849543662597,19.3181037685932,-13.9045615009806));
#93586=CARTESIAN_POINT('Ctrl Pts',(20.8519805772149,19.2451434941231,-13.9089352726976));
#93587=CARTESIAN_POINT('Ctrl Pts',(20.8506449171335,19.1722276545358,-13.9133090444145));
#93588=CARTESIAN_POINT('Ctrl Pts',(20.849309663498,19.0993340034833,-13.9176814851781));
#93589=CARTESIAN_POINT('Ctrl Pts',(20.8442041231405,19.0264852424758,-13.9220539259416));
#93590=CARTESIAN_POINT('Ctrl Pts',(20.8353544889709,18.9540986343324,-13.9264263667052));
#93591=CARTESIAN_POINT('Ctrl Pts',(20.8265046285152,18.8817101752555,-13.9307989192725));
#93592=CARTESIAN_POINT('Ctrl Pts',(20.8139105446929,18.8097843710748,-13.9351714718399));
#93593=CARTESIAN_POINT('Ctrl Pts',(20.7976501258783,18.7387319003335,-13.9395440244072));
#93594=CARTESIAN_POINT('Ctrl Pts',(20.7813728313877,18.667605688658,-13.9439211149745));
#93595=CARTESIAN_POINT('Ctrl Pts',(20.7614217126854,18.5973550912948,-13.9482982055419));
#93596=CARTESIAN_POINT('Ctrl Pts',(20.7379253105681,18.5283783261098,-13.9526752961092));
#93597=CARTESIAN_POINT('Ctrl Pts',(20.7144160761935,18.4593638901533,-13.9570547771681));
#93598=CARTESIAN_POINT('Ctrl Pts',(20.6873578824891,18.391625119753,-13.9614342582271));
#93599=CARTESIAN_POINT('Ctrl Pts',(20.656927489488,18.3255403057331,-13.965813739286));
#93600=CARTESIAN_POINT('Ctrl Pts',(20.6264431588197,18.259338356824,-13.9702009829457));
#93601=CARTESIAN_POINT('Ctrl Pts',(20.592574916967,18.1947966461511,-13.9745882266055));
#93602=CARTESIAN_POINT('Ctrl Pts',(20.5555452556645,18.1322683922466,-13.9789754702652));
#93603=CARTESIAN_POINT('Ctrl Pts',(20.5303686541483,18.0897552047994,-13.9819583732));
#93604=CARTESIAN_POINT('Ctrl Pts',(20.5037315602571,18.0481722056908,-13.9849412761348));
#93605=CARTESIAN_POINT('Ctrl Pts',(20.475714693788,18.0076218693017,-13.9879241790697));
#93606=CARTESIAN_POINT('Ctrl Pts',(20.434498513999,17.9479674480279,-13.9923123880006));
#93607=CARTESIAN_POINT('Ctrl Pts',(20.3901335538168,17.8903165376487,-13.9967005969315));
#93608=CARTESIAN_POINT('Ctrl Pts',(20.3428413739373,17.8350209182159,-14.0010888058624));
#93609=CARTESIAN_POINT('Ctrl Pts',(20.2956193834939,17.7798073666505,-14.0054705019636));
#93610=CARTESIAN_POINT('Ctrl Pts',(20.2454791086755,17.7269425302634,-14.0098521980649));
#93611=CARTESIAN_POINT('Ctrl Pts',(20.1926848492424,17.6767485504029,-14.0142338941661));
#93612=CARTESIAN_POINT('Ctrl Pts',(20.1399526272656,17.6266135524633,-14.0186104414258));
#93613=CARTESIAN_POINT('Ctrl Pts',(20.0845729637369,17.5791435071862,-14.0229869886854));
#93614=CARTESIAN_POINT('Ctrl Pts',(20.0268486678901,17.5346255424474,-14.027363535945));
#93615=CARTESIAN_POINT('Ctrl Pts',(19.9691609799527,17.4901358103547,-14.031737307662));
#93616=CARTESIAN_POINT('Ctrl Pts',(19.909131991,17.4485947380415,-14.036111079379));
#93617=CARTESIAN_POINT('Ctrl Pts',(19.8470983416195,17.4102498557868,-14.040484851096));
#93618=CARTESIAN_POINT('Ctrl Pts',(19.7850835692869,17.3719166420085,-14.0448572918595));
#93619=CARTESIAN_POINT('Ctrl Pts',(19.7210657576846,17.3367779408325,-14.0492297326231));
#93620=CARTESIAN_POINT('Ctrl Pts',(19.6554099365357,17.3050375846168,-14.0536021733866));
#93621=CARTESIAN_POINT('Ctrl Pts',(19.5897524365603,17.2732964167967,-14.057974725954));
#93622=CARTESIAN_POINT('Ctrl Pts',(19.5224572790425,17.2449539746122,-14.0623472785213));
#93623=CARTESIAN_POINT('Ctrl Pts',(19.4539119391454,17.2201670587726,-14.0667198310886));
#93624=CARTESIAN_POINT('Ctrl Pts',(19.3852954603089,17.1953544181369,-14.0710969216559));
#93625=CARTESIAN_POINT('Ctrl Pts',(19.3154266631739,17.1741048356878,-14.0754740122233));
#93626=CARTESIAN_POINT('Ctrl Pts',(19.2447099626415,17.1565257767354,-14.0798511027906));
#93627=CARTESIAN_POINT('Ctrl Pts',(19.1739546410942,17.1389371172064,-14.0842305838495));
#93628=CARTESIAN_POINT('Ctrl Pts',(19.1023509680274,17.1250230644095,-14.0886100649085));
#93629=CARTESIAN_POINT('Ctrl Pts',(19.0303127030118,17.114839752778,-14.0929895459674));
#93630=CARTESIAN_POINT('Ctrl Pts',(18.958146750655,17.104638391295,-14.0973767896271));
#93631=CARTESIAN_POINT('Ctrl Pts',(18.8855451489732,17.0981810190707,-14.1017640332868));
#93632=CARTESIAN_POINT('Ctrl Pts',(18.8129253294102,17.0954717462587,-14.1061512769466));
#93633=CARTESIAN_POINT('Ctrl Pts',(18.7635508497362,17.0936297018115,-14.1091341798814));
#93634=CARTESIAN_POINT('Ctrl Pts',(18.7141679744274,17.093519193629,-14.1121170828162));
#93635=CARTESIAN_POINT('Ctrl Pts',(18.6649065603162,17.0951278165748,-14.1150999857511));
#93636=CARTESIAN_POINT('Ctrl Pts',(18.5924370961486,17.0974942943756,-14.119488194682));
#93637=CARTESIAN_POINT('Ctrl Pts',(18.5199478924754,17.1035928606293,-14.1238764036129));
#93638=CARTESIAN_POINT('Ctrl Pts',(18.4478546672521,17.1134276297237,-14.1282646125438));
#93639=CARTESIAN_POINT('Ctrl Pts',(18.3758684403283,17.1232478023901,-14.132646308645));
#93640=CARTESIAN_POINT('Ctrl Pts',(18.3042774991947,17.1367931053665,-14.1370280047463));
#93641=CARTESIAN_POINT('Ctrl Pts',(18.2334957741926,17.1540156733828,-14.1414097008476));
#93642=CARTESIAN_POINT('Ctrl Pts',(18.1627972233503,17.171218003511,-14.1457862481072));
#93643=CARTESIAN_POINT('Ctrl Pts',(18.0929064660602,17.192088901349,-14.1501627953668));
#93644=CARTESIAN_POINT('Ctrl Pts',(18.0242288363214,17.2165291691252,-14.1545393426265));
#93645=CARTESIAN_POINT('Ctrl Pts',(17.9555947609373,17.2409539372388,-14.1589131143435));
#93646=CARTESIAN_POINT('Ctrl Pts',(17.888172739959,17.2689434226001,-14.1632868860604));
#93647=CARTESIAN_POINT('Ctrl Pts',(17.8223531243435,17.300348547195,-14.1676606577774));
#93648=CARTESIAN_POINT('Ctrl Pts',(17.7565535378581,17.331744115105,-14.172033098541));
#93649=CARTESIAN_POINT('Ctrl Pts',(17.6923558237627,17.3665530511359,-14.1764055393045));
#93650=CARTESIAN_POINT('Ctrl Pts',(17.6301289564787,17.4045787536471,-14.1807779800681));
#93651=CARTESIAN_POINT('Ctrl Pts',(17.5679004980471,17.4426054284796,-14.1851505326354));
#93652=CARTESIAN_POINT('Ctrl Pts',(17.5076433970478,17.4838487798649,-14.1895230852027));
#93653=CARTESIAN_POINT('Ctrl Pts',(17.4496992310202,17.5280678757603,-14.1938956377701));
#93654=CARTESIAN_POINT('Ctrl Pts',(17.3916949283512,17.5723328639015,-14.1982727283374));
#93655=CARTESIAN_POINT('Ctrl Pts',(17.3360087376082,17.6195794693658,-14.2026498189047));
#93656=CARTESIAN_POINT('Ctrl Pts',(17.2829499222257,17.6695258121554,-14.2070269094721));
#93657=CARTESIAN_POINT('Ctrl Pts',(17.2298621294548,17.7194994324966,-14.211406390531));
#93658=CARTESIAN_POINT('Ctrl Pts',(17.1794049028391,17.7721753771409,-14.21578587159));
#93659=CARTESIAN_POINT('Ctrl Pts',(17.1318494027618,17.8272361242722,-14.2201653526489));
#93660=CARTESIAN_POINT('Ctrl Pts',(17.0842096108798,17.8823944662081,-14.2245525963086));
#93661=CARTESIAN_POINT('Ctrl Pts',(17.0394821127485,17.9399456706587,-14.2289398399683));
#93662=CARTESIAN_POINT('Ctrl Pts',(16.9978963120797,17.999540968588,-14.2333270836281));
#93663=CARTESIAN_POINT('Ctrl Pts',(16.9696219748233,18.0400600285906,-14.2363099865629));
#93664=CARTESIAN_POINT('Ctrl Pts',(16.9427990411459,18.0815233957323,-14.2392928894977));
#93665=CARTESIAN_POINT('Ctrl Pts',(16.9174873693316,18.1238151663023,-14.2422757924325));
#93666=CARTESIAN_POINT('Ctrl Pts',(16.8789822269094,18.1881511240784,-14.2468135054362));
#93667=CARTESIAN_POINT('Ctrl Pts',(16.8438347836024,18.2546416817585,-14.2513512184399));
#93668=CARTESIAN_POINT('Ctrl Pts',(16.812283422931,18.3229153208065,-14.2558889314436));
#93669=CARTESIAN_POINT('Ctrl Pts',(16.7877996092446,18.3758955734034,-14.259410190666));
#93670=CARTESIAN_POINT('Ctrl Pts',(16.7654805065503,18.4299488289352,-14.2629314498885));
#93671=CARTESIAN_POINT('Ctrl Pts',(16.7454194503191,18.4848895418526,-14.2664527091109));
#93672=CARTESIAN_POINT('',(16.6170000012625,19.2109341693971,-13.288902674305));
#93673=CARTESIAN_POINT('Ctrl Pts',(16.7454194461219,18.4848895533475,-14.0426552599844));
#93674=CARTESIAN_POINT('Ctrl Pts',(16.772186960543,18.4115820298175,-14.0381451053267));
#93675=CARTESIAN_POINT('Ctrl Pts',(16.8029921867809,18.3397980179233,-14.0337655819529));
#93676=CARTESIAN_POINT('Ctrl Pts',(16.8976427044821,18.1490857001761,-14.0220205001263));
#93677=CARTESIAN_POINT('Ctrl Pts',(16.9689849518298,18.0343140293839,-14.0148420577156));
#93678=CARTESIAN_POINT('Ctrl Pts',(17.0971457051432,17.8662887412611,-14.0031497934935));
#93679=CARTESIAN_POINT('Ctrl Pts',(17.1467942049591,17.8080333367713,-13.9988302088228));
#93680=CARTESIAN_POINT('Ctrl Pts',(17.2060220522024,17.7457141580633,-13.9937348316427));
#93681=CARTESIAN_POINT('Ctrl Pts',(17.2126111809091,17.7388738976982,-13.9931687017829));
#93682=CARTESIAN_POINT('Ctrl Pts',(17.2224462449038,17.7288005427014,-13.9923243422884));
#93683=CARTESIAN_POINT('Ctrl Pts',(17.2256571117592,17.7255331655166,-13.9920487855116));
#93684=CARTESIAN_POINT('Ctrl Pts',(17.2313903512507,17.7197367764892,-13.9915568833361));
#93685=CARTESIAN_POINT('Ctrl Pts',(17.2339085440865,17.7172037013116,-13.991340866976));
#93686=CARTESIAN_POINT('Ctrl Pts',(17.2393381903972,17.711769541655,-13.9908751700234));
#93687=CARTESIAN_POINT('Ctrl Pts',(17.2422516423897,17.7088706017064,-13.9906253338696));
#93688=CARTESIAN_POINT('Ctrl Pts',(17.2503213435166,17.7008877267193,-13.9899335183858));
#93689=CARTESIAN_POINT('Ctrl Pts',(17.2554952068252,17.6958217904527,-13.9894901677374));
#93690=CARTESIAN_POINT('Ctrl Pts',(17.284054811362,17.6681435048652,-13.9870445275097));
#93691=CARTESIAN_POINT('Ctrl Pts',(17.307932019281,17.6460472658879,-13.9850059114159));
#93692=CARTESIAN_POINT('Ctrl Pts',(17.4542418809832,17.516779730233,-13.9726000423114));
#93693=CARTESIAN_POINT('Ctrl Pts',(17.5881860853029,17.4234671841384,-13.9616427791892));
#93694=CARTESIAN_POINT('Ctrl Pts',(17.8343782967887,17.2911003264758,-13.9433846914952));
#93695=CARTESIAN_POINT('Ctrl Pts',(17.9416765422598,17.244387351351,-13.9359438477381));
#93696=CARTESIAN_POINT('Ctrl Pts',(18.0658261081519,17.2021603260421,-13.9279367871828));
#93697=CARTESIAN_POINT('Ctrl Pts',(18.0794008269881,17.1976959683585,-13.9270688110954));
#93698=CARTESIAN_POINT('Ctrl Pts',(18.1010776420156,17.1908094724633,-13.9256945024792));
#93699=CARTESIAN_POINT('Ctrl Pts',(18.1091506623598,17.1882978995226,-13.9251852418818));
#93700=CARTESIAN_POINT('Ctrl Pts',(18.1234152322038,17.1839536437119,-13.9242898637858));
#93701=CARTESIAN_POINT('Ctrl Pts',(18.1296004856164,17.1821008113632,-13.92390309016));
#93702=CARTESIAN_POINT('Ctrl Pts',(18.1424111057155,17.1783270889427,-13.9231050215036));
#93703=CARTESIAN_POINT('Ctrl Pts',(18.1490375854781,17.1764102235303,-13.9226938618534));
#93704=CARTESIAN_POINT('Ctrl Pts',(18.1660708893333,17.1715730333901,-13.9216411523522));
#93705=CARTESIAN_POINT('Ctrl Pts',(18.1764910048977,17.1686999354118,-13.9210011438014));
#93706=CARTESIAN_POINT('Ctrl Pts',(18.2200727024244,17.157041730456,-13.9183404806011));
#93707=CARTESIAN_POINT('Ctrl Pts',(18.2534244414615,17.1489832276731,-13.9163433546428));
#93708=CARTESIAN_POINT('Ctrl Pts',(18.3408210818376,17.1301021427088,-13.9111992837305));
#93709=CARTESIAN_POINT('Ctrl Pts',(18.3951196385407,17.1205726991408,-13.9080917276388));
#93710=CARTESIAN_POINT('Ctrl Pts',(18.558087380421,17.0984895566629,-13.8989473222286));
#93711=CARTESIAN_POINT('Ctrl Pts',(18.6674211654396,17.0922235216181,-13.893059202318));
#93712=CARTESIAN_POINT('Ctrl Pts',(18.8224676635182,17.0953550632807,-13.8846160999925));
#93713=CARTESIAN_POINT('Ctrl Pts',(18.8681429011629,17.0977594858628,-13.8821158007853));
#93714=CARTESIAN_POINT('Ctrl Pts',(18.9364164280094,17.1035759246098,-13.8783162827748));
#93715=CARTESIAN_POINT('Ctrl Pts',(18.9590965582257,17.1058776445365,-13.877043720576));
#93716=CARTESIAN_POINT('Ctrl Pts',(18.9827750623048,17.1086677079573,-13.8757003527279));
#93717=CARTESIAN_POINT('Ctrl Pts',(18.983815525844,17.1087910901075,-13.8756412934919));
#93718=CARTESIAN_POINT('Ctrl Pts',(19.0033419620488,17.111121310921,-13.874532356538));
#93719=CARTESIAN_POINT('Ctrl Pts',(19.021797634707,17.1135710773078,-13.8734746599374));
#93720=CARTESIAN_POINT('Ctrl Pts',(19.0731066231257,17.1210716594486,-13.8705016082187));
#93721=CARTESIAN_POINT('Ctrl Pts',(19.1058753321376,17.1266530443555,-13.8685655654256));
#93722=CARTESIAN_POINT('Ctrl Pts',(19.1452810068388,17.1343236408959,-13.8661775442856));
#93723=CARTESIAN_POINT('Ctrl Pts',(19.1520584313266,17.135677395663,-13.8657646728492));
#93724=CARTESIAN_POINT('Ctrl Pts',(19.1631803939236,17.1379556399812,-13.8650834176778));
#93725=CARTESIAN_POINT('Ctrl Pts',(19.1675289266338,17.1388606711713,-13.8648161199363));
#93726=CARTESIAN_POINT('Ctrl Pts',(19.1753590643847,17.1405160322012,-13.8643330723287));
#93727=CARTESIAN_POINT('Ctrl Pts',(19.1788416478259,17.1412614675625,-13.8641176045042));
#93728=CARTESIAN_POINT('Ctrl Pts',(19.1864395999814,17.1429078463782,-13.8636461447825));
#93729=CARTESIAN_POINT('Ctrl Pts',(19.1905541150568,17.1438122758649,-13.8633899597197));
#93730=CARTESIAN_POINT('Ctrl Pts',(19.2021937108581,17.146407271562,-13.8626628083845));
#93731=CARTESIAN_POINT('Ctrl Pts',(19.2097122002091,17.1481266680721,-13.8621902364993));
#93732=CARTESIAN_POINT('Ctrl Pts',(19.2565499218101,17.1591076143776,-13.8592290357217));
#93733=CARTESIAN_POINT('Ctrl Pts',(19.2956040176872,17.1694512696271,-13.8566841535996));
#93734=CARTESIAN_POINT('Ctrl Pts',(19.5036481990321,17.2309736327929,-13.8428030798992));
#93735=CARTESIAN_POINT('Ctrl Pts',(19.6660334920268,17.3020258847687,-13.8308761830411));
#93736=CARTESIAN_POINT('Ctrl Pts',(19.8993933048557,17.4410884904146,-13.8132954712525));
#93737=CARTESIAN_POINT('Ctrl Pts',(19.9777034384407,17.4952102720973,-13.807291482931));
#93738=CARTESIAN_POINT('Ctrl Pts',(20.0629554360456,17.5630442267656,-13.800643043298));
#93739=CARTESIAN_POINT('Ctrl Pts',(20.073707399759,17.5717730849976,-13.7998021978815));
#93740=CARTESIAN_POINT('Ctrl Pts',(20.0907853702842,17.5859179154142,-13.7984626409209));
#93741=CARTESIAN_POINT('Ctrl Pts',(20.097166282787,17.5912666851531,-13.7979612272631));
#93742=CARTESIAN_POINT('Ctrl Pts',(20.1084236618522,17.6008167731039,-13.7970749364925));
#93743=CARTESIAN_POINT('Ctrl Pts',(20.1133128050623,17.6050029222795,-13.7966894451928));
#93744=CARTESIAN_POINT('Ctrl Pts',(20.1234437014717,17.6137575184025,-13.7958894311574));
#93745=CARTESIAN_POINT('Ctrl Pts',(20.1286821981731,17.6183296284381,-13.7954750665526));
#93746=CARTESIAN_POINT('Ctrl Pts',(20.1421935539587,17.6302399925289,-13.7944044513535));
#93747=CARTESIAN_POINT('Ctrl Pts',(20.1504316775105,17.637617466541,-13.793749846204));
#93748=CARTESIAN_POINT('Ctrl Pts',(20.18564352839,17.6696513837465,-13.7909434514846));
#93749=CARTESIAN_POINT('Ctrl Pts',(20.2120351048847,17.6949403193713,-13.7888186075554));
#93750=CARTESIAN_POINT('Ctrl Pts',(20.2801018311239,17.7636310703656,-13.7832657133661));
#93751=CARTESIAN_POINT('Ctrl Pts',(20.3206051550771,17.8081484124568,-13.779885786088));
#93752=CARTESIAN_POINT('Ctrl Pts',(20.4657756217887,17.9820490384535,-13.7673389447173));
#93753=CARTESIAN_POINT('Ctrl Pts',(20.556955443388,18.121874937997,-13.7585778867394));
#93754=CARTESIAN_POINT('Ctrl Pts',(20.6551319224734,18.3199681555161,-13.7461585627983));
#93755=CARTESIAN_POINT('Ctrl Pts',(20.6775267384532,18.3699361882389,-13.7430205534932));
#93756=CARTESIAN_POINT('Ctrl Pts',(20.7012336832368,18.4288506413052,-13.7392523631202));
#93757=CARTESIAN_POINT('Ctrl Pts',(20.7044583868121,18.4370105145514,-13.7387289609956));
#93758=CARTESIAN_POINT('Ctrl Pts',(20.7092581730469,18.4493804407384,-13.7379329190124));
#93759=CARTESIAN_POINT('Ctrl Pts',(20.7108707690888,18.4535759677009,-13.7376624753491));
#93760=CARTESIAN_POINT('Ctrl Pts',(20.713738306732,18.4611080448777,-13.7371760996539));
#93761=CARTESIAN_POINT('Ctrl Pts',(20.7149981924803,18.4644426555173,-13.73696046762));
#93762=CARTESIAN_POINT('Ctrl Pts',(20.7177140092992,18.4716860429504,-13.7364914056217));
#93763=CARTESIAN_POINT('Ctrl Pts',(20.7191667931368,18.4755958930546,-13.7362377976135));
#93764=CARTESIAN_POINT('Ctrl Pts',(20.7232064478981,18.4865669386609,-13.7355250579913));
#93765=CARTESIAN_POINT('Ctrl Pts',(20.725767232167,18.4936375799587,-13.7350644183323));
#93766=CARTESIAN_POINT('Ctrl Pts',(20.740681854981,18.5355142391036,-13.7323292424348));
#93767=CARTESIAN_POINT('Ctrl Pts',(20.7521599996268,18.5706228357228,-13.7300077413549));
#93768=CARTESIAN_POINT('Ctrl Pts',(20.7865881523832,18.6860709763428,-13.7223220446735));
#93769=CARTESIAN_POINT('Ctrl Pts',(20.8057014669072,18.7674689253233,-13.7168251389049));
#93770=CARTESIAN_POINT('Ctrl Pts',(20.8507472032,19.0275946055128,-13.6993878992263));
#93771=CARTESIAN_POINT('Ctrl Pts',(20.8586826193205,19.2086589435697,-13.6875184404006));
#93772=CARTESIAN_POINT('Ctrl Pts',(20.8416464663426,19.4110637362939,-13.6750209748159));
#93773=CARTESIAN_POINT('Ctrl Pts',(20.8393920245303,19.433539009473,-13.6736425388368));
#93774=CARTESIAN_POINT('Ctrl Pts',(20.8356813389835,19.4653902656907,-13.6717016151011));
#93775=CARTESIAN_POINT('Ctrl Pts',(20.8345211680315,19.4747985692403,-13.6711298567217));
#93776=CARTESIAN_POINT('Ctrl Pts',(20.8325293674646,19.49010383894,-13.6702021846301));
#93777=CARTESIAN_POINT('Ctrl Pts',(20.8317359901649,19.4960055713757,-13.6698450682893));
#93778=CARTESIAN_POINT('Ctrl Pts',(20.830019674302,19.5083772612346,-13.6690976714534));
#93779=CARTESIAN_POINT('Ctrl Pts',(20.8290916545913,19.5148464594156,-13.6687075557897));
#93780=CARTESIAN_POINT('Ctrl Pts',(20.8268058318289,19.5302723180431,-13.6677789450173));
#93781=CARTESIAN_POINT('Ctrl Pts',(20.8254204598134,19.5392248116207,-13.6672413282709));
#93782=CARTESIAN_POINT('Ctrl Pts',(20.8205241904645,19.5695749222207,-13.6654229726085));
#93783=CARTESIAN_POINT('Ctrl Pts',(20.8167419583552,19.5909278333102,-13.6641508360488));
#93784=CARTESIAN_POINT('Ctrl Pts',(20.7940865938178,19.708300429984,-13.6571921801672));
#93785=CARTESIAN_POINT('Ctrl Pts',(20.76890064198,19.8029857492757,-13.6517121649714));
#93786=CARTESIAN_POINT('Ctrl Pts',(20.6836228057753,20.0525232618312,-13.6372227301703));
#93787=CARTESIAN_POINT('Ctrl Pts',(20.6117481725394,20.2025852827036,-13.6284820837651));
#93788=CARTESIAN_POINT('Ctrl Pts',(20.5026441817471,20.3750673776048,-13.6168430415648));
#93789=CARTESIAN_POINT('Ctrl Pts',(20.4813024986499,20.4068631482235,-13.6146214641122));
#93790=CARTESIAN_POINT('Ctrl Pts',(20.4549201536874,20.4439538222571,-13.6119159865254));
#93791=CARTESIAN_POINT('Ctrl Pts',(20.45069816667,20.4498255342641,-13.6114842039963));
#93792=CARTESIAN_POINT('Ctrl Pts',(20.44377710014,20.4593476589639,-13.6107780840839));
#93793=CARTESIAN_POINT('Ctrl Pts',(20.4410961780586,20.4630112810115,-13.6105049717883));
#93794=CARTESIAN_POINT('Ctrl Pts',(20.4362870973595,20.4695389824007,-13.6100157285358));
#93795=CARTESIAN_POINT('Ctrl Pts',(20.4341634631601,20.4724063303861,-13.6097999127502));
#93796=CARTESIAN_POINT('Ctrl Pts',(20.4295612152127,20.4785875869001,-13.6093326834355));
#93797=CARTESIAN_POINT('Ctrl Pts',(20.4270801657839,20.4818995540754,-13.609081103897));
#93798=CARTESIAN_POINT('Ctrl Pts',(20.4201536805303,20.49108948057,-13.6083796404286));
#93799=CARTESIAN_POINT('Ctrl Pts',(20.4156872878883,20.4969514667016,-13.6079283228567));
#93800=CARTESIAN_POINT('Ctrl Pts',(20.3901521341403,20.5301049351669,-13.605354306403));
#93801=CARTESIAN_POINT('Ctrl Pts',(20.3684510263718,20.5569001624006,-13.6031907385125));
#93802=CARTESIAN_POINT('Ctrl Pts',(20.2977990840365,20.6399073701967,-13.5962518038293));
#93803=CARTESIAN_POINT('Ctrl Pts',(20.2465309439854,20.6940685972412,-13.5913689263735));
#93804=CARTESIAN_POINT('Ctrl Pts',(20.0516358251991,20.8793242132415,-13.5736345637129));
#93805=CARTESIAN_POINT('Ctrl Pts',(19.8929451092822,20.9932311365298,-13.5607885073879));
#93806=CARTESIAN_POINT('Ctrl Pts',(19.7022563751483,21.0937143545054,-13.5475467500893));
#93807=CARTESIAN_POINT('Ctrl Pts',(19.6834527776957,21.1032666889502,-13.5462609631226));
#93808=CARTESIAN_POINT('Ctrl Pts',(19.6570599207315,21.1161819229198,-13.5444832774506));
#93809=CARTESIAN_POINT('Ctrl Pts',(19.6495893727501,21.1197833507891,-13.5439830780212));
#93810=CARTESIAN_POINT('Ctrl Pts',(19.6366465214609,21.1259294175532,-13.543121546231));
#93811=CARTESIAN_POINT('Ctrl Pts',(19.631184185674,21.1284947079627,-13.542759499694));
#93812=CARTESIAN_POINT('Ctrl Pts',(19.6198392828376,21.133763552057,-13.5420107294257));
#93813=CARTESIAN_POINT('Ctrl Pts',(19.613955127098,21.1364635514253,-13.5416241315505));
#93814=CARTESIAN_POINT('Ctrl Pts',(19.6001265799718,21.1427322780808,-13.5407196468724));
#93815=CARTESIAN_POINT('Ctrl Pts',(19.5921723309973,21.1462790756062,-13.5402025181951));
#93816=CARTESIAN_POINT('Ctrl Pts',(19.5661908523827,21.1576725266623,-13.5385233956705));
#93817=CARTESIAN_POINT('Ctrl Pts',(19.5480758285313,21.1653173040109,-13.537368289663));
#93818=CARTESIAN_POINT('Ctrl Pts',(19.4543620796197,21.2033365518719,-13.5314686907377));
#93819=CARTESIAN_POINT('Ctrl Pts',(19.3771580315603,21.229582747823,-13.5268645310888));
#93820=CARTESIAN_POINT('Ctrl Pts',(19.1363832251023,21.2962135020004,-13.5130215469545));
#93821=CARTESIAN_POINT('Ctrl Pts',(18.9693800175131,21.3215961515659,-13.5041631846135));
#93822=CARTESIAN_POINT('Ctrl Pts',(18.7474453267082,21.3286390134784,-13.4916795887112));
#93823=CARTESIAN_POINT('Ctrl Pts',(18.6937030129506,21.3282980144424,-13.4885974125898));
#93824=CARTESIAN_POINT('Ctrl Pts',(18.6313118133552,21.3255260497222,-13.4848913826419));
#93825=CARTESIAN_POINT('Ctrl Pts',(18.6225893090225,21.3250844189912,-13.4843703526577));
#93826=CARTESIAN_POINT('Ctrl Pts',(18.6093910426849,21.3243342691688,-13.4835772200895));
#93827=CARTESIAN_POINT('Ctrl Pts',(18.6049129953709,21.3240654674834,-13.4833072898137));
#93828=CARTESIAN_POINT('Ctrl Pts',(18.5968788155769,21.3235575694124,-13.4828214612585));
#93829=CARTESIAN_POINT('Ctrl Pts',(18.593322405034,21.3233237245459,-13.4826058600526));
#93830=CARTESIAN_POINT('Ctrl Pts',(18.5855986262203,21.3227962697519,-13.4821364250001));
#93831=CARTESIAN_POINT('Ctrl Pts',(18.5814315863527,21.322499308818,-13.4818824107136));
#93832=CARTESIAN_POINT('Ctrl Pts',(18.5697358180239,21.3216310163151,-13.4811674056511));
#93833=CARTESIAN_POINT('Ctrl Pts',(18.5622093155426,21.321031745093,-13.480704891678));
#93834=CARTESIAN_POINT('Ctrl Pts',(18.5173686190228,21.3172199596104,-13.4779357582697));
#93835=CARTESIAN_POINT('Ctrl Pts',(18.4801442511162,21.3130581660376,-13.4755808336327));
#93836=CARTESIAN_POINT('Ctrl Pts',(18.3583168866353,21.2961545684371,-13.467730711479));
#93837=CARTESIAN_POINT('Ctrl Pts',(18.2743769929017,21.2792727550932,-13.4620969643094));
#93838=CARTESIAN_POINT('Ctrl Pts',(18.020077711642,21.2118809968618,-13.44471710258));
#93839=CARTESIAN_POINT('Ctrl Pts',(17.8548271077964,21.1449827020762,-13.4330520983073));
#93840=CARTESIAN_POINT('Ctrl Pts',(17.6799397817977,21.0470737430313,-13.420717269158));
#93841=CARTESIAN_POINT('Ctrl Pts',(17.6602091605669,21.0356048971113,-13.4193243496196));
#93842=CARTESIAN_POINT('Ctrl Pts',(17.6326734614566,21.0189977872508,-13.4173778654637));
#93843=CARTESIAN_POINT('Ctrl Pts',(17.6247115938295,21.0141237837448,-13.416814735823));
#93844=CARTESIAN_POINT('Ctrl Pts',(17.6112424234108,21.0057554035469,-13.4158614750884));
#93845=CARTESIAN_POINT('Ctrl Pts',(17.6057186088762,21.0022879830647,-13.4154703594317));
#93846=CARTESIAN_POINT('Ctrl Pts',(17.5947619970581,20.9953394866808,-13.4146941845989));
#93847=CARTESIAN_POINT('Ctrl Pts',(17.5893289171412,20.9918589906455,-13.414309109558));
#93848=CARTESIAN_POINT('Ctrl Pts',(17.5784352157938,20.9848099054516,-13.4135365808641));
#93849=CARTESIAN_POINT('Ctrl Pts',(17.5729750064291,20.9812408076113,-13.4131491517415));
#93850=CARTESIAN_POINT('Ctrl Pts',(17.5534356229574,20.9683394837786,-13.4117618703299));
#93851=CARTESIAN_POINT('Ctrl Pts',(17.5394515131731,20.9588639096931,-13.4107673956052));
#93852=CARTESIAN_POINT('Ctrl Pts',(17.4132489974387,20.8711274689274,-13.4017735847869));
#93853=CARTESIAN_POINT('Ctrl Pts',(17.3087449610218,20.7823247702269,-13.394217729598));
#93854=CARTESIAN_POINT('Ctrl Pts',(17.1001166252823,20.5669798550728,-13.3778950017079));
#93855=CARTESIAN_POINT('Ctrl Pts',(17.0006189743921,20.4372259685206,-13.3692254413318));
#93856=CARTESIAN_POINT('Ctrl Pts',(16.9097822585343,20.2852981598106,-13.3588208783816));
#93857=CARTESIAN_POINT('Ctrl Pts',(16.9026838643018,20.2731525746587,-13.3579872729009));
#93858=CARTESIAN_POINT('Ctrl Pts',(16.8929614775417,20.2561300444947,-13.3568151139102));
#93859=CARTESIAN_POINT('Ctrl Pts',(16.8902346034894,20.2513118821481,-13.3564829157797));
#93860=CARTESIAN_POINT('Ctrl Pts',(16.8858822859146,20.2435508304247,-13.3559470450458));
#93861=CARTESIAN_POINT('Ctrl Pts',(16.8842448771525,20.2406146306563,-13.3557441357005));
#93862=CARTESIAN_POINT('Ctrl Pts',(16.8808341614646,20.2344641426313,-13.3553187051586));
#93863=CARTESIAN_POINT('Ctrl Pts',(16.8790622197217,20.2312491396409,-13.3550960960329));
#93864=CARTESIAN_POINT('Ctrl Pts',(16.8747876279606,20.2234453939803,-13.354555239141));
#93865=CARTESIAN_POINT('Ctrl Pts',(16.8722936017513,20.2188519759941,-13.3542364477892));
#93866=CARTESIAN_POINT('Ctrl Pts',(16.863585958373,20.2026719080558,-13.3531121280602));
#93867=CARTESIAN_POINT('Ctrl Pts',(16.8574634406875,20.1910369288681,-13.3523011333792));
#93868=CARTESIAN_POINT('Ctrl Pts',(16.8216449256196,20.1214025742036,-13.3474359490934));
#93869=CARTESIAN_POINT('Ctrl Pts',(16.7945337876491,20.0621192387778,-13.3432478442596));
#93870=CARTESIAN_POINT('Ctrl Pts',(16.7016675229783,19.831470838242,-13.3270234145345));
#93871=CARTESIAN_POINT('Ctrl Pts',(16.6555424809737,19.6530311175561,-13.3147001371237));
#93872=CARTESIAN_POINT('Ctrl Pts',(16.6297590820114,19.4445830695436,-13.301396301187));
#93873=CARTESIAN_POINT('Ctrl Pts',(16.6270006060779,19.4182306438173,-13.2997318591792));
#93874=CARTESIAN_POINT('Ctrl Pts',(16.6216845007598,19.356222630682,-13.2958565775225));
#93875=CARTESIAN_POINT('Ctrl Pts',(16.6195337089458,19.3205396234777,-13.2936584446058));
#93876=CARTESIAN_POINT('Ctrl Pts',(16.617898152872,19.2736622878227,-13.2908108231166));
#93877=CARTESIAN_POINT('Ctrl Pts',(16.6175971716277,19.2625040315736,-13.2901359642465));
#93878=CARTESIAN_POINT('Ctrl Pts',(16.6172522422965,19.2444074776532,-13.28904615179));
#93879=CARTESIAN_POINT('Ctrl Pts',(16.617154128961,19.237470537487,-13.2886295088657));
#93880=CARTESIAN_POINT('Ctrl Pts',(16.6170502015178,19.2262073902167,-13.2879548009108));
#93881=CARTESIAN_POINT('Ctrl Pts',(16.6170235456931,19.2218814682278,-13.2876960853544));
#93882=CARTESIAN_POINT('Ctrl Pts',(16.617003429377,19.2153852082466,-13.2873081997628));
#93883=CARTESIAN_POINT('Ctrl Pts',(16.6170000462453,19.2132149325987,-13.28717872004));
#93884=CARTESIAN_POINT('Ctrl Pts',(16.6170000004709,19.2110446506181,-13.2870493445712));
#93885=CARTESIAN_POINT('Ctrl Pts',(16.6170000013281,19.2109250126717,-13.2890562789747));
#93886=CARTESIAN_POINT('Ctrl Pts',(16.6170027225446,19.1341011600434,-13.2844612169082));
#93887=CARTESIAN_POINT('Ctrl Pts',(16.6211915380442,19.0573628289812,-13.2798661548417));
#93888=CARTESIAN_POINT('Ctrl Pts',(16.6295128869012,18.9811674722736,-13.2752710927752));
#93889=CARTESIAN_POINT('Ctrl Pts',(16.6378461991752,18.9048625712073,-13.2706694244908));
#93890=CARTESIAN_POINT('Ctrl Pts',(16.6503238258347,18.8291026016853,-13.2660677562064));
#93891=CARTESIAN_POINT('Ctrl Pts',(16.666841073,18.7543349471174,-13.261466087922));
#93892=CARTESIAN_POINT('Ctrl Pts',(16.6833972601622,18.679391025148,-13.2568535710412));
#93893=CARTESIAN_POINT('Ctrl Pts',(16.7040119873824,18.6054444839208,-13.2522410541604));
#93894=CARTESIAN_POINT('Ctrl Pts',(16.7285306582113,18.5329279395626,-13.2476285372796));
#93895=CARTESIAN_POINT('Ctrl Pts',(16.7339690428732,18.5168433456905,-13.2466054540451));
#93896=CARTESIAN_POINT('Ctrl Pts',(16.7395993072442,18.5008290221139,-13.2455823708106));
#93897=CARTESIAN_POINT('Ctrl Pts',(16.7454194503191,18.4848895418526,-13.2445592875761));
#93898=CARTESIAN_POINT('Origin',(18.734,19.211,0.));
#93899=CARTESIAN_POINT('',(16.7437496504382,18.4842640742323,-12.4443820746265));
#93900=CARTESIAN_POINT('',(16.7454195353148,18.4848893090773,-12.6679318638109));
#93901=CARTESIAN_POINT('',(16.7454194503191,18.4848895418526,0.));
#93902=CARTESIAN_POINT('Ctrl Pts',(16.7454195353148,18.4848893090773,-12.6679318638109));
#93903=CARTESIAN_POINT('Ctrl Pts',(16.7052039069762,18.5950268044879,-12.6745735300496));
#93904=CARTESIAN_POINT('Ctrl Pts',(16.6741842952664,18.7083782324412,-12.6809438201612));
#93905=CARTESIAN_POINT('Ctrl Pts',(16.6289120083485,18.9517192629599,-12.6943852175721));
#93906=CARTESIAN_POINT('Ctrl Pts',(16.6169601910973,19.0815565992033,-12.7014276223083));
#93907=CARTESIAN_POINT('Ctrl Pts',(16.6170011043132,19.2149245295939,-12.7092186109573));
#93908=CARTESIAN_POINT('Ctrl Pts',(16.6170097091036,19.2181996006972,-12.7094102823505));
#93909=CARTESIAN_POINT('Ctrl Pts',(16.617103391712,19.2371333371875,-12.7105204617434));
#93910=CARTESIAN_POINT('Ctrl Pts',(16.6173546002336,19.2527901998201,-12.7114467850276));
#93911=CARTESIAN_POINT('Ctrl Pts',(16.6179364422518,19.2742257229631,-12.7127280872513));
#93912=CARTESIAN_POINT('Ctrl Pts',(16.6181171315258,19.2800083877722,-12.7130750497816));
#93913=CARTESIAN_POINT('Ctrl Pts',(16.618441995659,19.2891982068463,-12.7136286204981));
#93914=CARTESIAN_POINT('Ctrl Pts',(16.6185707051684,19.2926059279293,-12.7138343687611));
#93915=CARTESIAN_POINT('Ctrl Pts',(16.6188536043165,19.2996449963843,-12.7142603779025));
#93916=CARTESIAN_POINT('Ctrl Pts',(16.6190089118102,19.3032762518521,-12.7144807030064));
#93917=CARTESIAN_POINT('Ctrl Pts',(16.6194013908054,19.311930724983,-12.7150071183992));
#93918=CARTESIAN_POINT('Ctrl Pts',(16.619647110743,19.3169535169137,-12.7153136835633));
#93919=CARTESIAN_POINT('Ctrl Pts',(16.6205368812465,19.3339037197371,-12.7163516706919));
#93920=CARTESIAN_POINT('Ctrl Pts',(16.6212639692446,19.3458262879094,-12.7170875202413));
#93921=CARTESIAN_POINT('Ctrl Pts',(16.6311148216221,19.4875998170897,-12.725900906759));
#93922=CARTESIAN_POINT('Ctrl Pts',(16.652094711903,19.6163356545092,-12.7345186157036));
#93923=CARTESIAN_POINT('Ctrl Pts',(16.7254974566956,19.899444657587,-12.7538452517802));
#93924=CARTESIAN_POINT('Ctrl Pts',(16.7841817064134,20.0513962791147,-12.7644510068483));
#93925=CARTESIAN_POINT('Ctrl Pts',(16.8706981570032,20.2161655755375,-12.7759141072705));
#93926=CARTESIAN_POINT('Ctrl Pts',(16.8820773058399,20.2369795314881,-12.7773627487528));
#93927=CARTESIAN_POINT('Ctrl Pts',(16.8985833620852,20.2660015239528,-12.7793842660749));
#93928=CARTESIAN_POINT('Ctrl Pts',(16.9034200610182,20.2743717798231,-12.7799674882416));
#93929=CARTESIAN_POINT('Ctrl Pts',(16.9113457913493,20.2878734848133,-12.7809086614212));
#93930=CARTESIAN_POINT('Ctrl Pts',(16.914399521296,20.2930253997259,-12.7812678855963));
#93931=CARTESIAN_POINT('Ctrl Pts',(16.9208163214209,20.3037471249721,-12.7820157029795));
#93932=CARTESIAN_POINT('Ctrl Pts',(16.9241832932101,20.3093145363157,-12.7824041488162));
#93933=CARTESIAN_POINT('Ctrl Pts',(16.9322154696904,20.3224588056794,-12.783321601295));
#93934=CARTESIAN_POINT('Ctrl Pts',(16.9369029054475,20.3300219867452,-12.7838497853492));
#93935=CARTESIAN_POINT('Ctrl Pts',(16.9526722167393,20.355111133069,-12.7856030608958));
#93936=CARTESIAN_POINT('Ctrl Pts',(16.9639641003298,20.3725041606249,-12.786820376726));
#93937=CARTESIAN_POINT('Ctrl Pts',(17.0256054181123,20.4644639285047,-12.7932712650584));
#93938=CARTESIAN_POINT('Ctrl Pts',(17.0804171160334,20.5359340336159,-12.7983318959407));
#93939=CARTESIAN_POINT('Ctrl Pts',(17.2287601945877,20.7057586991185,-12.8107686852582));
#93940=CARTESIAN_POINT('Ctrl Pts',(17.3274918566426,20.7990122929935,-12.8179808560139));
#93941=CARTESIAN_POINT('Ctrl Pts',(17.49397403342,20.9284717959191,-12.8296567230741));
#93942=CARTESIAN_POINT('Ctrl Pts',(17.5559174155828,20.9715375976412,-12.8339174608333));
#93943=CARTESIAN_POINT('Ctrl Pts',(17.6280873322142,21.0161970053271,-12.8389474680712));
#93944=CARTESIAN_POINT('Ctrl Pts',(17.6361903782605,21.0211362058263,-12.8395131308456));
#93945=CARTESIAN_POINT('Ctrl Pts',(17.6482524128825,21.0283778221811,-12.8403569256539));
#93946=CARTESIAN_POINT('Ctrl Pts',(17.6521862350008,21.0307222173841,-12.8406323900183));
#93947=CARTESIAN_POINT('Ctrl Pts',(17.6592016978509,21.0348723548971,-12.8411241911849));
#93948=CARTESIAN_POINT('Ctrl Pts',(17.6622803319866,21.0366830804448,-12.8413401994724));
#93949=CARTESIAN_POINT('Ctrl Pts',(17.6689124245777,21.0405612472733,-12.8418059520832));
#93950=CARTESIAN_POINT('Ctrl Pts',(17.6724672751306,21.0426261010944,-12.8420558523538));
#93951=CARTESIAN_POINT('Ctrl Pts',(17.6823041924359,21.0483016710118,-12.8427480218648));
#93952=CARTESIAN_POINT('Ctrl Pts',(17.6885987479381,21.0518904694853,-12.8431916646886));
#93953=CARTESIAN_POINT('Ctrl Pts',(17.7233138396346,21.0714475812456,-12.8456418709247));
#93954=CARTESIAN_POINT('Ctrl Pts',(17.7520802240921,21.0867891673616,-12.8476849176515));
#93955=CARTESIAN_POINT('Ctrl Pts',(17.9264327534546,21.1746647794746,-12.8600922840244));
#93956=CARTESIAN_POINT('Ctrl Pts',(18.0796263352478,21.2308859544734,-12.8710454969299));
#93957=CARTESIAN_POINT('Ctrl Pts',(18.3512830812101,21.2963913895576,-12.8892984033384));
#93958=CARTESIAN_POINT('Ctrl Pts',(18.4669061863381,21.3143302605256,-12.8967379696179));
#93959=CARTESIAN_POINT('Ctrl Pts',(18.5976891509857,21.3236553269854,-12.9047438411114));
#93960=CARTESIAN_POINT('Ctrl Pts',(18.6119522492214,21.3245272745922,-12.905611801654));
#93961=CARTESIAN_POINT('Ctrl Pts',(18.6346668396305,21.3256851777068,-12.9069860904373));
#93962=CARTESIAN_POINT('Ctrl Pts',(18.6431129130332,21.3260650151293,-12.9074953466142));
#93963=CARTESIAN_POINT('Ctrl Pts',(18.6580129416594,21.3266456830078,-12.9083907196266));
#93964=CARTESIAN_POINT('Ctrl Pts',(18.6644659223258,21.3268676004277,-12.9087774925651));
#93965=CARTESIAN_POINT('Ctrl Pts',(18.6778148984399,21.3272655357924,-12.9095755623785));
#93966=CARTESIAN_POINT('Ctrl Pts',(18.6847109487929,21.3274373779497,-12.90998672386));
#93967=CARTESIAN_POINT('Ctrl Pts',(18.7024143993206,21.3277919547547,-12.9110394433812));
#93968=CARTESIAN_POINT('Ctrl Pts',(18.7132226663786,21.3279256337554,-12.9116794600636));
#93969=CARTESIAN_POINT('Ctrl Pts',(18.7583375612461,21.3281380695703,-12.9143402016399));
#93970=CARTESIAN_POINT('Ctrl Pts',(18.7926436572675,21.3274656955864,-12.9163373960773));
#93971=CARTESIAN_POINT('Ctrl Pts',(18.8819742401333,21.3235409984975,-12.9214816830752));
#93972=CARTESIAN_POINT('Ctrl Pts',(18.9369157781641,21.3189733581146,-12.9245893824405));
#93973=CARTESIAN_POINT('Ctrl Pts',(19.1001554904761,21.2989598321755,-12.9337340379255));
#93974=CARTESIAN_POINT('Ctrl Pts',(19.2075002130258,21.2772634235775,-12.9396222654781));
#93975=CARTESIAN_POINT('Ctrl Pts',(19.3568792873577,21.2348134725387,-12.9480771111795));
#93976=CARTESIAN_POINT('Ctrl Pts',(19.4006488841573,21.2208205398169,-12.9505891240598));
#93977=CARTESIAN_POINT('Ctrl Pts',(19.4649304433797,21.1979390318556,-12.9543731565326));
#93978=CARTESIAN_POINT('Ctrl Pts',(19.48581374606,21.1901316459796,-12.955617730027));
#93979=CARTESIAN_POINT('Ctrl Pts',(19.5544213984807,21.1632395748825,-12.9597687632216));
#93980=CARTESIAN_POINT('Ctrl Pts',(19.6015704635986,21.1427482232981,-12.9627220878745));
#93981=CARTESIAN_POINT('Ctrl Pts',(19.6550282824944,21.1171631493982,-12.9662396426317));
#93982=CARTESIAN_POINT('Ctrl Pts',(19.6621144097553,21.1137229665191,-12.9667094201342));
#93983=CARTESIAN_POINT('Ctrl Pts',(19.6733817542589,21.1081749640014,-12.9674622573819));
#93984=CARTESIAN_POINT('Ctrl Pts',(19.6775755405013,21.10609264224,-12.9677437720412));
#93985=CARTESIAN_POINT('Ctrl Pts',(19.6849752315678,21.102387855306,-12.9682428555774));
#93986=CARTESIAN_POINT('Ctrl Pts',(19.6881839569367,21.1007711201164,-12.9684600645359));
#93987=CARTESIAN_POINT('Ctrl Pts',(19.694959044111,21.0973357975639,-12.9689203898002));
#93988=CARTESIAN_POINT('Ctrl Pts',(19.6985243123295,21.0955152893888,-12.9691636209902));
#93989=CARTESIAN_POINT('Ctrl Pts',(19.7080948748259,21.0905940660458,-12.9698191778722));
#93990=CARTESIAN_POINT('Ctrl Pts',(19.714090460338,21.0874747173837,-12.970232651474));
#93991=CARTESIAN_POINT('Ctrl Pts',(19.7432955114369,21.0721019314086,-12.9722600090599));
#93992=CARTESIAN_POINT('Ctrl Pts',(19.7662895574433,21.0594469025525,-12.9738973382631));
#93993=CARTESIAN_POINT('Ctrl Pts',(19.8314788515691,21.0219735606818,-12.9786454989434));
#93994=CARTESIAN_POINT('Ctrl Pts',(19.873055014891,20.996115712638,-12.9818039056192));
#93995=CARTESIAN_POINT('Ctrl Pts',(19.9939452209303,20.9149858227036,-12.9913043555429));
#93996=CARTESIAN_POINT('Ctrl Pts',(20.0704124407586,20.8556979152358,-12.9977331918203));
#93997=CARTESIAN_POINT('Ctrl Pts',(20.2478329620457,20.6975679354631,-13.0133686048274));
#93998=CARTESIAN_POINT('Ctrl Pts',(20.3434829207567,20.5934444083241,-13.0224360965622));
#93999=CARTESIAN_POINT('Ctrl Pts',(20.436643474715,20.4691328175676,-13.0319214066967));
#94000=CARTESIAN_POINT('Ctrl Pts',(20.445092924387,20.4576170255684,-13.032788958786));
#94001=CARTESIAN_POINT('Ctrl Pts',(20.4583563850384,20.4391512538863,-13.0341627251219));
#94002=CARTESIAN_POINT('Ctrl Pts',(20.4632463132491,20.4322565809021,-13.0346718638424));
#94003=CARTESIAN_POINT('Ctrl Pts',(20.4717983248134,20.4200441130374,-13.0355671002427));
#94004=CARTESIAN_POINT('Ctrl Pts',(20.4754775950576,20.414738539858,-13.0359538533955));
#94005=CARTESIAN_POINT('Ctrl Pts',(20.4830379611024,20.403729141521,-13.0367519493366));
#94006=CARTESIAN_POINT('Ctrl Pts',(20.4869155667619,20.3980230039669,-13.0371631564015));
#94007=CARTESIAN_POINT('Ctrl Pts',(20.4967985977,20.3833254713842,-13.0382161312676));
#94008=CARTESIAN_POINT('Ctrl Pts',(20.5027632050298,20.3743067686587,-13.0388563562433));
#94009=CARTESIAN_POINT('Ctrl Pts',(20.5273801315396,20.3364580204881,-13.0415191231348));
#94010=CARTESIAN_POINT('Ctrl Pts',(20.5453993509157,20.3072210729232,-13.0435180888477));
#94011=CARTESIAN_POINT('Ctrl Pts',(20.5904982511446,20.2298953114509,-13.0486679704026));
#94012=CARTESIAN_POINT('Ctrl Pts',(20.6164236518648,20.1811624887711,-13.0517793805904));
#94013=CARTESIAN_POINT('Ctrl Pts',(20.6879861440396,20.0329468982281,-13.0609305093062));
#94014=CARTESIAN_POINT('Ctrl Pts',(20.7278477889549,19.9308822305411,-13.0668215209849));
#94015=CARTESIAN_POINT('Ctrl Pts',(20.7744321528768,19.7774945257218,-13.0755495348637));
#94016=CARTESIAN_POINT('Ctrl Pts',(20.7874609051876,19.7282788220588,-13.078333815612));
#94017=CARTESIAN_POINT('Ctrl Pts',(20.802178873281,19.6632971740539,-13.0820406762741));
#94018=CARTESIAN_POINT('Ctrl Pts',(20.8054834256903,19.6479130178728,-13.0829205093056));
#94019=CARTESIAN_POINT('Ctrl Pts',(20.8191178887894,19.5808034153836,-13.0867736962881));
#94020=CARTESIAN_POINT('Ctrl Pts',(20.827683232228,19.5287431522477,-13.0898016468224));
#94021=CARTESIAN_POINT('Ctrl Pts',(20.8353850230393,19.4677986381042,-13.0934472438762));
#94022=CARTESIAN_POINT('Ctrl Pts',(20.8364216868069,19.4591684922929,-13.0939658298833));
#94023=CARTESIAN_POINT('Ctrl Pts',(20.8379117366798,19.4460839204166,-13.0947559640095));
#94024=CARTESIAN_POINT('Ctrl Pts',(20.8384042009665,19.4416339165982,-13.0950253643043));
#94025=CARTESIAN_POINT('Ctrl Pts',(20.8392632774401,19.4336392414121,-13.0955106296755));
#94026=CARTESIAN_POINT('Ctrl Pts',(20.8396350588344,19.4300951799123,-13.0957262006997));
#94027=CARTESIAN_POINT('Ctrl Pts',(20.8404239568601,19.4223873794548,-13.0961960282573));
#94028=CARTESIAN_POINT('Ctrl Pts',(20.8408376718472,19.4182233915687,-13.0964504677323));
#94029=CARTESIAN_POINT('Ctrl Pts',(20.8419662927639,19.4065111164214,-13.0971678461313));
#94030=CARTESIAN_POINT('Ctrl Pts',(20.8426529878326,19.3989602643751,-13.0976323242002));
#94031=CARTESIAN_POINT('Ctrl Pts',(20.8465378407345,19.3535387381931,-13.1004376346023));
#94032=CARTESIAN_POINT('Ctrl Pts',(20.8487560505634,19.3155937455552,-13.1028282215272));
#94033=CARTESIAN_POINT('Ctrl Pts',(20.8527120529054,19.1899309861176,-13.1108564233111));
#94034=CARTESIAN_POINT('Ctrl Pts',(20.8500194568677,19.1021680664631,-13.1166390251248));
#94035=CARTESIAN_POINT('Ctrl Pts',(20.8257290893626,18.8411604580203,-13.1339593777633));
#94036=CARTESIAN_POINT('Ctrl Pts',(20.7881616451049,18.6701165934674,-13.1454065260778));
#94037=CARTESIAN_POINT('Ctrl Pts',(20.7223354003542,18.4838525800512,-13.1575671972136));
#94038=CARTESIAN_POINT('Ctrl Pts',(20.7142945415091,18.4622312576192,-13.1589753569944));
#94039=CARTESIAN_POINT('Ctrl Pts',(20.7024239027215,18.4318416702177,-13.1609503877165));
#94040=CARTESIAN_POINT('Ctrl Pts',(20.6988858334063,18.4229619107927,-13.1615269784075));
#94041=CARTESIAN_POINT('Ctrl Pts',(20.693040799752,18.4085763125025,-13.1624603359689));
#94042=CARTESIAN_POINT('Ctrl Pts',(20.6907705052105,18.4030558061212,-13.1628183350449));
#94043=CARTESIAN_POINT('Ctrl Pts',(20.6859705826036,18.3915231006353,-13.1635658736304));
#94044=CARTESIAN_POINT('Ctrl Pts',(20.68343645292,18.3855128338747,-13.1639552557864));
#94045=CARTESIAN_POINT('Ctrl Pts',(20.6773439865215,18.3712476839298,-13.1648790189078));
#94046=CARTESIAN_POINT('Ctrl Pts',(20.6737607526023,18.3630035207892,-13.1654125457858));
#94047=CARTESIAN_POINT('Ctrl Pts',(20.6615229545414,18.3353307588443,-13.1672024723544));
#94048=CARTESIAN_POINT('Ctrl Pts',(20.6526279692529,18.3160094277984,-13.1684506363171));
#94049=CARTESIAN_POINT('Ctrl Pts',(20.576743556568,18.1575091963893,-13.1786846154419));
#94050=CARTESIAN_POINT('Ctrl Pts',(20.4949970992559,18.0259078674962,-13.1871019308589));
#94051=CARTESIAN_POINT('Ctrl Pts',(20.3152304177142,17.7967489626181,-13.2029186321855));
#94052=CARTESIAN_POINT('Ctrl Pts',(20.2205943327123,17.6975858008316,-13.2103042190342));
#94053=CARTESIAN_POINT('Ctrl Pts',(20.1052749072516,17.5980718968109,-13.2192364117658));
#94054=CARTESIAN_POINT('Ctrl Pts',(20.0933629586772,17.5880199471401,-13.2201585175607));
#94055=CARTESIAN_POINT('Ctrl Pts',(20.0768874423479,17.5744256318437,-13.2214348710614));
#94056=CARTESIAN_POINT('Ctrl Pts',(20.0724184242064,17.570768776883,-13.2217811820341));
#94057=CARTESIAN_POINT('Ctrl Pts',(20.0652882038302,17.5649828880212,-13.2223339698506));
#94058=CARTESIAN_POINT('Ctrl Pts',(20.0626366872115,17.5628418863469,-13.2225395911249));
#94059=CARTESIAN_POINT('Ctrl Pts',(20.0571456049062,17.5584299019976,-13.2229655592243));
#94060=CARTESIAN_POINT('Ctrl Pts',(20.0543053626281,17.5561598357449,-13.2231859712692));
#94061=CARTESIAN_POINT('Ctrl Pts',(20.0475167446075,17.5507626282338,-13.2237129598209));
#94062=CARTESIAN_POINT('Ctrl Pts',(20.043563041487,17.5476422489008,-13.2240200139323));
#94063=CARTESIAN_POINT('Ctrl Pts',(20.0301588921483,17.5371407109705,-13.2250613581153));
#94064=CARTESIAN_POINT('Ctrl Pts',(20.0206570807284,17.5298259059479,-13.2258001140365));
#94065=CARTESIAN_POINT('Ctrl Pts',(19.9093813361156,17.4456580927729,-13.2344533314345));
#94066=CARTESIAN_POINT('Ctrl Pts',(19.8009353596003,17.3780800536971,-13.2428867790967));
#94067=CARTESIAN_POINT('Ctrl Pts',(19.5396983782028,17.246366908696,-13.2622205408024));
#94068=CARTESIAN_POINT('Ctrl Pts',(19.384101406228,17.1895349610642,-13.2730158708654));
#94069=CARTESIAN_POINT('Ctrl Pts',(19.2004915747925,17.1459014922146,-13.2846391282991));
#94070=CARTESIAN_POINT('Ctrl Pts',(19.1774349445044,17.1408280851586,-13.2860807526524));
#94071=CARTESIAN_POINT('Ctrl Pts',(19.1448415465023,17.1342257445272,-13.2880942056105));
#94072=CARTESIAN_POINT('Ctrl Pts',(19.1353724653406,17.1323749175442,-13.2886762707289));
#94073=CARTESIAN_POINT('Ctrl Pts',(19.1200089926158,17.129480871443,-13.2896160792048));
#94074=CARTESIAN_POINT('Ctrl Pts',(19.1141223285347,17.1283978196924,-13.2899750885476));
#94075=CARTESIAN_POINT('Ctrl Pts',(19.1018246015711,17.1261891141695,-13.2907228505603));
#94076=CARTESIAN_POINT('Ctrl Pts',(19.0954127732787,17.1250680317975,-13.2911114541395));
#94077=CARTESIAN_POINT('Ctrl Pts',(19.0802087078043,17.1224818703207,-13.2920299803864));
#94078=CARTESIAN_POINT('Ctrl Pts',(19.0714121427314,17.1210427045038,-13.2925590751139));
#94079=CARTESIAN_POINT('Ctrl Pts',(19.0426191470949,17.1165185402009,-13.2942834805689));
#94080=CARTESIAN_POINT('Ctrl Pts',(19.0225871647994,17.113664582481,-13.2954714796688));
#94081=CARTESIAN_POINT('Ctrl Pts',(18.9749213752585,17.1075695041379,-13.2982724952258));
#94082=CARTESIAN_POINT('Ctrl Pts',(18.9472582218675,17.1045850382485,-13.2998775526848));
#94083=CARTESIAN_POINT('Ctrl Pts',(18.7508359254928,17.0873032062144,-13.3111481900545));
#94084=CARTESIAN_POINT('Ctrl Pts',(18.5809622467596,17.0927569562635,-13.3201753502847));
#94085=CARTESIAN_POINT('Ctrl Pts',(18.3107907901892,17.1341299011228,-13.3351122077079));
#94086=CARTESIAN_POINT('Ctrl Pts',(18.2093464381105,17.1574108875477,-13.3408765536017));
#94087=CARTESIAN_POINT('Ctrl Pts',(18.1007796311637,17.1908973247029,-13.3476075900357));
#94088=CARTESIAN_POINT('Ctrl Pts',(18.0915420544373,17.1938161624729,-13.3481849022349));
#94089=CARTESIAN_POINT('Ctrl Pts',(18.0779311500703,17.1982198353205,-13.3490427707239));
#94090=CARTESIAN_POINT('Ctrl Pts',(18.0735419752895,17.1996557918038,-13.3493205285213));
#94091=CARTESIAN_POINT('Ctrl Pts',(18.0657629029168,17.2022289909374,-13.3498148489441));
#94092=CARTESIAN_POINT('Ctrl Pts',(18.0623711510381,17.2033604721463,-13.3500310700607));
#94093=CARTESIAN_POINT('Ctrl Pts',(18.0551094864893,17.205803409574,-13.3504954971452));
#94094=CARTESIAN_POINT('Ctrl Pts',(18.0512405577055,17.2071174588076,-13.3507438496981));
#94095=CARTESIAN_POINT('Ctrl Pts',(18.0406289265565,17.2107559094706,-13.3514274834749));
#94096=CARTESIAN_POINT('Ctrl Pts',(18.0338942007325,17.2131031724135,-13.3518640841223));
#94097=CARTESIAN_POINT('Ctrl Pts',(17.9984774581856,17.2256480806605,-13.3541740085612));
#94098=CARTESIAN_POINT('Ctrl Pts',(17.9700075820052,17.2364289034281,-13.3560790349566));
#94099=CARTESIAN_POINT('Ctrl Pts',(17.7914208948333,17.3084954257281,-13.3682924678814));
#94100=CARTESIAN_POINT('Ctrl Pts',(17.6485332974991,17.3862423988859,-13.3792084614568));
#94101=CARTESIAN_POINT('Ctrl Pts',(17.4180928270384,17.5483562544187,-13.3976307189773));
#94102=CARTESIAN_POINT('Ctrl Pts',(17.3262603589321,17.6253539589863,-13.405258330257));
#94103=CARTESIAN_POINT('Ctrl Pts',(17.2302711969332,17.7207867640229,-13.4135235169064));
#94104=CARTESIAN_POINT('Ctrl Pts',(17.2192537711696,17.7319869219712,-13.4144773235938));
#94105=CARTESIAN_POINT('Ctrl Pts',(17.2027731932283,17.7491181832114,-13.4159122515394));
#94106=CARTESIAN_POINT('Ctrl Pts',(17.1972177505116,17.7549593753963,-13.416397389438));
#94107=CARTESIAN_POINT('Ctrl Pts',(17.1873222617206,17.7654835745059,-13.4172641789679));
#94108=CARTESIAN_POINT('Ctrl Pts',(17.1829698046096,17.7701547283509,-13.4176463632809));
#94109=CARTESIAN_POINT('Ctrl Pts',(17.1737790452115,17.7801083605335,-13.4184554225023));
#94110=CARTESIAN_POINT('Ctrl Pts',(17.168946279506,17.7853958594475,-13.4188820586169));
#94111=CARTESIAN_POINT('Ctrl Pts',(17.1591628934814,17.7962095095405,-13.4197482692234));
#94112=CARTESIAN_POINT('Ctrl Pts',(17.1542142974444,17.8017373629848,-13.4201877554741));
#94113=CARTESIAN_POINT('Ctrl Pts',(17.1324256418596,17.8263354810243,-13.4221289502548));
#94114=CARTESIAN_POINT('Ctrl Pts',(17.1159006354143,17.8456829001378,-13.4236175525859));
#94115=CARTESIAN_POINT('Ctrl Pts',(17.0457285954405,17.930904173027,-13.4300186729676));
#94116=CARTESIAN_POINT('Ctrl Pts',(16.9957224712622,17.9996787795795,-13.4347858967342));
#94117=CARTESIAN_POINT('Ctrl Pts',(16.9128101383288,18.1294624461232,-13.4432735431789));
#94118=CARTESIAN_POINT('Ctrl Pts',(16.8785074211341,18.1894307972629,-13.4470186741641));
#94119=CARTESIAN_POINT('Ctrl Pts',(16.8085769124412,18.3268692270204,-13.4553932840246));
#94120=CARTESIAN_POINT('Ctrl Pts',(16.7745951535261,18.4049867853306,-13.4600145404506));
#94121=CARTESIAN_POINT('Ctrl Pts',(16.7454194857027,18.4848894449486,-13.4647888259555));
#94122=CARTESIAN_POINT('',(16.6170008459317,19.2091074688849,-12.4890563034237));
#94123=CARTESIAN_POINT('Ctrl Pts',(16.7454194503191,18.4848895418526,-13.2445592875761));
#94124=CARTESIAN_POINT('Ctrl Pts',(16.771739242225,18.4128081860915,-13.2399327109632));
#94125=CARTESIAN_POINT('Ctrl Pts',(16.8019456372607,18.3422595341822,-13.2353061343503));
#94126=CARTESIAN_POINT('Ctrl Pts',(16.8358258585856,18.2736505833652,-13.2306795577375));
#94127=CARTESIAN_POINT('Ctrl Pts',(16.8465556085575,18.251922363793,-13.2292143367814));
#94128=CARTESIAN_POINT('Ctrl Pts',(16.8576534980229,18.23038848217,-13.2277491158253));
#94129=CARTESIAN_POINT('Ctrl Pts',(16.869111861991,18.209061262994,-13.2262838948692));
#94130=CARTESIAN_POINT('Ctrl Pts',(16.9034286623953,18.145188102246,-13.2218956859383));
#94131=CARTESIAN_POINT('Ctrl Pts',(16.9410977666971,18.0829553476818,-13.2175074770074));
#94132=CARTESIAN_POINT('Ctrl Pts',(16.9819381659419,18.0227372640544,-13.2131192680765));
#94133=CARTESIAN_POINT('Ctrl Pts',(17.0227179512629,17.9626085540473,-13.2087375719752));
#94134=CARTESIAN_POINT('Ctrl Pts',(17.0666594195119,17.9044889751322,-13.2043558758739));
#94135=CARTESIAN_POINT('Ctrl Pts',(17.1135357879725,17.8487280970606,-13.1999741797727));
#94136=CARTESIAN_POINT('Ctrl Pts',(17.1603570729695,17.7930327424584,-13.195597632513));
#94137=CARTESIAN_POINT('Ctrl Pts',(17.2101060983657,17.7396909501816,-13.1912210852534));
#94138=CARTESIAN_POINT('Ctrl Pts',(17.2625139124407,17.6890217826396,-13.1868445379937));
#94139=CARTESIAN_POINT('Ctrl Pts',(17.3148884902417,17.6383847487473,-13.1824707662767));
#94140=CARTESIAN_POINT('Ctrl Pts',(17.3699181652077,17.5904173110759,-13.1780969945597));
#94141=CARTESIAN_POINT('Ctrl Pts',(17.4272959551564,17.5454029481326,-13.1737232228428));
#94142=CARTESIAN_POINT('Ctrl Pts',(17.484656284851,17.500402283211,-13.1693507820792));
#94143=CARTESIAN_POINT('Ctrl Pts',(17.5443629316542,17.4583532065242,-13.1649783413156));
#94144=CARTESIAN_POINT('Ctrl Pts',(17.606075834685,17.4194989318177,-13.1606059005521));
#94145=CARTESIAN_POINT('Ctrl Pts',(17.6677903157216,17.380643663603,-13.1562333479847));
#94146=CARTESIAN_POINT('Ctrl Pts',(17.7315107455623,17.3449836148749,-13.1518607954174));
#94147=CARTESIAN_POINT('Ctrl Pts',(17.7968695201159,17.3127177597438,-13.14748824285));
#94148=CARTESIAN_POINT('Ctrl Pts',(17.862296126471,17.2804184178912,-13.1431111522827));
#94149=CARTESIAN_POINT('Ctrl Pts',(17.929364038908,17.2515205167786,-13.1387340617153));
#94150=CARTESIAN_POINT('Ctrl Pts',(17.9976833250416,17.2261758883523,-13.134356971148));
#94151=CARTESIAN_POINT('Ctrl Pts',(18.0660399228729,17.2008174182837,-13.1299774900891));
#94152=CARTESIAN_POINT('Ctrl Pts',(18.1356487944388,17.179016228838,-13.1255980090301));
#94153=CARTESIAN_POINT('Ctrl Pts',(18.2061050046754,17.1608741809559,-13.1212185279712));
#94154=CARTESIAN_POINT('Ctrl Pts',(18.2766860980717,17.1426999764157,-13.1168312843114));
#94155=CARTESIAN_POINT('Ctrl Pts',(18.3481170562262,17.1281979613854,-13.1124440406517));
#94156=CARTESIAN_POINT('Ctrl Pts',(18.4199835016944,17.1174187049957,-13.108056796992));
#94157=CARTESIAN_POINT('Ctrl Pts',(18.4688457595774,17.1100898493375,-13.1050738940572));
#94158=CARTESIAN_POINT('Ctrl Pts',(18.5179091821644,17.1044808253816,-13.1020909911225));
#94159=CARTESIAN_POINT('Ctrl Pts',(18.567043338876,17.1005937658104,-13.0991080881877));
#94160=CARTESIAN_POINT('Ctrl Pts',(18.6393255921075,17.0948754337364,-13.0947198792568));
#94161=CARTESIAN_POINT('Ctrl Pts',(18.7120430618564,17.0928637794812,-13.0903316703259));
#94162=CARTESIAN_POINT('Ctrl Pts',(18.7847830739805,17.0946091855716,-13.085943461395));
#94163=CARTESIAN_POINT('Ctrl Pts',(18.8574151278661,17.0963520011899,-13.0815617652938));
#94164=CARTESIAN_POINT('Ctrl Pts',(18.9300691794581,17.1018407963575,-13.0771800691925));
#94165=CARTESIAN_POINT('Ctrl Pts',(19.0023285427329,17.1110740981752,-13.0727983730912));
#94166=CARTESIAN_POINT('Ctrl Pts',(19.0745029955053,17.1202965501284,-13.0684218258316));
#94167=CARTESIAN_POINT('Ctrl Pts',(19.1462832051704,17.1332547070803,-13.0640452785719));
#94168=CARTESIAN_POINT('Ctrl Pts',(19.2172553122695,17.1498951256272,-13.0596687313123));
#94169=CARTESIAN_POINT('Ctrl Pts',(19.2881824098898,17.1665249910625,-13.0552949595953));
#94170=CARTESIAN_POINT('Ctrl Pts',(19.3583019532985,17.1868323748369,-13.0509211878784));
#94171=CARTESIAN_POINT('Ctrl Pts',(19.4272094182998,17.2107125950553,-13.0465474161614));
#94172=CARTESIAN_POINT('Ctrl Pts',(19.4960959145281,17.2345855484424,-13.0421749753978));
#94173=CARTESIAN_POINT('Ctrl Pts',(19.5637706090995,17.2620290219354,-13.0378025346343));
#94174=CARTESIAN_POINT('Ctrl Pts',(19.6298449292381,17.2928887251365,-13.0334300938707));
#94175=CARTESIAN_POINT('Ctrl Pts',(19.6959209389044,17.3237492174237,-13.0290575413034));
#94176=CARTESIAN_POINT('Ctrl Pts',(19.7603960566788,17.3580259069127,-13.024684988736));
#94177=CARTESIAN_POINT('Ctrl Pts',(19.8229039997004,17.3955173976497,-13.0203124361687));
#94178=CARTESIAN_POINT('Ctrl Pts',(19.885476815823,17.43304779847,-13.0159353456014));
#94179=CARTESIAN_POINT('Ctrl Pts',(19.9460779664252,17.473799413322,-13.011558255034));
#94180=CARTESIAN_POINT('Ctrl Pts',(20.0043687218637,17.5175265545305,-13.0071811644667));
#94181=CARTESIAN_POINT('Ctrl Pts',(20.0626913120471,17.5612775767537,-13.0028016834078));
#94182=CARTESIAN_POINT('Ctrl Pts',(20.1187006241998,17.608007051543,-12.9984222023488));
#94183=CARTESIAN_POINT('Ctrl Pts',(20.1720918257207,17.6574296279874,-12.9940427212899));
#94184=CARTESIAN_POINT('Ctrl Pts',(20.2255776627878,17.7069398056168,-12.9896554776302));
#94185=CARTESIAN_POINT('Ctrl Pts',(20.2764357852884,17.759152271547,-12.9852682339705));
#94186=CARTESIAN_POINT('Ctrl Pts',(20.3243993779349,17.813745972035,-12.9808809903107));
#94187=CARTESIAN_POINT('Ctrl Pts',(20.3570099991736,17.8508644277303,-12.9778980873759));
#94188=CARTESIAN_POINT('Ctrl Pts',(20.3882834007588,17.8890829433879,-12.9749151844411));
#94189=CARTESIAN_POINT('Ctrl Pts',(20.4181471898432,17.9282930019123,-12.9719322815063));
#94190=CARTESIAN_POINT('Ctrl Pts',(20.4620804149045,17.9859757132704,-12.9675440725754));
#94191=CARTESIAN_POINT('Ctrl Pts',(20.5031324849612,18.0460307272458,-12.9631558636445));
#94192=CARTESIAN_POINT('Ctrl Pts',(20.541037663595,18.1081383212981,-12.9587676547136));
#94193=CARTESIAN_POINT('Ctrl Pts',(20.5788865846589,18.1701537373831,-12.9543859586124));
#94194=CARTESIAN_POINT('Ctrl Pts',(20.6135976366773,18.23421527774,-12.9500042625111));
#94195=CARTESIAN_POINT('Ctrl Pts',(20.6449465138837,18.2999717781125,-12.9456225664098));
#94196=CARTESIAN_POINT('Ctrl Pts',(20.6762585536647,18.3656510093639,-12.9412460191502));
#94197=CARTESIAN_POINT('Ctrl Pts',(20.7042160604133,18.4330208108149,-12.9368694718905));
#94198=CARTESIAN_POINT('Ctrl Pts',(20.728639957299,18.5017042642547,-12.9324929246309));
#94199=CARTESIAN_POINT('Ctrl Pts',(20.7530483649042,18.5703441596466,-12.9281191529139));
#94200=CARTESIAN_POINT('Ctrl Pts',(20.7739274477879,18.640295600672,-12.923745381197));
#94201=CARTESIAN_POINT('Ctrl Pts',(20.7911462655828,18.7111617841753,-12.91937160948));
#94202=CARTESIAN_POINT('Ctrl Pts',(20.8083598436336,18.782006402861,-12.9149991687164));
#94203=CARTESIAN_POINT('Ctrl Pts',(20.8219152540693,18.853764742938,-12.9106267279529));
#94204=CARTESIAN_POINT('Ctrl Pts',(20.8317319036235,18.9260265617289,-12.9062542871893));
#94205=CARTESIAN_POINT('Ctrl Pts',(20.8415488041905,18.9982902282625,-12.901881734622));
#94206=CARTESIAN_POINT('Ctrl Pts',(20.847626691118,19.0710569208137,-12.8975091820546));
#94207=CARTESIAN_POINT('Ctrl Pts',(20.8499366445659,19.143909641652,-12.8931366294873));
#94208=CARTESIAN_POINT('Ctrl Pts',(20.8522489953706,19.2168379717919,-12.88875953892));
#94209=CARTESIAN_POINT('Ctrl Pts',(20.8507855897922,19.2898520253122,-12.8843824483526));
#94210=CARTESIAN_POINT('Ctrl Pts',(20.8455696643533,19.3625339981092,-12.8800053577853));
#94211=CARTESIAN_POINT('Ctrl Pts',(20.8403508903039,19.4352556652291,-12.8756258767264));
#94212=CARTESIAN_POINT('Ctrl Pts',(20.8313755754734,19.5076444114925,-12.8712463956674));
#94213=CARTESIAN_POINT('Ctrl Pts',(20.818718654715,19.5792894658868,-12.8668669146085));
#94214=CARTESIAN_POINT('Ctrl Pts',(20.8060392996495,19.6510615106591,-12.8624796709487));
#94215=CARTESIAN_POINT('Ctrl Pts',(20.7896654157131,19.72208676073,-12.858092427289));
#94216=CARTESIAN_POINT('Ctrl Pts',(20.7697225362412,19.7919670863653,-12.8537051836293));
#94217=CARTESIAN_POINT('Ctrl Pts',(20.7561632998915,19.8394789741454,-12.8507222806945));
#94218=CARTESIAN_POINT('Ctrl Pts',(20.7409552755656,19.8864619134098,-12.8477393777596));
#94219=CARTESIAN_POINT('Ctrl Pts',(20.7241505240926,19.9327962949848,-12.8447564748248));
#94220=CARTESIAN_POINT('Ctrl Pts',(20.6994287137936,20.0009597422968,-12.8403682658939));
#94221=CARTESIAN_POINT('Ctrl Pts',(20.6711526578598,20.0679846766149,-12.835980056963));
#94222=CARTESIAN_POINT('Ctrl Pts',(20.6394473542676,20.1334745959182,-12.8315918480321));
#94223=CARTESIAN_POINT('Ctrl Pts',(20.6077891066028,20.1988673173228,-12.8272101519309));
#94224=CARTESIAN_POINT('Ctrl Pts',(20.5727119232316,20.2627291156992,-12.8228284558296));
#94225=CARTESIAN_POINT('Ctrl Pts',(20.5343896652635,20.3246813068434,-12.8184467597283));
#94226=CARTESIAN_POINT('Ctrl Pts',(20.4961124389983,20.3865606992326,-12.8140702124687));
#94227=CARTESIAN_POINT('Ctrl Pts',(20.4545979656272,20.4465345337929,-12.8096936652091));
#94228=CARTESIAN_POINT('Ctrl Pts',(20.4100662428249,20.5042482165705,-12.8053171179494));
#94229=CARTESIAN_POINT('Ctrl Pts',(20.3655627613939,20.5619252981693,-12.8009433462325));
#94230=CARTESIAN_POINT('Ctrl Pts',(20.3180461211089,20.617344690981,-12.7965695745155));
#94231=CARTESIAN_POINT('Ctrl Pts',(20.2677790950909,20.6701815128564,-12.7921958027985));
#94232=CARTESIAN_POINT('Ctrl Pts',(20.2175273654978,20.7230022563095,-12.787823362035));
#94233=CARTESIAN_POINT('Ctrl Pts',(20.1645272440668,20.7732416397748,-12.7834509212714));
#94234=CARTESIAN_POINT('Ctrl Pts',(20.1090800563606,20.8206098404891,-12.7790784805079));
#94235=CARTESIAN_POINT('Ctrl Pts',(20.0536314508637,20.8679792524136,-12.7747059279405));
#94236=CARTESIAN_POINT('Ctrl Pts',(19.9957360229244,20.9124770240216,-12.7703333753732));
#94237=CARTESIAN_POINT('Ctrl Pts',(19.9357287478821,20.9538531253418,-12.7659608228058));
#94238=CARTESIAN_POINT('Ctrl Pts',(19.8756591950264,20.9952721683406,-12.7615837322385));
#94239=CARTESIAN_POINT('Ctrl Pts',(19.8134738170563,21.0335627981877,-12.7572066416712));
#94240=CARTESIAN_POINT('Ctrl Pts',(19.7495364985934,21.068518403684,-12.7528295511039));
#94241=CARTESIAN_POINT('Ctrl Pts',(19.6855642615878,21.1034930997338,-12.7484500700449));
#94242=CARTESIAN_POINT('Ctrl Pts',(19.6198386140603,21.135128935727,-12.744070588986));
#94243=CARTESIAN_POINT('Ctrl Pts',(19.5527455102414,21.163266577458,-12.7396911079271));
#94244=CARTESIAN_POINT('Ctrl Pts',(19.4855334843463,21.1914540929701,-12.7353038642673));
#94245=CARTESIAN_POINT('Ctrl Pts',(19.4169496162067,21.2161308685659,-12.7309166206076));
#94246=CARTESIAN_POINT('Ctrl Pts',(19.3473966187371,21.2371869578402,-12.7265293769479));
#94247=CARTESIAN_POINT('Ctrl Pts',(19.3001072825686,21.2515030695869,-12.7235464740131));
#94248=CARTESIAN_POINT('Ctrl Pts',(19.2523702507341,21.2641465017728,-12.7205635710783));
#94249=CARTESIAN_POINT('Ctrl Pts',(19.2043142751595,21.2750962871391,-12.7175806681434));
#94250=CARTESIAN_POINT('Ctrl Pts',(19.1336181560408,21.2912047381968,-12.7131924592126));
#94251=CARTESIAN_POINT('Ctrl Pts',(19.0619555004259,21.3037083756574,-12.7088042502817));
#94252=CARTESIAN_POINT('Ctrl Pts',(18.9897273628005,21.3124976840137,-12.7044160413508));
#94253=CARTESIAN_POINT('Ctrl Pts',(18.9176064237069,21.3212739475792,-12.7000343452495));
#94254=CARTESIAN_POINT('Ctrl Pts',(18.8449221435536,21.3263467676749,-12.6956526491482));
#94255=CARTESIAN_POINT('Ctrl Pts',(18.7720870435491,21.3276573594027,-12.691270953047));
#94256=CARTESIAN_POINT('Ctrl Pts',(18.6993375305835,21.3289664110809,-12.6868944057873));
#94257=CARTESIAN_POINT('Ctrl Pts',(18.6264380297318,21.3265220079374,-12.6825178585277));
#94258=CARTESIAN_POINT('Ctrl Pts',(18.5538057789622,21.3203171982195,-12.6781413112681));
#94259=CARTESIAN_POINT('Ctrl Pts',(18.4812195905104,21.3141163235017,-12.6737675395511));
#94260=CARTESIAN_POINT('Ctrl Pts',(18.4089007953028,21.3041598149104,-12.6693937678341));
#94261=CARTESIAN_POINT('Ctrl Pts',(18.33726480192,21.2904927705103,-12.6650199961171));
#94262=CARTESIAN_POINT('Ctrl Pts',(18.2656506076105,21.2768298850376,-12.6606475553536));
#94263=CARTESIAN_POINT('Ctrl Pts',(18.1947192761672,21.2594587957696,-12.65627511459));
#94264=CARTESIAN_POINT('Ctrl Pts',(18.1248776044805,21.2384759942541,-12.6519026738265));
#94265=CARTESIAN_POINT('Ctrl Pts',(18.0550341469344,21.217492656206,-12.6475301212591));
#94266=CARTESIAN_POINT('Ctrl Pts',(17.9862808658672,21.1928975632636,-12.6431575686918));
#94267=CARTESIAN_POINT('Ctrl Pts',(17.9190093127144,21.1648370401949,-12.6387850161244));
#94268=CARTESIAN_POINT('Ctrl Pts',(17.8516679426063,21.136747394857,-12.6344079255571));
#94269=CARTESIAN_POINT('Ctrl Pts',(17.7858118168723,21.1051853247306,-12.6300308349898));
#94270=CARTESIAN_POINT('Ctrl Pts',(17.7218116266776,21.0703449644729,-12.6256537444225));
#94271=CARTESIAN_POINT('Ctrl Pts',(17.6577764836036,21.0354855766014,-12.6212742633635));
#94272=CARTESIAN_POINT('Ctrl Pts',(17.5955997055918,20.9973445863421,-12.6168947823046));
#94273=CARTESIAN_POINT('Ctrl Pts',(17.5356241771986,20.9561602755406,-12.6125153012456));
#94274=CARTESIAN_POINT('Ctrl Pts',(17.4755423425838,20.9149029658247,-12.6081280575859));
#94275=CARTESIAN_POINT('Ctrl Pts',(17.4176699324641,20.8705918569496,-12.6037408139262));
#94276=CARTESIAN_POINT('Ctrl Pts',(17.3623173752294,20.8235060548421,-12.5993535702665));
#94277=CARTESIAN_POINT('Ctrl Pts',(17.3246829700695,20.791492246586,-12.5963706673317));
#94278=CARTESIAN_POINT('Ctrl Pts',(17.2882126945401,20.7581966074029,-12.5933877643968));
#94279=CARTESIAN_POINT('Ctrl Pts',(17.2529938697633,20.7237160481073,-12.590404861462));
#94280=CARTESIAN_POINT('Ctrl Pts',(17.2019441492121,20.6737364440846,-12.5860811407752));
#94281=CARTESIAN_POINT('Ctrl Pts',(17.1533139178897,20.6210584681426,-12.5817574200883));
#94282=CARTESIAN_POINT('Ctrl Pts',(17.1074080252022,20.5659492785796,-12.5774336994015));
#94283=CARTESIAN_POINT('Ctrl Pts',(17.0615630887849,20.5109132659108,-12.5731157199794));
#94284=CARTESIAN_POINT('Ctrl Pts',(17.0184356374497,20.453452815078,-12.5687977405574));
#94285=CARTESIAN_POINT('Ctrl Pts',(16.9782947055965,20.3938727400712,-12.5644797611354));
#94286=CARTESIAN_POINT('Ctrl Pts',(16.9381929308677,20.3343507849011,-12.5601659938641));
#94287=CARTESIAN_POINT('Ctrl Pts',(16.9010721765565,20.2727137148021,-12.5558522265928));
#94288=CARTESIAN_POINT('Ctrl Pts',(16.867160867601,20.2092988799672,-12.5515384593216));
#94289=CARTESIAN_POINT('Ctrl Pts',(16.8332706976893,20.1459235755725,-12.5472273810917));
#94290=CARTESIAN_POINT('Ctrl Pts',(16.8025862384803,20.0807731423996,-12.5429163028619));
#94291=CARTESIAN_POINT('Ctrl Pts',(16.7752912625975,20.0142117292613,-12.5386052246321));
#94292=CARTESIAN_POINT('Ctrl Pts',(16.7479923079759,19.9476406135874,-12.5342935179843));
#94293=CARTESIAN_POINT('Ctrl Pts',(16.7240840285397,19.8796585609645,-12.5299818113365));
#94294=CARTESIAN_POINT('Ctrl Pts',(16.7037024934053,19.8106507606227,-12.5256701046887));
#94295=CARTESIAN_POINT('Ctrl Pts',(16.6833204782337,19.7416413349709,-12.5213582964891));
#94296=CARTESIAN_POINT('Ctrl Pts',(16.6664655033664,19.6716065941827,-12.5170464882896));
#94297=CARTESIAN_POINT('Ctrl Pts',(16.6532233605847,19.6009456075705,-12.5127346800901));
#94298=CARTESIAN_POINT('Ctrl Pts',(16.6399664562209,19.5302058521387,-12.5084180653338));
#94299=CARTESIAN_POINT('Ctrl Pts',(16.630330506581,19.4588389489556,-12.5041014505775));
#94300=CARTESIAN_POINT('Ctrl Pts',(16.6243497245844,19.387251852299,-12.4997848358212));
#94301=CARTESIAN_POINT('Ctrl Pts',(16.6193948377084,19.3279442289965,-12.4962086583554));
#94302=CARTESIAN_POINT('Ctrl Pts',(16.6169477636251,19.2684857254403,-12.4926324808896));
#94303=CARTESIAN_POINT('Ctrl Pts',(16.6170008459317,19.2091074688849,-12.4890563034237));
#94304=CARTESIAN_POINT('Ctrl Pts',(16.6163526568764,19.2091064841458,-12.4890562790225));
#94305=CARTESIAN_POINT('Ctrl Pts',(16.6150299493055,19.0661177741218,-12.4804472042752));
#94306=CARTESIAN_POINT('Ctrl Pts',(16.637935879823,18.8192068412717,-12.4655558028099));
#94307=CARTESIAN_POINT('Ctrl Pts',(16.7071054573079,18.5818111963998,-12.4506644013445));
#94308=CARTESIAN_POINT('Ctrl Pts',(16.7437496504382,18.4842640742323,-12.4443820746265));
#94309=CARTESIAN_POINT('Origin',(18.734,19.211,0.));
#94310=CARTESIAN_POINT('',(16.7454194497538,18.4848895434008,-11.642549296791));
#94311=CARTESIAN_POINT('',(16.745419450367,18.4848895417216,-11.8674650022761));
#94312=CARTESIAN_POINT('',(16.7454194503191,18.4848895418526,0.));
#94313=CARTESIAN_POINT('',(16.6170009281725,19.212592427459,-11.9120627660338));
#94314=CARTESIAN_POINT('Ctrl Pts',(16.745419450367,18.4848895417216,-11.8674650022761));
#94315=CARTESIAN_POINT('Ctrl Pts',(16.7321284697392,18.5212892179149,-11.8699796928237));
#94316=CARTESIAN_POINT('Ctrl Pts',(16.7198387402319,18.5580487608643,-11.8724726230257));
#94317=CARTESIAN_POINT('Ctrl Pts',(16.7056938648529,18.6045673299265,-11.8755657071326));
#94318=CARTESIAN_POINT('Ctrl Pts',(16.7028893298231,18.6140277968553,-11.8761915999689));
#94319=CARTESIAN_POINT('Ctrl Pts',(16.6846213657658,18.6772699474235,-11.8803545196368));
#94320=CARTESIAN_POINT('Ctrl Pts',(16.6712285045199,18.7316303769976,-11.8838303722935));
#94321=CARTESIAN_POINT('Ctrl Pts',(16.6575927178034,18.7982452759099,-11.8879694743463));
#94322=CARTESIAN_POINT('Ctrl Pts',(16.6552811518111,18.810049101049,-11.8886984089892));
#94323=CARTESIAN_POINT('Ctrl Pts',(16.6516247957419,18.8296021107529,-11.8898986170216));
#94324=CARTESIAN_POINT('Ctrl Pts',(16.6502223883534,18.8373401158341,-11.8903717176368));
#94325=CARTESIAN_POINT('Ctrl Pts',(16.647762557358,18.851357294918,-11.891225390359));
#94326=CARTESIAN_POINT('Ctrl Pts',(16.6466902893433,18.857633737363,-11.8916064304635));
#94327=CARTESIAN_POINT('Ctrl Pts',(16.6446635453822,18.8698283232991,-11.892344452161));
#94328=CARTESIAN_POINT('Ctrl Pts',(16.6437058581411,18.875745864719,-11.8927015323105));
#94329=CARTESIAN_POINT('Ctrl Pts',(16.6416603294046,18.8887347544387,-11.8934830469093));
#94330=CARTESIAN_POINT('Ctrl Pts',(16.6405831710185,18.895807729015,-11.8939071403275));
#94331=CARTESIAN_POINT('Ctrl Pts',(16.6380228019412,18.9132122853069,-11.8949471700198));
#94332=CARTESIAN_POINT('Ctrl Pts',(16.636580092012,18.9235497030916,-11.8955618303798));
#94333=CARTESIAN_POINT('Ctrl Pts',(16.6230153970491,19.0262892828788,-11.9016413772041));
#94334=CARTESIAN_POINT('Ctrl Pts',(16.616930382029,19.1193894136381,-11.9069087404323));
#94335=CARTESIAN_POINT('Ctrl Pts',(16.6170006007779,19.2125948959813,-11.9120634735223));
#94336=CARTESIAN_POINT('Ctrl Pts',(16.6170005988961,19.2125923962176,-11.9120633352727));
#94337=CARTESIAN_POINT('Ctrl Pts',(16.6171096431973,19.3575605377985,-11.9200808075036));
#94338=CARTESIAN_POINT('Ctrl Pts',(16.6321085830719,19.5021326107325,-11.9277753928028));
#94339=CARTESIAN_POINT('Ctrl Pts',(16.6753598874925,19.7091047616055,-11.9395052990425));
#94340=CARTESIAN_POINT('Ctrl Pts',(16.6920125343409,19.7734881594003,-11.9432642931686));
#94341=CARTESIAN_POINT('Ctrl Pts',(16.7155919333298,19.8496660885941,-11.9479594196532));
#94342=CARTESIAN_POINT('Ctrl Pts',(16.719639492168,19.862319599458,-11.9487476794528));
#94343=CARTESIAN_POINT('Ctrl Pts',(16.72545184711,19.8799176825956,-11.9498567722796));
#94344=CARTESIAN_POINT('Ctrl Pts',(16.7271164455099,19.8848953523641,-11.9501719199984));
#94345=CARTESIAN_POINT('Ctrl Pts',(16.7299780585381,19.8933478330375,-11.9507095947849));
#94346=CARTESIAN_POINT('Ctrl Pts',(16.731165656707,19.8968258526719,-11.9509315671638));
#94347=CARTESIAN_POINT('Ctrl Pts',(16.7334554379233,19.9034750727794,-11.9513573594417));
#94348=CARTESIAN_POINT('Ctrl Pts',(16.7345561151745,19.9066467654954,-11.9515610853202));
#94349=CARTESIAN_POINT('Ctrl Pts',(16.7374837715901,19.9150187002132,-11.9521004549986));
#94350=CARTESIAN_POINT('Ctrl Pts',(16.7393235090342,19.9202144071966,-11.9524368465735));
#94351=CARTESIAN_POINT('Ctrl Pts',(16.7458814187719,19.9385076035979,-11.9536269110739));
#94352=CARTESIAN_POINT('Ctrl Pts',(16.7507083566868,19.9515653518591,-11.9544866873335));
#94353=CARTESIAN_POINT('Ctrl Pts',(16.8148892225599,20.1200575249106,-11.9657060977763));
#94354=CARTESIAN_POINT('Ctrl Pts',(16.8922334230719,20.2680061410319,-11.9768935262057));
#94355=CARTESIAN_POINT('Ctrl Pts',(17.0313948872008,20.4716635449461,-11.9930979087352));
#94356=CARTESIAN_POINT('Ctrl Pts',(17.080435770946,20.5353353551139,-11.9983095844323));
#94357=CARTESIAN_POINT('Ctrl Pts',(17.1587118285267,20.6258155367969,-12.0058900509515));
#94358=CARTESIAN_POINT('Ctrl Pts',(17.1852688175454,20.6548378940967,-12.0083516948774));
#94359=CARTESIAN_POINT('Ctrl Pts',(17.2310760798334,20.7021784255388,-12.0124188401085));
#94360=CARTESIAN_POINT('Ctrl Pts',(17.2498894116488,20.7209037282837,-12.0140420857559));
#94361=CARTESIAN_POINT('Ctrl Pts',(17.2761175036621,20.7460450992286,-12.0162427142381));
#94362=CARTESIAN_POINT('Ctrl Pts',(17.2832314096017,20.7527701942719,-12.0168335153521));
#94363=CARTESIAN_POINT('Ctrl Pts',(17.2947498907459,20.7635088161135,-12.0177804811171));
#94364=CARTESIAN_POINT('Ctrl Pts',(17.2991251469649,20.7675534550262,-12.018137979877));
#94365=CARTESIAN_POINT('Ctrl Pts',(17.3082764796628,20.7759418907548,-12.0188811854216));
#94366=CARTESIAN_POINT('Ctrl Pts',(17.3130554731019,20.7802824254369,-12.0192667512797));
#94367=CARTESIAN_POINT('Ctrl Pts',(17.3241346827433,20.7902530434893,-12.0201547977397));
#94368=CARTESIAN_POINT('Ctrl Pts',(17.3304489253187,20.795867430447,-12.0206566140765));
#94369=CARTESIAN_POINT('Ctrl Pts',(17.3475179863695,20.8108625826355,-12.0220017942487));
#94370=CARTESIAN_POINT('Ctrl Pts',(17.3583344437239,20.8201727531766,-12.0228422265579));
#94371=CARTESIAN_POINT('Ctrl Pts',(17.458578271993,20.9047072351699,-12.030524409898));
#94372=CARTESIAN_POINT('Ctrl Pts',(17.5540015251732,20.9725202664418,-12.0370493181345));
#94373=CARTESIAN_POINT('Ctrl Pts',(17.7945472526606,21.1151019582931,-12.0523574721807));
#94374=CARTESIAN_POINT('Ctrl Pts',(17.9436329802301,21.1816556906102,-12.0609576997701));
#94375=CARTESIAN_POINT('Ctrl Pts',(18.1298554940101,21.24022521602,-12.0721667263814));
#94376=CARTESIAN_POINT('Ctrl Pts',(18.1610814346634,21.2492614203661,-12.0740625626132));
#94377=CARTESIAN_POINT('Ctrl Pts',(18.1994995612107,21.2594263934635,-12.0764287290479));
#94378=CARTESIAN_POINT('Ctrl Pts',(18.2065074413095,21.2612421821793,-12.0768617015604));
#94379=CARTESIAN_POINT('Ctrl Pts',(18.2175078875264,21.2640323394769,-12.0775436736093));
#94380=CARTESIAN_POINT('Ctrl Pts',(18.2214942884731,21.2650311059421,-12.0777912874916));
#94381=CARTESIAN_POINT('Ctrl Pts',(18.2289509060658,21.2668762539518,-12.0782553870358));
#94382=CARTESIAN_POINT('Ctrl Pts',(18.232420365192,21.2677254625099,-12.0784717073496));
#94383=CARTESIAN_POINT('Ctrl Pts',(18.2403449178979,21.2696438863852,-12.0789666632021));
#94384=CARTESIAN_POINT('Ctrl Pts',(18.2448013281175,21.2707074184343,-12.0792456206439));
#94385=CARTESIAN_POINT('Ctrl Pts',(18.2585093924889,21.2739318809382,-12.0801055216055));
#94386=CARTESIAN_POINT('Ctrl Pts',(18.2677720208626,21.2760449697184,-12.0806891046106));
#94387=CARTESIAN_POINT('Ctrl Pts',(18.3518861181507,21.2946392113131,-12.0860096904517));
#94388=CARTESIAN_POINT('Ctrl Pts',(18.4275592304074,21.3071046800085,-12.0909455788181));
#94389=CARTESIAN_POINT('Ctrl Pts',(18.654447904586,21.3319308530719,-12.1058777259792));
#94390=CARTESIAN_POINT('Ctrl Pts',(18.8065177145713,21.3321847429283,-12.1160236107794));
#94391=CARTESIAN_POINT('Ctrl Pts',(19.0322519158724,21.3082396384638,-12.130611715981));
#94392=CARTESIAN_POINT('Ctrl Pts',(19.1067209252473,21.2962936463815,-12.135353870288));
#94393=CARTESIAN_POINT('Ctrl Pts',(19.198829694997,21.2764243504998,-12.1411265578811));
#94394=CARTESIAN_POINT('Ctrl Pts',(19.2172042100089,21.2722030759988,-12.1422736217243));
#94395=CARTESIAN_POINT('Ctrl Pts',(19.2438390872505,21.2657083542146,-12.1439302146524));
#94396=CARTESIAN_POINT('Ctrl Pts',(19.252145518692,21.2636294211552,-12.1444459728751));
#94397=CARTESIAN_POINT('Ctrl Pts',(19.2666870459439,21.2598960733974,-12.1453474133604));
#94398=CARTESIAN_POINT('Ctrl Pts',(19.2729275758728,21.2582634607915,-12.1457337942411));
#94399=CARTESIAN_POINT('Ctrl Pts',(19.2850308851751,21.2550378840272,-12.1464822815137));
#94400=CARTESIAN_POINT('Ctrl Pts',(19.2908944548695,21.2534481572551,-12.1468444884299));
#94401=CARTESIAN_POINT('Ctrl Pts',(19.3048955079425,21.2495874259188,-12.1477084383598));
#94402=CARTESIAN_POINT('Ctrl Pts',(19.3130264400135,21.247292896175,-12.1482094135657));
#94403=CARTESIAN_POINT('Ctrl Pts',(19.3423181631736,21.2388372077739,-12.1500116421698));
#94404=CARTESIAN_POINT('Ctrl Pts',(19.3633966292388,21.2323942380903,-12.1513037236844));
#94405=CARTESIAN_POINT('Ctrl Pts',(19.5615602018388,21.1684220296981,-12.1634154528012));
#94406=CARTESIAN_POINT('Ctrl Pts',(19.7304240961551,21.0880993238893,-12.1733718258654));
#94407=CARTESIAN_POINT('Ctrl Pts',(19.9535081067484,20.9432959069571,-12.1878722757483));
#94408=CARTESIAN_POINT('Ctrl Pts',(20.0178898790075,20.8961332069108,-12.1922591821868));
#94409=CARTESIAN_POINT('Ctrl Pts',(20.1071884375814,20.8226243594735,-12.1988759154432));
#94410=CARTESIAN_POINT('Ctrl Pts',(20.1343368086098,20.799091948806,-12.2009656715114));
#94411=CARTESIAN_POINT('Ctrl Pts',(20.1663822772901,20.7698539574843,-12.2035472600936));
#94412=CARTESIAN_POINT('Ctrl Pts',(20.171866336212,20.7647969765995,-12.2039932552835));
#94413=CARTESIAN_POINT('Ctrl Pts',(20.180365229202,20.7568764219995,-12.2046912189808));
#94414=CARTESIAN_POINT('Ctrl Pts',(20.1833986098913,20.7540327142679,-12.2049416927658));
#94415=CARTESIAN_POINT('Ctrl Pts',(20.1890179701563,20.748733534535,-12.2054082753903));
#94416=CARTESIAN_POINT('Ctrl Pts',(20.1916061301188,20.7462804582696,-12.2056242011531));
#94417=CARTESIAN_POINT('Ctrl Pts',(20.1974553340714,20.7407084190773,-12.2061145178176));
#94418=CARTESIAN_POINT('Ctrl Pts',(20.2007125948627,20.7375855774955,-12.2063892069038));
#94419=CARTESIAN_POINT('Ctrl Pts',(20.209099549725,20.7294931114919,-12.2071006915996));
#94420=CARTESIAN_POINT('Ctrl Pts',(20.2142140748927,20.7245079452776,-12.2075386567639));
#94421=CARTESIAN_POINT('Ctrl Pts',(20.2455220078266,20.693681387191,-12.210244313257));
#94422=CARTESIAN_POINT('Ctrl Pts',(20.2710615509035,20.6671882734104,-12.2125585183994));
#94423=CARTESIAN_POINT('Ctrl Pts',(20.4110382717863,20.5141986494772,-12.2257933979694));
#94424=CARTESIAN_POINT('Ctrl Pts',(20.5105487228058,20.3748994255009,-12.2373030417796));
#94425=CARTESIAN_POINT('Ctrl Pts',(20.6378804230543,20.1415880144799,-12.2545747517269));
#94426=CARTESIAN_POINT('Ctrl Pts',(20.6778077626523,20.0550203373955,-12.2606236815293));
#94427=CARTESIAN_POINT('Ctrl Pts',(20.7193968869128,19.9460815808388,-12.2677862145821));
#94428=CARTESIAN_POINT('Ctrl Pts',(20.7267165667087,19.9260010254396,-12.2690888545118));
#94429=CARTESIAN_POINT('Ctrl Pts',(20.7366870790697,19.8973050180554,-12.2709260702917));
#94430=CARTESIAN_POINT('Ctrl Pts',(20.7395887362517,19.8887786802632,-12.2714689368068));
#94431=CARTESIAN_POINT('Ctrl Pts',(20.7444988638096,19.8740429123714,-12.2724020347105));
#94432=CARTESIAN_POINT('Ctrl Pts',(20.746533179379,19.867842285792,-12.2727931158146));
#94433=CARTESIAN_POINT('Ctrl Pts',(20.750372201096,19.8559556052995,-12.2735398881133));
#94434=CARTESIAN_POINT('Ctrl Pts',(20.7521816049166,19.8502711450222,-12.2738957308973));
#94435=CARTESIAN_POINT('Ctrl Pts',(20.756821661761,19.8354777876433,-12.2748185044937));
#94436=CARTESIAN_POINT('Ctrl Pts',(20.7596148434133,19.8263572078229,-12.2753842022615));
#94437=CARTESIAN_POINT('Ctrl Pts',(20.7689166512403,19.7952342630008,-12.277303881443));
#94438=CARTESIAN_POINT('Ctrl Pts',(20.7751293294765,19.7731446188228,-12.2786482176882));
#94439=CARTESIAN_POINT('Ctrl Pts',(20.825898967173,19.5806767085031,-12.2902153262119));
#94440=CARTESIAN_POINT('Ctrl Pts',(20.8493946346846,19.4054591659866,-12.2996809660499));
#94441=CARTESIAN_POINT('Ctrl Pts',(20.8516705394732,19.1427783830044,-12.3139756449634));
#94442=CARTESIAN_POINT('Ctrl Pts',(20.8471102895636,19.0562575131338,-12.3187160867395));
#94443=CARTESIAN_POINT('Ctrl Pts',(20.8329796080339,18.9327989813262,-12.3258117197912));
#94444=CARTESIAN_POINT('Ctrl Pts',(20.8276910922077,18.8954553657526,-12.3280024935771));
#94445=CARTESIAN_POINT('Ctrl Pts',(20.8201480559763,18.8508159871393,-12.3306961049287));
#94446=CARTESIAN_POINT('Ctrl Pts',(20.8188475968985,18.8433633201579,-12.3311483316482));
#94447=CARTESIAN_POINT('Ctrl Pts',(20.816766487635,18.8318031674425,-12.3318539409595));
#94448=CARTESIAN_POINT('Ctrl Pts',(20.8160135529639,18.8276906674528,-12.3321057753653));
#94449=CARTESIAN_POINT('Ctrl Pts',(20.814596239774,18.8200767486476,-12.3325735800166));
#94450=CARTESIAN_POINT('Ctrl Pts',(20.8139352000489,18.8165747670038,-12.3327893588814));
#94451=CARTESIAN_POINT('Ctrl Pts',(20.8124228702988,18.8086724472087,-12.3332776537651));
#94452=CARTESIAN_POINT('Ctrl Pts',(20.81156645218,18.8042731586955,-12.333550457455));
#94453=CARTESIAN_POINT('Ctrl Pts',(20.8090037942633,18.791328474557,-12.3343559463221));
#94454=CARTESIAN_POINT('Ctrl Pts',(20.8072587783973,18.7827909771194,-12.3348907647034));
#94455=CARTESIAN_POINT('Ctrl Pts',(20.7944756120108,18.722159673948,-12.3387131405802));
#94456=CARTESIAN_POINT('Ctrl Pts',(20.7815289897598,18.670492260103,-12.3420974229617));
#94457=CARTESIAN_POINT('Ctrl Pts',(20.7620074593084,18.6034222527144,-12.3466116864115));
#94458=CARTESIAN_POINT('Ctrl Pts',(20.7571773535687,18.5875271862588,-12.3476906473172));
#94459=CARTESIAN_POINT('Ctrl Pts',(20.7477278573139,18.5576971662977,-12.3497308935988));
#94460=CARTESIAN_POINT('Ctrl Pts',(20.7431495701874,18.5437500695347,-12.3506912143554));
#94461=CARTESIAN_POINT('Ctrl Pts',(20.6967208145958,18.4071233431848,-12.3601554002246));
#94462=CARTESIAN_POINT('Ctrl Pts',(20.643827624164,18.2884747834949,-12.3688036312122));
#94463=CARTESIAN_POINT('Ctrl Pts',(20.5373339064651,18.098601224779,-12.3828978167145));
#94464=CARTESIAN_POINT('Ctrl Pts',(20.4895004456536,18.0245490779237,-12.3884735194934));
#94465=CARTESIAN_POINT('Ctrl Pts',(20.4250118794719,17.9371915185115,-12.3951371656135));
#94466=CARTESIAN_POINT('Ctrl Pts',(20.4125977907129,17.9208764681488,-12.3963859236246));
#94467=CARTESIAN_POINT('Ctrl Pts',(20.3944833488965,17.8977740131278,-12.3981608747712));
#94468=CARTESIAN_POINT('Ctrl Pts',(20.3889746155053,17.8908384680965,-12.3986946130581));
#94469=CARTESIAN_POINT('Ctrl Pts',(20.3793484338425,17.8788739663909,-12.3996169764498));
#94470=CARTESIAN_POINT('Ctrl Pts',(20.3752510843287,17.8738290618553,-12.4000063998237));
#94471=CARTESIAN_POINT('Ctrl Pts',(20.3673276039515,17.8641644803954,-12.4007534303614));
#94472=CARTESIAN_POINT('Ctrl Pts',(20.3635049492072,17.8595420464004,-12.4011111726863));
#94473=CARTESIAN_POINT('Ctrl Pts',(20.3534379427263,17.8474736224625,-12.4020464007615));
#94474=CARTESIAN_POINT('Ctrl Pts',(20.3471618317371,17.8400542162463,-12.4026225856986));
#94475=CARTESIAN_POINT('Ctrl Pts',(20.325195478112,17.8144460449859,-12.4046158489699));
#94476=CARTESIAN_POINT('Ctrl Pts',(20.3092465616662,17.7964808809792,-12.4060222392967));
#94477=CARTESIAN_POINT('Ctrl Pts',(20.1927354910093,17.6696557498313,-12.4160193822394));
#94478=CARTESIAN_POINT('Ctrl Pts',(20.0812918925884,17.5713468127318,-12.4241001588517));
#94479=CARTESIAN_POINT('Ctrl Pts',(19.9229286085026,17.4587841409114,-12.4346515884927));
#94480=CARTESIAN_POINT('Ctrl Pts',(19.8845151478869,17.4333255505874,-12.4371511184435));
#94481=CARTESIAN_POINT('Ctrl Pts',(19.7845337156379,17.3716616922227,-12.4435769042513));
#94482=CARTESIAN_POINT('Ctrl Pts',(19.721912533718,17.3372834331545,-12.4475273896887));
#94483=CARTESIAN_POINT('Ctrl Pts',(19.6274697117914,17.291487528235,-12.4535470183183));
#94484=CARTESIAN_POINT('Ctrl Pts',(19.596917157227,17.2775600736383,-12.4555036208632));
#94485=CARTESIAN_POINT('Ctrl Pts',(19.5593255912544,17.2614923387313,-12.4579373551384));
#94486=CARTESIAN_POINT('Ctrl Pts',(19.5525880771511,17.2586537168506,-12.4583745682869));
#94487=CARTESIAN_POINT('Ctrl Pts',(19.5420260971823,17.2542680701593,-12.4590617496848));
#94488=CARTESIAN_POINT('Ctrl Pts',(19.5382115089865,17.2526971972823,-12.4593102971578));
#94489=CARTESIAN_POINT('Ctrl Pts',(19.5310875593136,17.2497878324102,-12.4597751937771));
#94490=CARTESIAN_POINT('Ctrl Pts',(19.5277793955357,17.2484465576455,-12.4599913717436));
#94491=CARTESIAN_POINT('Ctrl Pts',(19.5202392979072,17.2454116544916,-12.4604847515597));
#94492=CARTESIAN_POINT('Ctrl Pts',(19.5160052936139,17.2437233297185,-12.460762267312));
#94493=CARTESIAN_POINT('Ctrl Pts',(19.5049830520162,17.239369375471,-12.4614858655785));
#94494=CARTESIAN_POINT('Ctrl Pts',(19.4981865003339,17.2367251520474,-12.4619331834344));
#94495=CARTESIAN_POINT('Ctrl Pts',(19.4548264452209,17.2201132058259,-12.4647935106258));
#94496=CARTESIAN_POINT('Ctrl Pts',(19.4178976208762,17.2071276018675,-12.4672591479848));
#94497=CARTESIAN_POINT('Ctrl Pts',(19.368876677719,17.1914027538968,-12.4705515730435));
#94498=CARTESIAN_POINT('Ctrl Pts',(19.3570878125481,17.1877345701858,-12.4713448221732));
#94499=CARTESIAN_POINT('Ctrl Pts',(19.3221513500614,17.1771981510138,-12.4736986868448));
#94500=CARTESIAN_POINT('Ctrl Pts',(19.2989179713522,17.1706226831521,-12.4752679828094));
#94501=CARTESIAN_POINT('Ctrl Pts',(19.136219586817,17.1275679421086,-12.4862637304607));
#94502=CARTESIAN_POINT('Ctrl Pts',(18.9934447957794,17.1050172893108,-12.4959108505562));
#94503=CARTESIAN_POINT('Ctrl Pts',(18.7877688675211,17.0937805088541,-12.5092191007373));
#94504=CARTESIAN_POINT('Ctrl Pts',(18.725928863084,17.0931129746347,-12.5131506922479));
#94505=CARTESIAN_POINT('Ctrl Pts',(18.6269048287152,17.0963823389101,-12.5193243150439));
#94506=CARTESIAN_POINT('Ctrl Pts',(18.589703425803,17.0985947349766,-12.5216162621416));
#94507=CARTESIAN_POINT('Ctrl Pts',(18.5414838681116,17.1027423008144,-12.5245533575229));
#94508=CARTESIAN_POINT('Ctrl Pts',(18.5303974165945,17.1037840683346,-12.5252263380837));
#94509=CARTESIAN_POINT('Ctrl Pts',(18.5123855124175,17.1056200820047,-12.526316088961));
#94510=CARTESIAN_POINT('Ctrl Pts',(18.5054549622964,17.1063611360252,-12.5267345251576));
#94511=CARTESIAN_POINT('Ctrl Pts',(18.4921372978715,17.1078516962115,-12.5275369491177));
#94512=CARTESIAN_POINT('Ctrl Pts',(18.4857497012345,17.108596103271,-12.5279210927996));
#94513=CARTESIAN_POINT('Ctrl Pts',(18.4711367115343,17.1103666195087,-12.528798286207));
#94514=CARTESIAN_POINT('Ctrl Pts',(18.4629137212387,17.1114119594293,-12.5292907239928));
#94515=CARTESIAN_POINT('Ctrl Pts',(18.4410945113366,17.1143160276475,-12.5305943799195));
#94516=CARTESIAN_POINT('Ctrl Pts',(18.4275097236942,17.116258720279,-12.5314029463139));
#94517=CARTESIAN_POINT('Ctrl Pts',(18.3247120659353,17.1319807427865,-12.5374997844465));
#94518=CARTESIAN_POINT('Ctrl Pts',(18.2364379517191,17.1513222199464,-12.5426055671439));
#94519=CARTESIAN_POINT('Ctrl Pts',(18.0155892138936,17.2147454531445,-12.5553255416308));
#94520=CARTESIAN_POINT('Ctrl Pts',(17.8856584964277,17.2664020691091,-12.5627450038856));
#94521=CARTESIAN_POINT('Ctrl Pts',(17.7126395441167,17.3558533749178,-12.5735037395324));
#94522=CARTESIAN_POINT('Ctrl Pts',(17.6645406028387,17.3831592167064,-12.5766018451786));
#94523=CARTESIAN_POINT('Ctrl Pts',(17.5933680159443,17.4273355104765,-12.5814337294784));
#94524=CARTESIAN_POINT('Ctrl Pts',(17.5694739196579,17.4428430040043,-12.5831003750124));
#94525=CARTESIAN_POINT('Ctrl Pts',(17.5401543114251,17.4627237960453,-12.5852109951811));
#94526=CARTESIAN_POINT('Ctrl Pts',(17.5344266221051,17.466648853745,-12.58562648726));
#94527=CARTESIAN_POINT('Ctrl Pts',(17.5253935807098,17.4729045251356,-12.586286969709));
#94528=CARTESIAN_POINT('Ctrl Pts',(17.5220753618901,17.4752165954805,-12.5865307152054));
#94529=CARTESIAN_POINT('Ctrl Pts',(17.5158296036695,17.4795951581254,-12.5869916705161));
#94530=CARTESIAN_POINT('Ctrl Pts',(17.512900678641,17.48165958018,-12.587208739687));
#94531=CARTESIAN_POINT('Ctrl Pts',(17.5062161283549,17.4863965638748,-12.587706208314));
#94532=CARTESIAN_POINT('Ctrl Pts',(17.5024639856418,17.4890739586793,-12.5879869371815));
#94533=CARTESIAN_POINT('Ctrl Pts',(17.4925254489283,17.4962148433087,-12.5887344254519));
#94534=CARTESIAN_POINT('Ctrl Pts',(17.4863544516233,17.500699507057,-12.5892025899524));
#94535=CARTESIAN_POINT('Ctrl Pts',(17.4432974580955,17.5323474527857,-12.5924967257349));
#94536=CARTESIAN_POINT('Ctrl Pts',(17.407280202645,17.5606663014199,-12.5953947608523));
#94537=CARTESIAN_POINT('Ctrl Pts',(17.3434298709737,17.6143106269932,-12.6007561933977));
#94538=CARTESIAN_POINT('Ctrl Pts',(17.315297263426,17.6392542963525,-12.6032035501016));
#94539=CARTESIAN_POINT('Ctrl Pts',(17.1921807784063,17.7544145681658,-12.6142536644186));
#94540=CARTESIAN_POINT('Ctrl Pts',(17.1050207995226,17.8525898696697,-12.6229968670819));
#94541=CARTESIAN_POINT('Ctrl Pts',(16.9752027213444,18.0294209688657,-12.6372013371042));
#94542=CARTESIAN_POINT('Ctrl Pts',(16.9274171728916,18.1038600867,-12.6427967365363));
#94543=CARTESIAN_POINT('Ctrl Pts',(16.8744284151348,18.1990196298712,-12.6494812445963));
#94544=CARTESIAN_POINT('Ctrl Pts',(16.8646987222113,18.2171068828746,-12.6507322979998));
#94545=CARTESIAN_POINT('Ctrl Pts',(16.8511486118679,18.2431992926252,-12.6525099078202));
#94546=CARTESIAN_POINT('Ctrl Pts',(16.8471131308596,18.2510908867055,-12.653044040467));
#94547=CARTESIAN_POINT('Ctrl Pts',(16.8402042040713,18.26481358278,-12.6539668662221));
#94548=CARTESIAN_POINT('Ctrl Pts',(16.8373078572203,18.2706329600688,-12.6543563598096));
#94549=CARTESIAN_POINT('Ctrl Pts',(16.8317911219144,18.281846436332,-12.6551033731214));
#94550=CARTESIAN_POINT('Ctrl Pts',(16.8291667639027,18.2872385023488,-12.6554610287311));
#94551=CARTESIAN_POINT('Ctrl Pts',(16.8223533113959,18.3013900762796,-12.6563956933988));
#94552=CARTESIAN_POINT('Ctrl Pts',(16.8182014751491,18.3101674448976,-12.65697140473));
#94553=CARTESIAN_POINT('Ctrl Pts',(16.8040088660262,18.340713888129,-12.6589613795846));
#94554=CARTESIAN_POINT('Ctrl Pts',(16.7942773401895,18.3626252210065,-12.6603650026611));
#94555=CARTESIAN_POINT('Ctrl Pts',(16.770898167933,18.417771972556,-12.6638421750932));
#94556=CARTESIAN_POINT('Ctrl Pts',(16.7577281090364,18.4511801383449,-12.6658990859603));
#94557=CARTESIAN_POINT('Ctrl Pts',(16.7454195353148,18.4848893090773,-12.6679318638109));
#94558=CARTESIAN_POINT('',(16.6141771432254,19.2120774369074,-11.6890562790225));
#94559=CARTESIAN_POINT('Ctrl Pts',(16.7437496504382,18.4842640742323,-12.4443820746265));
#94560=CARTESIAN_POINT('Ctrl Pts',(16.9543734431303,17.9235819283861,-12.4082724657841));
#94561=CARTESIAN_POINT('Ctrl Pts',(17.94829019586,16.8917270960979,-12.329770921381));
#94562=CARTESIAN_POINT('Ctrl Pts',(20.2082246499765,17.1878857088602,-12.2088774414178));
#94563=CARTESIAN_POINT('Ctrl Pts',(21.2330887962208,19.3555162351247,-12.0817016347362));
#94564=CARTESIAN_POINT('Ctrl Pts',(19.9651940828767,21.3905620853514,-11.9545258280549));
#94565=CARTESIAN_POINT('Ctrl Pts',(17.567755215016,21.4259950011477,-11.8273500213734));
#94566=CARTESIAN_POINT('Ctrl Pts',(16.6440838354548,20.0366853275688,-11.7388601716959));
#94567=CARTESIAN_POINT('Ctrl Pts',(16.613796038846,19.2734660709366,-11.692762257579));
#94568=CARTESIAN_POINT('Ctrl Pts',(16.6141771432254,19.2120774369074,-11.6890562790225));
#94569=CARTESIAN_POINT('Ctrl Pts',(16.6170002227512,19.2119711480246,-11.6906772989821));
#94570=CARTESIAN_POINT('Ctrl Pts',(16.6169205026538,19.0381897839503,-11.6794990057181));
#94571=CARTESIAN_POINT('Ctrl Pts',(16.6382377399725,18.865048996398,-11.6677742008829));
#94572=CARTESIAN_POINT('Ctrl Pts',(16.6953336165312,18.6371881017047,-11.6526052839768));
#94573=CARTESIAN_POINT('Ctrl Pts',(16.7127403586391,18.5785988026368,-11.6487214519702));
#94574=CARTESIAN_POINT('Ctrl Pts',(16.7368041306635,18.5088181354777,-11.6441232612583));
#94575=CARTESIAN_POINT('Ctrl Pts',(16.7410579839532,18.4968341807256,-11.6433345260294));
#94576=CARTESIAN_POINT('Ctrl Pts',(16.7454194497538,18.4848895434008,-11.642549296791));
#94577=CARTESIAN_POINT('Origin',(18.734,19.211,0.));
#94578=CARTESIAN_POINT('',(16.7454194500511,18.4848895425866,-10.8441190257052));
#94579=CARTESIAN_POINT('',(16.7454194505824,18.4848895411316,-11.0644158872188));
#94580=CARTESIAN_POINT('',(16.7454194503191,18.4848895418526,0.));
#94581=CARTESIAN_POINT('Ctrl Pts',(16.7454194505824,18.4848895411316,-11.0644158872188));
#94582=CARTESIAN_POINT('Ctrl Pts',(16.7100155209546,18.5818493975431,-11.0708123982825));
#94583=CARTESIAN_POINT('Ctrl Pts',(16.6817531128539,18.681261479843,-11.0775606724488));
#94584=CARTESIAN_POINT('Ctrl Pts',(16.6317924842058,18.922881279888,-11.0938351315304));
#94585=CARTESIAN_POINT('Ctrl Pts',(16.6170952308513,19.0660441061833,-11.103353731068));
#94586=CARTESIAN_POINT('Ctrl Pts',(16.6169595358832,19.2715966104105,-11.1164063514006));
#94587=CARTESIAN_POINT('Ctrl Pts',(16.6196417425651,19.3335670533862,-11.1202673935233));
#94588=CARTESIAN_POINT('Ctrl Pts',(16.6261219959195,19.4077067085304,-11.1248001812546));
#94589=CARTESIAN_POINT('Ctrl Pts',(16.6273121369466,19.4200680923591,-11.1255530928494));
#94590=CARTESIAN_POINT('Ctrl Pts',(16.6294460864631,19.4403590520909,-11.1267844640882));
#94591=CARTESIAN_POINT('Ctrl Pts',(16.630326098816,19.448294900835,-11.1272649195133));
#94592=CARTESIAN_POINT('Ctrl Pts',(16.6319896971689,19.4625598422829,-11.1281265638762));
#94593=CARTESIAN_POINT('Ctrl Pts',(16.6327570213205,19.4688907004645,-11.1285082603374));
#94594=CARTESIAN_POINT('Ctrl Pts',(16.6344530088735,19.4823732466887,-11.1293196760289));
#94595=CARTESIAN_POINT('Ctrl Pts',(16.635389634705,19.489523865437,-11.1297491389087));
#94596=CARTESIAN_POINT('Ctrl Pts',(16.6380125560209,19.5087836565671,-11.1309035772139));
#94597=CARTESIAN_POINT('Ctrl Pts',(16.6397672554953,19.5208833534279,-11.131626385958));
#94598=CARTESIAN_POINT('Ctrl Pts',(16.6490971429036,19.5815156080685,-11.1352369209254));
#94599=CARTESIAN_POINT('Ctrl Pts',(16.6582553385621,19.6297915850873,-11.1380741281951));
#94600=CARTESIAN_POINT('Ctrl Pts',(16.6895710865478,19.768345710885,-11.1461497711089));
#94601=CARTESIAN_POINT('Ctrl Pts',(16.7160033333925,19.8575410347184,-11.1512603757036));
#94602=CARTESIAN_POINT('Ctrl Pts',(16.8056500760732,20.1001682217777,-11.1653488990541));
#94603=CARTESIAN_POINT('Ctrl Pts',(16.8811330610567,20.2483141341045,-11.1741493464689));
#94604=CARTESIAN_POINT('Ctrl Pts',(16.9808577988162,20.3977505844248,-11.1847107227762));
#94605=CARTESIAN_POINT('Ctrl Pts',(16.98873445628,20.4093040873631,-11.1855393832611));
#94606=CARTESIAN_POINT('Ctrl Pts',(16.9998805489716,20.4253101852528,-11.1867056854588));
#94607=CARTESIAN_POINT('Ctrl Pts',(17.0030540294999,20.429829578773,-11.1870370549439));
#94608=CARTESIAN_POINT('Ctrl Pts',(17.0081863109764,20.4370780543811,-11.1875719354958));
#94609=CARTESIAN_POINT('Ctrl Pts',(17.0101340133915,20.4398150163902,-11.1877746886095));
#94610=CARTESIAN_POINT('Ctrl Pts',(17.0142251821318,20.4455351634391,-11.1882001112914));
#94611=CARTESIAN_POINT('Ctrl Pts',(17.0163699007564,20.4485174081177,-11.1884228701987));
#94612=CARTESIAN_POINT('Ctrl Pts',(17.0215923833213,20.4557395728477,-11.1889646379422));
#94613=CARTESIAN_POINT('Ctrl Pts',(17.0246781354243,20.4599736633754,-11.1892841947015));
#94614=CARTESIAN_POINT('Ctrl Pts',(17.0356087267315,20.4748556096623,-11.1904140905413));
#94615=CARTESIAN_POINT('Ctrl Pts',(17.0435374119241,20.4854411077792,-11.1912299669469));
#94616=CARTESIAN_POINT('Ctrl Pts',(17.0915650921809,20.5483255707599,-11.1961467131398));
#94617=CARTESIAN_POINT('Ctrl Pts',(17.1339858129166,20.5987986288466,-11.2003844459875));
#94618=CARTESIAN_POINT('Ctrl Pts',(17.2439182046635,20.7178479316795,-11.2109620835965));
#94619=CARTESIAN_POINT('Ctrl Pts',(17.3138862261073,20.7839625368012,-11.2173577552389));
#94620=CARTESIAN_POINT('Ctrl Pts',(17.4967378702986,20.9345654833649,-11.2329412957291));
#94621=CARTESIAN_POINT('Ctrl Pts',(17.6140380995269,21.0129972723151,-11.2419898342652));
#94622=CARTESIAN_POINT('Ctrl Pts',(17.7508858945676,21.0859346175174,-11.2514584834878));
#94623=CARTESIAN_POINT('Ctrl Pts',(17.7635632818766,21.09252750607,-11.2523264140155));
#94624=CARTESIAN_POINT('Ctrl Pts',(17.7838464437517,21.1028162423241,-11.2537006644079));
#94625=CARTESIAN_POINT('Ctrl Pts',(17.7914091180115,21.1065956603674,-11.2542099119544));
#94626=CARTESIAN_POINT('Ctrl Pts',(17.8047871230571,21.1131814104047,-11.2551052749282));
#94627=CARTESIAN_POINT('Ctrl Pts',(17.8105929944578,21.1160066121445,-11.2554920464123));
#94628=CARTESIAN_POINT('Ctrl Pts',(17.8226282448171,21.1217951507859,-11.2562901181425));
#94629=CARTESIAN_POINT('Ctrl Pts',(17.8288593712895,21.124754693894,-11.2567012829711));
#94630=CARTESIAN_POINT('Ctrl Pts',(17.8448911769946,21.1322733632655,-11.2577540212421));
#94631=CARTESIAN_POINT('Ctrl Pts',(17.8547125856237,21.1367880166358,-11.2583940532195));
#94632=CARTESIAN_POINT('Ctrl Pts',(17.8958499820366,21.1553175219463,-11.2610549434631));
#94633=CARTESIAN_POINT('Ctrl Pts',(17.9274707809677,21.1686457530066,-11.2630522679164));
#94634=CARTESIAN_POINT('Ctrl Pts',(18.0106938833782,21.2013654595668,-11.2681969654979));
#94635=CARTESIAN_POINT('Ctrl Pts',(18.0627550250274,21.2195211550232,-11.2713049371841));
#94636=CARTESIAN_POINT('Ctrl Pts',(18.2200495712485,21.267575302397,-11.2804500677529));
#94637=CARTESIAN_POINT('Ctrl Pts',(18.326951961139,21.2913749168322,-11.2863384996509));
#94638=CARTESIAN_POINT('Ctrl Pts',(18.4810914173601,21.3133495800491,-11.2948153811085));
#94639=CARTESIAN_POINT('Ctrl Pts',(18.5271698631718,21.3183816819776,-11.2973493723591));
#94640=CARTESIAN_POINT('Ctrl Pts',(18.5947048982484,21.3235206463984,-11.3011064844839));
#94641=CARTESIAN_POINT('Ctrl Pts',(18.6160578680894,21.3248202897957,-11.302300710048));
#94642=CARTESIAN_POINT('Ctrl Pts',(18.6892274552065,21.328161630565,-11.3064251205685));
#94643=CARTESIAN_POINT('Ctrl Pts',(18.7410935464018,21.3286228862856,-11.3094038028982));
#94644=CARTESIAN_POINT('Ctrl Pts',(18.8015714079021,21.326939039566,-11.3129945970821));
#94645=CARTESIAN_POINT('Ctrl Pts',(18.8102216347434,21.3266450956905,-11.3135110055463));
#94646=CARTESIAN_POINT('Ctrl Pts',(18.8233352824615,21.3261189520454,-11.3142984672772));
#94647=CARTESIAN_POINT('Ctrl Pts',(18.8278002913827,21.3259256437256,-11.3145673944245));
#94648=CARTESIAN_POINT('Ctrl Pts',(18.8358238574311,21.3255528126936,-11.3150521583737));
#94649=CARTESIAN_POINT('Ctrl Pts',(18.8393825996404,21.3253784436563,-11.3152677038226));
#94650=CARTESIAN_POINT('Ctrl Pts',(18.8471261192545,21.3249794330817,-11.3157378880298));
#94651=CARTESIAN_POINT('Ctrl Pts',(18.8513106211726,21.3247513524082,-11.3159927119883));
#94652=CARTESIAN_POINT('Ctrl Pts',(18.8630926175503,21.3240740687784,-11.3167122389516));
#94653=CARTESIAN_POINT('Ctrl Pts',(18.8706883165142,21.3235963230442,-11.3171784956036));
#94654=CARTESIAN_POINT('Ctrl Pts',(18.9167068270839,21.320452687094,-11.3200171058944));
#94655=CARTESIAN_POINT('Ctrl Pts',(18.9550510197204,21.3167797699134,-11.3224405678));
#94656=CARTESIAN_POINT('Ctrl Pts',(19.0823648430219,21.3010692722043,-11.3306354298562));
#94657=CARTESIAN_POINT('Ctrl Pts',(19.1706640183234,21.2844199232623,-11.3365579453396));
#94658=CARTESIAN_POINT('Ctrl Pts',(19.4238479021482,21.219787298917,-11.3538250265188));
#94659=CARTESIAN_POINT('Ctrl Pts',(19.5843218646416,21.1573019400146,-11.3650715601222));
#94660=CARTESIAN_POINT('Ctrl Pts',(19.7560026546548,21.0651144753561,-11.3770690621102));
#94661=CARTESIAN_POINT('Ctrl Pts',(19.7763109033676,21.0537745283356,-11.3784890982728));
#94662=CARTESIAN_POINT('Ctrl Pts',(19.8047237576558,21.0372890253844,-11.3804777561737));
#94663=CARTESIAN_POINT('Ctrl Pts',(19.8129860064507,21.0324198231231,-11.3810562797581));
#94664=CARTESIAN_POINT('Ctrl Pts',(19.8263416651968,21.024426145331,-11.3819919138221));
#94665=CARTESIAN_POINT('Ctrl Pts',(19.8314553672487,21.0213359953691,-11.3823502684009));
#94666=CARTESIAN_POINT('Ctrl Pts',(19.8421199202348,21.0148297376691,-11.3830978784549));
#94667=CARTESIAN_POINT('Ctrl Pts',(19.8476682224185,21.0114095567289,-11.3834869795186));
#94668=CARTESIAN_POINT('Ctrl Pts',(19.8608077636216,21.0032258728076,-11.3844088635331));
#94669=CARTESIAN_POINT('Ctrl Pts',(19.8683847630615,20.9984396572793,-11.3849408017873));
#94670=CARTESIAN_POINT('Ctrl Pts',(19.8937060804997,20.9822189036811,-11.3867197736012));
#94671=CARTESIAN_POINT('Ctrl Pts',(19.9113100788448,20.9705668852392,-11.3879587104262));
#94672=CARTESIAN_POINT('Ctrl Pts',(20.0055409993628,20.9061483842077,-11.3946073244253));
#94673=CARTESIAN_POINT('Ctrl Pts',(20.078804807354,20.8486347238049,-11.3998314008981));
#94674=CARTESIAN_POINT('Ctrl Pts',(20.2632259593262,20.683109805168,-11.4134782156319));
#94675=CARTESIAN_POINT('Ctrl Pts',(20.3667062475343,20.5674303073793,-11.4216619975953));
#94676=CARTESIAN_POINT('Ctrl Pts',(20.4878082271995,20.3978948919597,-11.4333763599681));
#94677=CARTESIAN_POINT('Ctrl Pts',(20.5172970523708,20.3531091772455,-11.4364518106027));
#94678=CARTESIAN_POINT('Ctrl Pts',(20.549577226751,20.2997812907847,-11.4401509216324));
#94679=CARTESIAN_POINT('Ctrl Pts',(20.5540560298866,20.2922776736705,-11.4406722443179));
#94680=CARTESIAN_POINT('Ctrl Pts',(20.560764084092,20.2808794867444,-11.4414657359611));
#94681=CARTESIAN_POINT('Ctrl Pts',(20.5630276825952,20.277005098737,-11.44173572967));
#94682=CARTESIAN_POINT('Ctrl Pts',(20.5670671435151,20.2700403916653,-11.442221625785));
#94683=CARTESIAN_POINT('Ctrl Pts',(20.5688475333894,20.2669527606548,-11.4424372307562));
#94684=CARTESIAN_POINT('Ctrl Pts',(20.5726974245113,20.2602369736901,-11.4429066194741));
#94685=CARTESIAN_POINT('Ctrl Pts',(20.5747639609768,20.2566072327294,-11.4431605833631));
#94686=CARTESIAN_POINT('Ctrl Pts',(20.5805341218841,20.2464021868462,-11.44387530714));
#94687=CARTESIAN_POINT('Ctrl Pts',(20.5842133049146,20.2398132358139,-11.4443375883397));
#94688=CARTESIAN_POINT('Ctrl Pts',(20.6059098000369,20.2004647616597,-11.4471024736854));
#94689=CARTESIAN_POINT('Ctrl Pts',(20.6230907602157,20.1672544205329,-11.4494532142814));
#94690=CARTESIAN_POINT('Ctrl Pts',(20.6765544968016,20.056840541456,-11.4572826234238));
#94691=CARTESIAN_POINT('Ctrl Pts',(20.7090509171831,19.9779003835404,-11.4628991004263));
#94692=CARTESIAN_POINT('Ctrl Pts',(20.7943638057795,19.7289198915577,-11.4802860895096));
#94693=CARTESIAN_POINT('Ctrl Pts',(20.8305987731937,19.5539840016201,-11.4919767010469));
#94694=CARTESIAN_POINT('Ctrl Pts',(20.8462998904509,19.3538217910648,-11.5043325981684));
#94695=CARTESIAN_POINT('Ctrl Pts',(20.8477156735588,19.3310625102459,-11.5057243585255));
#94696=CARTESIAN_POINT('Ctrl Pts',(20.84920078048,19.298779221499,-11.5076805794816));
#94697=CARTESIAN_POINT('Ctrl Pts',(20.8495739469298,19.2892714070752,-11.5082545108053));
#94698=CARTESIAN_POINT('Ctrl Pts',(20.8500766254266,19.2738032695293,-11.5091847384302));
#94699=CARTESIAN_POINT('Ctrl Pts',(20.8502450821908,19.2678444242939,-11.5095422506322));
#94700=CARTESIAN_POINT('Ctrl Pts',(20.8505453138515,19.2553572855913,-11.5102897046013));
#94701=CARTESIAN_POINT('Ctrl Pts',(20.850672059687,19.2488289252443,-11.5106794849216));
#94702=CARTESIAN_POINT('Ctrl Pts',(20.8509020667678,19.2332739296784,-11.5116058889582));
#94703=CARTESIAN_POINT('Ctrl Pts',(20.8509778009979,19.2242469677634,-11.5121416453721));
#94704=CARTESIAN_POINT('Ctrl Pts',(20.8510386375244,19.1937256073128,-11.51394702882));
#94705=CARTESIAN_POINT('Ctrl Pts',(20.8507541321625,19.1722315662489,-11.5152082218536));
#94706=CARTESIAN_POINT('Ctrl Pts',(20.8450347463484,18.9713680465519,-11.5269079776311));
#94707=CARTESIAN_POINT('Ctrl Pts',(20.8171428806372,18.7933710984562,-11.536549798781));
#94708=CARTESIAN_POINT('Ctrl Pts',(20.7335446954159,18.5052876122127,-11.5528749525616));
#94709=CARTESIAN_POINT('Ctrl Pts',(20.6901482449709,18.392657448145,-11.5594858166961));
#94710=CARTESIAN_POINT('Ctrl Pts',(20.6332623359645,18.2758092422703,-11.5671880479486));
#94711=CARTESIAN_POINT('Ctrl Pts',(20.629048433378,18.2672995169497,-11.5677540744023));
#94712=CARTESIAN_POINT('Ctrl Pts',(20.6227172211405,18.2547274231828,-11.5685983089103));
#94713=CARTESIAN_POINT('Ctrl Pts',(20.6206436794066,18.2506429785462,-11.5688738452561));
#94714=CARTESIAN_POINT('Ctrl Pts',(20.6169297065753,18.2433856769471,-11.5693657251252));
#94715=CARTESIAN_POINT('Ctrl Pts',(20.6152944857216,18.24021021027,-11.5695817397259));
#94716=CARTESIAN_POINT('Ctrl Pts',(20.6117602214748,18.2333894206513,-11.5700474490644));
#94717=CARTESIAN_POINT('Ctrl Pts',(20.6098586237131,18.2297455389222,-11.5702972994488));
#94718=CARTESIAN_POINT('Ctrl Pts',(20.6045771761872,18.2196965768834,-11.5709891934025));
#94719=CARTESIAN_POINT('Ctrl Pts',(20.6011750893326,18.2133033371612,-11.5714326087916));
#94720=CARTESIAN_POINT('Ctrl Pts',(20.5823043108541,18.1782757462077,-11.5738792592153));
#94721=CARTESIAN_POINT('Ctrl Pts',(20.5662105856455,18.1499852449713,-11.5759188554206));
#94722=CARTESIAN_POINT('Ctrl Pts',(20.4657863631264,17.9825558733656,-11.5883250567758));
#94723=CARTESIAN_POINT('Ctrl Pts',(20.3662985886181,17.8531486721246,-11.5992814249176));
#94724=CARTESIAN_POINT('Ctrl Pts',(20.1716286397717,17.6526190376877,-11.6175367886597));
#94725=CARTESIAN_POINT('Ctrl Pts',(20.0834797711903,17.5756897918332,-11.6249758593466));
#94726=CARTESIAN_POINT('Ctrl Pts',(19.977903867916,17.4979335280801,-11.6329821446538));
#94727=CARTESIAN_POINT('Ctrl Pts',(19.9663015454054,17.4895684774626,-11.6338509484377));
#94728=CARTESIAN_POINT('Ctrl Pts',(19.9477042316927,17.4764445576263,-11.6352263157279));
#94729=CARTESIAN_POINT('Ctrl Pts',(19.9407641100374,17.4716090345565,-11.6357358143247));
#94730=CARTESIAN_POINT('Ctrl Pts',(19.9284749314416,17.4631555173197,-11.6366314693461));
#94731=CARTESIAN_POINT('Ctrl Pts',(19.9231379873602,17.4595201839791,-11.6370182831746));
#94732=CARTESIAN_POINT('Ctrl Pts',(19.9120669488827,17.4520529213889,-11.6378162993372));
#94733=CARTESIAN_POINT('Ctrl Pts',(19.9063305894001,17.4482244747865,-11.6382273669583));
#94734=CARTESIAN_POINT('Ctrl Pts',(19.8915620700298,17.4384719394702,-11.6392795606297));
#94735=CARTESIAN_POINT('Ctrl Pts',(19.88250302337,17.432588775566,-11.639919148345));
#94736=CARTESIAN_POINT('Ctrl Pts',(19.8445393624395,17.4083453262,-11.6425757237159));
#94737=CARTESIAN_POINT('Ctrl Pts',(19.8152355009437,17.3906177501525,-11.6445692748649));
#94738=CARTESIAN_POINT('Ctrl Pts',(19.7378064449826,17.3463062053433,-11.6497020610826));
#94739=CARTESIAN_POINT('Ctrl Pts',(19.689052331027,17.3208714294798,-11.6528021335327));
#94740=CARTESIAN_POINT('Ctrl Pts',(19.4687975385746,17.2166667699708,-11.6663520848232));
#94741=CARTESIAN_POINT('Ctrl Pts',(19.2882348186666,17.1591466038571,-11.676199034747));
#94742=CARTESIAN_POINT('Ctrl Pts',(19.0615060721991,17.1190729992212,-11.6892860808687));
#94743=CARTESIAN_POINT('Ctrl Pts',(19.0203485402759,17.1130431840534,-11.6916931939166));
#94744=CARTESIAN_POINT('Ctrl Pts',(18.9716773735515,17.107371358697,-11.6946045333284));
#94745=CARTESIAN_POINT('Ctrl Pts',(18.9643070613432,17.1065516997908,-11.6950471432882));
#94746=CARTESIAN_POINT('Ctrl Pts',(18.9523628739711,17.1052868730707,-11.6957674704168));
#94747=CARTESIAN_POINT('Ctrl Pts',(18.9477915162596,17.1048178368638,-11.6960438795591));
#94748=CARTESIAN_POINT('Ctrl Pts',(18.9396629405831,17.1040105545768,-11.6965367156421));
#94749=CARTESIAN_POINT('Ctrl Pts',(18.9361063568446,17.1036664268429,-11.6967528087136));
#94750=CARTESIAN_POINT('Ctrl Pts',(18.9284663623562,17.1029467158834,-11.6972180021051));
#94751=CARTESIAN_POINT('Ctrl Pts',(18.9243827872086,17.1025739974004,-11.6974672544637));
#94752=CARTESIAN_POINT('Ctrl Pts',(18.9131279491697,17.1015797024991,-11.6981558473679));
#94753=CARTESIAN_POINT('Ctrl Pts',(18.9059546370801,17.1009828405817,-11.698596538687));
#94754=CARTESIAN_POINT('Ctrl Pts',(18.8669668991856,17.0979389614568,-11.7010010834842));
#94755=CARTESIAN_POINT('Ctrl Pts',(18.8351051101092,17.0961750306914,-11.7029998679537));
#94756=CARTESIAN_POINT('Ctrl Pts',(18.6400669976789,17.0897946270919,-11.7153925853025));
#94757=CARTESIAN_POINT('Ctrl Pts',(18.4768512194941,17.1033449061866,-11.7263866650558));
#94758=CARTESIAN_POINT('Ctrl Pts',(18.2021472560211,17.1585620523851,-11.7446901786636));
#94759=CARTESIAN_POINT('Ctrl Pts',(18.0895729457072,17.1910766162971,-11.7521410671031));
#94760=CARTESIAN_POINT('Ctrl Pts',(17.9668806479234,17.2378245269314,-11.7601581549207));
#94761=CARTESIAN_POINT('Ctrl Pts',(17.9535675697509,17.2430521385401,-11.7610269113944));
#94762=CARTESIAN_POINT('Ctrl Pts',(17.9324669831045,17.2515854538265,-11.7624022181774));
#94763=CARTESIAN_POINT('Ctrl Pts',(17.9246447253978,17.2548035416535,-11.7629117031755));
#94764=CARTESIAN_POINT('Ctrl Pts',(17.9108849981836,17.2605609748596,-11.7638073423756));
#94765=CARTESIAN_POINT('Ctrl Pts',(17.9049395065154,17.2630807520377,-11.7641941539084));
#94766=CARTESIAN_POINT('Ctrl Pts',(17.8935303125682,17.2679778163649,-11.7649361045598));
#94767=CARTESIAN_POINT('Ctrl Pts',(17.8880649432119,17.2703510409135,-11.7652913774634));
#94768=CARTESIAN_POINT('Ctrl Pts',(17.8736608244107,17.2766781458925,-11.7662273665438));
#94769=CARTESIAN_POINT('Ctrl Pts',(17.8647392445906,17.2806709409273,-11.7668067473283));
#94770=CARTESIAN_POINT('Ctrl Pts',(17.8317010538587,17.2957324672595,-11.7689512898718));
#94771=CARTESIAN_POINT('Ctrl Pts',(17.8077649211115,17.3071928191867,-11.7705029649683));
#94772=CARTESIAN_POINT('Ctrl Pts',(17.7489473058214,17.3367259996946,-11.7743156033247));
#94773=CARTESIAN_POINT('Ctrl Pts',(17.7143408393757,17.3553256488277,-11.7765585052556));
#94774=CARTESIAN_POINT('Ctrl Pts',(17.5863822676452,17.4287596349442,-11.7848823970765));
#94775=CARTESIAN_POINT('Ctrl Pts',(17.4967606761279,17.4897655030613,-11.7907660869569));
#94776=CARTESIAN_POINT('Ctrl Pts',(17.3058049039953,17.6424022672289,-11.8040416132686));
#94777=CARTESIAN_POINT('Ctrl Pts',(17.2078836658889,17.7375011907802,-11.8113988810374));
#94778=CARTESIAN_POINT('Ctrl Pts',(17.1096883072435,17.8532282409597,-11.8202986671002));
#94779=CARTESIAN_POINT('Ctrl Pts',(17.0997220691599,17.8652406464747,-11.8212220557389));
#94780=CARTESIAN_POINT('Ctrl Pts',(17.0862500246481,17.881848991758,-11.8224999145189));
#94781=CARTESIAN_POINT('Ctrl Pts',(17.0826285856442,17.8863510525239,-11.8228464237323));
#94782=CARTESIAN_POINT('Ctrl Pts',(17.0769000683556,17.8935325675376,-11.8233994497365));
#94783=CARTESIAN_POINT('Ctrl Pts',(17.0747809227125,17.896202421572,-11.8236051096339));
#94784=CARTESIAN_POINT('Ctrl Pts',(17.0704149017352,17.9017304179976,-11.824031090084));
#94785=CARTESIAN_POINT('Ctrl Pts',(17.0681689443317,17.904589225887,-11.8242514755533));
#94786=CARTESIAN_POINT('Ctrl Pts',(17.0628304824508,17.911420534078,-11.8247782891491));
#94787=CARTESIAN_POINT('Ctrl Pts',(17.0597447723599,17.9153982957134,-11.8250851940471));
#94788=CARTESIAN_POINT('Ctrl Pts',(17.049365876394,17.9288766354773,-11.8261255129335));
#94789=CARTESIAN_POINT('Ctrl Pts',(17.0421392928358,17.9384278862813,-11.8268633810667));
#94790=CARTESIAN_POINT('Ctrl Pts',(16.9597880216623,18.0492114749439,-11.8354243973394));
#94791=CARTESIAN_POINT('Ctrl Pts',(16.8937765996098,18.1568880964307,-11.8437552150637));
#94792=CARTESIAN_POINT('Ctrl Pts',(16.8040373419541,18.3376845881892,-11.8570939358174));
#94793=CARTESIAN_POINT('Ctrl Pts',(16.7740037944131,18.4073511308399,-11.8620971063111));
#94794=CARTESIAN_POINT('Ctrl Pts',(16.7469837870813,18.4806160275211,-11.8671696042913));
#94795=CARTESIAN_POINT('Ctrl Pts',(16.7461998925523,18.4827521642303,-11.8673173404412));
#94796=CARTESIAN_POINT('Ctrl Pts',(16.745419450367,18.4848895417216,-11.8674650022761));
#94797=CARTESIAN_POINT('Ctrl Pts',(16.7454194497538,18.4848895434008,-11.642549296791));
#94798=CARTESIAN_POINT('Ctrl Pts',(16.7537303157283,18.4621287825794,-11.6410530257533));
#94799=CARTESIAN_POINT('Ctrl Pts',(16.7624319238914,18.4395107822216,-11.6395695084242));
#94800=CARTESIAN_POINT('Ctrl Pts',(16.775684223823,18.4067540355932,-11.6374251889696));
#94801=CARTESIAN_POINT('Ctrl Pts',(16.7799287754304,18.3964952994903,-11.636754235569));
#94802=CARTESIAN_POINT('Ctrl Pts',(16.7869663593863,18.3798577254545,-11.6356669465138));
#94803=CARTESIAN_POINT('Ctrl Pts',(16.7897104679755,18.3734585409185,-11.6352489590199));
#94804=CARTESIAN_POINT('Ctrl Pts',(16.7950506416844,18.3611730935298,-11.6344468462473));
#94805=CARTESIAN_POINT('Ctrl Pts',(16.7976420614972,18.3552849069457,-11.6340625679936));
#94806=CARTESIAN_POINT('Ctrl Pts',(16.8036402809634,18.3418226152657,-11.63318430541));
#94807=CARTESIAN_POINT('Ctrl Pts',(16.8070649042254,18.334256530857,-11.6326909381855));
#94808=CARTESIAN_POINT('Ctrl Pts',(16.8162885431216,18.3141936893783,-11.6313831862252));
#94809=CARTESIAN_POINT('Ctrl Pts',(16.82216522995,18.3017329237105,-11.6305714802213));
#94810=CARTESIAN_POINT('Ctrl Pts',(16.8683721768321,18.2061858018263,-11.6243495950424));
#94811=CARTESIAN_POINT('Ctrl Pts',(16.9139813992593,18.1257562142081,-11.619130978086));
#94812=CARTESIAN_POINT('Ctrl Pts',(17.041917556151,17.9310313317199,-11.6062461808229));
#94813=CARTESIAN_POINT('Ctrl Pts',(17.1306448023584,17.8214991450386,-11.5987713230542));
#94814=CARTESIAN_POINT('Ctrl Pts',(17.2668063055862,17.6839661268175,-11.588061457965));
#94815=CARTESIAN_POINT('Ctrl Pts',(17.3054348652333,17.6477691538067,-11.5850901223378));
#94816=CARTESIAN_POINT('Ctrl Pts',(17.3592463171664,17.6010065272359,-11.5809739587186));
#94817=CARTESIAN_POINT('Ctrl Pts',(17.3732725095626,17.5891346168386,-11.5799030318111));
#94818=CARTESIAN_POINT('Ctrl Pts',(17.3942177790491,17.571869284245,-11.5783036650403));
#94819=CARTESIAN_POINT('Ctrl Pts',(17.4010190524951,17.5663335624578,-11.5777843004343));
#94820=CARTESIAN_POINT('Ctrl Pts',(17.4133338152716,17.5564368420864,-11.5768434634185));
#94821=CARTESIAN_POINT('Ctrl Pts',(17.4188350463919,17.5520607133902,-11.5764230156726));
#94822=CARTESIAN_POINT('Ctrl Pts',(17.4275540980235,17.5451954933169,-11.575756204837));
#94823=CARTESIAN_POINT('Ctrl Pts',(17.4307575301666,17.5426880946719,-11.5755111232871));
#94824=CARTESIAN_POINT('Ctrl Pts',(17.4339774662751,17.5401827113813,-11.5752646653457));
#94825=CARTESIAN_POINT('Ctrl Pts',(17.4339867942605,17.5401754535432,-11.5752639513691));
#94826=CARTESIAN_POINT('Ctrl Pts',(17.4340054865226,17.5401609098811,-11.5752625206361));
#94827=CARTESIAN_POINT('Ctrl Pts',(17.434014850249,17.5401536244862,-11.5752618039219));
#94828=CARTESIAN_POINT('Ctrl Pts',(17.434033613905,17.5401390257819,-11.5752603677205));
#94829=CARTESIAN_POINT('Ctrl Pts',(17.43404301422,17.5401317121737,-11.5752596482038));
#94830=CARTESIAN_POINT('Ctrl Pts',(17.4340618514356,17.5401170567482,-11.5752582063681));
#94831=CARTESIAN_POINT('Ctrl Pts',(17.4340712881365,17.5401097150872,-11.5752574840644));
#94832=CARTESIAN_POINT('Ctrl Pts',(17.4340908542789,17.540094493086,-11.5752559864312));
#94833=CARTESIAN_POINT('Ctrl Pts',(17.434100984293,17.5400866123199,-11.5752552110577));
#94834=CARTESIAN_POINT('Ctrl Pts',(17.4341214209354,17.5400707136867,-11.5752536467901));
#94835=CARTESIAN_POINT('Ctrl Pts',(17.4341317269927,17.5400626962691,-11.5752528579396));
#94836=CARTESIAN_POINT('Ctrl Pts',(17.434152519508,17.5400465214031,-11.575251266428));
#94837=CARTESIAN_POINT('Ctrl Pts',(17.4341630058967,17.540038364014,-11.5752504637721));
#94838=CARTESIAN_POINT('Ctrl Pts',(17.4341841625331,17.5400219065311,-11.5752488443848));
#94839=CARTESIAN_POINT('Ctrl Pts',(17.4341948330354,17.5400136062448,-11.5752480276338));
#94840=CARTESIAN_POINT('Ctrl Pts',(17.4342163619203,17.5399968598565,-11.5752463797486));
#94841=CARTESIAN_POINT('Ctrl Pts',(17.4342272202797,17.5399884137783,-11.5752455486159));
#94842=CARTESIAN_POINT('Ctrl Pts',(17.4342491291808,17.5399713724772,-11.5752438716378));
#94843=CARTESIAN_POINT('Ctrl Pts',(17.4342601794598,17.5399627774648,-11.5752430258124));
#94844=CARTESIAN_POINT('Ctrl Pts',(17.4342824761245,17.5399454352613,-11.5752413191482));
#94845=CARTESIAN_POINT('Ctrl Pts',(17.43429372272,17.5399366879134,-11.5752404582932));
#94846=CARTESIAN_POINT('Ctrl Pts',(17.4343164162529,17.5399190377637,-11.5752387212457));
#94847=CARTESIAN_POINT('Ctrl Pts',(17.4343278632199,17.5399101349456,-11.5752378450508));
#94848=CARTESIAN_POINT('Ctrl Pts',(17.4343509618229,17.5398921705099,-11.5752360769918));
#94849=CARTESIAN_POINT('Ctrl Pts',(17.4343626136718,17.5398831087336,-11.5752351851114));
#94850=CARTESIAN_POINT('Ctrl Pts',(17.434386126887,17.5398648226317,-11.5752333853103));
#94851=CARTESIAN_POINT('Ctrl Pts',(17.4343979878672,17.5398555986133,-11.5752324774191));
#94852=CARTESIAN_POINT('Ctrl Pts',(17.434421923896,17.5398369845094,-11.5752306452478));
#94853=CARTESIAN_POINT('Ctrl Pts',(17.434433998984,17.5398275944005,-11.5752297209646));
#94854=CARTESIAN_POINT('Ctrl Pts',(17.4344583676632,17.5398086446891,-11.5752278556698));
#94855=CARTESIAN_POINT('Ctrl Pts',(17.4344706615746,17.5397990848452,-11.5752269146336));
#94856=CARTESIAN_POINT('Ctrl Pts',(17.4344954730773,17.5397797916615,-11.5752250154361));
#94857=CARTESIAN_POINT('Ctrl Pts',(17.4345079904292,17.5397700585159,-11.5752240572932));
#94858=CARTESIAN_POINT('Ctrl Pts',(17.4345332538001,17.5397504148748,-11.5752221235005));
#94859=CARTESIAN_POINT('Ctrl Pts',(17.4345459999316,17.5397405043002,-11.575221147842));
#94860=CARTESIAN_POINT('Ctrl Pts',(17.437250611522,17.5376376213878,-11.5750141217284));
#94861=CARTESIAN_POINT('Ctrl Pts',(17.4399474717246,17.5355512003818,-11.5748076050558));
#94862=CARTESIAN_POINT('Ctrl Pts',(17.4462709869107,17.530683399605,-11.5743231848071));
#94863=CARTESIAN_POINT('Ctrl Pts',(17.4499016039276,17.5279072524029,-11.5740449174992));
#94864=CARTESIAN_POINT('Ctrl Pts',(17.4610616695905,17.5194308488903,-11.5731892055801));
#94865=CARTESIAN_POINT('Ctrl Pts',(17.468620175123,17.5137692916967,-11.5726091579254));
#94866=CARTESIAN_POINT('Ctrl Pts',(17.5754084836177,17.4348913575707,-11.5644102390713));
#94867=CARTESIAN_POINT('Ctrl Pts',(17.6808018981422,17.3704394858355,-11.5562848639047));
#94868=CARTESIAN_POINT('Ctrl Pts',(17.8857840624119,17.2684808440113,-11.5411575016869));
#94869=CARTESIAN_POINT('Ctrl Pts',(17.9837751780056,17.2285729770792,-11.5341809049508));
#94870=CARTESIAN_POINT('Ctrl Pts',(18.1555570656964,17.1731846035542,-11.5225856324242));
#94871=CARTESIAN_POINT('Ctrl Pts',(18.2279451053839,17.1540123016869,-11.5178784450629));
#94872=CARTESIAN_POINT('Ctrl Pts',(18.3195866473613,17.1348730200115,-11.5121434907082));
#94873=CARTESIAN_POINT('Ctrl Pts',(18.338020080335,17.1312784795129,-11.5110008996551));
#94874=CARTESIAN_POINT('Ctrl Pts',(18.3649114913913,17.126405132787,-11.5093495386187));
#94875=CARTESIAN_POINT('Ctrl Pts',(18.3733328529419,17.1249316166578,-11.5088345946421));
#94876=CARTESIAN_POINT('Ctrl Pts',(18.3881215259821,17.1224362200008,-11.5079340935157));
#94877=CARTESIAN_POINT('Ctrl Pts',(18.3944849675306,17.1213923511654,-11.5075478422133));
#94878=CARTESIAN_POINT('Ctrl Pts',(18.4068564931693,17.1194209119807,-11.5067992546602));
#94879=CARTESIAN_POINT('Ctrl Pts',(18.4128639921794,17.1184901144396,-11.5064368195371));
#94880=CARTESIAN_POINT('Ctrl Pts',(18.4272443835318,17.1163254148662,-11.5055717660214));
#94881=CARTESIAN_POINT('Ctrl Pts',(18.4356208709167,17.1151158132358,-11.5050699199557));
#94882=CARTESIAN_POINT('Ctrl Pts',(18.4659300130887,17.1109244288998,-11.5032612523006));
#94883=CARTESIAN_POINT('Ctrl Pts',(18.4879023268843,17.1082363632617,-11.5019636897966));
#94884=CARTESIAN_POINT('Ctrl Pts',(18.6941992808494,17.0862762480149,-11.4898979823811));
#94885=CARTESIAN_POINT('Ctrl Pts',(18.8802578409069,17.090941085481,-11.4799835944544));
#94886=CARTESIAN_POINT('Ctrl Pts',(19.1426782767497,17.1322693759548,-11.4655024263769));
#94887=CARTESIAN_POINT('Ctrl Pts',(19.2212307941875,17.1492669720571,-11.4610863327069));
#94888=CARTESIAN_POINT('Ctrl Pts',(19.3333901630184,17.1803050707585,-11.454429905064));
#94889=CARTESIAN_POINT('Ctrl Pts',(19.3679052646057,17.1908133183191,-11.4523315833809));
#94890=CARTESIAN_POINT('Ctrl Pts',(19.409219946611,17.2045546830729,-11.4497404917154));
#94891=CARTESIAN_POINT('Ctrl Pts',(19.4162945803703,17.2069493798944,-11.4492939543135));
#94892=CARTESIAN_POINT('Ctrl Pts',(19.4272894743913,17.210736015001,-11.4485953252124));
#94893=CARTESIAN_POINT('Ctrl Pts',(19.4312186348412,17.2121021838192,-11.4483447328549));
#94894=CARTESIAN_POINT('Ctrl Pts',(19.4385082998727,17.2146609078947,-11.4478780447719));
#94895=CARTESIAN_POINT('Ctrl Pts',(19.4418698272535,17.2158503759576,-11.4476621328499));
#94896=CARTESIAN_POINT('Ctrl Pts',(19.4494759398482,17.2185634220459,-11.4471719970456));
#94897=CARTESIAN_POINT('Ctrl Pts',(19.4537186499034,17.2200920659705,-11.4468974759139));
#94898=CARTESIAN_POINT('Ctrl Pts',(19.4646596249247,17.2240736308564,-11.4461867090372));
#94899=CARTESIAN_POINT('Ctrl Pts',(19.4713503717001,17.2265468486405,-11.4457492975838));
#94900=CARTESIAN_POINT('Ctrl Pts',(19.5123412425618,17.2419349410125,-11.4430531143187));
#94901=CARTESIAN_POINT('Ctrl Pts',(19.5463114948161,17.2557041250254,-11.4407481931253));
#94902=CARTESIAN_POINT('Ctrl Pts',(19.7361891263442,17.338469255174,-11.4275297172256));
#94903=CARTESIAN_POINT('Ctrl Pts',(19.8836712324236,17.4252190568367,-11.4160261126721));
#94904=CARTESIAN_POINT('Ctrl Pts',(20.0949859578043,17.5866501800109,-11.3987444948252));
#94905=CARTESIAN_POINT('Ctrl Pts',(20.1668205443087,17.6496465295991,-11.3926814966654));
#94906=CARTESIAN_POINT('Ctrl Pts',(20.2492640454183,17.7324460840374,-11.3855042061676));
#94907=CARTESIAN_POINT('Ctrl Pts',(20.2641306937055,17.7478366725905,-11.3842000039093));
#94908=CARTESIAN_POINT('Ctrl Pts',(20.2849231306298,17.7700254567663,-11.3823609872685));
#94909=CARTESIAN_POINT('Ctrl Pts',(20.2910423941322,17.7766398018038,-11.381817860106));
#94910=CARTESIAN_POINT('Ctrl Pts',(20.3015207911573,17.7881120337705,-11.3808844548083));
#94911=CARTESIAN_POINT('Ctrl Pts',(20.3058999963008,17.7929513413632,-11.380493325479));
#94912=CARTESIAN_POINT('Ctrl Pts',(20.3142383720796,17.8022518809185,-11.3797465565772));
#94913=CARTESIAN_POINT('Ctrl Pts',(20.3182011981886,17.8067097378434,-11.379390764956));
#94914=CARTESIAN_POINT('Ctrl Pts',(20.3284490254618,17.8183362952035,-11.3784683300911));
#94915=CARTESIAN_POINT('Ctrl Pts',(20.3347045810452,17.825530859891,-11.3779029180621));
#94916=CARTESIAN_POINT('Ctrl Pts',(20.355829665661,17.8501610583487,-11.375985266427));
#94917=CARTESIAN_POINT('Ctrl Pts',(20.3704649459568,17.8677961321829,-11.3746426438942));
#94918=CARTESIAN_POINT('Ctrl Pts',(20.4953050086257,18.0232945841486,-11.3630542855609));
#94919=CARTESIAN_POINT('Ctrl Pts',(20.5881539763528,18.1741976220399,-11.3535696039358));
#94920=CARTESIAN_POINT('Ctrl Pts',(20.6969165631051,18.413444741087,-11.3392675806512));
#94921=CARTESIAN_POINT('Ctrl Pts',(20.7277899346988,18.494107283399,-11.3345411645067));
#94922=CARTESIAN_POINT('Ctrl Pts',(20.7649367519452,18.612333223203,-11.3274644531751));
#94923=CARTESIAN_POINT('Ctrl Pts',(20.7752597745061,18.6485374331556,-11.3252775754328));
#94924=CARTESIAN_POINT('Ctrl Pts',(20.7864902979372,18.6923192200176,-11.3225882826959));
#94925=CARTESIAN_POINT('Ctrl Pts',(20.7883297695293,18.6996533770857,-11.3221362898946));
#94926=CARTESIAN_POINT('Ctrl Pts',(20.7911250362954,18.7110569455564,-11.3214309675287));
#94927=CARTESIAN_POINT('Ctrl Pts',(20.7921081565871,18.7151196840608,-11.3211791841287));
#94928=CARTESIAN_POINT('Ctrl Pts',(20.7939072000034,18.7226517335949,-11.3207114257733));
#94929=CARTESIAN_POINT('Ctrl Pts',(20.7947263971961,18.7261202033062,-11.320495641889));
#94930=CARTESIAN_POINT('Ctrl Pts',(20.7965562803961,18.7339563041672,-11.3200072733806));
#94931=CARTESIAN_POINT('Ctrl Pts',(20.7975618477738,18.7383250619169,-11.3197344006999));
#94932=CARTESIAN_POINT('Ctrl Pts',(20.8004823201187,18.7512002102937,-11.318928523378));
#94933=CARTESIAN_POINT('Ctrl Pts',(20.8023585299626,18.7597151548073,-11.318393382518));
#94934=CARTESIAN_POINT('Ctrl Pts',(20.8153373852477,18.8203996581062,-11.3145652512978));
#94935=CARTESIAN_POINT('Ctrl Pts',(20.8245165545187,18.8729564556639,-11.3111752227075));
#94936=CARTESIAN_POINT('Ctrl Pts',(20.834092808793,18.9433912930584,-11.3065812275964));
#94937=CARTESIAN_POINT('Ctrl Pts',(20.8362632431785,18.9610130860804,-11.3054276363247));
#94938=CARTESIAN_POINT('Ctrl Pts',(20.8435209819836,19.0267434879935,-11.301113365274));
#94939=CARTESIAN_POINT('Ctrl Pts',(20.8471803864982,19.074993919207,-11.2979242541586));
#94940=CARTESIAN_POINT('Ctrl Pts',(20.8537136925562,19.232613474925,-11.287503402309));
#94941=CARTESIAN_POINT('Ctrl Pts',(20.8497671240275,19.3420962371424,-11.2802707081327));
#94942=CARTESIAN_POINT('Ctrl Pts',(20.8311348064382,19.50553451864,-11.2696972801468));
#94943=CARTESIAN_POINT('Ctrl Pts',(20.8227584661425,19.5600184381416,-11.2662081684419));
#94944=CARTESIAN_POINT('Ctrl Pts',(20.8057330654138,19.647792627328,-11.2606506343006));
#94945=CARTESIAN_POINT('Ctrl Pts',(20.7983833242257,19.6813056459291,-11.2585437737274));
#94946=CARTESIAN_POINT('Ctrl Pts',(20.7876507349811,19.7251249658662,-11.2558072506868));
#94947=CARTESIAN_POINT('Ctrl Pts',(20.7849990549321,19.7356033790098,-11.2551542470154));
#94948=CARTESIAN_POINT('Ctrl Pts',(20.780523766397,19.7527352268918,-11.2540887483289));
#94949=CARTESIAN_POINT('Ctrl Pts',(20.7787477045698,19.7594007739709,-11.2536747238756));
#94950=CARTESIAN_POINT('Ctrl Pts',(20.7752461823634,19.7722884396261,-11.252875208879));
#94951=CARTESIAN_POINT('Ctrl Pts',(20.7735247749198,19.7785115711466,-11.2524895919934));
#94952=CARTESIAN_POINT('Ctrl Pts',(20.7694836224523,19.7928650218427,-11.2516011714039));
#94953=CARTESIAN_POINT('Ctrl Pts',(20.7671435796942,19.800989549422,-11.2510990337664));
#94954=CARTESIAN_POINT('Ctrl Pts',(20.7607177169652,19.8228075626819,-11.2497524230434));
#94955=CARTESIAN_POINT('Ctrl Pts',(20.7565417741932,19.8364742077569,-11.2489108913707));
#94956=CARTESIAN_POINT('Ctrl Pts',(20.716956134961,19.9614829877329,-11.2412290520041));
#94957=CARTESIAN_POINT('Ctrl Pts',(20.6725224675458,20.0697640270365,-11.2347054284596));
#94958=CARTESIAN_POINT('Ctrl Pts',(20.5453373570925,20.3188107702178,-11.2193964995653));
#94959=CARTESIAN_POINT('Ctrl Pts',(20.4548364695359,20.4547434210946,-11.2107943962046));
#94960=CARTESIAN_POINT('Ctrl Pts',(20.3286974594612,20.6037249329809,-11.1995852224268));
#94961=CARTESIAN_POINT('Ctrl Pts',(20.307156146158,20.6280117168745,-11.1976918670049));
#94962=CARTESIAN_POINT('Ctrl Pts',(20.2801414461308,20.657094047366,-11.1953284605241));
#94963=CARTESIAN_POINT('Ctrl Pts',(20.2751894210102,20.6623705696336,-11.1948956644689));
#94964=CARTESIAN_POINT('Ctrl Pts',(20.2673832948863,20.6706032182577,-11.1942139092523));
#94965=CARTESIAN_POINT('Ctrl Pts',(20.264547419957,20.6735766572689,-11.1939663342924));
#94966=CARTESIAN_POINT('Ctrl Pts',(20.2592301031966,20.6791195086974,-11.1935022677287));
#94967=CARTESIAN_POINT('Ctrl Pts',(20.2567508088608,20.6816909032737,-11.1932859412293));
#94968=CARTESIAN_POINT('Ctrl Pts',(20.2510759262806,20.6875468614301,-11.192790918483));
#94969=CARTESIAN_POINT('Ctrl Pts',(20.2478761845755,20.690827319981,-11.192511899994));
#94970=CARTESIAN_POINT('Ctrl Pts',(20.2380064594572,20.7008805082811,-11.1916516277518));
#94971=CARTESIAN_POINT('Ctrl Pts',(20.2313015975227,20.7076186145295,-11.1910677312704));
#94972=CARTESIAN_POINT('Ctrl Pts',(20.1699489746241,20.7684505026365,-11.1857314418229));
#94973=CARTESIAN_POINT('Ctrl Pts',(20.1124428459899,20.8195689972922,-11.180778892149));
#94974=CARTESIAN_POINT('Ctrl Pts',(19.9424160350423,20.9548861742614,-11.1665611288904));
#94975=CARTESIAN_POINT('Ctrl Pts',(19.8241015915385,21.0311899909556,-11.1571727597118));
#94976=CARTESIAN_POINT('Ctrl Pts',(19.643972914943,21.1234525820152,-11.1440958692517));
#94977=CARTESIAN_POINT('Ctrl Pts',(19.5876273275295,21.1492587823443,-11.1401556591136));
#94978=CARTESIAN_POINT('Ctrl Pts',(19.4956516973328,21.1865930970191,-11.1339701548899));
#94979=CARTESIAN_POINT('Ctrl Pts',(19.4607101614286,21.1997116463354,-11.1316747066117));
#94980=CARTESIAN_POINT('Ctrl Pts',(19.4149083637398,21.2155390790436,-11.1287338360591));
#94981=CARTESIAN_POINT('Ctrl Pts',(19.4043497533942,21.2190947026425,-11.128060492888));
#94982=CARTESIAN_POINT('Ctrl Pts',(19.3871393373693,21.2247394579314,-11.1269703016982));
#94983=CARTESIAN_POINT('Ctrl Pts',(19.3805045170662,21.2268793390655,-11.1265517852828));
#94984=CARTESIAN_POINT('Ctrl Pts',(19.3677296186385,21.2309299788452,-11.1257493054663));
#94985=CARTESIAN_POINT('Ctrl Pts',(19.361591177199,21.2328456085191,-11.1253651856213));
#94986=CARTESIAN_POINT('Ctrl Pts',(19.3475229199278,21.2371656614455,-11.1244881821812));
#94987=CARTESIAN_POINT('Ctrl Pts',(19.3395874926901,21.2395515651752,-11.1239959096082));
#94988=CARTESIAN_POINT('Ctrl Pts',(19.318483101908,21.2457620366185,-11.1226929811458));
#94989=CARTESIAN_POINT('Ctrl Pts',(19.3052905030726,21.2495053878711,-11.1218849722252));
#94990=CARTESIAN_POINT('Ctrl Pts',(19.2053492726639,21.2768169150562,-11.1158107534666));
#94991=CARTESIAN_POINT('Ctrl Pts',(19.1172093912315,21.2949681044395,-11.110725416215));
#94992=CARTESIAN_POINT('Ctrl Pts',(18.8901023292052,21.3268355391554,-11.0980275873393));
#94993=CARTESIAN_POINT('Ctrl Pts',(18.7504613617129,21.3325219043984,-11.090611099825));
#94994=CARTESIAN_POINT('Ctrl Pts',(18.5557493997068,21.3212155361911,-11.0798403700041));
#94995=CARTESIAN_POINT('Ctrl Pts',(18.5003726130913,21.3158040923634,-11.0767245883081));
#94996=CARTESIAN_POINT('Ctrl Pts',(18.4169477110041,21.3043190448105,-11.0718677501062));
#94997=CARTESIAN_POINT('Ctrl Pts',(18.3887016049855,21.2998455217526,-11.0701946530488));
#94998=CARTESIAN_POINT('Ctrl Pts',(18.3537129044125,21.2935751036294,-11.0680768213649));
#94999=CARTESIAN_POINT('Ctrl Pts',(18.3468756188353,21.2923149804333,-11.0676608022763));
#95000=CARTESIAN_POINT('Ctrl Pts',(18.3360691591824,21.2902682410911,-11.0669996716658));
#95001=CARTESIAN_POINT('Ctrl Pts',(18.3320957506295,21.2895038720654,-11.0667558091685));
#95002=CARTESIAN_POINT('Ctrl Pts',(18.3246080495659,21.2880411813226,-11.0662947629143));
#95003=CARTESIAN_POINT('Ctrl Pts',(18.321093329879,21.2873453275034,-11.0660777205625));
#95004=CARTESIAN_POINT('Ctrl Pts',(18.3130642432425,21.2857345144377,-11.0655804829601));
#95005=CARTESIAN_POINT('Ctrl Pts',(18.3085510904496,21.28481374312,-11.0652999594098));
#95006=CARTESIAN_POINT('Ctrl Pts',(18.2965825301838,21.28233120955,-11.0645533721343));
#95007=CARTESIAN_POINT('Ctrl Pts',(18.2891325644589,21.2807439414929,-11.0640859085787));
#95008=CARTESIAN_POINT('Ctrl Pts',(18.2371681829844,21.2693790433653,-11.0608069054905));
#95009=CARTESIAN_POINT('Ctrl Pts',(18.1929744732382,21.2582070830349,-11.0579240295177));
#95010=CARTESIAN_POINT('Ctrl Pts',(18.1432661850623,21.2439191858732,-11.0545994519143));
#95011=CARTESIAN_POINT('Ctrl Pts',(18.1373603453429,21.2421937321747,-11.0542031267414));
#95012=CARTESIAN_POINT('Ctrl Pts',(18.1271215696667,21.2391538581471,-11.0535138048808));
#95013=CARTESIAN_POINT('Ctrl Pts',(18.1227851482519,21.2378512293834,-11.0532211618298));
#95014=CARTESIAN_POINT('Ctrl Pts',(18.0946964125259,21.2293152423388,-11.051321217674));
#95015=CARTESIAN_POINT('Ctrl Pts',(18.0710692840745,21.2216785667851,-11.0497027582124));
#95016=CARTESIAN_POINT('Ctrl Pts',(18.0104645888448,21.2009058054057,-11.0455069403706));
#95017=CARTESIAN_POINT('Ctrl Pts',(17.9737081440305,21.1871540401087,-11.0429190833576));
#95018=CARTESIAN_POINT('Ctrl Pts',(17.8360959829326,21.1312610353945,-11.033107423052));
#95019=CARTESIAN_POINT('Ctrl Pts',(17.73816525062,21.0823499640679,-11.0258810809025));
#95020=CARTESIAN_POINT('Ctrl Pts',(17.5972933620927,20.9977880025836,-11.0153209921847));
#95021=CARTESIAN_POINT('Ctrl Pts',(17.5512600005505,20.9676559871331,-11.011838823645));
#95022=CARTESIAN_POINT('Ctrl Pts',(17.4785407936619,20.9159001720591,-11.0062910547081));
#95023=CARTESIAN_POINT('Ctrl Pts',(17.4511174496957,20.8953618949057,-11.004187184367));
#95024=CARTESIAN_POINT('Ctrl Pts',(17.4157162759546,20.867482334929,-11.0014539183714));
#95025=CARTESIAN_POINT('Ctrl Pts',(17.4072804091997,20.8607335655119,-11.000801250945));
#95026=CARTESIAN_POINT('Ctrl Pts',(17.3935441125473,20.8495708955155,-10.9997361602729));
#95027=CARTESIAN_POINT('Ctrl Pts',(17.3882130165235,20.8451952033627,-10.9993222098493));
#95028=CARTESIAN_POINT('Ctrl Pts',(17.3779321895364,20.8366724114031,-10.9985227406241));
#95029=CARTESIAN_POINT('Ctrl Pts',(17.3729798688147,20.832528568884,-10.9981370959896));
#95030=CARTESIAN_POINT('Ctrl Pts',(17.3615850302393,20.8229049854075,-10.9972484725364));
#95031=CARTESIAN_POINT('Ctrl Pts',(17.3551562083799,20.8174091423676,-10.9967461607605));
#95032=CARTESIAN_POINT('Ctrl Pts',(17.3379467302571,20.8025177534045,-10.9953987745792));
#95033=CARTESIAN_POINT('Ctrl Pts',(17.3272279334716,20.7930511556645,-10.9945566469522));
#95034=CARTESIAN_POINT('Ctrl Pts',(17.2292160350151,20.7047054740705,-10.9868265727809));
#95035=CARTESIAN_POINT('Ctrl Pts',(17.1485393427668,20.6187821816334,-10.9802600960631));
#95036=CARTESIAN_POINT('Ctrl Pts',(16.9737389830966,20.3984080756374,-10.9648655756459));
#95037=CARTESIAN_POINT('Ctrl Pts',(16.8872806450838,20.2588893352109,-10.9562204814614));
#95038=CARTESIAN_POINT('Ctrl Pts',(16.8045807840989,20.0827747064493,-10.9450299597384));
#95039=CARTESIAN_POINT('Ctrl Pts',(16.7920251373158,20.0544352694506,-10.9432200695927));
#95040=CARTESIAN_POINT('Ctrl Pts',(16.7773512455881,20.0192484369357,-10.9409495898788));
#95041=CARTESIAN_POINT('Ctrl Pts',(16.7746389808925,20.0126509698459,-10.9405228850975));
#95042=CARTESIAN_POINT('Ctrl Pts',(16.7704255502863,20.0022528534787,-10.9398486156054));
#95043=CARTESIAN_POINT('Ctrl Pts',(16.7689019287751,19.9984612800167,-10.939602385333));
#95044=CARTESIAN_POINT('Ctrl Pts',(16.7660657187978,19.9913438021033,-10.9391394410906));
#95045=CARTESIAN_POINT('Ctrl Pts',(16.7647505755529,19.9880189754749,-10.938922883739));
#95046=CARTESIAN_POINT('Ctrl Pts',(16.7617562475997,19.9803925555127,-10.9384254733093));
#95047=CARTESIAN_POINT('Ctrl Pts',(16.7600827149697,19.976088801569,-10.9381442859707));
#95048=CARTESIAN_POINT('Ctrl Pts',(16.7549425689509,19.9627409778176,-10.9372707693427));
#95049=CARTESIAN_POINT('Ctrl Pts',(16.7515239901557,19.9536787160888,-10.9366756803647));
#95050=CARTESIAN_POINT('Ctrl Pts',(16.7114754925612,19.845267729969,-10.9295352472));
#95051=CARTESIAN_POINT('Ctrl Pts',(16.6822910932671,19.7433402800352,-10.9226144786129));
#95052=CARTESIAN_POINT('Ctrl Pts',(16.6317924910195,19.4991187845646,-10.9061647804671));
#95053=CARTESIAN_POINT('Ctrl Pts',(16.6170952312495,19.3559559289461,-10.8966461787978));
#95054=CARTESIAN_POINT('Ctrl Pts',(16.616959535722,19.1504033908249,-10.8835935562426));
#95055=CARTESIAN_POINT('Ctrl Pts',(16.6196417426167,19.08843294355,-10.8797325138413));
#95056=CARTESIAN_POINT('Ctrl Pts',(16.626121996496,19.0142932853695,-10.875199725925));
#95057=CARTESIAN_POINT('Ctrl Pts',(16.6273121374375,19.0019319027675,-10.8744468144049));
#95058=CARTESIAN_POINT('Ctrl Pts',(16.6294460867381,18.9816409454271,-10.8732154433114));
#95059=CARTESIAN_POINT('Ctrl Pts',(16.630326098969,18.9737050978484,-10.8727349879567));
#95060=CARTESIAN_POINT('Ctrl Pts',(16.631989697049,18.959440158749,-10.8718733437355));
#95061=CARTESIAN_POINT('Ctrl Pts',(16.6327570210524,18.9531093017493,-10.8714916473455));
#95062=CARTESIAN_POINT('Ctrl Pts',(16.6344530082319,18.9396267583189,-10.8706802318216));
#95063=CARTESIAN_POINT('Ctrl Pts',(16.635389633832,18.9324761411828,-10.8702507690383));
#95064=CARTESIAN_POINT('Ctrl Pts',(16.6380125543847,18.9132163550913,-10.869096331034));
#95065=CARTESIAN_POINT('Ctrl Pts',(16.6397672532844,18.9011166616507,-10.8683735224932));
#95066=CARTESIAN_POINT('Ctrl Pts',(16.6490971359134,18.8404844345048,-10.8647629891558));
#95067=CARTESIAN_POINT('Ctrl Pts',(16.6582553257513,18.7922084812765,-10.8619257832645));
#95068=CARTESIAN_POINT('Ctrl Pts',(16.6889757434457,18.656288321238,-10.8540036612939));
#95069=CARTESIAN_POINT('Ctrl Pts',(16.7144720714676,18.5696443543303,-10.8490363878053));
#95070=CARTESIAN_POINT('Ctrl Pts',(16.7454194500511,18.4848895425866,-10.8441190257052));
#95071=CARTESIAN_POINT('Origin',(18.734,19.211,0.));
#95072=CARTESIAN_POINT('',(16.7454194503153,18.4848895418633,-10.0464611586511));
#95073=CARTESIAN_POINT('',(16.7460269850049,18.48512090247,-10.2662522550585));
#95074=CARTESIAN_POINT('',(16.7454194503191,18.4848895418526,0.));
#95075=CARTESIAN_POINT('',(16.6141769831468,19.2099225630115,-10.3109437209775));
#95076=CARTESIAN_POINT('Ctrl Pts',(16.746026985005,18.4851209024697,-10.2662522550585));
#95077=CARTESIAN_POINT('Ctrl Pts',(16.6804601501866,18.6593671879511,-10.2774434318084));
#95078=CARTESIAN_POINT('Ctrl Pts',(16.6235837846056,18.9018894313097,-10.2923405871147));
#95079=CARTESIAN_POINT('Ctrl Pts',(16.6137958787386,19.1485339243464,-10.307237742421));
#95080=CARTESIAN_POINT('Ctrl Pts',(16.6141769831468,19.2099225630115,-10.3109437209775));
#95081=CARTESIAN_POINT('Ctrl Pts',(16.6170002227485,19.2100288578692,-10.3093226092216));
#95082=CARTESIAN_POINT('Ctrl Pts',(16.6169204631466,19.3838973927067,-10.3205065096121));
#95083=CARTESIAN_POINT('Ctrl Pts',(16.6382591297735,19.5571243916928,-10.3322373725637));
#95084=CARTESIAN_POINT('Ctrl Pts',(16.6953904168952,19.7850075989709,-10.3474076082501));
#95085=CARTESIAN_POINT('Ctrl Pts',(16.7127857427009,19.8435407289489,-10.3512876713133));
#95086=CARTESIAN_POINT('Ctrl Pts',(16.7447265731386,19.9361507375324,-10.3573901651957));
#95087=CARTESIAN_POINT('Ctrl Pts',(16.7576771892852,19.9707373073503,-10.3596610984453));
#95088=CARTESIAN_POINT('Ctrl Pts',(16.7756892746449,20.0152582265561,-10.3625755207103));
#95089=CARTESIAN_POINT('Ctrl Pts',(16.7799328772434,20.0255145051719,-10.3632463129835));
#95090=CARTESIAN_POINT('Ctrl Pts',(16.7869692717986,20.0421490922638,-10.3643334064241));
#95091=CARTESIAN_POINT('Ctrl Pts',(16.7897131730314,20.0485477338096,-10.3647513583161));
#95092=CARTESIAN_POINT('Ctrl Pts',(16.7950532285592,20.0608328100748,-10.3655534466433));
#95093=CARTESIAN_POINT('Ctrl Pts',(16.7976447444331,20.0667211655728,-10.3659377358185));
#95094=CARTESIAN_POINT('Ctrl Pts',(16.803643604065,20.0801847771502,-10.3668160842831));
#95095=CARTESIAN_POINT('Ctrl Pts',(16.8070687834751,20.0877520070919,-10.3673095260527));
#95096=CARTESIAN_POINT('Ctrl Pts',(16.8162948647742,20.1078198951483,-10.3686176065359));
#95097=CARTESIAN_POINT('Ctrl Pts',(16.8221735008295,20.1202845321845,-10.3694295643482));
#95098=CARTESIAN_POINT('Ctrl Pts',(16.8684550180522,20.2159831237312,-10.3756613105747));
#95099=CARTESIAN_POINT('Ctrl Pts',(16.9141559267543,20.2965504389374,-10.3808888114111));
#95100=CARTESIAN_POINT('Ctrl Pts',(17.0421916993997,20.4913233443882,-10.3937778197207));
#95101=CARTESIAN_POINT('Ctrl Pts',(17.1308960704148,20.6007836880026,-10.4012490349878));
#95102=CARTESIAN_POINT('Ctrl Pts',(17.2669770060914,20.7381953313056,-10.4119516171495));
#95103=CARTESIAN_POINT('Ctrl Pts',(17.3055554878535,20.774338593815,-10.4149190303441));
#95104=CARTESIAN_POINT('Ctrl Pts',(17.3593008957968,20.8210398823636,-10.419030117648));
#95105=CARTESIAN_POINT('Ctrl Pts',(17.3733145398385,20.8329004538023,-10.4201000852955));
#95106=CARTESIAN_POINT('Ctrl Pts',(17.3942426183372,20.8501509875192,-10.4216981395917));
#95107=CARTESIAN_POINT('Ctrl Pts',(17.401039486941,20.8556829683932,-10.4222171682073));
#95108=CARTESIAN_POINT('Ctrl Pts',(17.4133468953465,20.8655735822389,-10.4231574440495));
#95109=CARTESIAN_POINT('Ctrl Pts',(17.4188451985767,20.8699473189401,-10.4235776683576));
#95110=CARTESIAN_POINT('Ctrl Pts',(17.4275606403491,20.8768096355525,-10.4242442034944));
#95111=CARTESIAN_POINT('Ctrl Pts',(17.4307634108325,20.8793164970593,-10.4244892345579));
#95112=CARTESIAN_POINT('Ctrl Pts',(17.4339826888945,20.8818213521995,-10.4247356422545));
#95113=CARTESIAN_POINT('Ctrl Pts',(17.4339920236012,20.8818286152205,-10.424736356746));
#95114=CARTESIAN_POINT('Ctrl Pts',(17.4340107290091,20.8818431690167,-10.4247377884858));
#95115=CARTESIAN_POINT('Ctrl Pts',(17.4340200996542,20.8818504597473,-10.42473850573));
#95116=CARTESIAN_POINT('Ctrl Pts',(17.4340388775657,20.881865069448,-10.4247399430233));
#95117=CARTESIAN_POINT('Ctrl Pts',(17.4340482844276,20.8818723881022,-10.4247406630415));
#95118=CARTESIAN_POINT('Ctrl Pts',(17.4340671346245,20.8818870535317,-10.4247421058715));
#95119=CARTESIAN_POINT('Ctrl Pts',(17.4340765784097,20.8818944006562,-10.4247428287178));
#95120=CARTESIAN_POINT('Ctrl Pts',(17.4340961827591,20.8819096522817,-10.4247443292762));
#95121=CARTESIAN_POINT('Ctrl Pts',(17.4341063432902,20.8819175567368,-10.4247451069859));
#95122=CARTESIAN_POINT('Ctrl Pts',(17.4341268414438,20.8819335031164,-10.4247466759625));
#95123=CARTESIAN_POINT('Ctrl Pts',(17.4341371790578,20.8819415450289,-10.4247474672289));
#95124=CARTESIAN_POINT('Ctrl Pts',(17.4341580351435,20.8819577692376,-10.4247490636072));
#95125=CARTESIAN_POINT('Ctrl Pts',(17.4341685535801,20.8819659515009,-10.4247498687165));
#95126=CARTESIAN_POINT('Ctrl Pts',(17.4341897753024,20.8819824594996,-10.4247514930866));
#95127=CARTESIAN_POINT('Ctrl Pts',(17.434200478368,20.8819907850581,-10.4247523123304));
#95128=CARTESIAN_POINT('Ctrl Pts',(17.4342220730779,20.8820075825311,-10.4247539652551));
#95129=CARTESIAN_POINT('Ctrl Pts',(17.4342329649436,20.882016054612,-10.4247547989528));
#95130=CARTESIAN_POINT('Ctrl Pts',(17.4342549414064,20.8820331483423,-10.4247564811033));
#95131=CARTESIAN_POINT('Ctrl Pts',(17.4342660258785,20.8820417698884,-10.4247573295464));
#95132=CARTESIAN_POINT('Ctrl Pts',(17.4342883914533,20.8820591655634,-10.4247590414862));
#95133=CARTESIAN_POINT('Ctrl Pts',(17.4342996730243,20.8820679400502,-10.4247599050188));
#95134=CARTESIAN_POINT('Ctrl Pts',(17.4343224374474,20.8820856452046,-10.4247616474936));
#95135=CARTESIAN_POINT('Ctrl Pts',(17.4343339199341,20.8820945755815,-10.4247625264078));
#95136=CARTESIAN_POINT('Ctrl Pts',(17.4343570904565,20.8821125958153,-10.4247642999728));
#95137=CARTESIAN_POINT('Ctrl Pts',(17.4343687787576,20.8821216858719,-10.4247651946439));
#95138=CARTESIAN_POINT('Ctrl Pts',(17.4343923656035,20.8821400290955,-10.4247670000821));
#95139=CARTESIAN_POINT('Ctrl Pts',(17.4344042638533,20.8821492820261,-10.4247679108266));
#95140=CARTESIAN_POINT('Ctrl Pts',(17.4344282753377,20.8821679546634,-10.4247697487748));
#95141=CARTESIAN_POINT('Ctrl Pts',(17.4344403884324,20.8821773742537,-10.4247706759677));
#95142=CARTESIAN_POINT('Ctrl Pts',(17.4344648343786,20.8821963838991,-10.4247725471781));
#95143=CARTESIAN_POINT('Ctrl Pts',(17.4344771670345,20.8822059737942,-10.4247734911806));
#95144=CARTESIAN_POINT('Ctrl Pts',(17.4345020565024,20.8822253274464,-10.4247753963471));
#95145=CARTESIAN_POINT('Ctrl Pts',(17.4345146139301,20.8822350916743,-10.4247763575583));
#95146=CARTESIAN_POINT('Ctrl Pts',(17.4345399581839,20.8822547980442,-10.4247782975434));
#95147=CARTESIAN_POINT('Ctrl Pts',(17.434552744946,20.8822647401279,-10.4247792763126));
#95148=CARTESIAN_POINT('Ctrl Pts',(17.4372582990783,20.8843683382574,-10.4249863747096));
#95149=CARTESIAN_POINT('Ctrl Pts',(17.4399560645314,20.8864554386411,-10.4251929608782));
#95150=CARTESIAN_POINT('Ctrl Pts',(17.4462822115505,20.8913252083239,-10.4256775831681));
#95151=CARTESIAN_POINT('Ctrl Pts',(17.4499145604095,20.8941026383864,-10.4259559835004));
#95152=CARTESIAN_POINT('Ctrl Pts',(17.4610851309162,20.9025868670852,-10.4268125018391));
#95153=CARTESIAN_POINT('Ctrl Pts',(17.4686524886779,20.9082548602956,-10.427393229884));
#95154=CARTESIAN_POINT('Ctrl Pts',(17.5750095848097,20.9868103023396,-10.4355590552967));
#95155=CARTESIAN_POINT('Ctrl Pts',(17.6799082885108,21.0510121631218,-10.4436462315541));
#95156=CARTESIAN_POINT('Ctrl Pts',(17.8838341102242,21.1526369452228,-10.4587009219142));
#95157=CARTESIAN_POINT('Ctrl Pts',(17.9812728736565,21.1924492383761,-10.4656428822374));
#95158=CARTESIAN_POINT('Ctrl Pts',(18.1337166699042,21.2418590230281,-10.4759436667052));
#95159=CARTESIAN_POINT('Ctrl Pts',(18.1868090635395,21.2568033505635,-10.4794348464486));
#95160=CARTESIAN_POINT('Ctrl Pts',(18.2737996457122,21.2776596972667,-10.4849952886683));
#95161=CARTESIAN_POINT('Ctrl Pts',(18.3073621497032,21.2848483627479,-10.4871030394444));
#95162=CARTESIAN_POINT('Ctrl Pts',(18.3517084402867,21.2932245365386,-10.4898405320932));
#95163=CARTESIAN_POINT('Ctrl Pts',(18.3623460337021,21.2951495131864,-10.4904936358572));
#95164=CARTESIAN_POINT('Ctrl Pts',(18.3797953896978,21.2981692987134,-10.4915592560542));
#95165=CARTESIAN_POINT('Ctrl Pts',(18.3865984880572,21.2993124236339,-10.4919733025979));
#95166=CARTESIAN_POINT('Ctrl Pts',(18.3997796019268,21.3014610527656,-10.492772831378));
#95167=CARTESIAN_POINT('Ctrl Pts',(18.4061568606474,21.3024706703712,-10.4931584401079));
#95168=CARTESIAN_POINT('Ctrl Pts',(18.4208944206659,21.3047347879344,-10.4940468006514));
#95169=CARTESIAN_POINT('Ctrl Pts',(18.4292578526009,21.3059684228594,-10.4945488866881));
#95170=CARTESIAN_POINT('Ctrl Pts',(18.4517745929107,21.3091520275368,-10.4958952674881));
#95171=CARTESIAN_POINT('Ctrl Pts',(18.4659407761214,21.3110088996141,-10.4967366224294));
#95172=CARTESIAN_POINT('Ctrl Pts',(18.5958916074904,21.3267061572386,-10.5044049443878));
#95173=CARTESIAN_POINT('Ctrl Pts',(18.712622761478,21.3311025274149,-10.510916559998));
#95174=CARTESIAN_POINT('Ctrl Pts',(18.99108064002,21.3185762881616,-10.5261771805903));
#95175=CARTESIAN_POINT('Ctrl Pts',(19.1516331336279,21.2927154600959,-10.5347448739599));
#95176=CARTESIAN_POINT('Ctrl Pts',(19.3396675783229,21.239783538358,-10.5459517653747));
#95177=CARTESIAN_POINT('Ctrl Pts',(19.3714734569208,21.230015397128,-10.5478910473071));
#95178=CARTESIAN_POINT('Ctrl Pts',(19.4099512067565,21.2171984258977,-10.5503055288682));
#95179=CARTESIAN_POINT('Ctrl Pts',(19.416856430259,21.2148585903524,-10.550741548787));
#95180=CARTESIAN_POINT('Ctrl Pts',(19.4276454244655,21.2111404969556,-10.5514272645558));
#95181=CARTESIAN_POINT('Ctrl Pts',(19.4315375671874,21.209786462867,-10.5516755495506));
#95182=CARTESIAN_POINT('Ctrl Pts',(19.4387944069447,21.2072381099467,-10.5521402206967));
#95183=CARTESIAN_POINT('Ctrl Pts',(19.4421600446531,21.2060466406018,-10.5523564373034));
#95184=CARTESIAN_POINT('Ctrl Pts',(19.449821827108,21.203312462588,-10.5528502539361));
#95185=CARTESIAN_POINT('Ctrl Pts',(19.4541159896977,21.2017643751152,-10.553128170088));
#95186=CARTESIAN_POINT('Ctrl Pts',(19.4672516784929,21.1969807697053,-10.5539817547056));
#95187=CARTESIAN_POINT('Ctrl Pts',(19.4760765151719,21.1937001991608,-10.5545600078046));
#95188=CARTESIAN_POINT('Ctrl Pts',(19.5526781134018,21.1646410573214,-10.5596193893968));
#95189=CARTESIAN_POINT('Ctrl Pts',(19.6191040196417,21.1354572821409,-10.5642788191431));
#95190=CARTESIAN_POINT('Ctrl Pts',(19.8068973631509,21.0411704709707,-10.5780020295135));
#95191=CARTESIAN_POINT('Ctrl Pts',(19.9235947535089,20.9675593305937,-10.5872082591452));
#95192=CARTESIAN_POINT('Ctrl Pts',(20.103958599869,20.8275174552415,-10.602012594859));
#95193=CARTESIAN_POINT('Ctrl Pts',(20.1719564835754,20.7673418928319,-10.6077623493589));
#95194=CARTESIAN_POINT('Ctrl Pts',(20.2505685235693,20.6882077023343,-10.6146100491986));
#95195=CARTESIAN_POINT('Ctrl Pts',(20.2650268232026,20.6732173565483,-10.615878929421));
#95196=CARTESIAN_POINT('Ctrl Pts',(20.2853543785955,20.6515096450945,-10.617677168591));
#95197=CARTESIAN_POINT('Ctrl Pts',(20.2914056849412,20.6449651257643,-10.6182143471985));
#95198=CARTESIAN_POINT('Ctrl Pts',(20.3018042242549,20.6335755801998,-10.619140748539));
#95199=CARTESIAN_POINT('Ctrl Pts',(20.30617074213,20.6287484001159,-10.6195307888579));
#95200=CARTESIAN_POINT('Ctrl Pts',(20.3145096746777,20.6194438197673,-10.6202776881177));
#95201=CARTESIAN_POINT('Ctrl Pts',(20.3184854937662,20.6149695674649,-10.6206346884924));
#95202=CARTESIAN_POINT('Ctrl Pts',(20.3288203889694,20.6032392085307,-10.6215650808578));
#95203=CARTESIAN_POINT('Ctrl Pts',(20.3351489772521,20.595956332947,-10.6221371984599));
#95204=CARTESIAN_POINT('Ctrl Pts',(20.3567895491851,20.5707059794782,-10.6241021168707));
#95205=CARTESIAN_POINT('Ctrl Pts',(20.3718510049027,20.5525254090591,-10.6254846366877));
#95206=CARTESIAN_POINT('Ctrl Pts',(20.4897305425364,20.4052886485305,-10.6364378418479));
#95207=CARTESIAN_POINT('Ctrl Pts',(20.5774443167171,20.2648667575945,-10.6453574776964));
#95208=CARTESIAN_POINT('Ctrl Pts',(20.70253723511,20.0002136892172,-10.6612639004333));
#95209=CARTESIAN_POINT('Ctrl Pts',(20.7465429414333,19.8800729594498,-10.6682206367713));
#95210=CARTESIAN_POINT('Ctrl Pts',(20.7825276384248,19.7451963967067,-10.6764580419348));
#95211=CARTESIAN_POINT('Ctrl Pts',(20.7855048900749,19.733646101001,-10.6771668630869));
#95212=CARTESIAN_POINT('Ctrl Pts',(20.7895976349125,19.7171942548811,-10.6781821102731));
#95213=CARTESIAN_POINT('Ctrl Pts',(20.7907935820669,19.7123126967421,-10.67848405377));
#95214=CARTESIAN_POINT('Ctrl Pts',(20.7928242986144,19.7038942219651,-10.6790060496715));
#95215=CARTESIAN_POINT('Ctrl Pts',(20.7936673735354,19.700359292192,-10.6792256252976));
#95216=CARTESIAN_POINT('Ctrl Pts',(20.7952841107707,19.6935022791095,-10.6796523355483));
#95217=CARTESIAN_POINT('Ctrl Pts',(20.796058848062,19.6901804893864,-10.679859401165));
#95218=CARTESIAN_POINT('Ctrl Pts',(20.7981269180614,19.6812154666972,-10.6804191610052));
#95219=CARTESIAN_POINT('Ctrl Pts',(20.7994051233856,19.6755688253309,-10.6807727093471));
#95220=CARTESIAN_POINT('Ctrl Pts',(20.8040603688816,19.6546046675034,-10.6820887777589));
#95221=CARTESIAN_POINT('Ctrl Pts',(20.8072902056153,19.6392554400284,-10.683059191357));
#95222=CARTESIAN_POINT('Ctrl Pts',(20.8366569416978,19.4915690978127,-10.6924524721151));
#95223=CARTESIAN_POINT('Ctrl Pts',(20.8502570013305,19.3570661317236,-10.7014189017867));
#95224=CARTESIAN_POINT('Ctrl Pts',(20.851796465475,19.0660234767047,-10.7206395247686));
#95225=CARTESIAN_POINT('Ctrl Pts',(20.8353383464365,18.9102103424607,-10.7307940198684));
#95226=CARTESIAN_POINT('Ctrl Pts',(20.7973223148153,18.7368243171045,-10.741696039587));
#95227=CARTESIAN_POINT('Ctrl Pts',(20.7924531514088,18.7161139238528,-10.7429926253305));
#95228=CARTESIAN_POINT('Ctrl Pts',(20.7850833571015,18.6867606668681,-10.7448228599915));
#95229=CARTESIAN_POINT('Ctrl Pts',(20.7828386727821,18.6780554315964,-10.7453647141445));
#95230=CARTESIAN_POINT('Ctrl Pts',(20.7788697392067,18.6630590401828,-10.7462966183727));
#95231=CARTESIAN_POINT('Ctrl Pts',(20.7771717528396,18.6567611204135,-10.746687512427));
#95232=CARTESIAN_POINT('Ctrl Pts',(20.7738642628297,18.644715251271,-10.7474342994409));
#95233=CARTESIAN_POINT('Ctrl Pts',(20.7722595064745,18.638966073731,-10.7477903422013));
#95234=CARTESIAN_POINT('Ctrl Pts',(20.7680219782952,18.6240290139886,-10.7487144389166));
#95235=CARTESIAN_POINT('Ctrl Pts',(20.7653512446754,18.6148519714732,-10.7492812526719));
#95236=CARTESIAN_POINT('Ctrl Pts',(20.7560248139155,18.5835954752886,-10.7512088474962));
#95237=CARTESIAN_POINT('Ctrl Pts',(20.7490704023506,18.5616063437684,-10.75255987335));
#95238=CARTESIAN_POINT('Ctrl Pts',(20.6864183968474,18.374213915443,-10.7640406437286));
#95239=CARTESIAN_POINT('Ctrl Pts',(20.61082554301,18.2161727935064,-10.7734290120852));
#95240=CARTESIAN_POINT('Ctrl Pts',(20.4693976187957,17.9953641567839,-10.7876944135508));
#95241=CARTESIAN_POINT('Ctrl Pts',(20.4175745700575,17.9245515434608,-10.7924920188208));
#95242=CARTESIAN_POINT('Ctrl Pts',(20.3372203347245,17.8279537470279,-10.7996647054004));
#95243=CARTESIAN_POINT('Ctrl Pts',(20.3121440866085,17.7994075597901,-10.8018712644293));
#95244=CARTESIAN_POINT('Ctrl Pts',(20.2811604063603,17.765994410635,-10.8045823714871));
#95245=CARTESIAN_POINT('Ctrl Pts',(20.2759757835987,17.7604631493269,-10.8050355405535));
#95246=CARTESIAN_POINT('Ctrl Pts',(20.2678837174925,17.7519224660663,-10.8057423056499));
#95247=CARTESIAN_POINT('Ctrl Pts',(20.2649968124311,17.7488935509174,-10.8059943453365));
#95248=CARTESIAN_POINT('Ctrl Pts',(20.2596346803069,17.7433009431118,-10.8064623364636));
#95249=CARTESIAN_POINT('Ctrl Pts',(20.2571619527434,17.7407349339384,-10.8066780952769));
#95250=CARTESIAN_POINT('Ctrl Pts',(20.2515677533157,17.7349589567297,-10.8071660947011));
#95251=CARTESIAN_POINT('Ctrl Pts',(20.2484425881291,17.7317526597183,-10.8074386214364));
#95252=CARTESIAN_POINT('Ctrl Pts',(20.2392197801862,17.7223502808093,-10.808242552339));
#95253=CARTESIAN_POINT('Ctrl Pts',(20.2330942018934,17.716181903707,-10.8087760776419));
#95254=CARTESIAN_POINT('Ctrl Pts',(20.1895028101289,17.6728233612784,-10.8125686256485));
#95255=CARTESIAN_POINT('Ctrl Pts',(20.1506985209919,17.6370114056801,-10.8159227194899));
#95256=CARTESIAN_POINT('Ctrl Pts',(20.0957757162228,17.5900013321829,-10.820593319889));
#95257=CARTESIAN_POINT('Ctrl Pts',(20.0807765488779,17.5775182348891,-10.821861474106));
#95258=CARTESIAN_POINT('Ctrl Pts',(19.9517444227291,17.4731162590869,-10.8326955011036));
#95259=CARTESIAN_POINT('Ctrl Pts',(19.828615780575,17.3930443130447,-10.8425032285957));
#95260=CARTESIAN_POINT('Ctrl Pts',(19.6432609809496,17.2982159581411,-10.8559541035116));
#95261=CARTESIAN_POINT('Ctrl Pts',(19.5871079499187,17.2725195966533,-10.8598797274755));
#95262=CARTESIAN_POINT('Ctrl Pts',(19.4954182103749,17.2353186860394,-10.8660451208996));
#95263=CARTESIAN_POINT('Ctrl Pts',(19.4605639994366,17.2222367219779,-10.868334641453));
#95264=CARTESIAN_POINT('Ctrl Pts',(19.4148606264061,17.20644476179,-10.8712691199407));
#95265=CARTESIAN_POINT('Ctrl Pts',(19.404311455207,17.2028925685969,-10.8719418488147));
#95266=CARTESIAN_POINT('Ctrl Pts',(19.3871126056886,17.1972518797462,-10.8730312940388));
#95267=CARTESIAN_POINT('Ctrl Pts',(19.3804798687238,17.1951127638984,-10.873449674523));
#95268=CARTESIAN_POINT('Ctrl Pts',(19.3677063568714,17.191062720914,-10.8742520596825));
#95269=CARTESIAN_POINT('Ctrl Pts',(19.3615672099427,17.1891469498021,-10.8746362199113));
#95270=CARTESIAN_POINT('Ctrl Pts',(19.3474936454902,17.1848254549282,-10.8755135452868));
#95271=CARTESIAN_POINT('Ctrl Pts',(19.3395536022625,17.1824382982206,-10.8760060978563));
#95272=CARTESIAN_POINT('Ctrl Pts',(19.3184289104591,17.1762222881013,-10.8773102593886));
#95273=CARTESIAN_POINT('Ctrl Pts',(19.3052205555679,17.172474901218,-10.8781192132815));
#95274=CARTESIAN_POINT('Ctrl Pts',(19.2046461184331,17.1449948741627,-10.8842317136741));
#95275=CARTESIAN_POINT('Ctrl Pts',(19.1158694186432,17.1267582717938,-10.8893516473796));
#95276=CARTESIAN_POINT('Ctrl Pts',(18.8875827937008,17.0949456594772,-10.9021096701358));
#95277=CARTESIAN_POINT('Ctrl Pts',(18.7474098404639,17.0894223146684,-10.909551936079));
#95278=CARTESIAN_POINT('Ctrl Pts',(18.553049335465,17.101036611233,-10.9203112158582));
#95279=CARTESIAN_POINT('Ctrl Pts',(18.4985288706157,17.1064237572823,-10.9233813833286));
#95280=CARTESIAN_POINT('Ctrl Pts',(18.4162441323342,17.1177916078714,-10.9281737958323));
#95281=CARTESIAN_POINT('Ctrl Pts',(18.3882876363909,17.1222269273104,-10.9298302036767));
#95282=CARTESIAN_POINT('Ctrl Pts',(18.3536094120211,17.1284438742993,-10.931929377588));
#95283=CARTESIAN_POINT('Ctrl Pts',(18.3467949373701,17.129700105088,-10.9323440288116));
#95284=CARTESIAN_POINT('Ctrl Pts',(18.3360163096586,17.1317418839388,-10.9330034770276));
#95285=CARTESIAN_POINT('Ctrl Pts',(18.3320479585407,17.1325053796746,-10.9332470357568));
#95286=CARTESIAN_POINT('Ctrl Pts',(18.324564258863,17.1339674485832,-10.933707846386));
#95287=CARTESIAN_POINT('Ctrl Pts',(18.321048489529,17.1346635881807,-10.9339249588606));
#95288=CARTESIAN_POINT('Ctrl Pts',(18.313009880892,17.1362764964414,-10.9344227985276));
#95289=CARTESIAN_POINT('Ctrl Pts',(18.3084882653152,17.1371991273701,-10.9347038569164));
#95290=CARTESIAN_POINT('Ctrl Pts',(18.2964825160983,17.1396898053008,-10.9354527921197));
#95291=CARTESIAN_POINT('Ctrl Pts',(18.2890038796562,17.1412836135805,-10.9359220825106));
#95292=CARTESIAN_POINT('Ctrl Pts',(18.2364179485021,17.152788638724,-10.9392405685189));
#95293=CARTESIAN_POINT('Ctrl Pts',(18.1916403919869,17.1641323302927,-10.9421630057524));
#95294=CARTESIAN_POINT('Ctrl Pts',(18.1424653069691,17.178316859662,-10.94545429852));
#95295=CARTESIAN_POINT('Ctrl Pts',(18.1376620980046,17.1797208099239,-10.945776655514));
#95296=CARTESIAN_POINT('Ctrl Pts',(18.128021654444,17.1825757966011,-10.946425362081));
#95297=CARTESIAN_POINT('Ctrl Pts',(18.1231845415712,17.184027138981,-10.9467517191992));
#95298=CARTESIAN_POINT('Ctrl Pts',(18.0946334810105,17.1927051674271,-10.9486830040868));
#95299=CARTESIAN_POINT('Ctrl Pts',(18.071043300849,17.2003304769855,-10.950298953644));
#95300=CARTESIAN_POINT('Ctrl Pts',(18.010471619697,17.2210915666476,-10.9544924724536));
#95301=CARTESIAN_POINT('Ctrl Pts',(17.9737117390221,17.2348445047715,-10.9570805682199));
#95302=CARTESIAN_POINT('Ctrl Pts',(17.8360961842241,17.2907388688282,-10.9668924698946));
#95303=CARTESIAN_POINT('Ctrl Pts',(17.7381654209825,17.3396499435766,-10.9741188140958));
#95304=CARTESIAN_POINT('Ctrl Pts',(17.5972934727949,17.4242119259793,-10.9846789070399));
#95305=CARTESIAN_POINT('Ctrl Pts',(17.5512600820858,17.4543439569409,-10.9881610777322));
#95306=CARTESIAN_POINT('Ctrl Pts',(17.4785408336145,17.5060997981951,-10.9937088497862));
#95307=CARTESIAN_POINT('Ctrl Pts',(17.4511174762757,17.5266380845204,-10.9958127211388));
#95308=CARTESIAN_POINT('Ctrl Pts',(17.4157162871133,17.5545176561701,-10.9985459883161));
#95309=CARTESIAN_POINT('Ctrl Pts',(17.4072804178645,17.5612664274993,-10.9991986559339));
#95310=CARTESIAN_POINT('Ctrl Pts',(17.3935441175242,17.5724291004065,-11.0002637468903));
#95311=CARTESIAN_POINT('Ctrl Pts',(17.388213020286,17.5768047935323,-11.0006776974077));
#95312=CARTESIAN_POINT('Ctrl Pts',(17.3779321912045,17.5853275872008,-11.0014771667954));
#95313=CARTESIAN_POINT('Ctrl Pts',(17.3729798695991,17.589471430453,-11.0018628114986));
#95314=CARTESIAN_POINT('Ctrl Pts',(17.361585029332,17.5990950153594,-11.0027514350841));
#95315=CARTESIAN_POINT('Ctrl Pts',(17.3551562066668,17.6045908590972,-11.0032537469233));
#95316=CARTESIAN_POINT('Ctrl Pts',(17.3379467271139,17.619482249345,-11.0046011332184));
#95317=CARTESIAN_POINT('Ctrl Pts',(17.3272279297078,17.6289488476746,-11.0054432608958));
#95318=CARTESIAN_POINT('Ctrl Pts',(17.2292160894668,17.7172944772884,-11.0131733304963));
#95319=CARTESIAN_POINT('Ctrl Pts',(17.148539446951,17.8032177076299,-11.0197398030854));
#95320=CARTESIAN_POINT('Ctrl Pts',(16.9737390750565,18.0235917797716,-11.0351343229601));
#95321=CARTESIAN_POINT('Ctrl Pts',(16.887280695856,18.1631105659485,-11.0437794201131));
#95322=CARTESIAN_POINT('Ctrl Pts',(16.8045807992905,18.3392252594405,-11.0549699459295));
#95323=CARTESIAN_POINT('Ctrl Pts',(16.792025146537,18.3675647088137,-11.056779836859));
#95324=CARTESIAN_POINT('Ctrl Pts',(16.7773512486298,18.4027515556841,-11.0590503174971));
#95325=CARTESIAN_POINT('Ctrl Pts',(16.7746389831887,18.4093490245247,-11.0594770223914));
#95326=CARTESIAN_POINT('Ctrl Pts',(16.7704255515091,18.4197471434822,-11.060151292051));
#95327=CARTESIAN_POINT('Ctrl Pts',(16.7689019296574,18.4235387177769,-11.0603975223774));
#95328=CARTESIAN_POINT('Ctrl Pts',(16.7660657190921,18.4306561971514,-11.0608604667148));
#95329=CARTESIAN_POINT('Ctrl Pts',(16.7647505755981,18.4339810244076,-11.0610770241073));
#95330=CARTESIAN_POINT('Ctrl Pts',(16.7617562471194,18.4416074457138,-11.0615744346246));
#95331=CARTESIAN_POINT('Ctrl Pts',(16.7600827142152,18.4459112003731,-11.0618556220099));
#95332=CARTESIAN_POINT('Ctrl Pts',(16.7549425674859,18.4592590260229,-11.0627291387621));
#95333=CARTESIAN_POINT('Ctrl Pts',(16.7515239882663,18.4683212889383,-11.063324227818));
#95334=CARTESIAN_POINT('Ctrl Pts',(16.7472469472449,18.4798992073903,-11.0640868013895));
#95335=CARTESIAN_POINT('Ctrl Pts',(16.7463308326445,18.4823935618772,-11.0642512256825));
#95336=CARTESIAN_POINT('Ctrl Pts',(16.7454194505824,18.4848895411316,-11.0644158872188));
#95337=CARTESIAN_POINT('',(16.617000600774,19.2094051091123,-10.0879364343762));
#95338=CARTESIAN_POINT('Ctrl Pts',(16.7454194500511,18.4848895425866,-10.8441190257052));
#95339=CARTESIAN_POINT('Ctrl Pts',(16.7463456808613,18.4823528974314,-10.8439718529077));
#95340=CARTESIAN_POINT('Ctrl Pts',(16.7472767944397,18.4798179447603,-10.8438247200276));
#95341=CARTESIAN_POINT('Ctrl Pts',(16.8056499912094,18.3218319417938,-10.8346510184629));
#95342=CARTESIAN_POINT('Ctrl Pts',(16.8811330175697,18.1736859260385,-10.8258505658532));
#95343=CARTESIAN_POINT('Ctrl Pts',(16.9808578142822,18.0242493928235,-10.8152891834463));
#95344=CARTESIAN_POINT('Ctrl Pts',(16.9887344673045,18.012695896675,-10.8144605234353));
#95345=CARTESIAN_POINT('Ctrl Pts',(16.9998805543149,17.9966898071256,-10.8132942218365));
#95346=CARTESIAN_POINT('Ctrl Pts',(17.0030540337233,17.992170415238,-10.8129628524692));
#95347=CARTESIAN_POINT('Ctrl Pts',(17.0081863135995,17.984921941929,-10.8124279720849));
#95348=CARTESIAN_POINT('Ctrl Pts',(17.0101340155467,17.9821849805886,-10.8122252190202));
#95349=CARTESIAN_POINT('Ctrl Pts',(17.0142251834924,17.9764648346671,-10.8117997964212));
#95350=CARTESIAN_POINT('Ctrl Pts',(17.0163699017911,17.9734825904479,-10.8115770375478));
#95351=CARTESIAN_POINT('Ctrl Pts',(17.0215923838649,17.9662604264057,-10.8110352698552));
#95352=CARTESIAN_POINT('Ctrl Pts',(17.0246781358047,17.9620263361052,-10.8107157131127));
#95353=CARTESIAN_POINT('Ctrl Pts',(17.0356087281354,17.9471443884301,-10.8095858171662));
#95354=CARTESIAN_POINT('Ctrl Pts',(17.0435374145466,17.9365588887214,-10.8087699406346));
#95355=CARTESIAN_POINT('Ctrl Pts',(17.091565113561,17.8736744015733,-10.8038531925198));
#95356=CARTESIAN_POINT('Ctrl Pts',(17.1339858538914,17.823201322556,-10.799615457748));
#95357=CARTESIAN_POINT('Ctrl Pts',(17.243918256593,17.7041520182491,-10.7890378193802));
#95358=CARTESIAN_POINT('Ctrl Pts',(17.3138862653416,17.6380374290032,-10.7826421490396));
#95359=CARTESIAN_POINT('Ctrl Pts',(17.4967378903779,17.4874345028501,-10.7670586103127));
#95360=CARTESIAN_POINT('Ctrl Pts',(17.6140381139118,17.4090027193463,-10.7580100722682));
#95361=CARTESIAN_POINT('Ctrl Pts',(17.7508859012075,17.3360653790118,-10.7485414236086));
#95362=CARTESIAN_POINT('Ctrl Pts',(17.7635632872765,17.3294724911557,-10.7476734931677));
#95363=CARTESIAN_POINT('Ctrl Pts',(17.7838464468078,17.3191837561465,-10.7462992429362));
#95364=CARTESIAN_POINT('Ctrl Pts',(17.7914091199717,17.3154043386634,-10.7457899954639));
#95365=CARTESIAN_POINT('Ctrl Pts',(17.8047871228633,17.308818589694,-10.7448946326345));
#95366=CARTESIAN_POINT('Ctrl Pts',(17.8105929932058,17.3059933884664,-10.7445078612206));
#95367=CARTESIAN_POINT('Ctrl Pts',(17.8226282411554,17.3002048509659,-10.7437097896492));
#95368=CARTESIAN_POINT('Ctrl Pts',(17.8288593662753,17.2972453084829,-10.7432986249091));
#95369=CARTESIAN_POINT('Ctrl Pts',(17.8448911680343,17.2897266408971,-10.7422458868943));
#95370=CARTESIAN_POINT('Ctrl Pts',(17.8547125740576,17.285211988661,-10.7416058550837));
#95371=CARTESIAN_POINT('Ctrl Pts',(17.8958499553497,17.2666824897977,-10.7389449658021));
#95372=CARTESIAN_POINT('Ctrl Pts',(17.9274707415219,17.2533542634829,-10.7369476421261));
#95373=CARTESIAN_POINT('Ctrl Pts',(18.0106938051536,17.2206345696118,-10.7318029468363));
#95374=CARTESIAN_POINT('Ctrl Pts',(18.0627549203165,17.2024788807158,-10.7286949766252));
#95375=CARTESIAN_POINT('Ctrl Pts',(18.2200494142554,17.1544247381263,-10.7195498487507));
#95376=CARTESIAN_POINT('Ctrl Pts',(18.3269517784088,17.1306251201954,-10.7136614180894));
#95377=CARTESIAN_POINT('Ctrl Pts',(18.4810888913437,17.1086507754174,-10.7051846655704));
#95378=CARTESIAN_POINT('Ctrl Pts',(18.5271649999029,17.1036188467924,-10.7026508028881));
#95379=CARTESIAN_POINT('Ctrl Pts',(18.5947027911534,17.0984794406683,-10.6988935419683));
#95380=CARTESIAN_POINT('Ctrl Pts',(18.6160608743801,17.0971794906358,-10.6976990306905));
#95381=CARTESIAN_POINT('Ctrl Pts',(18.6892330596353,17.0938383129726,-10.6935744655786));
#95382=CARTESIAN_POINT('Ctrl Pts',(18.7410966161713,17.0933771860091,-10.6905959233844));
#95383=CARTESIAN_POINT('Ctrl Pts',(18.8015718362507,17.0950609745616,-10.6870052852223));
#95384=CARTESIAN_POINT('Ctrl Pts',(18.8102219541795,17.0953549162636,-10.6864888831743));
#95385=CARTESIAN_POINT('Ctrl Pts',(18.8233354689785,17.0958810558833,-10.685701429351));
#95386=CARTESIAN_POINT('Ctrl Pts',(18.8278004538525,17.096074363531,-10.6854325036307));
#95387=CARTESIAN_POINT('Ctrl Pts',(18.8358239937517,17.0964471938743,-10.6849477412303));
#95388=CARTESIAN_POINT('Ctrl Pts',(18.8393827338521,17.0966215630365,-10.6847321958953));
#95389=CARTESIAN_POINT('Ctrl Pts',(18.8471262686733,17.0970205748798,-10.6842620107358));
#95390=CARTESIAN_POINT('Ctrl Pts',(18.8513107879042,17.0972486568108,-10.6840071857044));
#95391=CARTESIAN_POINT('Ctrl Pts',(18.8630928837328,17.0979259471869,-10.6832876526075));
#95392=CARTESIAN_POINT('Ctrl Pts',(18.8706886647821,17.0984036991928,-10.6828213908528));
#95393=CARTESIAN_POINT('Ctrl Pts',(18.9167087457112,17.1015474518372,-10.6799826831708));
#95394=CARTESIAN_POINT('Ctrl Pts',(18.9550544199134,17.1052205597344,-10.6775591249822));
#95395=CARTESIAN_POINT('Ctrl Pts',(19.0823756916008,17.120932276181,-10.6693637707954));
#95396=CARTESIAN_POINT('Ctrl Pts',(19.1706807197682,17.1375833322489,-10.6634408411964));
#95397=CARTESIAN_POINT('Ctrl Pts',(19.4238615944747,17.20221812311,-10.6461739133023));
#95398=CARTESIAN_POINT('Ctrl Pts',(19.5843273030891,17.2647011797319,-10.6349279670057));
#95399=CARTESIAN_POINT('Ctrl Pts',(19.7560012174503,17.3568847258749,-10.6229309459337));
#95400=CARTESIAN_POINT('Ctrl Pts',(19.7763099310615,17.3682249150958,-10.6215108773086));
#95401=CARTESIAN_POINT('Ctrl Pts',(19.8047233172305,17.3847107159517,-10.6195221822124));
#95402=CARTESIAN_POINT('Ctrl Pts',(19.8129856408882,17.3895799598714,-10.6189436533945));
#95403=CARTESIAN_POINT('Ctrl Pts',(19.8263413871064,17.3975736871088,-10.6180080132134));
#95404=CARTESIAN_POINT('Ctrl Pts',(19.8314551022912,17.4006638439605,-10.6176496577185));
#95405=CARTESIAN_POINT('Ctrl Pts',(19.8421196563331,17.407170100265,-10.6169020475993));
#95406=CARTESIAN_POINT('Ctrl Pts',(19.8476679465778,17.410590272699,-10.6165129473782));
#95407=CARTESIAN_POINT('Ctrl Pts',(19.8608074120459,17.4187739065306,-10.6155910686919));
#95408=CARTESIAN_POINT('Ctrl Pts',(19.8683843481337,17.4235600797718,-10.6150591348975));
#95409=CARTESIAN_POINT('Ctrl Pts',(19.893705234678,17.4397805477699,-10.6132801934133));
#95410=CARTESIAN_POINT('Ctrl Pts',(19.9113088721777,17.4514323126798,-10.612041282077));
#95411=CARTESIAN_POINT('Ctrl Pts',(20.0055364870751,17.5158484304989,-10.6053929023444));
#95412=CARTESIAN_POINT('Ctrl Pts',(20.0787976271102,17.5733595863709,-10.6001690193662));
#95413=CARTESIAN_POINT('Ctrl Pts',(20.2631903066744,17.7388569404021,-10.5865243612946));
#95414=CARTESIAN_POINT('Ctrl Pts',(20.3666500472961,17.8545061476902,-10.5783423827433));
#95415=CARTESIAN_POINT('Ctrl Pts',(20.4877612361527,18.0240340843417,-10.5666284270531));
#95416=CARTESIAN_POINT('Ctrl Pts',(20.5172708705414,18.0688482910641,-10.5635510417338));
#95417=CARTESIAN_POINT('Ctrl Pts',(20.5495711994075,18.1222086343617,-10.5598496860012));
#95418=CARTESIAN_POINT('Ctrl Pts',(20.5540515795039,18.1297148109813,-10.5593281862634));
#95419=CARTESIAN_POINT('Ctrl Pts',(20.5607615168274,18.1411161270856,-10.5585344774732));
#95420=CARTESIAN_POINT('Ctrl Pts',(20.5630254499802,18.1449910678816,-10.5582644454499));
#95421=CARTESIAN_POINT('Ctrl Pts',(20.5670652689543,18.151956363566,-10.5577785085781));
#95422=CARTESIAN_POINT('Ctrl Pts',(20.5688456856062,18.1550440284572,-10.5575629013832));
#95423=CARTESIAN_POINT('Ctrl Pts',(20.5726953637035,18.1617594168982,-10.5570935408109));
#95424=CARTESIAN_POINT('Ctrl Pts',(20.5747616630726,18.1653887238561,-10.5568396074713));
#95425=CARTESIAN_POINT('Ctrl Pts',(20.5805304866881,18.1755913467433,-10.5561250539674));
#95426=CARTESIAN_POINT('Ctrl Pts',(20.5842085882237,18.1821782984234,-10.5556629136313));
#95427=CARTESIAN_POINT('Ctrl Pts',(20.605885280426,18.221490332854,-10.5529005931958));
#95428=CARTESIAN_POINT('Ctrl Pts',(20.6230493304123,18.2546652699205,-10.5505523783761));
#95429=CARTESIAN_POINT('Ctrl Pts',(20.676436359367,18.3649035356381,-10.5427354543226));
#95430=CARTESIAN_POINT('Ctrl Pts',(20.7088879644602,18.4436969970264,-10.5371293825934));
#95431=CARTESIAN_POINT('Ctrl Pts',(20.7942920234098,18.6927187536137,-10.5197380965397));
#95432=CARTESIAN_POINT('Ctrl Pts',(20.8305935381181,18.8678692505629,-10.508032042151));
#95433=CARTESIAN_POINT('Ctrl Pts',(20.8463035046377,19.068234531975,-10.4956638611662));
#95434=CARTESIAN_POINT('Ctrl Pts',(20.8477176651531,19.0909759597103,-10.4942732103255));
#95435=CARTESIAN_POINT('Ctrl Pts',(20.8492014991643,19.1232384179958,-10.4923182623713));
#95436=CARTESIAN_POINT('Ctrl Pts',(20.849574477277,19.1327432874682,-10.4917445112734));
#95437=CARTESIAN_POINT('Ctrl Pts',(20.8500769567745,19.1482079464258,-10.4908144957193));
#95438=CARTESIAN_POINT('Ctrl Pts',(20.8502453676407,19.1541662595599,-10.4904570164647));
#95439=CARTESIAN_POINT('Ctrl Pts',(20.8505455380383,19.166653342831,-10.4897095677839));
#95440=CARTESIAN_POINT('Ctrl Pts',(20.8506722596,19.1731821800572,-10.4893197600837));
#95441=CARTESIAN_POINT('Ctrl Pts',(20.8509022271688,19.1887402617858,-10.4883931749867));
#95442=CARTESIAN_POINT('Ctrl Pts',(20.8509779171904,19.1977698332267,-10.4878572657998));
#95443=CARTESIAN_POINT('Ctrl Pts',(20.8510385098232,19.2283093128937,-10.4860508192928));
#95444=CARTESIAN_POINT('Ctrl Pts',(20.8507533655752,19.2498188599572,-10.4847887297042));
#95445=CARTESIAN_POINT('Ctrl Pts',(20.8450120733732,19.4512312258627,-10.4730571815745));
#95446=CARTESIAN_POINT('Ctrl Pts',(20.8169638006571,19.6297502361542,-10.4633898141733));
#95447=CARTESIAN_POINT('Ctrl Pts',(20.7331540340856,19.9177188354101,-10.4470657321036));
#95448=CARTESIAN_POINT('Ctrl Pts',(20.689927413938,20.0297844315691,-10.4404845547594));
#95449=CARTESIAN_POINT('Ctrl Pts',(20.6332938716225,20.146126906848,-10.4328161010472));
#95450=CARTESIAN_POINT('Ctrl Pts',(20.629071614573,20.1546541266213,-10.4322489339741));
#95451=CARTESIAN_POINT('Ctrl Pts',(20.6227301663004,20.1672470268566,-10.4314033205938));
#95452=CARTESIAN_POINT('Ctrl Pts',(20.6206549544595,20.1713348891776,-10.4311275586822));
#95453=CARTESIAN_POINT('Ctrl Pts',(20.6169391562285,20.1785959356094,-10.4306354320642));
#95454=CARTESIAN_POINT('Ctrl Pts',(20.6153038003953,20.1817717399348,-10.4304193975591));
#95455=CARTESIAN_POINT('Ctrl Pts',(20.6117705938852,20.1885906455286,-10.4299538232286));
#95456=CARTESIAN_POINT('Ctrl Pts',(20.6098702035568,20.1922323130788,-10.4297041286948));
#95457=CARTESIAN_POINT('Ctrl Pts',(20.6045953937572,20.2022689623246,-10.4290130952983));
#95458=CARTESIAN_POINT('Ctrl Pts',(20.6011988278623,20.2086521520893,-10.4285703901153));
#95459=CARTESIAN_POINT('Ctrl Pts',(20.5824139318691,20.2435227717658,-10.4261348021302));
#95460=CARTESIAN_POINT('Ctrl Pts',(20.5664071964543,20.2716700423081,-10.4241059367913));
#95461=CARTESIAN_POINT('Ctrl Pts',(20.4660409327737,20.4391039225393,-10.4117033358881));
#95462=CARTESIAN_POINT('Ctrl Pts',(20.366487666859,20.5686409554826,-10.4007371245855));
#95463=CARTESIAN_POINT('Ctrl Pts',(20.1716614589363,20.769358343412,-10.3824655434921));
#95464=CARTESIAN_POINT('Ctrl Pts',(20.083434795197,20.8463546256413,-10.3750199444763));
#95465=CARTESIAN_POINT('Ctrl Pts',(19.9777952958741,20.9241450474022,-10.3670096145457));
#95466=CARTESIAN_POINT('Ctrl Pts',(19.966217442339,20.9324914701889,-10.3661427030888));
#95467=CARTESIAN_POINT('Ctrl Pts',(19.9476520770016,20.9455918914904,-10.3647697562727));
#95468=CARTESIAN_POINT('Ctrl Pts',(19.9407191318255,20.950422126499,-10.364260801866));
#95469=CARTESIAN_POINT('Ctrl Pts',(19.9284383166171,20.9588694992475,-10.3633657798626));
#95470=CARTESIAN_POINT('Ctrl Pts',(19.9231025057767,20.962503899736,-10.3629790577809));
#95471=CARTESIAN_POINT('Ctrl Pts',(19.9120295316824,20.9699721526607,-10.3621809208398));
#95472=CARTESIAN_POINT('Ctrl Pts',(19.9062900761022,20.9738024820034,-10.3617696422219));
#95473=CARTESIAN_POINT('Ctrl Pts',(19.8915045302492,20.9835657365504,-10.360716266342));
#95474=CARTESIAN_POINT('Ctrl Pts',(19.8824314348382,20.989457554734,-10.3600757142129));
#95475=CARTESIAN_POINT('Ctrl Pts',(19.8443316550008,21.0137853508032,-10.3574097625365));
#95476=CARTESIAN_POINT('Ctrl Pts',(19.8149021775307,21.0315828972413,-10.355408011231));
#95477=CARTESIAN_POINT('Ctrl Pts',(19.7370616172996,21.0761039464869,-10.3502493270476));
#95478=CARTESIAN_POINT('Ctrl Pts',(19.6880134213877,21.1016624187991,-10.3471320771683));
#95479=CARTESIAN_POINT('Ctrl Pts',(19.4673801613852,21.2058567861411,-10.3335668218609));
#95480=CARTESIAN_POINT('Ctrl Pts',(19.2867569893165,21.2632538229222,-10.3237191112559));
#95481=CARTESIAN_POINT('Ctrl Pts',(19.0604411030488,21.3030841887266,-10.3106515664));
#95482=CARTESIAN_POINT('Ctrl Pts',(19.0197450698734,21.3090298619439,-10.3082707374228));
#95483=CARTESIAN_POINT('Ctrl Pts',(18.9715637294868,21.3146413900157,-10.3053885547431));
#95484=CARTESIAN_POINT('Ctrl Pts',(18.964218284229,21.3154579257725,-10.3049474213742));
#95485=CARTESIAN_POINT('Ctrl Pts',(18.9523064932537,21.3167189563785,-10.3042290304884));
#95486=CARTESIAN_POINT('Ctrl Pts',(18.9477426418276,21.3171871071688,-10.3039530695453));
#95487=CARTESIAN_POINT('Ctrl Pts',(18.939622305831,21.3179934101271,-10.3034607249753));
#95488=CARTESIAN_POINT('Ctrl Pts',(18.9360664511866,21.3183373987221,-10.3032446726777));
#95489=CARTESIAN_POINT('Ctrl Pts',(18.9284222596688,21.3190573617101,-10.3027792164663));
#95490=CARTESIAN_POINT('Ctrl Pts',(18.9243337551308,21.3194304390496,-10.3025296586692));
#95491=CARTESIAN_POINT('Ctrl Pts',(18.9130516005739,21.3204268562338,-10.3018393801654));
#95492=CARTESIAN_POINT('Ctrl Pts',(18.9058558854201,21.3210252815201,-10.3013972979557));
#95493=CARTESIAN_POINT('Ctrl Pts',(18.8665230637097,21.3240938303984,-10.2989713643165));
#95494=CARTESIAN_POINT('Ctrl Pts',(18.8343376672896,21.3258664234142,-10.2969518591124));
#95495=CARTESIAN_POINT('Ctrl Pts',(18.639249404319,21.3321477476314,-10.2845523662688));
#95496=CARTESIAN_POINT('Ctrl Pts',(18.4763162096868,21.3185683610775,-10.273577526453));
#95497=CARTESIAN_POINT('Ctrl Pts',(18.2019753830702,21.2633884481375,-10.2552983262862));
#95498=CARTESIAN_POINT('Ctrl Pts',(18.0894871427162,21.2308909697044,-10.2478532317566));
#95499=CARTESIAN_POINT('Ctrl Pts',(17.9668770779023,21.1841740787605,-10.2398415196094));
#95500=CARTESIAN_POINT('Ctrl Pts',(17.9535648266366,21.1789467672255,-10.2389728172653));
#95501=CARTESIAN_POINT('Ctrl Pts',(17.9324653004991,21.1704138567701,-10.2375975797614));
#95502=CARTESIAN_POINT('Ctrl Pts',(17.9246432817456,21.1671958599451,-10.2370881103717));
#95503=CARTESIAN_POINT('Ctrl Pts',(17.910883833508,21.161438533487,-10.2361924893891));
#95504=CARTESIAN_POINT('Ctrl Pts',(17.9049383828698,21.158918769581,-10.2358056805486));
#95505=CARTESIAN_POINT('Ctrl Pts',(17.8935292333466,21.1540217168015,-10.2350637328261));
#95506=CARTESIAN_POINT('Ctrl Pts',(17.8880638675277,21.1516484901846,-10.2347084601706));
#95507=CARTESIAN_POINT('Ctrl Pts',(17.8736594669946,21.1453212519478,-10.2337724528282));
#95508=CARTESIAN_POINT('Ctrl Pts',(17.8647376036873,21.1413283217344,-10.2331930536703));
#95509=CARTESIAN_POINT('Ctrl Pts',(17.831697139405,21.1262657191009,-10.2310483636955));
#95510=CARTESIAN_POINT('Ctrl Pts',(17.8077590499509,21.1148043550685,-10.2294965619977));
#95511=CARTESIAN_POINT('Ctrl Pts',(17.7489357811437,21.0852680325913,-10.2256835572129));
#95512=CARTESIAN_POINT('Ctrl Pts',(17.7143256919695,21.0666661180826,-10.2234404200608));
#95513=CARTESIAN_POINT('Ctrl Pts',(17.5863680018275,20.9932309106059,-10.2151165739654));
#95514=CARTESIAN_POINT('Ctrl Pts',(17.4967505080721,20.9322269100176,-10.2092331319849));
#95515=CARTESIAN_POINT('Ctrl Pts',(17.305801095767,20.7795940084054,-10.1959580068644));
#95516=CARTESIAN_POINT('Ctrl Pts',(17.2078821672328,20.6844969836559,-10.1886008864898));
#95517=CARTESIAN_POINT('Ctrl Pts',(17.1096885924245,20.5687721019393,-10.1797012671102));
#95518=CARTESIAN_POINT('Ctrl Pts',(17.0997222558615,20.5567595820042,-10.1787778696874));
#95519=CARTESIAN_POINT('Ctrl Pts',(17.0862501011173,20.5401511031376,-10.1775000006378));
#95520=CARTESIAN_POINT('Ctrl Pts',(17.082628647919,20.535649025208,-10.1771534901056));
#95521=CARTESIAN_POINT('Ctrl Pts',(17.0769001140311,20.5284674899228,-10.1766004625432));
#95522=CARTESIAN_POINT('Ctrl Pts',(17.0747809658554,20.5257976328828,-10.1763948024152));
#95523=CARTESIAN_POINT('Ctrl Pts',(17.0704149445373,20.5202696363774,-10.1759688219611));
#95524=CARTESIAN_POINT('Ctrl Pts',(17.0681689892963,20.517410831438,-10.1757484367202));
#95525=CARTESIAN_POINT('Ctrl Pts',(17.0628305404511,20.510579540437,-10.1752216244526));
#95526=CARTESIAN_POINT('Ctrl Pts',(17.059744841147,20.5066017931078,-10.1749147206601));
#95527=CARTESIAN_POINT('Ctrl Pts',(17.0493660175254,20.493123549008,-10.1738744091635));
#95528=CARTESIAN_POINT('Ctrl Pts',(17.0421394942459,20.4835723805295,-10.1731365473979));
#95529=CARTESIAN_POINT('Ctrl Pts',(16.9597944676103,20.3727972400555,-10.1645761840224));
#95530=CARTESIAN_POINT('Ctrl Pts',(16.8937877008371,20.2651300396035,-10.1562460925395));
#95531=CARTESIAN_POINT('Ctrl Pts',(16.8040456883625,20.0843347708155,-10.1429073629733));
#95532=CARTESIAN_POINT('Ctrl Pts',(16.7740074419759,20.0146587587977,-10.1379034860672));
#95533=CARTESIAN_POINT('Ctrl Pts',(16.7335752731302,19.9050267144563,-10.1303131071387));
#95534=CARTESIAN_POINT('Ctrl Pts',(16.7205007735365,19.8661284806985,-10.1276720524118));
#95535=CARTESIAN_POINT('Ctrl Pts',(16.7056936940796,19.8174321089819,-10.1244341631383));
#95536=CARTESIAN_POINT('Ctrl Pts',(16.7028889868685,19.807971046537,-10.123808231091));
#95537=CARTESIAN_POINT('Ctrl Pts',(16.6846210540898,19.7447287996249,-10.1196453076624));
#95538=CARTESIAN_POINT('Ctrl Pts',(16.6712283474928,19.6903688847012,-10.1161694891358));
#95539=CARTESIAN_POINT('Ctrl Pts',(16.6575926826235,19.6237545460312,-10.1120304221958));
#95540=CARTESIAN_POINT('Ctrl Pts',(16.6552811246771,19.6119507571611,-10.111301489832));
#95541=CARTESIAN_POINT('Ctrl Pts',(16.6516247786829,19.5923977958541,-10.1101012848126));
#95542=CARTESIAN_POINT('Ctrl Pts',(16.6502223738101,19.5846598028042,-10.1096281849467));
#95543=CARTESIAN_POINT('Ctrl Pts',(16.647762545748,19.5706426376986,-10.1087745130955));
#95544=CARTESIAN_POINT('Ctrl Pts',(16.646690278268,19.5643661971801,-10.1083934731164));
#95545=CARTESIAN_POINT('Ctrl Pts',(16.6446635349805,19.5521716130033,-10.1076554515411));
#95546=CARTESIAN_POINT('Ctrl Pts',(16.6437058478971,19.5462540714129,-10.1072983713889));
#95547=CARTESIAN_POINT('Ctrl Pts',(16.6416603185898,19.5332651754798,-10.106516856433));
#95548=CARTESIAN_POINT('Ctrl Pts',(16.6405831595346,19.5261921948508,-10.1060927626622));
#95549=CARTESIAN_POINT('Ctrl Pts',(16.6380227879121,19.508787616514,-10.1050527316809));
#95550=CARTESIAN_POINT('Ctrl Pts',(16.6365800762816,19.4984501827135,-10.10443807039));
#95551=CARTESIAN_POINT('Ctrl Pts',(16.6230153915459,19.3957106312585,-10.098358525497));
#95552=CARTESIAN_POINT('Ctrl Pts',(16.6169303822837,19.3026105459037,-10.0930911649182));
#95553=CARTESIAN_POINT('Ctrl Pts',(16.617000600774,19.2094051091123,-10.0879364343762));
#95554=CARTESIAN_POINT('Ctrl Pts',(16.6170005988921,19.2094076090818,-10.0879365726371));
#95555=CARTESIAN_POINT('Ctrl Pts',(16.6171166072579,19.0551806300102,-10.079407039861));
#95556=CARTESIAN_POINT('Ctrl Pts',(16.6340851386937,18.901431767422,-10.0712484902641));
#95557=CARTESIAN_POINT('Ctrl Pts',(16.6803058095911,18.6938498832741,-10.0593799989335));
#95558=CARTESIAN_POINT('Ctrl Pts',(16.6953621981461,18.6373635760974,-10.0560550010929));
#95559=CARTESIAN_POINT('Ctrl Pts',(16.716425838712,18.5697218254495,-10.0518778646937));
#95560=CARTESIAN_POINT('Ctrl Pts',(16.7202219175506,18.5578989270259,-10.0511403713423));
#95561=CARTESIAN_POINT('Ctrl Pts',(16.7257260431972,18.5412606411189,-10.0500911539455));
#95562=CARTESIAN_POINT('Ctrl Pts',(16.7273479344961,18.536416735182,-10.0497843303886));
#95563=CARTESIAN_POINT('Ctrl Pts',(16.7301583328951,18.5281230810269,-10.0492565739232));
#95564=CARTESIAN_POINT('Ctrl Pts',(16.7313382697674,18.5246704090759,-10.0490361462883));
#95565=CARTESIAN_POINT('Ctrl Pts',(16.7336315060848,18.5180163227447,-10.0486099114122));
#95566=CARTESIAN_POINT('Ctrl Pts',(16.7347435721344,18.5148145192164,-10.0484041827799));
#95567=CARTESIAN_POINT('Ctrl Pts',(16.7377395838904,18.5062549352212,-10.0478525254537));
#95568=CARTESIAN_POINT('Ctrl Pts',(16.7396373932051,18.500902086918,-10.0475057854285));
#95569=CARTESIAN_POINT('Ctrl Pts',(16.7428347657553,18.4919976967176,-10.0469261397184));
#95570=CARTESIAN_POINT('Ctrl Pts',(16.7441223562984,18.4884418608032,-10.0466939075207));
#95571=CARTESIAN_POINT('Ctrl Pts',(16.7454194503153,18.4848895418633,-10.0464611586511));
#95572=CARTESIAN_POINT('Origin',(18.734,19.211,0.));
#95573=CARTESIAN_POINT('',(16.7454193052938,18.48488993903,-9.24346979856369));
#95574=CARTESIAN_POINT('',(16.7454194503191,18.4848895418526,-9.46634969422496));
#95575=CARTESIAN_POINT('',(16.7454194503191,18.4848895418526,0.));
#95576=CARTESIAN_POINT('',(16.6163914501725,19.212893456819,-9.51094371951111));
#95577=CARTESIAN_POINT('Ctrl Pts',(16.7454194503191,18.4848895418526,-9.46634969422496));
#95578=CARTESIAN_POINT('Ctrl Pts',(16.7207383638393,18.552483016052,-9.47066127900277));
#95579=CARTESIAN_POINT('Ctrl Pts',(16.6995057450598,18.6213417166538,-9.47497286378058));
#95580=CARTESIAN_POINT('Ctrl Pts',(16.6818386275887,18.6910743307134,-9.47928444855839));
#95581=CARTESIAN_POINT('Ctrl Pts',(16.6641689584331,18.7608170163443,-9.48359665606395));
#95582=CARTESIAN_POINT('Ctrl Pts',(16.6500659226405,18.8314333804341,-9.48790886356951));
#95583=CARTESIAN_POINT('Ctrl Pts',(16.6395956397896,18.9025208662947,-9.49222107107507));
#95584=CARTESIAN_POINT('Ctrl Pts',(16.6291143285382,18.9736832289539,-9.49653782065002));
#95585=CARTESIAN_POINT('Ctrl Pts',(16.6222734603225,19.0453172089163,-9.50085457022496));
#95586=CARTESIAN_POINT('Ctrl Pts',(16.6190872658805,19.1170152828417,-9.5051713197999));
#95587=CARTESIAN_POINT('Ctrl Pts',(16.6176670680779,19.14897361084,-9.50709544539002));
#95588=CARTESIAN_POINT('Ctrl Pts',(16.6169722855427,19.1809446693594,-9.50901957098014));
#95589=CARTESIAN_POINT('Ctrl Pts',(16.6170008459316,19.2128925310153,-9.51094369657026));
#95590=CARTESIAN_POINT('Ctrl Pts',(16.616352496962,19.2128935159973,-9.51094372097751));
#95591=CARTESIAN_POINT('Ctrl Pts',(16.6150297892913,19.3558822368191,-9.51955279572481));
#95592=CARTESIAN_POINT('Ctrl Pts',(16.6934794697575,20.2015184257048,-9.57055380603261));
#95593=CARTESIAN_POINT('Ctrl Pts',(17.8308508198777,21.5456632002202,-9.66394675190086));
#95594=CARTESIAN_POINT('Ctrl Pts',(20.2082247613025,21.2341144439155,-9.79112255858231));
#95595=CARTESIAN_POINT('Ctrl Pts',(21.2330889849398,19.0664837539622,-9.91829836526374));
#95596=CARTESIAN_POINT('Ctrl Pts',(19.9651941758507,17.0314377500589,-10.0454741719452));
#95597=CARTESIAN_POINT('Ctrl Pts',(17.7787242164569,16.9991228464334,-10.1614588018767));
#95598=CARTESIAN_POINT('Ctrl Pts',(16.9288259028377,17.999326025981,-10.2350514962479));
#95599=CARTESIAN_POINT('Ctrl Pts',(16.746026985005,18.4851209024697,-10.2662522550585));
#95600=CARTESIAN_POINT('Ctrl Pts',(16.7454194503153,18.4848895418633,-10.0464611586511));
#95601=CARTESIAN_POINT('Ctrl Pts',(16.7492540692639,18.4743877668629,-10.0457730795959));
#95602=CARTESIAN_POINT('Ctrl Pts',(16.7531717467079,18.4639167294962,-10.0450804854191));
#95603=CARTESIAN_POINT('Ctrl Pts',(16.8130754566754,18.3075922481247,-10.0346477479531));
#95604=CARTESIAN_POINT('Ctrl Pts',(16.8849512981194,18.168354599542,-10.0241793135717));
#95605=CARTESIAN_POINT('Ctrl Pts',(17.008579340344,17.9825467946946,-10.0094871214254));
#95606=CARTESIAN_POINT('Ctrl Pts',(17.0483025349942,17.9285808762599,-10.0051142817485));
#95607=CARTESIAN_POINT('Ctrl Pts',(17.1238637070005,17.8355188273289,-9.99742294536467));
#95608=CARTESIAN_POINT('Ctrl Pts',(17.1587373763441,17.7957135494896,-9.99407827262933));
#95609=CARTESIAN_POINT('Ctrl Pts',(17.2102742753661,17.7411567222447,-9.98941730963709));
#95610=CARTESIAN_POINT('Ctrl Pts',(17.2257324572609,17.7252986765136,-9.98805258656972));
#95611=CARTESIAN_POINT('Ctrl Pts',(17.2533937989356,17.6977985785221,-9.98566773739921));
#95612=CARTESIAN_POINT('Ctrl Pts',(17.2654923617964,17.6860545560752,-9.98464318061443));
#95613=CARTESIAN_POINT('Ctrl Pts',(17.2836655776281,17.6688307694723,-9.98313106070535));
#95614=CARTESIAN_POINT('Ctrl Pts',(17.2896335483837,17.663239867202,-9.9826386954157));
#95615=CARTESIAN_POINT('Ctrl Pts',(17.3003433859421,17.6533225906868,-9.98176252567437));
#95616=CARTESIAN_POINT('Ctrl Pts',(17.3050727895254,17.6489829619723,-9.98137815627133));
#95617=CARTESIAN_POINT('Ctrl Pts',(17.3143686781063,17.6405307471637,-9.98062757758779));
#95618=CARTESIAN_POINT('Ctrl Pts',(17.3189334744815,17.6364164062244,-9.98026129592865));
#95619=CARTESIAN_POINT('Ctrl Pts',(17.3313367527173,17.6253345876643,-9.97927218697373));
#95620=CARTESIAN_POINT('Ctrl Pts',(17.3392092648349,17.6184053258125,-9.97865096555531));
#95621=CARTESIAN_POINT('Ctrl Pts',(17.3689940318019,17.5925795012267,-9.97632483663104));
#95622=CARTESIAN_POINT('Ctrl Pts',(17.391242049636,17.5740737920539,-9.97463603941793));
#95623=CARTESIAN_POINT('Ctrl Pts',(17.4163835301155,17.5540189405063,-9.97277793205473));
#95624=CARTESIAN_POINT('Ctrl Pts',(17.4189083850078,17.5520143347317,-9.97259188201449));
#95625=CARTESIAN_POINT('Ctrl Pts',(17.5510070719603,17.4476257986891,-9.9628864276219));
#95626=CARTESIAN_POINT('Ctrl Pts',(17.6921098443273,17.3607484032004,-9.9540113924558));
#95627=CARTESIAN_POINT('Ctrl Pts',(17.9201176582946,17.254798050159,-9.94032893772111));
#95628=CARTESIAN_POINT('Ctrl Pts',(18.0004913157635,17.2232643051149,-9.93560410729653));
#95629=CARTESIAN_POINT('Ctrl Pts',(18.1183659381789,17.1851421289355,-9.92852953561705));
#95630=CARTESIAN_POINT('Ctrl Pts',(18.1544750131813,17.1745187681236,-9.92634309891679));
#95631=CARTESIAN_POINT('Ctrl Pts',(18.1981532580054,17.1629242111301,-9.92365429506091));
#95632=CARTESIAN_POINT('Ctrl Pts',(18.2054713226853,17.1610235120352,-9.92320232876492));
#95633=CARTESIAN_POINT('Ctrl Pts',(18.2168505578096,17.1581329983979,-9.92249703890991));
#95634=CARTESIAN_POINT('Ctrl Pts',(18.2209048278413,17.1571159196686,-9.92224526128661));
#95635=CARTESIAN_POINT('Ctrl Pts',(18.2284214636035,17.1552538956571,-9.92177750816716));
#95636=CARTESIAN_POINT('Ctrl Pts',(18.2318829607817,17.1544056840669,-9.92156172370697));
#95637=CARTESIAN_POINT('Ctrl Pts',(18.2397035969862,17.1525102223619,-9.92107334683157));
#95638=CARTESIAN_POINT('Ctrl Pts',(18.2440639056234,17.1514680820039,-9.92080046631611));
#95639=CARTESIAN_POINT('Ctrl Pts',(18.2569148476295,17.1484397478758,-9.91999454489041));
#95640=CARTESIAN_POINT('Ctrl Pts',(18.2654143600164,17.1464921825656,-9.91945936741901));
#95641=CARTESIAN_POINT('Ctrl Pts',(18.3259979202234,17.1330035481429,-9.9156306099981));
#95642=CARTESIAN_POINT('Ctrl Pts',(18.3784854394883,17.1233833416842,-9.91223995785051));
#95643=CARTESIAN_POINT('Ctrl Pts',(18.4487909540028,17.1132254620416,-9.90764899083443));
#95644=CARTESIAN_POINT('Ctrl Pts',(18.466337582523,17.1109145213346,-9.90649910286534));
#95645=CARTESIAN_POINT('Ctrl Pts',(18.6323989769895,17.0911587229751,-9.89558919544303));
#95646=CARTESIAN_POINT('Ctrl Pts',(18.7823572736117,17.089274972707,-9.88557070750275));
#95647=CARTESIAN_POINT('Ctrl Pts',(18.9915058265951,17.1088484888464,-9.87201180486261));
#95648=CARTESIAN_POINT('Ctrl Pts',(19.0514851450734,17.1170672228508,-9.86816628965925));
#95649=CARTESIAN_POINT('Ctrl Pts',(19.1471454487915,17.134380980075,-9.8621115742965));
#95650=CARTESIAN_POINT('Ctrl Pts',(19.1830819600255,17.1418549172568,-9.8598548080031));
#95651=CARTESIAN_POINT('Ctrl Pts',(19.2295884228364,17.1527959847386,-9.85695568532932));
#95652=CARTESIAN_POINT('Ctrl Pts',(19.2403490877864,17.1554168073544,-9.85628637957847));
#95653=CARTESIAN_POINT('Ctrl Pts',(19.257834825701,17.1598211996922,-9.85520109132212));
#95654=CARTESIAN_POINT('Ctrl Pts',(19.2645724428938,17.1615536649894,-9.85478346835702));
#95655=CARTESIAN_POINT('Ctrl Pts',(19.2775258510273,17.1649525763561,-9.85398160591887));
#95656=CARTESIAN_POINT('Ctrl Pts',(19.2837428139334,17.1666142119269,-9.8535972158727));
#95657=CARTESIAN_POINT('Ctrl Pts',(19.2979781359502,17.1704885812375,-9.85271807302966));
#95658=CARTESIAN_POINT('Ctrl Pts',(19.3059912566813,17.1727202858234,-9.85222394158878));
#95659=CARTESIAN_POINT('Ctrl Pts',(19.3272832161136,17.1787856797925,-9.85091281873817));
#95660=CARTESIAN_POINT('Ctrl Pts',(19.3405381561843,17.1827023156396,-9.85009852836811));
#95661=CARTESIAN_POINT('Ctrl Pts',(19.4430477054654,17.214087105365,-9.84381412368992));
#95662=CARTESIAN_POINT('Ctrl Pts',(19.5304405352526,17.2473056883049,-9.83854010890437));
#95663=CARTESIAN_POINT('Ctrl Pts',(19.7430328055279,17.3446509004538,-9.82561620829409));
#95664=CARTESIAN_POINT('Ctrl Pts',(19.8645634469252,17.4156643549884,-9.81815228126884));
#95665=CARTESIAN_POINT('Ctrl Pts',(20.0204612238266,17.5289062587479,-9.80748377970363));
#95666=CARTESIAN_POINT('Ctrl Pts',(20.061601687841,17.5611833884103,-9.80454707106764));
#95667=CARTESIAN_POINT('Ctrl Pts',(20.1224477667727,17.6126712996269,-9.79994373655688));
#95668=CARTESIAN_POINT('Ctrl Pts',(20.1430453062894,17.6307996967275,-9.79833692891243));
#95669=CARTESIAN_POINT('Ctrl Pts',(20.1683434615907,17.6539531536821,-9.79629325551477));
#95670=CARTESIAN_POINT('Ctrl Pts',(20.1733807068907,17.658608546427,-9.79588275767558));
#95671=CARTESIAN_POINT('Ctrl Pts',(20.1813381984575,17.6660348403788,-9.79522841857553));
#95672=CARTESIAN_POINT('Ctrl Pts',(20.1842733679834,17.6687897800061,-9.79498578314173));
#95673=CARTESIAN_POINT('Ctrl Pts',(20.1898094649726,17.6740157214674,-9.7945256771551));
#95674=CARTESIAN_POINT('Ctrl Pts',(20.1924119755468,17.6764849692458,-9.79430833996899));
#95675=CARTESIAN_POINT('Ctrl Pts',(20.1983673842118,17.6821642630852,-9.79380861865852));
#95676=CARTESIAN_POINT('Ctrl Pts',(20.2017160071915,17.6853787273052,-9.79352589431809));
#95677=CARTESIAN_POINT('Ctrl Pts',(20.2106189760876,17.6939814490588,-9.79276962965887));
#95678=CARTESIAN_POINT('Ctrl Pts',(20.2161543345916,17.6993891345004,-9.79229463244431));
#95679=CARTESIAN_POINT('Ctrl Pts',(20.2556991517151,17.7384478838658,-9.78886744999699));
#95680=CARTESIAN_POINT('Ctrl Pts',(20.2885861840402,17.7732103543356,-9.78583671952136));
#95681=CARTESIAN_POINT('Ctrl Pts',(20.3224481120616,17.8115242172951,-9.78254440456992));
#95682=CARTESIAN_POINT('Ctrl Pts',(20.3246257969968,17.8139998407904,-9.782331879831));
#95683=CARTESIAN_POINT('Ctrl Pts',(20.4269986198787,17.9309284304711,-9.77230397843741));
#95684=CARTESIAN_POINT('Ctrl Pts',(20.5145729492168,18.0558419406547,-9.76208554370552));
#95685=CARTESIAN_POINT('Ctrl Pts',(20.6351908030188,18.2746685108814,-9.74582900641361));
#95686=CARTESIAN_POINT('Ctrl Pts',(20.6763948395662,18.3634447106208,-9.73961186505247));
#95687=CARTESIAN_POINT('Ctrl Pts',(20.7190611821095,18.4750035762942,-9.73227315357857));
#95688=CARTESIAN_POINT('Ctrl Pts',(20.7264914836894,18.4953629588576,-9.73095197618365));
#95689=CARTESIAN_POINT('Ctrl Pts',(20.7365820843569,18.5243880131049,-9.72909340797457));
#95690=CARTESIAN_POINT('Ctrl Pts',(20.7395011965821,18.5329616680246,-9.7285474622993));
#95691=CARTESIAN_POINT('Ctrl Pts',(20.744431741942,18.5477535024243,-9.72761072930052));
#95692=CARTESIAN_POINT('Ctrl Pts',(20.7464695496129,18.5539626959433,-9.72721907476441));
#95693=CARTESIAN_POINT('Ctrl Pts',(20.7503093568817,18.5658480478928,-9.72647232728343));
#95694=CARTESIAN_POINT('Ctrl Pts',(20.752116217565,18.5715225590581,-9.72611707735638));
#95695=CARTESIAN_POINT('Ctrl Pts',(20.7567377754345,18.5862514157768,-9.72519824456619));
#95696=CARTESIAN_POINT('Ctrl Pts',(20.7595156508851,18.5953172455518,-9.72463587349696));
#95697=CARTESIAN_POINT('Ctrl Pts',(20.7687082540731,18.6260537846362,-9.72273973530326));
#95698=CARTESIAN_POINT('Ctrl Pts',(20.7748369877245,18.6478089120701,-9.72141528972613));
#95699=CARTESIAN_POINT('Ctrl Pts',(20.8267306204514,18.844000015531,-9.70961825731916));
#95700=CARTESIAN_POINT('Ctrl Pts',(20.8503804708857,19.0235151551127,-9.69994615606126));
#95701=CARTESIAN_POINT('Ctrl Pts',(20.8512697721163,19.2875215914897,-9.68556915647499));
#95702=CARTESIAN_POINT('Ctrl Pts',(20.8465929758142,19.3711110805741,-9.68097955105233));
#95703=CARTESIAN_POINT('Ctrl Pts',(20.8327384784995,19.4909142006391,-9.67408773917421));
#95704=CARTESIAN_POINT('Ctrl Pts',(20.8275318223549,19.5275111297979,-9.67193934244312));
#95705=CARTESIAN_POINT('Ctrl Pts',(20.8201163022152,19.5713669674984,-9.66929271173391));
#95706=CARTESIAN_POINT('Ctrl Pts',(20.8188227543208,19.57877663989,-9.66884305623137));
#95707=CARTESIAN_POINT('Ctrl Pts',(20.8167505002429,19.5902845297706,-9.6681406010822));
#95708=CARTESIAN_POINT('Ctrl Pts',(20.8159991064496,19.594387689994,-9.66788932746214));
#95709=CARTESIAN_POINT('Ctrl Pts',(20.8145831201494,19.6019930786009,-9.6674220294971));
#95710=CARTESIAN_POINT('Ctrl Pts',(20.8139218071814,19.6054958590183,-9.66720619311979));
#95711=CARTESIAN_POINT('Ctrl Pts',(20.8124067153879,19.6134111384847,-9.66671707865762));
#95712=CARTESIAN_POINT('Ctrl Pts',(20.8115477348622,19.6178225749063,-9.66644350862493));
#95713=CARTESIAN_POINT('Ctrl Pts',(20.8089707809303,19.6308359239727,-9.66563370134964));
#95714=CARTESIAN_POINT('Ctrl Pts',(20.8072134085111,19.6394298092203,-9.6650952972764));
#95715=CARTESIAN_POINT('Ctrl Pts',(20.7941141569381,19.7015191875241,-9.66118046218243));
#95716=CARTESIAN_POINT('Ctrl Pts',(20.7807576067344,19.754563801033,-9.65770205393585));
#95717=CARTESIAN_POINT('Ctrl Pts',(20.7569589868554,19.8356737064115,-9.65223431796181));
#95718=CARTESIAN_POINT('Ctrl Pts',(20.7479487979251,19.864138911725,-9.65028631284497));
#95719=CARTESIAN_POINT('Ctrl Pts',(20.6966418051746,20.0150578664716,-9.63983132792635));
#95720=CARTESIAN_POINT('Ctrl Pts',(20.6437692710081,20.1336358389845,-9.63118811452694));
#95721=CARTESIAN_POINT('Ctrl Pts',(20.5373135348998,20.3234306219613,-9.61709969325426));
#95722=CARTESIAN_POINT('Ctrl Pts',(20.4894871086742,20.3974695509572,-9.61152497183786));
#95723=CARTESIAN_POINT('Ctrl Pts',(20.4250081502671,20.4848134022355,-9.60486236547195));
#95724=CARTESIAN_POINT('Ctrl Pts',(20.412595144485,20.5011269454122,-9.60361372204411));
#95725=CARTESIAN_POINT('Ctrl Pts',(20.3944820200499,20.5242276649228,-9.60183890369111));
#95726=CARTESIAN_POINT('Ctrl Pts',(20.3889734814306,20.5311629514248,-9.60130518516355));
#95727=CARTESIAN_POINT('Ctrl Pts',(20.3793475301045,20.5431271495623,-9.60038284499195));
#95728=CARTESIAN_POINT('Ctrl Pts',(20.3752502133798,20.5481720068729,-9.59999342518898));
#95729=CARTESIAN_POINT('Ctrl Pts',(20.3673267166262,20.5578365960045,-9.59924639392123));
#95730=CARTESIAN_POINT('Ctrl Pts',(20.3635040118203,20.5624590841693,-9.59888864733137));
#95731=CARTESIAN_POINT('Ctrl Pts',(20.3534366916731,20.5745278662587,-9.59795339129189));
#95732=CARTESIAN_POINT('Ctrl Pts',(20.3471603133288,20.5819475732814,-9.59737718280924));
#95733=CARTESIAN_POINT('Ctrl Pts',(20.3251921072876,20.6075578367705,-9.59538375582243));
#95734=CARTESIAN_POINT('Ctrl Pts',(20.309241548751,20.6255247421433,-9.59397722769793));
#95735=CARTESIAN_POINT('Ctrl Pts',(20.1932797773993,20.7517507599045,-9.58402729141683));
#95736=CARTESIAN_POINT('Ctrl Pts',(20.0825083053685,20.8495793783059,-9.57598757869103));
#95737=CARTESIAN_POINT('Ctrl Pts',(19.9242566551874,20.9623362202565,-9.56543471879967));
#95738=CARTESIAN_POINT('Ctrl Pts',(19.8851594843455,20.9882791564423,-9.56289016444519));
#95739=CARTESIAN_POINT('Ctrl Pts',(19.7844807513065,21.0503677683157,-9.55641965473239));
#95740=CARTESIAN_POINT('Ctrl Pts',(19.7218766022878,21.0847347369993,-9.55247023570512));
#95741=CARTESIAN_POINT('Ctrl Pts',(19.6274569851025,21.1305182915925,-9.5464520746851));
#95742=CARTESIAN_POINT('Ctrl Pts',(19.5969097691629,21.1444431205361,-9.54449580956827));
#95743=CARTESIAN_POINT('Ctrl Pts',(19.5593240133737,21.1605083277931,-9.54206245036514));
#95744=CARTESIAN_POINT('Ctrl Pts',(19.5525868589147,21.1633467924668,-9.54162526040247));
#95745=CARTESIAN_POINT('Ctrl Pts',(19.542025319404,21.1677322508391,-9.54093810751089));
#95746=CARTESIAN_POINT('Ctrl Pts',(19.5382108106522,21.1693030893185,-9.5406895651657));
#95747=CARTESIAN_POINT('Ctrl Pts',(19.5310869305714,21.1722124231457,-9.54022467301018));
#95748=CARTESIAN_POINT('Ctrl Pts',(19.5277787567277,21.1735537007471,-9.54000849434791));
#95749=CARTESIAN_POINT('Ctrl Pts',(19.5202385334113,21.1765886515958,-9.53951510622221));
#95750=CARTESIAN_POINT('Ctrl Pts',(19.5160044132099,21.178277020535,-9.53923758281343));
#95751=CARTESIAN_POINT('Ctrl Pts',(19.5049816719668,21.1826311657002,-9.5385139515651));
#95752=CARTESIAN_POINT('Ctrl Pts',(19.4981847353083,21.1852755326612,-9.53806660820199));
#95753=CARTESIAN_POINT('Ctrl Pts',(19.4548183114908,21.2018898647136,-9.53520585950243));
#95754=CARTESIAN_POINT('Ctrl Pts',(19.4178833833633,21.2148773819395,-9.53273980900384));
#95755=CARTESIAN_POINT('Ctrl Pts',(19.3688627141953,21.2306015937719,-9.52944739524212));
#95756=CARTESIAN_POINT('Ctrl Pts',(19.3570803642369,21.2342676818479,-9.52865458386929));
#95757=CARTESIAN_POINT('Ctrl Pts',(19.3221509550216,21.2448019569476,-9.52630119425002));
#95758=CARTESIAN_POINT('Ctrl Pts',(19.2989180848994,21.251377279152,-9.52473193265296));
#95759=CARTESIAN_POINT('Ctrl Pts',(19.1362200052563,21.2944319928249,-9.51373620565939));
#95760=CARTESIAN_POINT('Ctrl Pts',(18.9934449913382,21.3169827021489,-9.50408906971004));
#95761=CARTESIAN_POINT('Ctrl Pts',(18.7877688404288,21.3282194917069,-9.49078080512738));
#95762=CARTESIAN_POINT('Ctrl Pts',(18.7259288403398,21.3288870251516,-9.48684921389634));
#95763=CARTESIAN_POINT('Ctrl Pts',(18.6269048136485,21.3256176602687,-9.48067559158439));
#95764=CARTESIAN_POINT('Ctrl Pts',(18.5897034140495,21.3234052641623,-9.47838364469238));
#95765=CARTESIAN_POINT('Ctrl Pts',(18.5414838613437,21.3192576985587,-9.47544654961667));
#95766=CARTESIAN_POINT('Ctrl Pts',(18.5303974115057,21.3182159311648,-9.47477356915816));
#95767=CARTESIAN_POINT('Ctrl Pts',(18.5123855102357,21.3163799177615,-9.47368381845691));
#95768=CARTESIAN_POINT('Ctrl Pts',(18.5054549613428,21.3156388638672,-9.4732653823345));
#95769=CARTESIAN_POINT('Ctrl Pts',(18.4921372994051,21.314148303961,-9.47246295852408));
#95770=CARTESIAN_POINT('Ctrl Pts',(18.4857497040293,21.3134038970551,-9.47207881491793));
#95771=CARTESIAN_POINT('Ctrl Pts',(18.4711367174029,21.3116333812185,-9.47120162169463));
#95772=CARTESIAN_POINT('Ctrl Pts',(18.4629137289167,21.3105880415549,-9.47070918401676));
#95773=CARTESIAN_POINT('Ctrl Pts',(18.4410945242486,21.3076839741336,-9.46940552840154));
#95774=CARTESIAN_POINT('Ctrl Pts',(18.4275097400249,21.3057412820877,-9.46859696220938));
#95775=CARTESIAN_POINT('Ctrl Pts',(18.3247121551399,21.290019271718,-9.4625001283872));
#95776=CARTESIAN_POINT('Ctrl Pts',(18.2364381087653,21.2706778149047,-9.45739434951155));
#95777=CARTESIAN_POINT('Ctrl Pts',(18.0155894319129,21.2072546253011,-9.44467437854784));
#95778=CARTESIAN_POINT('Ctrl Pts',(17.8856587089938,21.1555980236109,-9.4372549163098));
#95779=CARTESIAN_POINT('Ctrl Pts',(17.7126396959872,21.0661467104089,-9.42649617802183));
#95780=CARTESIAN_POINT('Ctrl Pts',(17.6645407027813,21.0388408435081,-9.42339806931545));
#95781=CARTESIAN_POINT('Ctrl Pts',(17.5933680501374,20.9946645116841,-9.418566180751));
#95782=CARTESIAN_POINT('Ctrl Pts',(17.5694739381421,20.9791570084667,-9.41689953416408));
#95783=CARTESIAN_POINT('Ctrl Pts',(17.5401543141232,20.9592762057995,-9.41478891286748));
#95784=CARTESIAN_POINT('Ctrl Pts',(17.5344266243157,20.9553511477776,-9.41437342075452));
#95785=CARTESIAN_POINT('Ctrl Pts',(17.5253935827218,20.9490954762626,-9.41371293829239));
#95786=CARTESIAN_POINT('Ctrl Pts',(17.5220753641855,20.9467834061213,-9.41346919281735));
#95787=CARTESIAN_POINT('Ctrl Pts',(17.5158296068885,20.9424048441377,-9.41300823757602));
#95788=CARTESIAN_POINT('Ctrl Pts',(17.5129006824989,20.9403404225424,-9.41279116845311));
#95789=CARTESIAN_POINT('Ctrl Pts',(17.5062161342057,20.9356034402861,-9.41229369997646));
#95790=CARTESIAN_POINT('Ctrl Pts',(17.5024639928413,20.9329260464654,-9.4120129712115));
#95791=CARTESIAN_POINT('Ctrl Pts',(17.492525460807,20.9257851652729,-9.41126548329841));
#95792=CARTESIAN_POINT('Ctrl Pts',(17.4863544668134,20.9213005040056,-9.41079731905449));
#95793=CARTESIAN_POINT('Ctrl Pts',(17.443297529304,20.88965260017,-9.40750318760877));
#95794=CARTESIAN_POINT('Ctrl Pts',(17.4072803239944,20.8613337943083,-9.40460515677022));
#95795=CARTESIAN_POINT('Ctrl Pts',(17.3434297895935,20.8076893097437,-9.39924370791611));
#95796=CARTESIAN_POINT('Ctrl Pts',(17.3152969431568,20.7827454222939,-9.39679632998763));
#95797=CARTESIAN_POINT('Ctrl Pts',(17.192180401704,20.6675850159885,-9.38574620590467));
#95798=CARTESIAN_POINT('Ctrl Pts',(17.1050205714435,20.5694098384852,-9.37700301638097));
#95799=CARTESIAN_POINT('Ctrl Pts',(16.9752026493684,20.3925789203905,-9.36279856210357));
#95800=CARTESIAN_POINT('Ctrl Pts',(16.9274171308401,20.318139840831,-9.35720316584235));
#95801=CARTESIAN_POINT('Ctrl Pts',(16.8744284018121,20.2229803454949,-9.350518661249));
#95802=CARTESIAN_POINT('Ctrl Pts',(16.8646987126618,20.2048930990092,-9.34926760830961));
#95803=CARTESIAN_POINT('Ctrl Pts',(16.8511486070113,20.1788006979053,-9.3474899990882));
#95804=CARTESIAN_POINT('Ctrl Pts',(16.8471131270901,20.1709091058635,-9.34695586658156));
#95805=CARTESIAN_POINT('Ctrl Pts',(16.8402042019883,20.1571864130415,-9.34603304104757));
#95806=CARTESIAN_POINT('Ctrl Pts',(16.8373078557513,20.1513670369589,-9.34564354754152));
#95807=CARTESIAN_POINT('Ctrl Pts',(16.8317911215019,20.140153562817,-9.34489653437175));
#95808=CARTESIAN_POINT('Ctrl Pts',(16.8291667639353,20.1347614977118,-9.34453887882267));
#95809=CARTESIAN_POINT('Ctrl Pts',(16.8223533123523,20.1206099257183,-9.34360421428273));
#95810=CARTESIAN_POINT('Ctrl Pts',(16.8182014765784,20.1118325581299,-9.3430285030187));
#95811=CARTESIAN_POINT('Ctrl Pts',(16.8040088680341,20.0812861163131,-9.34103852825398));
#95812=CARTESIAN_POINT('Ctrl Pts',(16.7942773423047,20.0593747838186,-9.33963490520103));
#95813=CARTESIAN_POINT('Ctrl Pts',(16.7250855532629,19.896165311332,-9.32934404558491));
#95814=CARTESIAN_POINT('Ctrl Pts',(16.6807559351145,19.7489446285711,-9.32100721195334));
#95815=CARTESIAN_POINT('Ctrl Pts',(16.6289120186581,19.4702808470904,-9.30561469617625));
#95816=CARTESIAN_POINT('Ctrl Pts',(16.6169601914145,19.3404434587236,-9.29857228888663));
#95817=CARTESIAN_POINT('Ctrl Pts',(16.6170011042399,19.207075682044,-9.29078130925382));
#95818=CARTESIAN_POINT('Ctrl Pts',(16.6170097080016,19.2038008171236,-9.29058964995036));
#95819=CARTESIAN_POINT('Ctrl Pts',(16.6171033847899,19.1848671289577,-9.28947947365972));
#95820=CARTESIAN_POINT('Ctrl Pts',(16.6173545929795,19.169210108466,-9.288553141191));
#95821=CARTESIAN_POINT('Ctrl Pts',(16.6179364383876,19.1477744042352,-9.28727182822806));
#95822=CARTESIAN_POINT('Ctrl Pts',(16.6181171280736,19.1419917161239,-9.28692486431782));
#95823=CARTESIAN_POINT('Ctrl Pts',(16.6184419928259,19.1328018696173,-9.28637129196932));
#95824=CARTESIAN_POINT('Ctrl Pts',(16.6185707023715,19.129394144399,-9.28616554346365));
#95825=CARTESIAN_POINT('Ctrl Pts',(16.6188536013079,19.1223550755574,-9.28573953431244));
#95826=CARTESIAN_POINT('Ctrl Pts',(16.6190089085143,19.1187238238374,-9.28551920944345));
#95827=CARTESIAN_POINT('Ctrl Pts',(16.6194013861738,19.1100693729792,-9.28499279542433));
#95828=CARTESIAN_POINT('Ctrl Pts',(16.6196471049501,19.1050465995675,-9.28468623140508));
#95829=CARTESIAN_POINT('Ctrl Pts',(16.6205368678634,19.0880965206623,-9.28364825192569));
#95830=CARTESIAN_POINT('Ctrl Pts',(16.6212639477807,19.0761740577846,-9.28291240896649));
#95831=CARTESIAN_POINT('Ctrl Pts',(16.6311137078558,18.9344158113935,-9.27409997408766));
#95832=CARTESIAN_POINT('Ctrl Pts',(16.6520897229059,18.8056948566674,-9.26548333018932));
#95833=CARTESIAN_POINT('Ctrl Pts',(16.7018392867629,18.6137972733215,-9.25238337418594));
#95834=CARTESIAN_POINT('Ctrl Pts',(16.7220915832289,18.5487770275629,-9.24789461432881));
#95835=CARTESIAN_POINT('Ctrl Pts',(16.7454193052938,18.48488993903,-9.24346979856369));
#95836=CARTESIAN_POINT('Origin',(18.734,19.211,0.));
#95837=CARTESIAN_POINT('',(16.7454194503191,18.4848895418526,-8.44448864899009));
#95838=CARTESIAN_POINT('',(16.745419494333,18.4848894213129,-8.66553665550751));
#95839=CARTESIAN_POINT('',(16.7454194503191,18.4848895418526,0.));
#95840=CARTESIAN_POINT('',(16.6170000013281,19.2110749873286,-8.71094372102528));
#95841=CARTESIAN_POINT('Ctrl Pts',(16.745419494333,18.4848894213129,-8.66553665550751));
#95842=CARTESIAN_POINT('Ctrl Pts',(16.733311422067,18.5180494897324,-8.6678589517768));
#95843=CARTESIAN_POINT('Ctrl Pts',(16.7220302073804,18.5515194592593,-8.67019227608761));
#95844=CARTESIAN_POINT('Ctrl Pts',(16.6746521894853,18.7046488048368,-8.68078506136069));
#95845=CARTESIAN_POINT('Ctrl Pts',(16.6483548014453,18.827078406676,-8.68900850976821));
#95846=CARTESIAN_POINT('Ctrl Pts',(16.6297591080332,18.9774166931212,-8.69860359135708));
#95847=CARTESIAN_POINT('Ctrl Pts',(16.6270006266104,19.0037691441327,-8.70026803505595));
#95848=CARTESIAN_POINT('Ctrl Pts',(16.6216845094513,19.0657772309175,-8.70414332149744));
#95849=CARTESIAN_POINT('Ctrl Pts',(16.61953371278,19.1014602866226,-8.70634145746368));
#95850=CARTESIAN_POINT('Ctrl Pts',(16.6178981538474,19.1483376779776,-8.70918908236397));
#95851=CARTESIAN_POINT('Ctrl Pts',(16.6175971722505,19.1594959412993,-8.70986394166662));
#95852=CARTESIAN_POINT('Ctrl Pts',(16.6172522425656,19.177592504778,-8.71095375470374));
#95853=CARTESIAN_POINT('Ctrl Pts',(16.6171541291415,19.1845294474272,-8.71137039777877));
#95854=CARTESIAN_POINT('Ctrl Pts',(16.6170502016127,19.195792596711,-8.71204510585635));
#95855=CARTESIAN_POINT('Ctrl Pts',(16.6170235457636,19.2001185182293,-8.71230382138551));
#95856=CARTESIAN_POINT('Ctrl Pts',(16.6170034293859,19.2066147842418,-8.71269170733863));
#95857=CARTESIAN_POINT('Ctrl Pts',(16.6170000462397,19.2087850663916,-8.71282118744952));
#95858=CARTESIAN_POINT('Ctrl Pts',(16.6170000004708,19.2109553548739,-8.71295056330574));
#95859=CARTESIAN_POINT('Ctrl Pts',(16.6170000013281,19.2110749873285,-8.71094372102528));
#95860=CARTESIAN_POINT('Ctrl Pts',(16.6170027209272,19.2878531769883,-8.71553605185446));
#95861=CARTESIAN_POINT('Ctrl Pts',(16.6211865549027,19.36454594767,-8.72012838268363));
#95862=CARTESIAN_POINT('Ctrl Pts',(16.6294980530144,19.4406966589526,-8.72472071351281));
#95863=CARTESIAN_POINT('Ctrl Pts',(16.6378338109209,19.5170696407095,-8.72932644854445));
#95864=CARTESIAN_POINT('Ctrl Pts',(16.650321266275,19.5928969954323,-8.73393218357609));
#95865=CARTESIAN_POINT('Ctrl Pts',(16.6668554550742,19.6677301505086,-8.73853791860773));
#95866=CARTESIAN_POINT('Ctrl Pts',(16.6834151174018,19.7426785978757,-8.74315074950138));
#95867=CARTESIAN_POINT('Ctrl Pts',(16.7040338351224,19.8166294002008,-8.74776358039503));
#95868=CARTESIAN_POINT('Ctrl Pts',(16.7285569647206,19.8891498597281,-8.75237641128868));
#95869=CARTESIAN_POINT('Ctrl Pts',(16.7531478646363,19.9618707314645,-8.75700198986258));
#95870=CARTESIAN_POINT('Ctrl Pts',(16.781664593162,20.0331529809713,-8.76162756843648));
#95871=CARTESIAN_POINT('Ctrl Pts',(16.8139044122089,20.1025839465498,-8.76625314701037));
#95872=CARTESIAN_POINT('Ctrl Pts',(16.8312431022427,20.1399241682537,-8.76874079971719));
#95873=CARTESIAN_POINT('Ctrl Pts',(16.8496578472074,20.1767293760275,-8.77122845242401));
#95874=CARTESIAN_POINT('Ctrl Pts',(16.8691118619909,20.2129387370059,-8.77371610513083));
#95875=CARTESIAN_POINT('Ctrl Pts',(16.9034286623952,20.2768118977539,-8.77810431406173));
#95876=CARTESIAN_POINT('Ctrl Pts',(16.9410977666969,20.3390446523179,-8.78249252299263));
#95877=CARTESIAN_POINT('Ctrl Pts',(16.9819381659417,20.3992627359453,-8.78688073192353));
#95878=CARTESIAN_POINT('Ctrl Pts',(17.0227179512625,20.4593914459522,-8.79126242802479));
#95879=CARTESIAN_POINT('Ctrl Pts',(17.0666594195114,20.5175110248671,-8.79564412412605));
#95880=CARTESIAN_POINT('Ctrl Pts',(17.1135357879718,20.5732719029386,-8.80002582022732));
#95881=CARTESIAN_POINT('Ctrl Pts',(17.1603570729688,20.6289672575408,-8.80440236748696));
#95882=CARTESIAN_POINT('Ctrl Pts',(17.2101060983649,20.6823090498175,-8.8087789147466));
#95883=CARTESIAN_POINT('Ctrl Pts',(17.2625139124398,20.7329782173594,-8.81315546200624));
#95884=CARTESIAN_POINT('Ctrl Pts',(17.3148884902406,20.7836152512518,-8.81752923372322));
#95885=CARTESIAN_POINT('Ctrl Pts',(17.3699181652065,20.831582688923,-8.82190300544019));
#95886=CARTESIAN_POINT('Ctrl Pts',(17.4272959551551,20.8765970518664,-8.82627677715716));
#95887=CARTESIAN_POINT('Ctrl Pts',(17.4846562848495,20.9215977167879,-8.83064921792071));
#95888=CARTESIAN_POINT('Ctrl Pts',(17.5443629316526,20.9636467934747,-8.83502165868427));
#95889=CARTESIAN_POINT('Ctrl Pts',(17.6060758346833,21.0025010681813,-8.83939409944782));
#95890=CARTESIAN_POINT('Ctrl Pts',(17.6677903157196,21.0413563363958,-8.84376665201516));
#95891=CARTESIAN_POINT('Ctrl Pts',(17.7315107455601,21.0770163851239,-8.8481392045825));
#95892=CARTESIAN_POINT('Ctrl Pts',(17.7968695201135,21.1092822402551,-8.85251175714984));
#95893=CARTESIAN_POINT('Ctrl Pts',(17.8622961264685,21.1415815821077,-8.85688884771717));
#95894=CARTESIAN_POINT('Ctrl Pts',(17.9293640389054,21.1704794832203,-8.8612659382845));
#95895=CARTESIAN_POINT('Ctrl Pts',(17.9976833250388,21.1958241116467,-8.86564302885182));
#95896=CARTESIAN_POINT('Ctrl Pts',(18.06603992287,21.2211825817153,-8.87002250991077));
#95897=CARTESIAN_POINT('Ctrl Pts',(18.1356487944357,21.2429837711611,-8.87440199096971));
#95898=CARTESIAN_POINT('Ctrl Pts',(18.2061050046721,21.2611258190433,-8.87878147202865));
#95899=CARTESIAN_POINT('Ctrl Pts',(18.2766860980683,21.2793000235835,-8.88316871568837));
#95900=CARTESIAN_POINT('Ctrl Pts',(18.3481170562227,21.2938020386139,-8.88755595934809));
#95901=CARTESIAN_POINT('Ctrl Pts',(18.4199835016908,21.3045812950038,-8.89194320300781));
#95902=CARTESIAN_POINT('Ctrl Pts',(18.4688457595749,21.3119101506622,-8.89492610594263));
#95903=CARTESIAN_POINT('Ctrl Pts',(18.517909182163,21.3175191746183,-8.89790900887744));
#95904=CARTESIAN_POINT('Ctrl Pts',(18.5670433388758,21.3214062341896,-8.90089191181226));
#95905=CARTESIAN_POINT('Ctrl Pts',(18.6393255921071,21.3271245662635,-8.90528012074316));
#95906=CARTESIAN_POINT('Ctrl Pts',(18.712043061856,21.3291362205188,-8.90966832967406));
#95907=CARTESIAN_POINT('Ctrl Pts',(18.78478307398,21.3273908144285,-8.91405653860495));
#95908=CARTESIAN_POINT('Ctrl Pts',(18.8574151278656,21.3256479988102,-8.91843823470622));
#95909=CARTESIAN_POINT('Ctrl Pts',(18.9300691794575,21.3201592036426,-8.92281993080748));
#95910=CARTESIAN_POINT('Ctrl Pts',(19.0023285427324,21.3109259018249,-8.92720162690875));
#95911=CARTESIAN_POINT('Ctrl Pts',(19.0745029955047,21.3017034498717,-8.93157817416839));
#95912=CARTESIAN_POINT('Ctrl Pts',(19.1462832051698,21.2887452929198,-8.93595472142802));
#95913=CARTESIAN_POINT('Ctrl Pts',(19.2172553122688,21.2721048743729,-8.94033126868766));
#95914=CARTESIAN_POINT('Ctrl Pts',(19.2881824098891,21.2554750089377,-8.94470504040463));
#95915=CARTESIAN_POINT('Ctrl Pts',(19.3583019532977,21.2351676251633,-8.9490788121216));
#95916=CARTESIAN_POINT('Ctrl Pts',(19.427209418299,21.211287404945,-8.95345258383858));
#95917=CARTESIAN_POINT('Ctrl Pts',(19.4960959145273,21.1874144515579,-8.95782502460213));
#95918=CARTESIAN_POINT('Ctrl Pts',(19.5637706090987,21.159970978065,-8.96219746536568));
#95919=CARTESIAN_POINT('Ctrl Pts',(19.6298449292373,21.1291112748639,-8.96656990612923));
#95920=CARTESIAN_POINT('Ctrl Pts',(19.6959209389035,21.0982507825767,-8.97094245869657));
#95921=CARTESIAN_POINT('Ctrl Pts',(19.7603960566779,21.0639740930878,-8.97531501126391));
#95922=CARTESIAN_POINT('Ctrl Pts',(19.8229039996995,21.0264826023508,-8.97968756383126));
#95923=CARTESIAN_POINT('Ctrl Pts',(19.8854768158221,20.9889522015306,-8.98406465439858));
#95924=CARTESIAN_POINT('Ctrl Pts',(19.9460779664243,20.9482005866786,-8.9884417449659));
#95925=CARTESIAN_POINT('Ctrl Pts',(20.0043687218628,20.9044734454702,-8.99281883553323));
#95926=CARTESIAN_POINT('Ctrl Pts',(20.0626913120462,20.8607224232471,-8.99719831659217));
#95927=CARTESIAN_POINT('Ctrl Pts',(20.1187006241989,20.8139929484578,-9.00157779765111));
#95928=CARTESIAN_POINT('Ctrl Pts',(20.1720918257197,20.7645703720135,-9.00595727871005));
#95929=CARTESIAN_POINT('Ctrl Pts',(20.2255776627869,20.7150601943841,-9.01034452236977));
#95930=CARTESIAN_POINT('Ctrl Pts',(20.2764357852875,20.662847728454,-9.01473176602948));
#95931=CARTESIAN_POINT('Ctrl Pts',(20.324399377934,20.608254027966,-9.0191190096892));
#95932=CARTESIAN_POINT('Ctrl Pts',(20.357009999173,20.5711355722704,-9.02210191262404));
#95933=CARTESIAN_POINT('Ctrl Pts',(20.3882834007584,20.5329170566125,-9.02508481555887));
#95934=CARTESIAN_POINT('Ctrl Pts',(20.4181471898432,20.4937069980878,-9.0280677184937));
#95935=CARTESIAN_POINT('Ctrl Pts',(20.4620804149045,20.4360242867296,-9.0324559274246));
#95936=CARTESIAN_POINT('Ctrl Pts',(20.5031324849612,20.3759692727541,-9.0368441363555));
#95937=CARTESIAN_POINT('Ctrl Pts',(20.541037663595,20.3138616787018,-9.0412323452864));
#95938=CARTESIAN_POINT('Ctrl Pts',(20.578886584659,20.2518462626167,-9.04561404138767));
#95939=CARTESIAN_POINT('Ctrl Pts',(20.6135976366774,20.1877847222598,-9.04999573748893));
#95940=CARTESIAN_POINT('Ctrl Pts',(20.6449465138839,20.1220282218873,-9.0543774335902));
#95941=CARTESIAN_POINT('Ctrl Pts',(20.6762585536648,20.0563489906358,-9.05875398084984));
#95942=CARTESIAN_POINT('Ctrl Pts',(20.7042160604134,19.9889791891847,-9.06313052810949));
#95943=CARTESIAN_POINT('Ctrl Pts',(20.7286399572991,19.9202957357449,-9.06750707536913));
#95944=CARTESIAN_POINT('Ctrl Pts',(20.7530483649043,19.851655840353,-9.0718808470861));
#95945=CARTESIAN_POINT('Ctrl Pts',(20.773927447788,19.7817043993275,-9.07625461880308));
#95946=CARTESIAN_POINT('Ctrl Pts',(20.7911462655829,19.7108382158241,-9.08062839052005));
#95947=CARTESIAN_POINT('Ctrl Pts',(20.8083598436338,19.6399935971384,-9.08500083128361));
#95948=CARTESIAN_POINT('Ctrl Pts',(20.8219152540694,19.5682352570614,-9.08937327204716));
#95949=CARTESIAN_POINT('Ctrl Pts',(20.8317319036236,19.4959734382704,-9.09374571281071));
#95950=CARTESIAN_POINT('Ctrl Pts',(20.8415488041906,19.4237097717368,-9.09811826537806));
#95951=CARTESIAN_POINT('Ctrl Pts',(20.847626691118,19.3509430791855,-9.10249081794541));
#95952=CARTESIAN_POINT('Ctrl Pts',(20.8499366445659,19.2780903583472,-9.10686337051275));
#95953=CARTESIAN_POINT('Ctrl Pts',(20.8522489953706,19.2051620282073,-9.11124046108008));
#95954=CARTESIAN_POINT('Ctrl Pts',(20.8507855897922,19.1321479746869,-9.11561755164741));
#95955=CARTESIAN_POINT('Ctrl Pts',(20.8455696643532,19.0594660018899,-9.11999464221474));
#95956=CARTESIAN_POINT('Ctrl Pts',(20.8403508903038,18.9867443347699,-9.12437412327368));
#95957=CARTESIAN_POINT('Ctrl Pts',(20.8313755754733,18.9143555885064,-9.12875360433262));
#95958=CARTESIAN_POINT('Ctrl Pts',(20.8187186547148,18.8427105341121,-9.13313308539157));
#95959=CARTESIAN_POINT('Ctrl Pts',(20.8060392996493,18.7709384893398,-9.13752032905129));
#95960=CARTESIAN_POINT('Ctrl Pts',(20.7896654157129,18.6999132392689,-9.14190757271102));
#95961=CARTESIAN_POINT('Ctrl Pts',(20.7697225362409,18.6300329136336,-9.14629481637074));
#95962=CARTESIAN_POINT('Ctrl Pts',(20.7561632998913,18.582521025854,-9.14927771930554));
#95963=CARTESIAN_POINT('Ctrl Pts',(20.7409552755656,18.53553808659,-9.15226062224034));
#95964=CARTESIAN_POINT('Ctrl Pts',(20.7241505240927,18.4892037050155,-9.15524352517514));
#95965=CARTESIAN_POINT('Ctrl Pts',(20.6994287137937,18.4210402577035,-9.15963173410604));
#95966=CARTESIAN_POINT('Ctrl Pts',(20.6711526578599,18.3540153233853,-9.16401994303694));
#95967=CARTESIAN_POINT('Ctrl Pts',(20.6394473542677,18.288525404082,-9.16840815196783));
#95968=CARTESIAN_POINT('Ctrl Pts',(20.6077891066029,18.2231326826774,-9.1727898480691));
#95969=CARTESIAN_POINT('Ctrl Pts',(20.5727119232317,18.159270884301,-9.17717154417036));
#95970=CARTESIAN_POINT('Ctrl Pts',(20.5343896652636,18.0973186931568,-9.18155324027163));
#95971=CARTESIAN_POINT('Ctrl Pts',(20.4961124389984,18.0354393007675,-9.18592978753126));
#95972=CARTESIAN_POINT('Ctrl Pts',(20.4545979656273,17.9754654662072,-9.19030633479091));
#95973=CARTESIAN_POINT('Ctrl Pts',(20.410066242825,17.9177517834296,-9.19468288205054));
#95974=CARTESIAN_POINT('Ctrl Pts',(20.365562761394,17.8600747018308,-9.19905665376752));
#95975=CARTESIAN_POINT('Ctrl Pts',(20.3180461211089,17.8046553090191,-9.20343042548449));
#95976=CARTESIAN_POINT('Ctrl Pts',(20.267779095091,17.7518184871436,-9.20780419720146));
#95977=CARTESIAN_POINT('Ctrl Pts',(20.2175273654979,17.6989977436906,-9.21217663796501));
#95978=CARTESIAN_POINT('Ctrl Pts',(20.1645272440668,17.6487583602253,-9.21654907872856));
#95979=CARTESIAN_POINT('Ctrl Pts',(20.1090800563606,17.6013901595109,-9.22092151949211));
#95980=CARTESIAN_POINT('Ctrl Pts',(20.0536314508637,17.5540207475865,-9.22529407205946));
#95981=CARTESIAN_POINT('Ctrl Pts',(19.9957360229245,17.5095229759785,-9.2296666246268));
#95982=CARTESIAN_POINT('Ctrl Pts',(19.9357287478822,17.4681468746582,-9.23403917719414));
#95983=CARTESIAN_POINT('Ctrl Pts',(19.8756591950264,17.4267278316594,-9.23841626776147));
#95984=CARTESIAN_POINT('Ctrl Pts',(19.8134738170563,17.3884372018123,-9.24279335832879));
#95985=CARTESIAN_POINT('Ctrl Pts',(19.7495364985934,17.353481596316,-9.24717044889612));
#95986=CARTESIAN_POINT('Ctrl Pts',(19.6855642615878,17.3185069002662,-9.25154992995506));
#95987=CARTESIAN_POINT('Ctrl Pts',(19.6198386140603,17.286871064273,-9.255929411014));
#95988=CARTESIAN_POINT('Ctrl Pts',(19.5527455102414,17.258733422542,-9.26030889207294));
#95989=CARTESIAN_POINT('Ctrl Pts',(19.4855334843462,17.2305459070299,-9.26469613573266));
#95990=CARTESIAN_POINT('Ctrl Pts',(19.4169496162066,17.2058691314341,-9.26908337939238));
#95991=CARTESIAN_POINT('Ctrl Pts',(19.3473966187371,17.1848130421597,-9.2734706230521));
#95992=CARTESIAN_POINT('Ctrl Pts',(19.3001072825685,17.1704969304131,-9.27645352598692));
#95993=CARTESIAN_POINT('Ctrl Pts',(19.252370250734,17.1578534982272,-9.27943642892174));
#95994=CARTESIAN_POINT('Ctrl Pts',(19.2043142751594,17.1469037128609,-9.28241933185657));
#95995=CARTESIAN_POINT('Ctrl Pts',(19.1336181560408,17.1307952618032,-9.28680754078746));
#95996=CARTESIAN_POINT('Ctrl Pts',(19.0619555004259,17.1182916243426,-9.29119574971836));
#95997=CARTESIAN_POINT('Ctrl Pts',(18.9897273628004,17.1095023159863,-9.29558395864926));
#95998=CARTESIAN_POINT('Ctrl Pts',(18.9176064237069,17.1007260524208,-9.29996565475052));
#95999=CARTESIAN_POINT('Ctrl Pts',(18.8449221435536,17.0956532323251,-9.30434735085179));
#96000=CARTESIAN_POINT('Ctrl Pts',(18.7720870435491,17.0943426405973,-9.30872904695306));
#96001=CARTESIAN_POINT('Ctrl Pts',(18.6993375305835,17.0930335889191,-9.3131055942127));
#96002=CARTESIAN_POINT('Ctrl Pts',(18.6264380297319,17.0954779920626,-9.31748214147234));
#96003=CARTESIAN_POINT('Ctrl Pts',(18.5538057789622,17.1016828017805,-9.32185868873197));
#96004=CARTESIAN_POINT('Ctrl Pts',(18.4812195905104,17.1078836764983,-9.32623246044895));
#96005=CARTESIAN_POINT('Ctrl Pts',(18.4089007953029,17.1178401850896,-9.33060623216592));
#96006=CARTESIAN_POINT('Ctrl Pts',(18.3372648019201,17.1315072294897,-9.33498000388289));
#96007=CARTESIAN_POINT('Ctrl Pts',(18.2656506076106,17.1451701149624,-9.33935244464644));
#96008=CARTESIAN_POINT('Ctrl Pts',(18.1947192761673,17.1625412042304,-9.34372488540999));
#96009=CARTESIAN_POINT('Ctrl Pts',(18.1248776044805,17.1835240057459,-9.34809732617354));
#96010=CARTESIAN_POINT('Ctrl Pts',(18.0550341469345,17.204507343794,-9.35246987874089));
#96011=CARTESIAN_POINT('Ctrl Pts',(17.9862808658674,17.2291024367364,-9.35684243130823));
#96012=CARTESIAN_POINT('Ctrl Pts',(17.9190093127146,17.257162959805,-9.36121498387557));
#96013=CARTESIAN_POINT('Ctrl Pts',(17.8516679426066,17.2852526051428,-9.3655920744429));
#96014=CARTESIAN_POINT('Ctrl Pts',(17.7858118168726,17.3168146752692,-9.36996916501022));
#96015=CARTESIAN_POINT('Ctrl Pts',(17.7218116266779,17.3516550355269,-9.37434625557755));
#96016=CARTESIAN_POINT('Ctrl Pts',(17.6577764836039,17.3865144233984,-9.37872573663649));
#96017=CARTESIAN_POINT('Ctrl Pts',(17.5955997055921,17.4246554136578,-9.38310521769543));
#96018=CARTESIAN_POINT('Ctrl Pts',(17.5356241771988,17.4658397244592,-9.38748469875437));
#96019=CARTESIAN_POINT('Ctrl Pts',(17.4755423425841,17.5070970341751,-9.39187194241409));
#96020=CARTESIAN_POINT('Ctrl Pts',(17.4176699324644,17.5514081430501,-9.3962591860738));
#96021=CARTESIAN_POINT('Ctrl Pts',(17.3623173752297,17.5984939451576,-9.40064642973352));
#96022=CARTESIAN_POINT('Ctrl Pts',(17.3246829700697,17.6305077534137,-9.40362933266835));
#96023=CARTESIAN_POINT('Ctrl Pts',(17.2882126945403,17.6638033925969,-9.40661223560317));
#96024=CARTESIAN_POINT('Ctrl Pts',(17.2529938697635,17.6982839518925,-9.409595138538));
#96025=CARTESIAN_POINT('Ctrl Pts',(17.2019263404371,17.7482809913786,-9.4139203675616));
#96026=CARTESIAN_POINT('Ctrl Pts',(17.1532799906061,17.800978288147,-9.4182455965852));
#96027=CARTESIAN_POINT('Ctrl Pts',(17.1073599831677,17.8561083970887,-9.42257082560881));
#96028=CARTESIAN_POINT('Ctrl Pts',(17.0615168757445,17.9111461823036,-9.42688881138058));
#96029=CARTESIAN_POINT('Ctrl Pts',(17.0183913618817,17.9686083127059,-9.43120679715236));
#96030=CARTESIAN_POINT('Ctrl Pts',(16.9782524640738,18.0281899602688,-9.43552478292413));
#96031=CARTESIAN_POINT('Ctrl Pts',(16.9381523085285,18.0877140993308,-9.43983860095469));
#96032=CARTESIAN_POINT('Ctrl Pts',(16.90103333123,18.1493532901009,-9.44415241898526));
#96033=CARTESIAN_POINT('Ctrl Pts',(16.8671239501056,18.212770159567,-9.44846623701582));
#96034=CARTESIAN_POINT('Ctrl Pts',(16.8332351489704,18.2761485406136,-9.45277743694114));
#96035=CARTESIAN_POINT('Ctrl Pts',(16.8025523148359,18.3413020229706,-9.45708863686646));
#96036=CARTESIAN_POINT('Ctrl Pts',(16.775259218471,18.4078664178513,-9.46139983679178));
#96037=CARTESIAN_POINT('Ctrl Pts',(16.7648137942846,18.433341480517,-9.4630497892695));
#96038=CARTESIAN_POINT('Ctrl Pts',(16.7548643811019,18.459022946162,-9.46469974174723));
#96039=CARTESIAN_POINT('Ctrl Pts',(16.7454194503191,18.4848895418526,-9.46634969422496));
#96040=CARTESIAN_POINT('',(16.6170008950802,19.2129467328109,-8.48905627902251));
#96041=CARTESIAN_POINT('Ctrl Pts',(16.7454193052938,18.48488993903,-9.24346979856369));
#96042=CARTESIAN_POINT('Ctrl Pts',(16.7776919628128,18.3965055643205,-9.23734830228666));
#96043=CARTESIAN_POINT('Ctrl Pts',(16.8158509820645,18.3102897988965,-9.23135282458082));
#96044=CARTESIAN_POINT('Ctrl Pts',(16.8706991286688,18.205832638464,-9.22408567598336));
#96045=CARTESIAN_POINT('Ctrl Pts',(16.8820779852137,18.1850192571194,-9.22263707444487));
#96046=CARTESIAN_POINT('Ctrl Pts',(16.8985836792739,18.1559979252235,-9.22061560309788));
#96047=CARTESIAN_POINT('Ctrl Pts',(16.9034203259883,18.1476277650252,-9.2200323875879));
#96048=CARTESIAN_POINT('Ctrl Pts',(16.9113459932644,18.1341261735529,-9.2190912223094));
#96049=CARTESIAN_POINT('Ctrl Pts',(16.9143997135171,18.1289742771388,-9.21873199941962));
#96050=CARTESIAN_POINT('Ctrl Pts',(16.9208165120184,18.118252558687,-9.21798418250105));
#96051=CARTESIAN_POINT('Ctrl Pts',(16.9241834921427,18.1126851357967,-9.21759573585337));
#96052=CARTESIAN_POINT('Ctrl Pts',(16.9322157232303,18.0995407826206,-9.21667827751021));
#96053=CARTESIAN_POINT('Ctrl Pts',(16.9369032060674,18.0919775297912,-9.2161500884325));
#96054=CARTESIAN_POINT('Ctrl Pts',(16.9526728384797,18.0668878897934,-9.21439677833209));
#96055=CARTESIAN_POINT('Ctrl Pts',(16.9639650076356,18.0494944477354,-9.2131794334003));
#96056=CARTESIAN_POINT('Ctrl Pts',(17.025608981099,17.9575309212493,-9.20672828037623));
#96057=CARTESIAN_POINT('Ctrl Pts',(17.0804234607416,17.8860577695434,-9.20166743052635));
#96058=CARTESIAN_POINT('Ctrl Pts',(17.2287759526704,17.7162246665542,-9.18922997537975));
#96059=CARTESIAN_POINT('Ctrl Pts',(17.3275149905598,17.6229664971023,-9.18201737714853));
#96060=CARTESIAN_POINT('Ctrl Pts',(17.4939961859353,17.4935127703042,-9.17034166014399));
#96061=CARTESIAN_POINT('Ctrl Pts',(17.5559294866221,17.4504548711986,-9.16608160644238));
#96062=CARTESIAN_POINT('Ctrl Pts',(17.6280883177326,17.4058023925679,-9.16105237100025));
#96063=CARTESIAN_POINT('Ctrl Pts',(17.6361910981013,17.4008633592509,-9.16048672669509));
#96064=CARTESIAN_POINT('Ctrl Pts',(17.6482528121486,17.3936219394439,-9.15964295424813));
#96065=CARTESIAN_POINT('Ctrl Pts',(17.6521865813448,17.391277576873,-9.1593674935711));
#96066=CARTESIAN_POINT('Ctrl Pts',(17.6592019857842,17.3871274754381,-9.15887569647239));
#96067=CARTESIAN_POINT('Ctrl Pts',(17.6622806146186,17.3853167536561,-9.15865968854461));
#96068=CARTESIAN_POINT('Ctrl Pts',(17.6689127366999,17.3814385709335,-9.15819393383801));
#96069=CARTESIAN_POINT('Ctrl Pts',(17.6724676221806,17.3793736976805,-9.15794403109686));
#96070=CARTESIAN_POINT('Ctrl Pts',(17.6823047346558,17.3736980178888,-9.15725184780603));
#96071=CARTESIAN_POINT('Ctrl Pts',(17.6885994512144,17.3701091304156,-9.15680819358444));
#96072=CARTESIAN_POINT('Ctrl Pts',(17.7233170773638,17.3505506122997,-9.15435780814619));
#96073=CARTESIAN_POINT('Ctrl Pts',(17.7520858943435,17.3352078172821,-9.15231458744777));
#96074=CARTESIAN_POINT('Ctrl Pts',(17.9264391570361,17.247332778966,-9.13990716426774));
#96075=CARTESIAN_POINT('Ctrl Pts',(18.0796306930682,17.1911128202525,-9.12895411249994));
#96076=CARTESIAN_POINT('Ctrl Pts',(18.3512845594647,17.1256083792614,-9.11070140886584));
#96077=CARTESIAN_POINT('Ctrl Pts',(18.4669069626635,17.107669680694,-9.10326189030197));
#96078=CARTESIAN_POINT('Ctrl Pts',(18.597689201516,17.0983446698309,-9.09525606336226));
#96079=CARTESIAN_POINT('Ctrl Pts',(18.6119522884755,17.0974727232176,-9.09438810351552));
#96080=CARTESIAN_POINT('Ctrl Pts',(18.6346668635054,17.0963148211881,-9.09301381567209));
#96081=CARTESIAN_POINT('Ctrl Pts',(18.6431129328172,17.0959349840369,-9.09250455974448));
#96082=CARTESIAN_POINT('Ctrl Pts',(18.6580129557076,17.0953543164926,-9.09160918708027));
#96083=CARTESIAN_POINT('Ctrl Pts',(18.6644659347314,17.0951323991696,-9.0912224142415));
#96084=CARTESIAN_POINT('Ctrl Pts',(18.6778149088786,17.0947344639315,-9.09042434454801));
#96085=CARTESIAN_POINT('Ctrl Pts',(18.6847109589082,17.0945626218158,-9.09001318308699));
#96086=CARTESIAN_POINT('Ctrl Pts',(18.7024144115813,17.0942080450498,-9.08896046344141));
#96087=CARTESIAN_POINT('Ctrl Pts',(18.7132226811078,17.0940743660874,-9.08832044661547));
#96088=CARTESIAN_POINT('Ctrl Pts',(18.758337611066,17.0938619304738,-9.08565970298393));
#96089=CARTESIAN_POINT('Ctrl Pts',(18.7926437396989,17.0945343061688,-9.08366250668527));
#96090=CARTESIAN_POINT('Ctrl Pts',(18.8819744299117,17.0984590128382,-9.07851821364631));
#96091=CARTESIAN_POINT('Ctrl Pts',(18.9369160423201,17.1030266653512,-9.07541051022945));
#96092=CARTESIAN_POINT('Ctrl Pts',(19.1001558859863,17.1230402340134,-9.06626584779699));
#96093=CARTESIAN_POINT('Ctrl Pts',(19.2075006637055,17.1447366764978,-9.06037761733385));
#96094=CARTESIAN_POINT('Ctrl Pts',(19.3568853721499,17.187188268377,-9.05192245191781));
#96095=CARTESIAN_POINT('Ctrl Pts',(19.4006604436814,17.2011831617325,-9.04941012011181));
#96096=CARTESIAN_POINT('Ctrl Pts',(19.4649345943963,17.2240626462079,-9.04562649873492));
#96097=CARTESIAN_POINT('Ctrl Pts',(19.4858052914449,17.2318652939893,-9.04438267659672));
#96098=CARTESIAN_POINT('Ctrl Pts',(19.5544072084081,17.2587542776347,-9.04023203251112));
#96099=CARTESIAN_POINT('Ctrl Pts',(19.6015628117564,17.2792481541047,-9.03727832061984));
#96100=CARTESIAN_POINT('Ctrl Pts',(19.6550272041254,17.3048363284226,-9.03376033661468));
#96101=CARTESIAN_POINT('Ctrl Pts',(19.6621135787784,17.3082766270149,-9.03329054303779));
#96102=CARTESIAN_POINT('Ctrl Pts',(19.6733812409581,17.3138247816437,-9.03253768488937));
#96103=CARTESIAN_POINT('Ctrl Pts',(19.6775750985913,17.3159071375355,-9.03225616553865));
#96104=CARTESIAN_POINT('Ctrl Pts',(19.6849748705664,17.3196119631652,-9.0317570766856));
#96105=CARTESIAN_POINT('Ctrl Pts',(19.6881836056666,17.3212287025002,-9.0315398671278));
#96106=CARTESIAN_POINT('Ctrl Pts',(19.6949586638533,17.3246640088137,-9.03107954395319));
#96107=CARTESIAN_POINT('Ctrl Pts',(19.6985238934903,17.3264844963357,-9.03083631546905));
#96108=CARTESIAN_POINT('Ctrl Pts',(19.7080942453642,17.3314056084365,-9.03018077323934));
#96109=CARTESIAN_POINT('Ctrl Pts',(19.7140896595904,17.3345248650829,-9.02976731167012));
#96110=CARTESIAN_POINT('Ctrl Pts',(19.743292562101,17.349896500763,-9.02774010467501));
#96111=CARTESIAN_POINT('Ctrl Pts',(19.7662846696949,17.3625503996603,-9.02610291813721));
#96112=CARTESIAN_POINT('Ctrl Pts',(19.8314668289078,17.4000193195941,-9.02135529847618));
#96113=CARTESIAN_POINT('Ctrl Pts',(19.8730379760785,17.4258735837705,-9.01819730213773));
#96114=CARTESIAN_POINT('Ctrl Pts',(19.9939287975699,17.5070017119041,-9.00869692007588));
#96115=CARTESIAN_POINT('Ctrl Pts',(20.0704010149636,17.5662924672909,-9.00226770257484));
#96116=CARTESIAN_POINT('Ctrl Pts',(20.2478288301528,17.7244275561139,-8.98663169643754));
#96117=CARTESIAN_POINT('Ctrl Pts',(20.3434811724073,17.8285532324758,-8.97756398980603));
#96118=CARTESIAN_POINT('Ctrl Pts',(20.4366435887765,17.9528673372903,-8.96807848916196));
#96119=CARTESIAN_POINT('Ctrl Pts',(20.4450930116034,17.9643830946458,-8.96721093976882));
#96120=CARTESIAN_POINT('Ctrl Pts',(20.458356437897,17.9828488204215,-8.96583717693133));
#96121=CARTESIAN_POINT('Ctrl Pts',(20.4632463580122,17.989743482574,-8.96532803903539));
#96122=CARTESIAN_POINT('Ctrl Pts',(20.4717983596235,18.0019559370133,-8.96443280365217));
#96123=CARTESIAN_POINT('Ctrl Pts',(20.4754776279023,18.0072615076762,-8.96404605069599));
#96124=CARTESIAN_POINT('Ctrl Pts',(20.4830379938458,18.0182709064741,-8.9632479547465));
#96125=CARTESIAN_POINT('Ctrl Pts',(20.486915601317,18.0239770470414,-8.96283674747862));
#96126=CARTESIAN_POINT('Ctrl Pts',(20.4967986448851,18.0386745993831,-8.96178377123622));
#96127=CARTESIAN_POINT('Ctrl Pts',(20.502763262808,18.0476933190054,-8.96114354509566));
#96128=CARTESIAN_POINT('Ctrl Pts',(20.5273802987274,18.0855422402812,-8.95848076621297));
#96129=CARTESIAN_POINT('Ctrl Pts',(20.5453996095743,18.1147793486944,-8.95648178994889));
#96130=CARTESIAN_POINT('Ctrl Pts',(20.5904987855703,18.1921056400121,-8.95133187489823));
#96131=CARTESIAN_POINT('Ctrl Pts',(20.6164243500648,18.2408388425351,-8.94822044244671));
#96132=CARTESIAN_POINT('Ctrl Pts',(20.6879870350135,18.389055174631,-8.93906927501836));
#96133=CARTESIAN_POINT('Ctrl Pts',(20.7278486872358,18.491120205809,-8.9331782467684));
#96134=CARTESIAN_POINT('Ctrl Pts',(20.7744406658072,18.6445337473782,-8.92444876472104));
#96135=CARTESIAN_POINT('Ctrl Pts',(20.7874752342794,18.693775446934,-8.92166302191361));
#96136=CARTESIAN_POINT('Ctrl Pts',(20.8021904349712,18.7587566567361,-8.9179561528775));
#96137=CARTESIAN_POINT('Ctrl Pts',(20.8054888854613,18.7741138627915,-8.91707785508989));
#96138=CARTESIAN_POINT('Ctrl Pts',(20.8191178673619,18.8411964544295,-8.91322621911917));
#96139=CARTESIAN_POINT('Ctrl Pts',(20.8276832239092,18.893256782039,-8.91019826495504));
#96140=CARTESIAN_POINT('Ctrl Pts',(20.8353850229947,18.9542013615242,-8.90655266399877));
#96141=CARTESIAN_POINT('Ctrl Pts',(20.836421686787,18.9628315075318,-8.90603407798051));
#96142=CARTESIAN_POINT('Ctrl Pts',(20.8379117366309,18.9759160791536,-8.90524394387023));
#96143=CARTESIAN_POINT('Ctrl Pts',(20.838404200869,18.9803660825203,-8.90497454360295));
#96144=CARTESIAN_POINT('Ctrl Pts',(20.8392632772284,18.9883607565961,-8.90448927829947));
#96145=CARTESIAN_POINT('Ctrl Pts',(20.8396350585575,18.9919048174373,-8.90427370731551));
#96146=CARTESIAN_POINT('Ctrl Pts',(20.8404239564097,18.9996126160795,-8.90380387986917));
#96147=CARTESIAN_POINT('Ctrl Pts',(20.8408376712917,19.0037766028078,-8.90354944046532));
#96148=CARTESIAN_POINT('Ctrl Pts',(20.8419662918357,19.0154888736914,-8.90283206232885));
#96149=CARTESIAN_POINT('Ctrl Pts',(20.8426529866629,19.0230397226283,-8.90236758445281));
#96150=CARTESIAN_POINT('Ctrl Pts',(20.8465378364671,19.0684612085059,-8.89956227655246));
#96151=CARTESIAN_POINT('Ctrl Pts',(20.8487560454108,19.1064061638141,-8.89717169202978));
#96152=CARTESIAN_POINT('Ctrl Pts',(20.8527120497115,19.2320687438044,-8.88914350192847));
#96153=CARTESIAN_POINT('Ctrl Pts',(20.8500194721709,19.3198315215465,-8.88336090979676));
#96154=CARTESIAN_POINT('Ctrl Pts',(20.8257291667823,19.580839202345,-8.86604055281282));
#96155=CARTESIAN_POINT('Ctrl Pts',(20.7881616968977,19.7518832770795,-8.85459338990223));
#96156=CARTESIAN_POINT('Ctrl Pts',(20.7223353818401,19.9381474700761,-8.84243270707467));
#96157=CARTESIAN_POINT('Ctrl Pts',(20.7142945280051,19.9597687776114,-8.84102454826613));
#96158=CARTESIAN_POINT('Ctrl Pts',(20.7024238959517,19.9901583468403,-8.83904951872588));
#96159=CARTESIAN_POINT('Ctrl Pts',(20.6988858279249,19.99903810283,-8.83847292825812));
#96160=CARTESIAN_POINT('Ctrl Pts',(20.6930407961322,20.0134236963241,-8.83753957100816));
#96161=CARTESIAN_POINT('Ctrl Pts',(20.6907705021299,20.0189442013288,-8.83718157202157));
#96162=CARTESIAN_POINT('Ctrl Pts',(20.6859705804276,20.0304769045404,-8.83643403358372));
#96163=CARTESIAN_POINT('Ctrl Pts',(20.6834364511057,20.0364871704023,-8.83604465148605));
#96164=CARTESIAN_POINT('Ctrl Pts',(20.6773439851273,20.0507523192948,-8.83512088843328));
#96165=CARTESIAN_POINT('Ctrl Pts',(20.67376075126,20.0589964822795,-8.83458736156573));
#96166=CARTESIAN_POINT('Ctrl Pts',(20.6615229511862,20.0866692486636,-8.83279743471176));
#96167=CARTESIAN_POINT('Ctrl Pts',(20.6526279636924,20.1059905842415,-8.83154927045854));
#96168=CARTESIAN_POINT('Ctrl Pts',(20.5767424343973,20.2644931444036,-8.82131514099577));
#96169=CARTESIAN_POINT('Ctrl Pts',(20.4949943643222,20.396096532477,-8.81289769681896));
#96170=CARTESIAN_POINT('Ctrl Pts',(20.3152269098503,20.6252547001897,-8.79708100175859));
#96171=CARTESIAN_POINT('Ctrl Pts',(20.2205925139279,20.7244157436544,-8.78969554797914));
#96172=CARTESIAN_POINT('Ctrl Pts',(20.1052750743133,20.8239279618765,-8.78076350901784));
#96173=CARTESIAN_POINT('Ctrl Pts',(20.0933630696947,20.8339799605896,-8.77984139888985));
#96174=CARTESIAN_POINT('Ctrl Pts',(20.0768874881666,20.8475743305974,-8.77856504034232));
#96175=CARTESIAN_POINT('Ctrl Pts',(20.0724184618654,20.8512311924251,-8.77821872873846));
#96176=CARTESIAN_POINT('Ctrl Pts',(20.0652882320271,20.8570170891768,-8.77766594018967));
#96177=CARTESIAN_POINT('Ctrl Pts',(20.062636714158,20.859158091934,-8.77746031881893));
#96178=CARTESIAN_POINT('Ctrl Pts',(20.0571456323476,20.8635700760263,-8.77703435075884));
#96179=CARTESIAN_POINT('Ctrl Pts',(20.0543053918273,20.8658401409539,-8.77681393885086));
#96180=CARTESIAN_POINT('Ctrl Pts',(20.0475167831172,20.8712373412698,-8.77628695102302));
#96181=CARTESIAN_POINT('Ctrl Pts',(20.0435630875839,20.8743577147781,-8.77597989750151));
#96182=CARTESIAN_POINT('Ctrl Pts',(20.0301589877917,20.8848592145884,-8.77493855717006));
#96183=CARTESIAN_POINT('Ctrl Pts',(20.0206572188367,20.8921739879757,-8.77419980455329));
#96184=CARTESIAN_POINT('Ctrl Pts',(19.909385762269,20.9763385764823,-8.76554692061459));
#96185=CARTESIAN_POINT('Ctrl Pts',(19.8009445826786,21.0439142080287,-8.75711384414727));
#96186=CARTESIAN_POINT('Ctrl Pts',(19.5397082052372,21.1756295451071,-8.73778005157247));
#96187=CARTESIAN_POINT('Ctrl Pts',(19.3841059672341,21.2324640429033,-8.72698432156367));
#96188=CARTESIAN_POINT('Ctrl Pts',(19.2004907617823,21.2760986884311,-8.71536072834314));
#96189=CARTESIAN_POINT('Ctrl Pts',(19.1774343868463,21.281172031292,-8.71391912030088));
#96190=CARTESIAN_POINT('Ctrl Pts',(19.144841289946,21.2877743060172,-8.71190568615215));
#96191=CARTESIAN_POINT('Ctrl Pts',(19.1353722527908,21.289625123289,-8.71132362378549));
#96192=CARTESIAN_POINT('Ctrl Pts',(19.1200088330267,21.292519158126,-8.71038381860314));
#96193=CARTESIAN_POINT('Ctrl Pts',(19.1141221777934,21.2936022077952,-8.71002480981884));
#96194=CARTESIAN_POINT('Ctrl Pts',(19.1018244546276,21.2958109117717,-8.70927704807292));
#96195=CARTESIAN_POINT('Ctrl Pts',(19.0954126212641,21.2969319945566,-8.70888844420598));
#96196=CARTESIAN_POINT('Ctrl Pts',(19.0802085171673,21.2995181614255,-8.70796991567415));
#96197=CARTESIAN_POINT('Ctrl Pts',(19.0714119184816,21.3009573318447,-8.70744081896162));
#96198=CARTESIAN_POINT('Ctrl Pts',(19.0426186901461,21.3054815290722,-8.70571639971669));
#96199=CARTESIAN_POINT('Ctrl Pts',(19.0225865079875,21.3083355098344,-8.70452838897926));
#96200=CARTESIAN_POINT('Ctrl Pts',(18.9749201705925,21.3144306384531,-8.70172734196657));
#96201=CARTESIAN_POINT('Ctrl Pts',(18.9472566684265,21.3174151236312,-8.70012226493225));
#96202=CARTESIAN_POINT('Ctrl Pts',(18.7508332121769,21.3346968790879,-8.68885156679276));
#96203=CARTESIAN_POINT('Ctrl Pts',(18.5809587337328,21.3292428538322,-8.67982437037039));
#96204=CARTESIAN_POINT('Ctrl Pts',(18.3107879914595,21.287869456652,-8.66488754094842));
#96205=CARTESIAN_POINT('Ctrl Pts',(18.2093450688665,21.264588689951,-8.65912326933674));
#96206=CARTESIAN_POINT('Ctrl Pts',(18.1007796334846,21.2311026760289,-8.65239231796164));
#96207=CARTESIAN_POINT('Ctrl Pts',(18.0915420559092,21.2281838380001,-8.65181500571073));
#96208=CARTESIAN_POINT('Ctrl Pts',(18.0779311510278,21.2237801649908,-8.65095713719026));
#96209=CARTESIAN_POINT('Ctrl Pts',(18.0735419765791,21.2223442086189,-8.65067937941425));
#96210=CARTESIAN_POINT('Ctrl Pts',(18.0657629051375,21.2197710098002,-8.65018505905114));
#96211=CARTESIAN_POINT('Ctrl Pts',(18.0623711538575,21.2186395287958,-8.64996883797312));
#96212=CARTESIAN_POINT('Ctrl Pts',(18.055109491007,21.2161965919531,-8.64950441099816));
#96213=CARTESIAN_POINT('Ctrl Pts',(18.0512405633225,21.2148825431039,-8.64925605851655));
#96214=CARTESIAN_POINT('Ctrl Pts',(18.0406289361819,21.211244093855,-8.64857242500047));
#96215=CARTESIAN_POINT('Ctrl Pts',(18.0338942132641,21.2088968319668,-8.6481358245441));
#96216=CARTESIAN_POINT('Ctrl Pts',(17.9984775022011,21.1963519351799,-8.64582590217721));
#96217=CARTESIAN_POINT('Ctrl Pts',(17.9700076541501,21.1855711240172,-8.64392087772381));
#96218=CARTESIAN_POINT('Ctrl Pts',(17.791421086757,21.1135046606052,-8.63170745357483));
#96219=CARTESIAN_POINT('Ctrl Pts',(17.6485335709652,21.035757754653,-8.62079146716301));
#96220=CARTESIAN_POINT('Ctrl Pts',(17.4180930384394,20.8736439229559,-8.60236920622934));
#96221=CARTESIAN_POINT('Ctrl Pts',(17.3262604550972,20.7966461369471,-8.59474158559478));
#96222=CARTESIAN_POINT('Ctrl Pts',(17.230271194464,20.7012132334795,-8.58647639043208));
#96223=CARTESIAN_POINT('Ctrl Pts',(17.2192537691211,20.6900130759247,-8.58552258377925));
#96224=CARTESIAN_POINT('Ctrl Pts',(17.2027731923036,20.6728818158145,-8.5840876559297));
#96225=CARTESIAN_POINT('Ctrl Pts',(17.1972177502904,20.6670406243646,-8.58360251809225));
#96226=CARTESIAN_POINT('Ctrl Pts',(17.1873222629956,20.6565164268532,-8.58273572869331));
#96227=CARTESIAN_POINT('Ctrl Pts',(17.1829698066778,20.6518452738702,-8.58235354445013));
#96228=CARTESIAN_POINT('Ctrl Pts',(17.1737790492117,20.6418916438198,-8.58154448539988));
#96229=CARTESIAN_POINT('Ctrl Pts',(17.1689462846402,20.6366041461803,-8.58111784938631));
#96230=CARTESIAN_POINT('Ctrl Pts',(17.1591629009864,20.6257904988035,-8.58025163899237));
#96231=CARTESIAN_POINT('Ctrl Pts',(17.1542143061841,20.6202626468025,-8.57981215285311));
#96232=CARTESIAN_POINT('Ctrl Pts',(17.1324256586633,20.5956645382183,-8.57787095880103));
#96233=CARTESIAN_POINT('Ctrl Pts',(17.1159006587748,20.5763171273516,-8.57638235707686));
#96234=CARTESIAN_POINT('Ctrl Pts',(17.0457286186244,20.4910958580706,-8.56998123679427));
#96235=CARTESIAN_POINT('Ctrl Pts',(16.9957224886823,20.4223212459699,-8.56521401257862));
#96236=CARTESIAN_POINT('Ctrl Pts',(16.9128101519597,20.2925375766098,-8.55672636591948));
#96237=CARTESIAN_POINT('Ctrl Pts',(16.8785074356792,20.2325692289229,-8.55298123514122));
#96238=CARTESIAN_POINT('Ctrl Pts',(16.7878577128624,20.0544101491626,-8.54212537198846));
#96239=CARTESIAN_POINT('Ctrl Pts',(16.7394673000962,19.9325542232887,-8.53503483658883));
#96240=CARTESIAN_POINT('Ctrl Pts',(16.6982006722433,19.7919117099035,-8.52644200519389));
#96241=CARTESIAN_POINT('Ctrl Pts',(16.6939331602703,19.7767424980478,-8.52550991017736));
#96242=CARTESIAN_POINT('Ctrl Pts',(16.6883270785654,19.7559265504045,-8.52422183517333));
#96243=CARTESIAN_POINT('Ctrl Pts',(16.6868416776121,19.7503194304885,-8.52387398124809));
#96244=CARTESIAN_POINT('Ctrl Pts',(16.6845188928791,19.7414034699987,-8.52331933924958));
#96245=CARTESIAN_POINT('Ctrl Pts',(16.6836664224201,19.7380985388894,-8.52311341706873));
#96246=CARTESIAN_POINT('Ctrl Pts',(16.681923128137,19.7312717645712,-8.52268734978282));
#96247=CARTESIAN_POINT('Ctrl Pts',(16.6810333787433,19.7277496959568,-8.5224671418051));
#96248=CARTESIAN_POINT('Ctrl Pts',(16.6789361653896,19.7193569780708,-8.5219415020895));
#96249=CARTESIAN_POINT('Ctrl Pts',(16.677736949469,19.7144843069132,-8.52163559917055));
#96250=CARTESIAN_POINT('Ctrl Pts',(16.6752325974941,19.70415039399,-8.52098537573012));
#96251=CARTESIAN_POINT('Ctrl Pts',(16.6739318448009,19.6986881411743,-8.52064081713856));
#96252=CARTESIAN_POINT('Ctrl Pts',(16.6704195264811,19.6836740509122,-8.51969147471348));
#96253=CARTESIAN_POINT('Ctrl Pts',(16.6682525933811,19.6741120524001,-8.51908436795847));
#96254=CARTESIAN_POINT('Ctrl Pts',(16.6336164633659,19.5161922485616,-8.50902048576369));
#96255=CARTESIAN_POINT('Ctrl Pts',(16.6171414698285,19.3647964194431,-8.49886432390527));
#96256=CARTESIAN_POINT('Ctrl Pts',(16.617000907147,19.2129598110916,-8.48885784168996));
#96257=CARTESIAN_POINT('Ctrl Pts',(16.6170008950802,19.2129467328109,-8.48905627902251));
#96258=CARTESIAN_POINT('Ctrl Pts',(16.6169347305481,19.1409952794385,-8.48473008583425));
#96259=CARTESIAN_POINT('Ctrl Pts',(16.6205409900205,19.0689489014299,-8.480403892646));
#96260=CARTESIAN_POINT('Ctrl Pts',(16.6278220014955,18.9972168420672,-8.47607769945775));
#96261=CARTESIAN_POINT('Ctrl Pts',(16.6350980157525,18.9255340149771,-8.47175447549028));
#96262=CARTESIAN_POINT('Ctrl Pts',(16.6460437282405,18.8541655692476,-8.46743125152281));
#96263=CARTESIAN_POINT('Ctrl Pts',(16.6606094541867,18.7835182523991,-8.46310802755535));
#96264=CARTESIAN_POINT('Ctrl Pts',(16.6751723924898,18.712884456298,-8.45878563098263));
#96265=CARTESIAN_POINT('Ctrl Pts',(16.6933538757663,18.6429720006072,-8.45446323440992));
#96266=CARTESIAN_POINT('Ctrl Pts',(16.715052943236,18.5741783750656,-8.4501408378372));
#96267=CARTESIAN_POINT('Ctrl Pts',(16.7245112167564,18.5441923432816,-8.44825677488816));
#96268=CARTESIAN_POINT('Ctrl Pts',(16.7346371624495,18.5144187239461,-8.44637271193913));
#96269=CARTESIAN_POINT('Ctrl Pts',(16.7454194503191,18.4848895418526,-8.44448864899009));
#96270=CARTESIAN_POINT('Origin',(18.734,19.211,0.));
#96271=CARTESIAN_POINT('',(16.743090251011,18.4840590306076,-7.64456001983877));
#96272=CARTESIAN_POINT('',(16.7454194594376,18.48488951688,-7.86510585860832));
#96273=CARTESIAN_POINT('',(16.7454194503191,18.4848895418526,0.));
#96274=CARTESIAN_POINT('Ctrl Pts',(16.7454194594376,18.48488951688,-7.86510585860832));
#96275=CARTESIAN_POINT('Ctrl Pts',(16.7304230273875,18.5259598686323,-7.86752223947087));
#96276=CARTESIAN_POINT('Ctrl Pts',(16.7166995325181,18.5674931908287,-7.86996740497596));
#96277=CARTESIAN_POINT('Ctrl Pts',(16.6934926739549,18.6457943982049,-7.87462968920152));
#96278=CARTESIAN_POINT('Ctrl Pts',(16.6836949825475,18.6824392626494,-7.87683263687354));
#96279=CARTESIAN_POINT('Ctrl Pts',(16.6731275207629,18.7266952968784,-7.87953974144989));
#96280=CARTESIAN_POINT('Ctrl Pts',(16.6714072151537,18.7340750361865,-7.87999269565253));
#96281=CARTESIAN_POINT('Ctrl Pts',(16.6687987096677,18.7455430926281,-7.8806991972288));
#96282=CARTESIAN_POINT('Ctrl Pts',(16.6678829269928,18.7496251609123,-7.8809511901207));
#96283=CARTESIAN_POINT('Ctrl Pts',(16.6662094739841,18.7571894224134,-7.88141913869248));
#96284=CARTESIAN_POINT('Ctrl Pts',(16.6654484940501,18.7606708243268,-7.88163490202922));
#96285=CARTESIAN_POINT('Ctrl Pts',(16.6637510198014,18.7685316774695,-7.88212296858969));
#96286=CARTESIAN_POINT('Ctrl Pts',(16.6628196353636,18.7729121632044,-7.88239555828951));
#96287=CARTESIAN_POINT('Ctrl Pts',(16.6601202278895,18.7858090473554,-7.88319984325998));
#96288=CARTESIAN_POINT('Ctrl Pts',(16.6583908088322,18.7943333047062,-7.88373366240642));
#96289=CARTESIAN_POINT('Ctrl Pts',(16.6465062920967,18.85482238317,-7.88753626291812));
#96290=CARTESIAN_POINT('Ctrl Pts',(16.6382522074567,18.9071371206529,-7.89090068528666));
#96291=CARTESIAN_POINT('Ctrl Pts',(16.6301911627696,18.974565077764,-7.89528836083577));
#96292=CARTESIAN_POINT('Ctrl Pts',(16.6285719054459,18.9894472536599,-7.89625998535145));
#96293=CARTESIAN_POINT('Ctrl Pts',(16.6204362978251,19.0723914475444,-7.90168906101013));
#96294=CARTESIAN_POINT('Ctrl Pts',(16.6170625898628,19.1407193800489,-7.90621168660917));
#96295=CARTESIAN_POINT('Ctrl Pts',(16.6168557120902,19.3698585925268,-7.92135265286688));
#96296=CARTESIAN_POINT('Ctrl Pts',(16.6350247735365,19.530150830852,-7.93185065292163));
#96297=CARTESIAN_POINT('Ctrl Pts',(16.6765204029089,19.7100311479728,-7.94322215530368));
#96298=CARTESIAN_POINT('Ctrl Pts',(16.6822553139608,19.7331093704894,-7.94467443488116));
#96299=CARTESIAN_POINT('Ctrl Pts',(16.6908695969325,19.7654373693153,-7.94670013382866));
#96300=CARTESIAN_POINT('Ctrl Pts',(16.6934253009023,19.7747708246252,-7.94728395666081));
#96301=CARTESIAN_POINT('Ctrl Pts',(16.6976666647595,19.7898535532205,-7.94822583847425));
#96302=CARTESIAN_POINT('Ctrl Pts',(16.6993128688605,19.7956136910896,-7.94858517434873));
#96303=CARTESIAN_POINT('Ctrl Pts',(16.7027975181071,19.8076136024063,-7.9493330215632));
#96304=CARTESIAN_POINT('Ctrl Pts',(16.7046403188121,19.8138520538656,-7.9497213864207));
#96305=CARTESIAN_POINT('Ctrl Pts',(16.7090695326654,19.8285958470613,-7.95063828588326));
#96306=CARTESIAN_POINT('Ctrl Pts',(16.7116808365843,19.837093629421,-7.95116600065597));
#96307=CARTESIAN_POINT('Ctrl Pts',(16.7205471831887,19.8653124547349,-7.95291608286521));
#96308=CARTESIAN_POINT('Ctrl Pts',(16.7270379030043,19.8849586188442,-7.95413071405547));
#96309=CARTESIAN_POINT('Ctrl Pts',(16.7631661588376,19.9891582412885,-7.9605572763748));
#96310=CARTESIAN_POINT('Ctrl Pts',(16.7978624881053,20.0718661140701,-7.96559778768087));
#96311=CARTESIAN_POINT('Ctrl Pts',(16.8976428101316,20.2729144893916,-7.97797941932697));
#96312=CARTESIAN_POINT('Ctrl Pts',(16.9689850994329,20.3876861982128,-7.98515786453301));
#96313=CARTESIAN_POINT('Ctrl Pts',(17.0971458463586,20.5557114245438,-7.99685012662038));
#96314=CARTESIAN_POINT('Ctrl Pts',(17.1467942811044,20.6139667435398,-8.0011697055739));
#96315=CARTESIAN_POINT('Ctrl Pts',(17.2060220540859,20.6762858438946,-8.00626507637166));
#96316=CARTESIAN_POINT('Ctrl Pts',(17.2126111821523,20.6831261035805,-8.00683120617705));
#96317=CARTESIAN_POINT('Ctrl Pts',(17.2224462457332,20.6931994581455,-8.00767556563659));
#96318=CARTESIAN_POINT('Ctrl Pts',(17.2256571128251,20.6964668355668,-8.00795112243373));
#96319=CARTESIAN_POINT('Ctrl Pts',(17.2313903530047,20.7022632252796,-8.00844302466834));
#96320=CARTESIAN_POINT('Ctrl Pts',(17.2339085462928,20.7047963009055,-8.00865904106725));
#96321=CARTESIAN_POINT('Ctrl Pts',(17.2393381939048,20.7102304618452,-8.00912473813137));
#96322=CARTESIAN_POINT('Ctrl Pts',(17.24225164675,20.713129402627,-8.0093745743581));
#96323=CARTESIAN_POINT('Ctrl Pts',(17.2503213510491,20.7211122806969,-8.0100663901133));
#96324=CARTESIAN_POINT('Ctrl Pts',(17.255495216696,20.7261782191946,-8.01050974096148));
#96325=CARTESIAN_POINT('Ctrl Pts',(17.2840548479455,20.7538565302249,-8.01295538347109));
#96326=CARTESIAN_POINT('Ctrl Pts',(17.3079320812791,20.7759527913074,-8.01499400171965));
#96327=CARTESIAN_POINT('Ctrl Pts',(17.4542419784494,20.9052203437802,-8.02739987358347));
#96328=CARTESIAN_POINT('Ctrl Pts',(17.5881861916158,20.9985328843815,-8.03835713692242));
#96329=CARTESIAN_POINT('Ctrl Pts',(17.8343783743141,21.1308997070506,-8.05661522148226));
#96330=CARTESIAN_POINT('Ctrl Pts',(17.9416765787113,21.1776126605987,-8.06405606215507));
#96331=CARTESIAN_POINT('Ctrl Pts',(18.0658261019792,21.2198396719132,-8.07206311997383));
#96332=CARTESIAN_POINT('Ctrl Pts',(18.0794008219358,21.2243040300073,-8.07293109613394));
#96333=CARTESIAN_POINT('Ctrl Pts',(18.1010776391975,21.2311905266587,-8.07430540489296));
#96334=CARTESIAN_POINT('Ctrl Pts',(18.1091506606512,21.2337020999544,-8.07481466556056));
#96335=CARTESIAN_POINT('Ctrl Pts',(18.1234152327211,21.2380463564476,-8.07571004379625));
#96336=CARTESIAN_POINT('Ctrl Pts',(18.1296004872502,21.2398991891272,-8.07609681749158));
#96337=CARTESIAN_POINT('Ctrl Pts',(18.1424111099261,21.2436729122879,-8.07689488630773));
#96338=CARTESIAN_POINT('Ctrl Pts',(18.1490375911505,21.2455897781057,-8.07730604604789));
#96339=CARTESIAN_POINT('Ctrl Pts',(18.166070899332,21.25042696941,-8.07835875581398));
#96340=CARTESIAN_POINT('Ctrl Pts',(18.1764910177686,21.2533000681174,-8.07899876453877));
#96341=CARTESIAN_POINT('Ctrl Pts',(18.2200727323989,21.2649582772887,-8.08165942876993));
#96342=CARTESIAN_POINT('Ctrl Pts',(18.2534244858284,21.2730167829108,-8.0836565555659));
#96343=CARTESIAN_POINT('Ctrl Pts',(18.3408211698685,21.2918978747048,-8.08880062896024));
#96344=CARTESIAN_POINT('Ctrl Pts',(18.395119756103,21.3014273206944,-8.09190818665326));
#96345=CARTESIAN_POINT('Ctrl Pts',(18.558087554699,21.3235104592055,-8.10105259497788));
#96346=CARTESIAN_POINT('Ctrl Pts',(18.6674213665384,21.3297764860522,-8.10694071621996));
#96347=CARTESIAN_POINT('Ctrl Pts',(18.8224704760556,21.3266448750069,-8.11538396096906));
#96348=CARTESIAN_POINT('Ctrl Pts',(18.868148293439,21.3242402277935,-8.11788440221592));
#96349=CARTESIAN_POINT('Ctrl Pts',(18.9364182366071,21.3184238350479,-8.121683728107));
#96350=CARTESIAN_POINT('Ctrl Pts',(18.9590922383782,21.3161227506819,-8.12295594650712));
#96351=CARTESIAN_POINT('Ctrl Pts',(18.9827476317918,21.3133355293284,-8.12429799866372));
#96352=CARTESIAN_POINT('Ctrl Pts',(18.9837710919019,21.3132141812487,-8.12435609206462));
#96353=CARTESIAN_POINT('Ctrl Pts',(19.002979573237,21.3109224734936,-8.12544694983261));
#96354=CARTESIAN_POINT('Ctrl Pts',(19.0211352936121,21.3085170305476,-8.12648727956017));
#96355=CARTESIAN_POINT('Ctrl Pts',(19.0724306378924,21.3010424776495,-8.12945840902469));
#96356=CARTESIAN_POINT('Ctrl Pts',(19.1054826762905,21.2954215488278,-8.13141066199488));
#96357=CARTESIAN_POINT('Ctrl Pts',(19.1451886509711,21.2876947135554,-8.13381674319363));
#96358=CARTESIAN_POINT('Ctrl Pts',(19.1519854655372,21.2863373671765,-8.13423077766921));
#96359=CARTESIAN_POINT('Ctrl Pts',(19.1631327442401,21.2840542373189,-8.13491356382834));
#96360=CARTESIAN_POINT('Ctrl Pts',(19.1674872336785,21.2831480643169,-8.13518122117521));
#96361=CARTESIAN_POINT('Ctrl Pts',(19.1753236438988,21.2814915185107,-8.13566464617708));
#96362=CARTESIAN_POINT('Ctrl Pts',(19.1788065507276,21.2807460759703,-8.13588012973324));
#96363=CARTESIAN_POINT('Ctrl Pts',(19.186400010301,21.279100804254,-8.13635130159189));
#96364=CARTESIAN_POINT('Ctrl Pts',(19.1905097155735,21.2781975195304,-8.13660718127647));
#96365=CARTESIAN_POINT('Ctrl Pts',(19.2021221970862,21.2756088591033,-8.13733261939392));
#96366=CARTESIAN_POINT('Ctrl Pts',(19.2096184317918,21.2738948678181,-8.13780377169432));
#96367=CARTESIAN_POINT('Ctrl Pts',(19.2560133768138,21.2630204827113,-8.140736802999));
#96368=CARTESIAN_POINT('Ctrl Pts',(19.2946528830285,21.2528016295424,-8.14325373050464));
#96369=CARTESIAN_POINT('Ctrl Pts',(19.4980638283956,21.1927973433519,-8.1568181688231));
#96370=CARTESIAN_POINT('Ctrl Pts',(19.6565953930106,21.12414827831,-8.16843474910766));
#96371=CARTESIAN_POINT('Ctrl Pts',(19.8911270319894,20.986584227413,-8.18607030865468));
#96372=CARTESIAN_POINT('Ctrl Pts',(19.9735159336012,20.9300833420083,-8.19238237733184));
#96373=CARTESIAN_POINT('Ctrl Pts',(20.0625529989311,20.8592812133051,-8.19932540923305));
#96374=CARTESIAN_POINT('Ctrl Pts',(20.0733975307582,20.8504811064398,-8.20017343930853));
#96375=CARTESIAN_POINT('Ctrl Pts',(20.0905936595884,20.8362423005961,-8.20152220885994));
#96376=CARTESIAN_POINT('Ctrl Pts',(20.0970013530965,20.830872281222,-8.20202570948833));
#96377=CARTESIAN_POINT('Ctrl Pts',(20.1082896414763,20.8212976357773,-8.20291440908608));
#96378=CARTESIAN_POINT('Ctrl Pts',(20.113183140604,20.8171084523018,-8.20330023336711));
#96379=CARTESIAN_POINT('Ctrl Pts',(20.1233072365092,20.8083611164578,-8.20409968921891));
#96380=CARTESIAN_POINT('Ctrl Pts',(20.128534706106,20.8037994503438,-8.20451316885232));
#96381=CARTESIAN_POINT('Ctrl Pts',(20.1419842492729,20.791945958442,-8.20557884831614));
#96382=CARTESIAN_POINT('Ctrl Pts',(20.1501722045024,20.7846156022991,-8.20622943165243));
#96383=CARTESIAN_POINT('Ctrl Pts',(20.1848730068321,20.753059118047,-8.20899488465013));
#96384=CARTESIAN_POINT('Ctrl Pts',(20.210825083705,20.728223352771,-8.2110837944121));
#96385=CARTESIAN_POINT('Ctrl Pts',(20.2775057749932,20.6610779729768,-8.21652053183953));
#96386=CARTESIAN_POINT('Ctrl Pts',(20.3171285775791,20.6177127884411,-8.2198228258352));
#96387=CARTESIAN_POINT('Ctrl Pts',(20.4628437274544,20.444267609799,-8.23238322920137));
#96388=CARTESIAN_POINT('Ctrl Pts',(20.5551182790621,20.3034150048165,-8.24121620710234));
#96389=CARTESIAN_POINT('Ctrl Pts',(20.6314960346413,20.1497291724357,-8.25085098543962));
#96390=CARTESIAN_POINT('Ctrl Pts',(20.6331907606959,20.1462957365846,-8.25106625556775));
#96391=CARTESIAN_POINT('Ctrl Pts',(20.6577113722162,20.0962766791371,-8.25420295792358));
#96392=CARTESIAN_POINT('Ctrl Pts',(20.678824703109,20.0488759881436,-8.25718286206112));
#96393=CARTESIAN_POINT('Ctrl Pts',(20.7014034567775,19.9927209021678,-8.26077501603406));
#96394=CARTESIAN_POINT('Ctrl Pts',(20.7045833399969,19.984669971603,-8.26129148001002));
#96395=CARTESIAN_POINT('Ctrl Pts',(20.7093300393406,19.9724329986888,-8.26207900987483));
#96396=CARTESIAN_POINT('Ctrl Pts',(20.7109331643739,19.9682610108606,-8.26234794909308));
#96397=CARTESIAN_POINT('Ctrl Pts',(20.7137905577849,19.9607539883235,-8.26283272581797));
#96398=CARTESIAN_POINT('Ctrl Pts',(20.7150496273832,19.9574208392315,-8.26304827190273));
#96399=CARTESIAN_POINT('Ctrl Pts',(20.7177712210673,19.950160539718,-8.26351844693558));
#96400=CARTESIAN_POINT('Ctrl Pts',(20.7192304823261,19.9462322710219,-8.26377326102612));
#96401=CARTESIAN_POINT('Ctrl Pts',(20.7233068825824,19.9351581593428,-8.26449273281755));
#96402=CARTESIAN_POINT('Ctrl Pts',(20.7258971365562,19.9280025844964,-8.26495894379259));
#96403=CARTESIAN_POINT('Ctrl Pts',(20.7413585026825,19.8845601303327,-8.26779669235938));
#96404=CARTESIAN_POINT('Ctrl Pts',(20.7532754284984,19.847944048314,-8.27021930295199));
#96405=CARTESIAN_POINT('Ctrl Pts',(20.7896151056037,19.7249888869659,-8.2784098183297));
#96406=CARTESIAN_POINT('Ctrl Pts',(20.8095471149129,19.637427285596,-8.28432867735865));
#96407=CARTESIAN_POINT('Ctrl Pts',(20.8512543218205,19.3794525057696,-8.30159711793062));
#96408=CARTESIAN_POINT('Ctrl Pts',(20.8579468921458,19.2072970879756,-8.31284884369033));
#96409=CARTESIAN_POINT('Ctrl Pts',(20.8418510982953,19.0130266556424,-8.32485059558149));
#96410=CARTESIAN_POINT('Ctrl Pts',(20.8395493863457,18.9898856698573,-8.32627034371171));
#96411=CARTESIAN_POINT('Ctrl Pts',(20.8357605984607,18.9572612732565,-8.32825867100352));
#96412=CARTESIAN_POINT('Ctrl Pts',(20.8345896727262,18.9477434972117,-8.32883714757774));
#96413=CARTESIAN_POINT('Ctrl Pts',(20.8325842947206,18.9323090342857,-8.32977272625912));
#96414=CARTESIAN_POINT('Ctrl Pts',(20.8317894031988,18.9263874258171,-8.33013107217587));
#96415=CARTESIAN_POINT('Ctrl Pts',(20.8300749643775,18.9140130889018,-8.33087868039416));
#96416=CARTESIAN_POINT('Ctrl Pts',(20.8291506631589,18.9075610740465,-8.33126778821291));
#96417=CARTESIAN_POINT('Ctrl Pts',(20.8268846346344,18.8922473793663,-8.33218971753388));
#96418=CARTESIAN_POINT('Ctrl Pts',(20.8255163934888,18.883389703184,-8.33272169411313));
#96419=CARTESIAN_POINT('Ctrl Pts',(20.8207363892071,18.8536962049064,-8.33450092963488));
#96420=CARTESIAN_POINT('Ctrl Pts',(20.8170691270874,18.8329023680257,-8.33574008851171));
#96421=CARTESIAN_POINT('Ctrl Pts',(20.7955578853588,18.7207658163982,-8.34239075009146));
#96422=CARTESIAN_POINT('Ctrl Pts',(20.7720154745158,18.6306153875568,-8.34761651828512));
#96423=CARTESIAN_POINT('Ctrl Pts',(20.6936297918942,18.3951642806919,-8.36128220548598));
#96424=CARTESIAN_POINT('Ctrl Pts',(20.6286327564428,18.2538704220254,-8.3694817678823));
#96425=CARTESIAN_POINT('Ctrl Pts',(20.5213551863295,18.075266506892,-8.38119932045691));
#96426=CARTESIAN_POINT('Ctrl Pts',(20.4922016398175,18.0306377222315,-8.38425744364819));
#96427=CARTESIAN_POINT('Ctrl Pts',(20.4563594469984,17.9800479644633,-8.38793672734164));
#96428=CARTESIAN_POINT('Ctrl Pts',(20.4512766133898,17.9729668802289,-8.3884567441382));
#96429=CARTESIAN_POINT('Ctrl Pts',(20.4435140126833,17.9622922949229,-8.38924863379105));
#96430=CARTESIAN_POINT('Ctrl Pts',(20.4408662513414,17.9586754847638,-8.3895183445052));
#96431=CARTESIAN_POINT('Ctrl Pts',(20.4360927148667,17.9521981523849,-8.39000393956645));
#96432=CARTESIAN_POINT('Ctrl Pts',(20.4339711870085,17.9493345670877,-8.3902195280915));
#96433=CARTESIAN_POINT('Ctrl Pts',(20.4293453335256,17.9431235562909,-8.39068912492562));
#96434=CARTESIAN_POINT('Ctrl Pts',(20.4268383533856,17.9397782313739,-8.39094331470733));
#96435=CARTESIAN_POINT('Ctrl Pts',(20.4197678472627,17.9304013231137,-8.39165929895434));
#96436=CARTESIAN_POINT('Ctrl Pts',(20.4151819356171,17.9243868096831,-8.39212262318725));
#96437=CARTESIAN_POINT('Ctrl Pts',(20.3875576544783,17.8885568771406,-8.39490660566813));
#96438=CARTESIAN_POINT('Ctrl Pts',(20.3637603617581,17.8593382495859,-8.3972761613492));
#96439=CARTESIAN_POINT('Ctrl Pts',(20.2828441327697,17.765233076241,-8.40519900828723));
#96440=CARTESIAN_POINT('Ctrl Pts',(20.222532794194,17.7032107692611,-8.41089346404166));
#96441=CARTESIAN_POINT('Ctrl Pts',(20.0282225120172,17.5264390366334,-8.42824879052193));
#96442=CARTESIAN_POINT('Ctrl Pts',(19.8835097537651,17.4245485897652,-8.43982447440901));
#96443=CARTESIAN_POINT('Ctrl Pts',(19.7075711575063,17.331006923692,-8.45208853724492));
#96444=CARTESIAN_POINT('Ctrl Pts',(19.687151087674,17.3205720498639,-8.45348825398657));
#96445=CARTESIAN_POINT('Ctrl Pts',(19.6580039328834,17.3062699225899,-8.45545360106586));
#96446=CARTESIAN_POINT('Ctrl Pts',(19.6494146069852,17.3021270241979,-8.45602882258404));
#96447=CARTESIAN_POINT('Ctrl Pts',(19.6354074198043,17.2954872111137,-8.45696056837813));
#96448=CARTESIAN_POINT('Ctrl Pts',(19.6300065530493,17.2929549434672,-8.45731831645653));
#96449=CARTESIAN_POINT('Ctrl Pts',(19.6186744877923,17.2877000647936,-8.45806580946481));
#96450=CARTESIAN_POINT('Ctrl Pts',(19.6127412494342,17.2849819813592,-8.45845539494049));
#96451=CARTESIAN_POINT('Ctrl Pts',(19.5985882225104,17.2785773343802,-8.45938050958642));
#96452=CARTESIAN_POINT('Ctrl Pts',(19.5903572422829,17.274915696434,-8.45991517790893));
#96453=CARTESIAN_POINT('Ctrl Pts',(19.5625100943552,17.2627399310947,-8.46171300575328));
#96454=CARTESIAN_POINT('Ctrl Pts',(19.542787970593,17.2544703323282,-8.46296782850978));
#96455=CARTESIAN_POINT('Ctrl Pts',(19.4344865306406,17.2109764472891,-8.46976380966929));
#96456=CARTESIAN_POINT('Ctrl Pts',(19.3437260174913,17.1814648699934,-8.47510959358759));
#96457=CARTESIAN_POINT('Ctrl Pts',(19.0858065025412,17.1164738235139,-8.48974106747186));
#96458=CARTESIAN_POINT('Ctrl Pts',(18.9159230842882,17.0949424352635,-8.49871735792444));
#96459=CARTESIAN_POINT('Ctrl Pts',(18.7086783881462,17.0938343522178,-8.51055653629938));
#96460=CARTESIAN_POINT('Ctrl Pts',(18.672041428243,17.094589752273,-8.51268514326574));
#96461=CARTESIAN_POINT('Ctrl Pts',(18.6283201407103,17.0966273643405,-8.5152873411395));
#96462=CARTESIAN_POINT('Ctrl Pts',(18.6211970346115,17.0969954203394,-8.51571326305379));
#96463=CARTESIAN_POINT('Ctrl Pts',(18.6095737373756,17.0976549166907,-8.51641168402998));
#96464=CARTESIAN_POINT('Ctrl Pts',(18.6050723113554,17.0979247561399,-8.51668300189247));
#96465=CARTESIAN_POINT('Ctrl Pts',(18.5970131019333,17.0984337158775,-8.51717031272833));
#96466=CARTESIAN_POINT('Ctrl Pts',(18.5934550311703,17.0986674441479,-8.51738600072837));
#96467=CARTESIAN_POINT('Ctrl Pts',(18.5857471058617,17.0991933361385,-8.51785444316563));
#96468=CARTESIAN_POINT('Ctrl Pts',(18.5815975733909,17.0994887388824,-8.51810737162843));
#96469=CARTESIAN_POINT('Ctrl Pts',(18.5699997810276,17.1003487441403,-8.5188163272104));
#96470=CARTESIAN_POINT('Ctrl Pts',(18.5625536846635,17.1009405333451,-8.51927383721742));
#96471=CARTESIAN_POINT('Ctrl Pts',(18.5191536764231,17.1046210490033,-8.52195350479844));
#96472=CARTESIAN_POINT('Ctrl Pts',(18.4832826039097,17.1085890849786,-8.52422047812991));
#96473=CARTESIAN_POINT('Ctrl Pts',(18.3679222706884,17.1243442570112,-8.53164286914908));
#96474=CARTESIAN_POINT('Ctrl Pts',(18.2890001702411,17.139739870969,-8.53692186007904));
#96475=CARTESIAN_POINT('Ctrl Pts',(18.0316459477705,17.2053323900169,-8.5544565935549));
#96476=CARTESIAN_POINT('Ctrl Pts',(17.8588819769178,17.2744567631978,-8.56666089245527));
#96477=CARTESIAN_POINT('Ctrl Pts',(17.6780092373775,17.376044322465,-8.57941891882172));
#96478=CARTESIAN_POINT('Ctrl Pts',(17.6588830642299,17.387184641459,-8.58076925482921));
#96479=CARTESIAN_POINT('Ctrl Pts',(17.6320449020001,17.4033858566895,-8.58266649424393));
#96480=CARTESIAN_POINT('Ctrl Pts',(17.6241863729939,17.4082000536342,-8.58322233113494));
#96481=CARTESIAN_POINT('Ctrl Pts',(17.6108614664833,17.4164831450663,-8.58416540336677));
#96482=CARTESIAN_POINT('Ctrl Pts',(17.6053791590805,17.4199260464738,-8.58455358817342));
#96483=CARTESIAN_POINT('Ctrl Pts',(17.5944481450155,17.4268608659521,-8.58532796368129));
#96484=CARTESIAN_POINT('Ctrl Pts',(17.5889994863794,17.4303527286176,-8.58571415084382));
#96485=CARTESIAN_POINT('Ctrl Pts',(17.5780647883964,17.4374313528938,-8.58648960508637));
#96486=CARTESIAN_POINT('Ctrl Pts',(17.572579223143,17.4410187176184,-8.58687884406315));
#96487=CARTESIAN_POINT('Ctrl Pts',(17.5527646003415,17.4541085561743,-8.58828571269778));
#96488=CARTESIAN_POINT('Ctrl Pts',(17.5385345249328,17.4637601942952,-8.58929774595583));
#96489=CARTESIAN_POINT('Ctrl Pts',(17.4031522189394,17.5580124148171,-8.59894690493272));
#96490=CARTESIAN_POINT('Ctrl Pts',(17.2910488158158,17.6549076223824,-8.60705901703929));
#96491=CARTESIAN_POINT('Ctrl Pts',(17.0877647716834,17.8716328738512,-8.62320800980143));
#96492=CARTESIAN_POINT('Ctrl Pts',(16.9974183756671,17.9910548564931,-8.63121057716827));
#96493=CARTESIAN_POINT('Ctrl Pts',(16.9122949762965,18.1324237944112,-8.6408855694134));
#96494=CARTESIAN_POINT('Ctrl Pts',(16.904341119639,18.1459722193693,-8.6418149038339));
#96495=CARTESIAN_POINT('Ctrl Pts',(16.8936618097339,18.1646358622268,-8.64309973931608));
#96496=CARTESIAN_POINT('Ctrl Pts',(16.8908052566807,18.1696759871327,-8.64344716685032));
#96497=CARTESIAN_POINT('Ctrl Pts',(16.8862994306781,18.1777027310987,-8.64400129639221));
#96498=CARTESIAN_POINT('Ctrl Pts',(16.8846366033134,18.1806817644988,-8.64420713536483));
#96499=CARTESIAN_POINT('Ctrl Pts',(16.8812176602314,18.1868419043327,-8.64463317458206));
#96500=CARTESIAN_POINT('Ctrl Pts',(16.8794625363721,18.1900235072734,-8.64485343834559));
#96501=CARTESIAN_POINT('Ctrl Pts',(16.8753006132713,18.1976141787908,-8.64537944795096));
#96502=CARTESIAN_POINT('Ctrl Pts',(16.8729013065442,18.2020273121253,-8.64568566673566));
#96503=CARTESIAN_POINT('Ctrl Pts',(16.8648653629559,18.2169343069357,-8.64672128030589));
#96504=CARTESIAN_POINT('Ctrl Pts',(16.8593017156538,18.2274669699382,-8.6474550757251));
#96505=CARTESIAN_POINT('Ctrl Pts',(16.8124639527543,18.3179779859893,-8.65377488464604));
#96506=CARTESIAN_POINT('Ctrl Pts',(16.7762596204173,18.400428355294,-8.65962160080874));
#96507=CARTESIAN_POINT('Ctrl Pts',(16.745419494333,18.4848894213129,-8.66553665550751));
#96508=CARTESIAN_POINT('',(16.6172480928634,19.2105366953923,-7.68905625083793));
#96509=CARTESIAN_POINT('Ctrl Pts',(16.7454194503191,18.4848895418526,-8.44448864899009));
#96510=CARTESIAN_POINT('Ctrl Pts',(16.7701773779263,18.4170856247798,-8.44016252686615));
#96511=CARTESIAN_POINT('Ctrl Pts',(16.7983989656721,18.3505720253294,-8.43583640474221));
#96512=CARTESIAN_POINT('Ctrl Pts',(16.8299125180811,18.2857217385025,-8.43151028261827));
#96513=CARTESIAN_POINT('Ctrl Pts',(16.8614397445838,18.2208433123886,-8.42718228334008));
#96514=CARTESIAN_POINT('Ctrl Pts',(16.8962615406801,18.1576300696997,-8.42285428406188));
#96515=CARTESIAN_POINT('Ctrl Pts',(16.934160677018,18.0964294946269,-8.41852628478368));
#96516=CARTESIAN_POINT('Ctrl Pts',(16.9721294358797,18.0351164911742,-8.41419033476406));
#96517=CARTESIAN_POINT('Ctrl Pts',(17.0131865452822,17.9758239484975,-8.40985438474445));
#96518=CARTESIAN_POINT('Ctrl Pts',(17.0570722997309,17.9188690128048,-8.40551843472483));
#96519=CARTESIAN_POINT('Ctrl Pts',(17.097271661252,17.8666982781533,-8.40154670347478));
#96520=CARTESIAN_POINT('Ctrl Pts',(17.1398437335012,17.8164887482056,-8.39757497222472));
#96521=CARTESIAN_POINT('Ctrl Pts',(17.1845622179524,17.7684565657966,-8.39360324097467));
#96522=CARTESIAN_POINT('Ctrl Pts',(17.2339699045481,17.715387705255,-8.38921503204377));
#96523=CARTESIAN_POINT('Ctrl Pts',(17.2862036327226,17.6647565409339,-8.38482682311287));
#96524=CARTESIAN_POINT('Ctrl Pts',(17.3409933109755,17.6168791249303,-8.38043861418197));
#96525=CARTESIAN_POINT('Ctrl Pts',(17.3957016722614,17.5690727669504,-8.37605691808071));
#96526=CARTESIAN_POINT('Ctrl Pts',(17.4529580928698,17.5240123587828,-8.37167522197945));
#96527=CARTESIAN_POINT('Ctrl Pts',(17.5124544762691,17.4819784462151,-8.36729352587818));
#96528=CARTESIAN_POINT('Ctrl Pts',(17.5718809466829,17.4399939268397,-8.36291697861854));
#96529=CARTESIAN_POINT('Ctrl Pts',(17.6335417591175,17.4010291152648,-8.35854043135889));
#96530=CARTESIAN_POINT('Ctrl Pts',(17.6970957742214,17.3653243441595,-8.35416388409925));
#96531=CARTESIAN_POINT('Ctrl Pts',(17.7606094842925,17.3296422165011,-8.34979011238228));
#96532=CARTESIAN_POINT('Ctrl Pts',(17.826013595285,17.29721626287,-8.3454163406653));
#96533=CARTESIAN_POINT('Ctrl Pts',(17.8929392167475,17.2682427431934,-8.34104256894832));
#96534=CARTESIAN_POINT('Ctrl Pts',(17.9598444725186,17.2392780402562,-8.33667012818477));
#96535=CARTESIAN_POINT('Ctrl Pts',(18.0282698771516,17.2137638770621,-8.33229768742122));
#96536=CARTESIAN_POINT('Ctrl Pts',(18.0978247669405,17.1918491703586,-8.32792524665767));
#96537=CARTESIAN_POINT('Ctrl Pts',(18.1673814352556,17.1699339032935,-8.32355269409032));
#96538=CARTESIAN_POINT('Ctrl Pts',(18.2380671853845,17.1516184185037,-8.31918014152297));
#96539=CARTESIAN_POINT('Ctrl Pts',(18.3094759435897,17.1370018501626,-8.31480758895562));
#96540=CARTESIAN_POINT('Ctrl Pts',(18.3809588124976,17.1223701121955,-8.31043049838829));
#96541=CARTESIAN_POINT('Ctrl Pts',(18.4531657140458,17.1114450521883,-8.30605340782097));
#96542=CARTESIAN_POINT('Ctrl Pts',(18.5256809453885,17.1042745381788,-8.30167631725364));
#96543=CARTESIAN_POINT('Ctrl Pts',(18.5982357799905,17.0971001080854,-8.2972968361947));
#96544=CARTESIAN_POINT('Ctrl Pts',(18.6710987974679,17.0936843291133,-8.29291735513576));
#96545=CARTESIAN_POINT('Ctrl Pts',(18.7438524696358,17.0940229267084,-8.28853787407681));
#96546=CARTESIAN_POINT('Ctrl Pts',(18.8167350971993,17.0943621244655,-8.28415063041709));
#96547=CARTESIAN_POINT('Ctrl Pts',(18.8895075103792,17.0984689605669,-8.27976338675737));
#96548=CARTESIAN_POINT('Ctrl Pts',(18.9617560690979,17.1062871518924,-8.27537614309765));
#96549=CARTESIAN_POINT('Ctrl Pts',(19.0108781271719,17.1116027686346,-8.27239324016285));
#96550=CARTESIAN_POINT('Ctrl Pts',(19.0597581560643,17.1186329436866,-8.26941033722804));
#96551=CARTESIAN_POINT('Ctrl Pts',(19.1082694567067,17.1273466282089,-8.26642743429323));
#96552=CARTESIAN_POINT('Ctrl Pts',(19.1796354137562,17.1401655060193,-8.26203922536233));
#96553=CARTESIAN_POINT('Ctrl Pts',(19.2504813367647,17.1566801162964,-8.25765101643143));
#96554=CARTESIAN_POINT('Ctrl Pts',(19.3203952805281,17.1768344278367,-8.25326280750054));
#96555=CARTESIAN_POINT('Ctrl Pts',(19.3902054604072,17.1969588270371,-8.24888111139927));
#96556=CARTESIAN_POINT('Ctrl Pts',(19.4590859472334,17.2207120714409,-8.244499415298));
#96557=CARTESIAN_POINT('Ctrl Pts',(19.5266340795879,17.2479869547362,-8.24011771919673));
#96558=CARTESIAN_POINT('Ctrl Pts',(19.5941028375111,17.2752297878729,-8.23574117193709));
#96559=CARTESIAN_POINT('Ctrl Pts',(19.6602419060114,17.3059858596158,-8.23136462467746));
#96560=CARTESIAN_POINT('Ctrl Pts',(19.7246645510869,17.3400984132724,-8.22698807741783));
#96561=CARTESIAN_POINT('Ctrl Pts',(19.7890463402572,17.3741893332433,-8.22261430570085));
#96562=CARTESIAN_POINT('Ctrl Pts',(19.8517134405357,17.4116322864694,-8.21824053398388));
#96563=CARTESIAN_POINT('Ctrl Pts',(19.9123011549776,17.4522233262354,-8.2138667622669));
#96564=CARTESIAN_POINT('Ctrl Pts',(19.9728704323745,17.4928020140117,-8.20949432150335));
#96565=CARTESIAN_POINT('Ctrl Pts',(20.0313611796543,17.5365266181305,-8.2051218807398));
#96566=CARTESIAN_POINT('Ctrl Pts',(20.0874367225443,17.5831492580496,-8.20074943997625));
#96567=CARTESIAN_POINT('Ctrl Pts',(20.1435136992921,17.6297730901147,-8.19637688740891));
#96568=CARTESIAN_POINT('Ctrl Pts',(20.1971749793953,17.6792947951744,-8.19200433484157));
#96569=CARTESIAN_POINT('Ctrl Pts',(20.2481174066903,17.7314265889259,-8.18763178227423));
#96570=CARTESIAN_POINT('Ctrl Pts',(20.2991127039579,17.7836124870194,-8.18325469170691));
#96571=CARTESIAN_POINT('Ctrl Pts',(20.3473831767916,17.8384135364598,-8.17887760113958));
#96572=CARTESIAN_POINT('Ctrl Pts',(20.3926635636808,17.895506107001,-8.17450051057226));
#96573=CARTESIAN_POINT('Ctrl Pts',(20.43796867987,17.952629857914,-8.17012102951332));
#96574=CARTESIAN_POINT('Ctrl Pts',(20.4802801788309,18.0120472284178,-8.16574154845437));
#96575=CARTESIAN_POINT('Ctrl Pts',(20.5193756546996,18.073404829649,-8.16136206739543));
#96576=CARTESIAN_POINT('Ctrl Pts',(20.5585404270369,18.1348711868165,-8.15697482373571));
#96577=CARTESIAN_POINT('Ctrl Pts',(20.5944775548128,18.1982842223061,-8.15258758007599));
#96578=CARTESIAN_POINT('Ctrl Pts',(20.6270104676959,18.263265665287,-8.14820033641627));
#96579=CARTESIAN_POINT('Ctrl Pts',(20.6491297135924,18.3074467849172,-8.14521743348144));
#96580=CARTESIAN_POINT('Ctrl Pts',(20.6696762814795,18.3523524542015,-8.14223453054662));
#96581=CARTESIAN_POINT('Ctrl Pts',(20.688607698715,18.3978593331261,-8.13925162761179));
#96582=CARTESIAN_POINT('Ctrl Pts',(20.7164580900963,18.4648054245267,-8.1348634186809));
#96583=CARTESIAN_POINT('Ctrl Pts',(20.7409194707723,18.5333146794851,-8.13047520975));
#96584=CARTESIAN_POINT('Ctrl Pts',(20.7618159759921,18.6030103886487,-8.1260870008191));
#96585=CARTESIAN_POINT('Ctrl Pts',(20.7826814673335,18.6726026578242,-8.12170530471784));
#96586=CARTESIAN_POINT('Ctrl Pts',(20.7999924489196,18.7433774273515,-8.11732360861657));
#96587=CARTESIAN_POINT('Ctrl Pts',(20.813621111304,18.8149380939565,-8.1129419125153));
#96588=CARTESIAN_POINT('Ctrl Pts',(20.8272337589254,18.8864146710833,-8.10856536525567));
#96589=CARTESIAN_POINT('Ctrl Pts',(20.8371725931962,18.9586748392569,-8.10418881799603));
#96590=CARTESIAN_POINT('Ctrl Pts',(20.8433600899068,19.0313085669594,-8.09981227073639));
#96591=CARTESIAN_POINT('Ctrl Pts',(20.849543662597,19.1038962314074,-8.09543849901942));
#96592=CARTESIAN_POINT('Ctrl Pts',(20.8519805772149,19.1768565058775,-8.09106472730244));
#96593=CARTESIAN_POINT('Ctrl Pts',(20.8506449171335,19.2497723454649,-8.08669095558546));
#96594=CARTESIAN_POINT('Ctrl Pts',(20.8493096634979,19.3226659965175,-8.08231851482191));
#96595=CARTESIAN_POINT('Ctrl Pts',(20.8442041231404,19.3955147575252,-8.07794607405835));
#96596=CARTESIAN_POINT('Ctrl Pts',(20.8353544889708,19.4679013656687,-8.07357363329479));
#96597=CARTESIAN_POINT('Ctrl Pts',(20.826504628515,19.5402898247457,-8.06920108072744));
#96598=CARTESIAN_POINT('Ctrl Pts',(20.8139105446927,19.6122156289264,-8.06482852816009));
#96599=CARTESIAN_POINT('Ctrl Pts',(20.797650125878,19.6832680996678,-8.06045597559274));
#96600=CARTESIAN_POINT('Ctrl Pts',(20.7813728313873,19.7543943113433,-8.05607888502542));
#96601=CARTESIAN_POINT('Ctrl Pts',(20.761421712685,19.8246449087065,-8.05170179445809));
#96602=CARTESIAN_POINT('Ctrl Pts',(20.7379253105676,19.8936216738915,-8.04732470389076));
#96603=CARTESIAN_POINT('Ctrl Pts',(20.7144160761931,19.962636109848,-8.04294522283182));
#96604=CARTESIAN_POINT('Ctrl Pts',(20.6873578824886,20.0303748802483,-8.03856574177289));
#96605=CARTESIAN_POINT('Ctrl Pts',(20.6569274894875,20.0964596942681,-8.03418626071395));
#96606=CARTESIAN_POINT('Ctrl Pts',(20.626443158819,20.1626616431772,-8.02979901705423));
#96607=CARTESIAN_POINT('Ctrl Pts',(20.5925749169663,20.2272033538502,-8.02541177339451));
#96608=CARTESIAN_POINT('Ctrl Pts',(20.5555452556637,20.2897316077547,-8.02102452973479));
#96609=CARTESIAN_POINT('Ctrl Pts',(20.5303686541477,20.3322447952014,-8.01804162679998));
#96610=CARTESIAN_POINT('Ctrl Pts',(20.5037315602568,20.3738277943096,-8.01505872386517));
#96611=CARTESIAN_POINT('Ctrl Pts',(20.475714693788,20.4143781306983,-8.01207582093037));
#96612=CARTESIAN_POINT('Ctrl Pts',(20.434498513999,20.4740325519721,-8.00768761199947));
#96613=CARTESIAN_POINT('Ctrl Pts',(20.3901335538168,20.5316834623514,-8.00329940306858));
#96614=CARTESIAN_POINT('Ctrl Pts',(20.3428413739373,20.5869790817842,-7.99891119413768));
#96615=CARTESIAN_POINT('Ctrl Pts',(20.2956193834939,20.6421926333496,-7.99452949803642));
#96616=CARTESIAN_POINT('Ctrl Pts',(20.2454791086754,20.6950574697367,-7.99014780193516));
#96617=CARTESIAN_POINT('Ctrl Pts',(20.1926848492423,20.7452514495972,-7.9857661058339));
#96618=CARTESIAN_POINT('Ctrl Pts',(20.1399526272655,20.7953864475368,-7.98138955857427));
#96619=CARTESIAN_POINT('Ctrl Pts',(20.0845729637369,20.8428564928138,-7.97701301131463));
#96620=CARTESIAN_POINT('Ctrl Pts',(20.0268486678901,20.8873744575526,-7.972636464055));
#96621=CARTESIAN_POINT('Ctrl Pts',(19.9691609799528,20.9318641896452,-7.96826269233803));
#96622=CARTESIAN_POINT('Ctrl Pts',(19.9091319910002,20.9734052619583,-7.96388892062106));
#96623=CARTESIAN_POINT('Ctrl Pts',(19.8470983416198,21.011750144213,-7.95951514890408));
#96624=CARTESIAN_POINT('Ctrl Pts',(19.7850835692872,21.0500833579913,-7.95514270814054));
#96625=CARTESIAN_POINT('Ctrl Pts',(19.721065757685,21.0852220591673,-7.95077026737699));
#96626=CARTESIAN_POINT('Ctrl Pts',(19.6554099365361,21.116962415383,-7.94639782661344));
#96627=CARTESIAN_POINT('Ctrl Pts',(19.5897524365606,21.1487035832031,-7.94202527404609));
#96628=CARTESIAN_POINT('Ctrl Pts',(19.5224572790426,21.1770460253878,-7.93765272147875));
#96629=CARTESIAN_POINT('Ctrl Pts',(19.4539119391454,21.2018329412274,-7.9332801689114));
#96630=CARTESIAN_POINT('Ctrl Pts',(19.3852954603089,21.2266455818631,-7.92890307834408));
#96631=CARTESIAN_POINT('Ctrl Pts',(19.3154266631738,21.2478951643122,-7.92452598777675));
#96632=CARTESIAN_POINT('Ctrl Pts',(19.2447099626414,21.2654742232646,-7.92014889720943));
#96633=CARTESIAN_POINT('Ctrl Pts',(19.1739546410942,21.2830628827936,-7.91576941615049));
#96634=CARTESIAN_POINT('Ctrl Pts',(19.1023509680274,21.2969769355905,-7.91138993509155));
#96635=CARTESIAN_POINT('Ctrl Pts',(19.0303127030118,21.307160247222,-7.90701045403261));
#96636=CARTESIAN_POINT('Ctrl Pts',(18.958146750655,21.317361608705,-7.90262321037289));
#96637=CARTESIAN_POINT('Ctrl Pts',(18.8855451489733,21.3238189809293,-7.89823596671317));
#96638=CARTESIAN_POINT('Ctrl Pts',(18.8129253294104,21.3265282537412,-7.89384872305345));
#96639=CARTESIAN_POINT('Ctrl Pts',(18.7635508497363,21.3283702981885,-7.89086582011861));
#96640=CARTESIAN_POINT('Ctrl Pts',(18.7141679744274,21.328480806371,-7.88788291718377));
#96641=CARTESIAN_POINT('Ctrl Pts',(18.6649065603161,21.3268721834252,-7.88490001424893));
#96642=CARTESIAN_POINT('Ctrl Pts',(18.5924370961484,21.3245057056244,-7.88051180531802));
#96643=CARTESIAN_POINT('Ctrl Pts',(18.519947892475,21.3184071393706,-7.87612359638712));
#96644=CARTESIAN_POINT('Ctrl Pts',(18.4478546672516,21.3085723702762,-7.87173538745621));
#96645=CARTESIAN_POINT('Ctrl Pts',(18.3758684403278,21.2987521976098,-7.86735369135494));
#96646=CARTESIAN_POINT('Ctrl Pts',(18.3042774991941,21.2852068946333,-7.86297199525367));
#96647=CARTESIAN_POINT('Ctrl Pts',(18.233495774192,21.2679843266171,-7.8585902991524));
#96648=CARTESIAN_POINT('Ctrl Pts',(18.1627972233498,21.2507819964889,-7.85421375189275));
#96649=CARTESIAN_POINT('Ctrl Pts',(18.0929064660596,21.2299110986508,-7.84983720463311));
#96650=CARTESIAN_POINT('Ctrl Pts',(18.0242288363209,21.2054708308746,-7.84546065737347));
#96651=CARTESIAN_POINT('Ctrl Pts',(17.9555947609369,21.181046062761,-7.8410868856565));
#96652=CARTESIAN_POINT('Ctrl Pts',(17.8881727399585,21.1530565773997,-7.83671311393953));
#96653=CARTESIAN_POINT('Ctrl Pts',(17.8223531243431,21.1216514528048,-7.83233934222256));
#96654=CARTESIAN_POINT('Ctrl Pts',(17.7565535378578,21.0902558848948,-7.82796690145901));
#96655=CARTESIAN_POINT('Ctrl Pts',(17.6923558237623,21.055446948864,-7.82359446069545));
#96656=CARTESIAN_POINT('Ctrl Pts',(17.6301289564784,21.0174212463528,-7.8192220199319));
#96657=CARTESIAN_POINT('Ctrl Pts',(17.5679004980465,20.97939457152,-7.81484946736455));
#96658=CARTESIAN_POINT('Ctrl Pts',(17.507643397047,20.9381512201345,-7.81047691479719));
#96659=CARTESIAN_POINT('Ctrl Pts',(17.4496992310191,20.8939321242388,-7.80610436222984));
#96660=CARTESIAN_POINT('Ctrl Pts',(17.3916949283502,20.8496671360977,-7.80172727166251));
#96661=CARTESIAN_POINT('Ctrl Pts',(17.3360087376072,20.8024205306333,-7.79735018109518));
#96662=CARTESIAN_POINT('Ctrl Pts',(17.2829499222247,20.7524741878437,-7.79297309052785));
#96663=CARTESIAN_POINT('Ctrl Pts',(17.2298621294539,20.7025005675026,-7.78859360946891));
#96664=CARTESIAN_POINT('Ctrl Pts',(17.1794049028384,20.6498246228583,-7.78421412840997));
#96665=CARTESIAN_POINT('Ctrl Pts',(17.1318494027612,20.5947638757271,-7.77983464735103));
#96666=CARTESIAN_POINT('Ctrl Pts',(17.0842096108792,20.5396055337911,-7.7754474036913));
#96667=CARTESIAN_POINT('Ctrl Pts',(17.0394821127479,20.4820543293405,-7.77106016003157));
#96668=CARTESIAN_POINT('Ctrl Pts',(16.9978963120791,20.4224590314111,-7.76667291637185));
#96669=CARTESIAN_POINT('Ctrl Pts',(16.9696219748229,20.3819399714089,-7.76369001343706));
#96670=CARTESIAN_POINT('Ctrl Pts',(16.9427990411458,20.3404766042676,-7.76070711050228));
#96671=CARTESIAN_POINT('Ctrl Pts',(16.9174873693318,20.2981848336979,-7.75772420756749));
#96672=CARTESIAN_POINT('Ctrl Pts',(16.8789674908494,20.2338242543132,-7.75318475796429));
#96673=CARTESIAN_POINT('Ctrl Pts',(16.8438078846742,20.1673074236144,-7.74864530836108));
#96674=CARTESIAN_POINT('Ctrl Pts',(16.812247200043,20.0990062926902,-7.74410585875788));
#96675=CARTESIAN_POINT('Ctrl Pts',(16.7803526868132,20.0299827163854,-7.73951839377993));
#96676=CARTESIAN_POINT('Ctrl Pts',(16.7521339850624,19.9591372097164,-7.73493092880198));
#96677=CARTESIAN_POINT('Ctrl Pts',(16.7277918950442,19.8868831552936,-7.73034346382403));
#96678=CARTESIAN_POINT('Ctrl Pts',(16.7037989805435,19.8156655503633,-7.72582180381421));
#96679=CARTESIAN_POINT('Ctrl Pts',(16.6835723608136,19.7430799630089,-7.72130014380438));
#96680=CARTESIAN_POINT('Ctrl Pts',(16.667257251386,19.6695448844459,-7.71677848379455));
#96681=CARTESIAN_POINT('Ctrl Pts',(16.6505859845118,19.5944045413927,-7.71215811633255));
#96682=CARTESIAN_POINT('Ctrl Pts',(16.6379992287985,19.5182731789951,-7.70753774887054));
#96683=CARTESIAN_POINT('Ctrl Pts',(16.6295984951253,19.441615060829,-7.70291738140853));
#96684=CARTESIAN_POINT('Ctrl Pts',(16.6211977614521,19.3649569426629,-7.69829701394652));
#96685=CARTESIAN_POINT('Ctrl Pts',(16.6169831628437,19.2877725479369,-7.69367664648452));
#96686=CARTESIAN_POINT('Ctrl Pts',(16.617000050606,19.2105371115439,-7.68905627902251));
#96687=CARTESIAN_POINT('Ctrl Pts',(16.6203930058439,19.2105314190313,-7.68905589348729));
#96688=CARTESIAN_POINT('Ctrl Pts',(16.6199117136336,18.9629932582392,-7.67422393560445));
#96689=CARTESIAN_POINT('Ctrl Pts',(16.6606020170419,18.7156058265681,-7.65939197772161));
#96690=CARTESIAN_POINT('Ctrl Pts',(16.743090251011,18.4840590306076,-7.64456001983877));
#96691=CARTESIAN_POINT('Origin',(18.734,19.211,0.));
#96692=CARTESIAN_POINT('',(16.7454194487812,18.4848895460645,-6.84500598950246));
#96693=CARTESIAN_POINT('',(16.7454194586292,18.4848895190942,-7.06814843723424));
#96694=CARTESIAN_POINT('',(16.7454194503191,18.4848895418526,0.));
#96695=CARTESIAN_POINT('',(16.6170002518879,19.2120327115197,-7.10922273934007));
#96696=CARTESIAN_POINT('Ctrl Pts',(16.7454194586292,18.4848895190942,-7.06814843723424));
#96697=CARTESIAN_POINT('Ctrl Pts',(16.720259549706,18.553794329895,-7.07236993224033));
#96698=CARTESIAN_POINT('Ctrl Pts',(16.6986924511745,18.6239752665951,-7.07647898186573));
#96699=CARTESIAN_POINT('Ctrl Pts',(16.6383405809316,18.864188984939,-7.09013449006123));
#96700=CARTESIAN_POINT('Ctrl Pts',(16.6169152552473,19.0377944433565,-7.0992858278884));
#96701=CARTESIAN_POINT('Ctrl Pts',(16.6170002518879,19.2120327115197,-7.10922273934007));
#96702=CARTESIAN_POINT('Ctrl Pts',(16.6170002532712,19.2120355434925,-7.10922290084922));
#96703=CARTESIAN_POINT('Ctrl Pts',(16.6170133612054,19.2388325765887,-7.11075115282299));
#96704=CARTESIAN_POINT('Ctrl Pts',(16.6175352640855,19.2656259751736,-7.11229810151296));
#96705=CARTESIAN_POINT('Ctrl Pts',(16.619122764669,19.3068815384912,-7.11471891962847));
#96706=CARTESIAN_POINT('Ctrl Pts',(16.6198286091479,19.3213553104517,-7.11557560729638));
#96707=CARTESIAN_POINT('Ctrl Pts',(16.6209600187579,19.3405110738338,-7.11672054129347));
#96708=CARTESIAN_POINT('Ctrl Pts',(16.6212526901485,19.3452009103681,-7.11700173529727));
#96709=CARTESIAN_POINT('Ctrl Pts',(16.6217938177709,19.3534311768807,-7.11749681939946));
#96710=CARTESIAN_POINT('Ctrl Pts',(16.6220355692633,19.3569720496406,-7.11771034150998));
#96711=CARTESIAN_POINT('Ctrl Pts',(16.6225281743165,19.3639296116612,-7.11813095670815));
#96712=CARTESIAN_POINT('Ctrl Pts',(16.6227784202938,19.367346340043,-7.11833801621373));
#96713=CARTESIAN_POINT('Ctrl Pts',(16.6233330675212,19.3746749694206,-7.11878324617352));
#96714=CARTESIAN_POINT('Ctrl Pts',(16.6236400496941,19.3785866195106,-7.11902155756046));
#96715=CARTESIAN_POINT('Ctrl Pts',(16.6244765277737,19.3888783464362,-7.11965028919192));
#96716=CARTESIAN_POINT('Ctrl Pts',(16.6250240887253,19.3952568566875,-7.12004170273131));
#96717=CARTESIAN_POINT('Ctrl Pts',(16.6274167975964,19.4217202404669,-7.12167257857668));
#96718=CARTESIAN_POINT('Ctrl Pts',(16.6295199353153,19.441779975436,-7.12292547305272));
#96719=CARTESIAN_POINT('Ctrl Pts',(16.6324142650628,19.4660383676236,-7.12445835148569));
#96720=CARTESIAN_POINT('Ctrl Pts',(16.632932050339,19.470269436252,-7.12472636680322));
#96721=CARTESIAN_POINT('Ctrl Pts',(16.6366907788312,19.5002329405034,-7.12662890698868));
#96722=CARTESIAN_POINT('Ctrl Pts',(16.6403914564329,19.525904456337,-7.12828250345181));
#96723=CARTESIAN_POINT('Ctrl Pts',(16.6730372178307,19.7262310244932,-7.14133933788202));
#96724=CARTESIAN_POINT('Ctrl Pts',(16.7233160802222,19.8967032727669,-7.15328953573802));
#96725=CARTESIAN_POINT('Ctrl Pts',(16.8178243006676,20.1129025733623,-7.16850117879059));
#96726=CARTESIAN_POINT('Ctrl Pts',(16.8436568825246,20.1658620055677,-7.17224015923375));
#96727=CARTESIAN_POINT('Ctrl Pts',(16.8887823512088,20.2493430978163,-7.1781470852501));
#96728=CARTESIAN_POINT('Ctrl Pts',(16.9067037348598,20.2805668138392,-7.18035976692358));
#96729=CARTESIAN_POINT('Ctrl Pts',(16.9311299514349,20.3207159778056,-7.18321120806942));
#96730=CARTESIAN_POINT('Ctrl Pts',(16.9369196023259,20.3300674755601,-7.18387582991034));
#96731=CARTESIAN_POINT('Ctrl Pts',(16.9464809059165,20.3452454095263,-7.18495543093504));
#96732=CARTESIAN_POINT('Ctrl Pts',(16.9502087417741,20.3510990788551,-7.18537201838789));
#96733=CARTESIAN_POINT('Ctrl Pts',(16.9574518113397,20.3623500853074,-7.18617318186877));
#96734=CARTESIAN_POINT('Ctrl Pts',(16.9609630201946,20.3677499104074,-7.18655790159666));
#96735=CARTESIAN_POINT('Ctrl Pts',(16.9690857741152,20.3801178700886,-7.1874396026037));
#96736=CARTESIAN_POINT('Ctrl Pts',(16.9737140585374,20.3870749237335,-7.18793595018522));
#96737=CARTESIAN_POINT('Ctrl Pts',(16.9861789676203,20.4055732481931,-7.18925686416091));
#96738=CARTESIAN_POINT('Ctrl Pts',(16.9940887662805,20.4170648901248,-7.19007866420648));
#96739=CARTESIAN_POINT('Ctrl Pts',(17.0590934138735,20.5095354016538,-7.196703466659));
#96740=CARTESIAN_POINT('Ctrl Pts',(17.1216989541706,20.5864981666697,-7.20228401728065));
#96741=CARTESIAN_POINT('Ctrl Pts',(17.2825129833919,20.7580561297849,-7.21524692116285));
#96742=CARTESIAN_POINT('Ctrl Pts',(17.3848991732431,20.8481077382555,-7.2224861209784));
#96743=CARTESIAN_POINT('Ctrl Pts',(17.5367053128296,20.9576517992095,-7.23286053549933));
#96744=CARTESIAN_POINT('Ctrl Pts',(17.5792667629144,20.9860767655471,-7.23573770530333));
#96745=CARTESIAN_POINT('Ctrl Pts',(17.6381061458833,21.0223609477645,-7.23973190087502));
#96746=CARTESIAN_POINT('Ctrl Pts',(17.6535182966053,21.0315963494275,-7.24077963095591));
#96747=CARTESIAN_POINT('Ctrl Pts',(17.6765035697603,21.0449751267277,-7.24234724049342));
#96748=CARTESIAN_POINT('Ctrl Pts',(17.6839878773896,21.0492703833593,-7.24285845665203));
#96749=CARTESIAN_POINT('Ctrl Pts',(17.6975880446207,21.0569653894606,-7.24378921449107));
#96750=CARTESIAN_POINT('Ctrl Pts',(17.7036949403113,21.0603808264406,-7.24420780397234));
#96751=CARTESIAN_POINT('Ctrl Pts',(17.7133464704446,21.0657160488772,-7.24487055778848));
#96752=CARTESIAN_POINT('Ctrl Pts',(17.7168799117131,21.0676561272182,-7.24511344546357));
#96753=CARTESIAN_POINT('Ctrl Pts',(17.7204279624832,21.0695910590746,-7.24535761187313));
#96754=CARTESIAN_POINT('Ctrl Pts',(17.7204370861311,21.0695960345749,-7.24535823973754));
#96755=CARTESIAN_POINT('Ctrl Pts',(17.7204553884822,21.0696060154246,-7.24535949925876));
#96756=CARTESIAN_POINT('Ctrl Pts',(17.7204645681256,21.0696110212857,-7.2453601309803));
#96757=CARTESIAN_POINT('Ctrl Pts',(17.7204829830544,21.0696210631736,-7.24536139825621));
#96758=CARTESIAN_POINT('Ctrl Pts',(17.7204922183432,21.0696260992012,-7.24536203381084));
#96759=CARTESIAN_POINT('Ctrl Pts',(17.7205107451867,21.0696362017592,-7.24536330879594));
#96760=CARTESIAN_POINT('Ctrl Pts',(17.7205200368771,21.0696412683626,-7.24536394823579));
#96761=CARTESIAN_POINT('Ctrl Pts',(17.7205386774589,21.0696514325787,-7.24536523105573));
#96762=CARTESIAN_POINT('Ctrl Pts',(17.720548025621,21.0696565297926,-7.24536587438567));
#96763=CARTESIAN_POINT('Ctrl Pts',(17.7205667794415,21.0696667553876,-7.24536716500621));
#96764=CARTESIAN_POINT('Ctrl Pts',(17.7205761849688,21.0696718836961,-7.24536781228781));
#96765=CARTESIAN_POINT('Ctrl Pts',(17.7205950533626,21.0696821713911,-7.24536911080094));
#96766=CARTESIAN_POINT('Ctrl Pts',(17.7206045166479,21.0696873310048,-7.24536976206131));
#96767=CARTESIAN_POINT('Ctrl Pts',(17.7206235007403,21.0696976814065,-7.2453710685446));
#96768=CARTESIAN_POINT('Ctrl Pts',(17.7206330220353,21.0697028724593,-7.24537172380113));
#96769=CARTESIAN_POINT('Ctrl Pts',(17.7206521232753,21.0697132863507,-7.24537303835446));
#96770=CARTESIAN_POINT('Ctrl Pts',(17.7206617026036,21.069718508852,-7.24537369760885));
#96771=CARTESIAN_POINT('Ctrl Pts',(17.720680920904,21.0697289861786,-7.24537502022636));
#96772=CARTESIAN_POINT('Ctrl Pts',(17.7206905589489,21.0697342404973,-7.2453756835257));
#96773=CARTESIAN_POINT('Ctrl Pts',(17.7207098940811,21.0697447811275,-7.24537701419181));
#96774=CARTESIAN_POINT('Ctrl Pts',(17.7207195919305,21.0697500678533,-7.24537768161106));
#96775=CARTESIAN_POINT('Ctrl Pts',(17.7207390087232,21.0697606526068,-7.24537901790538));
#96776=CARTESIAN_POINT('Ctrl Pts',(17.7207487852062,21.069765982001,-7.24537969074065));
#96777=CARTESIAN_POINT('Ctrl Pts',(17.7207683803763,21.0697766635939,-7.24538103931955));
#96778=CARTESIAN_POINT('Ctrl Pts',(17.7207781970177,21.0697820146773,-7.2453817149226));
#96779=CARTESIAN_POINT('Ctrl Pts',(17.7207978923608,21.069792750471,-7.24538307040406));
#96780=CARTESIAN_POINT('Ctrl Pts',(17.7208077698294,21.0697981345078,-7.24538375019762));
#96781=CARTESIAN_POINT('Ctrl Pts',(17.7208275871355,21.0698089363729,-7.24538511408145));
#96782=CARTESIAN_POINT('Ctrl Pts',(17.7208375254755,21.0698143533836,-7.24538579806865));
#96783=CARTESIAN_POINT('Ctrl Pts',(17.7208574977835,21.0698252393204,-7.24538717262884));
#96784=CARTESIAN_POINT('Ctrl Pts',(17.7208674811768,21.0698306806786,-7.24538785972093));
#96785=CARTESIAN_POINT('Ctrl Pts',(17.7238790919266,21.0714721006418,-7.2455951300355));
#96786=CARTESIAN_POINT('Ctrl Pts',(17.7268846133439,21.0731007715878,-7.24580218197887));
#96787=CARTESIAN_POINT('Ctrl Pts',(17.7339322768655,21.0768977972676,-7.24628815832281));
#96788=CARTESIAN_POINT('Ctrl Pts',(17.7379775178711,21.0790602920898,-7.24656745015073));
#96789=CARTESIAN_POINT('Ctrl Pts',(17.7504472573001,21.0856743160113,-7.24742938504249));
#96790=CARTESIAN_POINT('Ctrl Pts',(17.7588946710058,21.0900820573763,-7.24801468537723));
#96791=CARTESIAN_POINT('Ctrl Pts',(17.8729484600565,21.1486175538417,-7.25593299112372));
#96792=CARTESIAN_POINT('Ctrl Pts',(17.9828828037535,21.193823226574,-7.26373568158187));
#96793=CARTESIAN_POINT('Ctrl Pts',(18.2002237608063,21.2625159034343,-7.2787929182716));
#96794=CARTESIAN_POINT('Ctrl Pts',(18.3068407073153,21.2873364328448,-7.28601942828048));
#96795=CARTESIAN_POINT('Ctrl Pts',(18.4895868515106,21.3152002007156,-7.29790063593097));
#96796=CARTESIAN_POINT('Ctrl Pts',(18.5648324033085,21.3225825308915,-7.30265488511632));
#96797=CARTESIAN_POINT('Ctrl Pts',(18.6591777524235,21.3267615574797,-7.30844061745585));
#96798=CARTESIAN_POINT('Ctrl Pts',(18.6780469354016,21.3273446381995,-7.30958922427399));
#96799=CARTESIAN_POINT('Ctrl Pts',(18.7054876263538,21.3278253208458,-7.31124762150342));
#96800=CARTESIAN_POINT('Ctrl Pts',(18.7140542951703,21.327923372882,-7.31176366012941));
#96801=CARTESIAN_POINT('Ctrl Pts',(18.729072507239,21.3280040948256,-7.31266542426654));
#96802=CARTESIAN_POINT('Ctrl Pts',(18.7355237710752,21.3280092813316,-7.31305184993446));
#96803=CARTESIAN_POINT('Ctrl Pts',(18.748048802387,21.3279620975784,-7.31380030337932));
#96804=CARTESIAN_POINT('Ctrl Pts',(18.7541225124443,21.3279130773624,-7.31416243224764));
#96805=CARTESIAN_POINT('Ctrl Pts',(18.7686385535778,21.3277334406176,-7.31502600444102));
#96806=CARTESIAN_POINT('Ctrl Pts',(18.7770805211379,21.3275784558716,-7.31552668150358));
#96807=CARTESIAN_POINT('Ctrl Pts',(18.8075218680721,21.3268373853055,-7.31732671733205));
#96808=CARTESIAN_POINT('Ctrl Pts',(18.829513194303,21.325958767784,-7.31861693378437));
#96809=CARTESIAN_POINT('Ctrl Pts',(19.0377788224135,21.3143827802219,-7.33074962236542));
#96810=CARTESIAN_POINT('Ctrl Pts',(19.2218783332728,21.2794490197337,-7.34072459828343));
#96811=CARTESIAN_POINT('Ctrl Pts',(19.4744933246417,21.1958620347866,-7.3552331381672));
#96812=CARTESIAN_POINT('Ctrl Pts',(19.5484874192376,21.1666625306593,-7.35960649227267));
#96813=CARTESIAN_POINT('Ctrl Pts',(19.6532159466919,21.1183585244683,-7.36620478456722));
#96814=CARTESIAN_POINT('Ctrl Pts',(19.6853846945999,21.1025182569949,-7.36829054926929));
#96815=CARTESIAN_POINT('Ctrl Pts',(19.7237363476259,21.0824076379036,-7.37086770932076));
#96816=CARTESIAN_POINT('Ctrl Pts',(19.730320715458,21.0789104938978,-7.37131345092288));
#96817=CARTESIAN_POINT('Ctrl Pts',(19.7405472972989,21.0734094122539,-7.37201110339174));
#96818=CARTESIAN_POINT('Ctrl Pts',(19.7442023882848,21.0714293629624,-7.37226152169424));
#96819=CARTESIAN_POINT('Ctrl Pts',(19.7509821795613,21.0677307192622,-7.37272805501671));
#96820=CARTESIAN_POINT('Ctrl Pts',(19.7541083777658,21.0660149903441,-7.37294398730038));
#96821=CARTESIAN_POINT('Ctrl Pts',(19.7611816898355,21.0621097076624,-7.3734343888156));
#96822=CARTESIAN_POINT('Ctrl Pts',(19.7651261254746,21.0599154351204,-7.37370915667037));
#96823=CARTESIAN_POINT('Ctrl Pts',(19.7752974442387,21.0542145028935,-7.37442097812567));
#96824=CARTESIAN_POINT('Ctrl Pts',(19.7815135839026,21.0506889300288,-7.37485920308778));
#96825=CARTESIAN_POINT('Ctrl Pts',(19.819683820957,21.0287839562399,-7.37756931814198));
#96826=CARTESIAN_POINT('Ctrl Pts',(19.8511691369719,21.0096051848397,-7.37988789408028));
#96827=CARTESIAN_POINT('Ctrl Pts',(20.0254135707649,20.8971265814173,-7.39312559558253));
#96828=CARTESIAN_POINT('Ctrl Pts',(20.1569903203571,20.7876653327158,-7.40463270078883));
#96829=CARTESIAN_POINT('Ctrl Pts',(20.3393210104831,20.594362805871,-7.42189956824913));
#96830=CARTESIAN_POINT('Ctrl Pts',(20.3998925301422,20.5207917785657,-7.4279462252364));
#96831=CARTESIAN_POINT('Ctrl Pts',(20.4677517420899,20.426010473709,-7.43510637373632));
#96832=CARTESIAN_POINT('Ctrl Pts',(20.4799269402268,20.4084492583596,-7.43640876104));
#96833=CARTESIAN_POINT('Ctrl Pts',(20.4968529829134,20.3832284174491,-7.43824568559007));
#96834=CARTESIAN_POINT('Ctrl Pts',(20.5018237175899,20.3757185966945,-7.43878850992832));
#96835=CARTESIAN_POINT('Ctrl Pts',(20.5103134076187,20.3627127512104,-7.43972155808636));
#96836=CARTESIAN_POINT('Ctrl Pts',(20.5138551202073,20.35723179852,-7.44011263138249));
#96837=CARTESIAN_POINT('Ctrl Pts',(20.5205859737462,20.3467090940383,-7.44085940422798));
#96838=CARTESIAN_POINT('Ctrl Pts',(20.5237792519135,20.3416700749597,-7.44121525529247));
#96839=CARTESIAN_POINT('Ctrl Pts',(20.5320232807208,20.328538491335,-7.44213808373598));
#96840=CARTESIAN_POINT('Ctrl Pts',(20.5370407453188,20.320425109179,-7.44270382777409));
#96841=CARTESIAN_POINT('Ctrl Pts',(20.5539416676872,20.29267832489,-7.44462383532946));
#96842=CARTESIAN_POINT('Ctrl Pts',(20.5655609045994,20.27288529779,-7.44596844912395));
#96843=CARTESIAN_POINT('Ctrl Pts',(20.6634974616737,20.0996615221443,-7.45753208502275));
#96844=CARTESIAN_POINT('Ctrl Pts',(20.7306862124172,19.9362107264801,-7.46699461391883));
#96845=CARTESIAN_POINT('Ctrl Pts',(20.7995881303978,19.6827372782856,-7.4812880978165));
#96846=CARTESIAN_POINT('Ctrl Pts',(20.8171549941907,19.5978504647584,-7.48603083331034));
#96847=CARTESIAN_POINT('Ctrl Pts',(20.8348390110948,19.4747944306692,-7.49312956016931));
#96848=CARTESIAN_POINT('Ctrl Pts',(20.8392056194943,19.4373204709446,-7.49532097023031));
#96849=CARTESIAN_POINT('Ctrl Pts',(20.8432431692171,19.3922167140733,-7.49801528684611));
#96850=CARTESIAN_POINT('Ctrl Pts',(20.8438773414933,19.3846774144376,-7.49846755170978));
#96851=CARTESIAN_POINT('Ctrl Pts',(20.8447991883511,19.3729668715092,-7.4991732078071));
#96852=CARTESIAN_POINT('Ctrl Pts',(20.8451149494973,19.3687978147029,-7.49942505052457));
#96853=CARTESIAN_POINT('Ctrl Pts',(20.8456769821951,19.3610733960172,-7.49989286271574));
#96854=CARTESIAN_POINT('Ctrl Pts',(20.8459266269316,19.357518337416,-7.50010864075819));
#96855=CARTESIAN_POINT('Ctrl Pts',(20.8464699483691,19.3494911662168,-7.50059692363118));
#96856=CARTESIAN_POINT('Ctrl Pts',(20.8467583996017,19.3450187671209,-7.50086971606983));
#96857=CARTESIAN_POINT('Ctrl Pts',(20.8475658337507,19.3318486124493,-7.50167514161818));
#96858=CARTESIAN_POINT('Ctrl Pts',(20.848045315119,19.3231486529459,-7.50220990744066));
#96859=CARTESIAN_POINT('Ctrl Pts',(20.8510723984326,19.261274143636,-7.50603130835539));
#96860=CARTESIAN_POINT('Ctrl Pts',(20.851666915218,19.208027556936,-7.50941461509519));
#96861=CARTESIAN_POINT('Ctrl Pts',(20.8497710029055,19.136609620182,-7.51403157684536));
#96862=CARTESIAN_POINT('Ctrl Pts',(20.8490525361865,19.1184062218512,-7.51521531632575));
#96863=CARTESIAN_POINT('Ctrl Pts',(20.8455854336163,19.0522439970115,-7.51953830220375));
#96864=CARTESIAN_POINT('Ctrl Pts',(20.8414396610375,19.0043738706043,-7.52270509319466));
#96865=CARTESIAN_POINT('Ctrl Pts',(20.8225299999094,18.8481021103046,-7.53310328181739));
#96866=CARTESIAN_POINT('Ctrl Pts',(20.8009940056968,18.740689798978,-7.54033569773389));
#96867=CARTESIAN_POINT('Ctrl Pts',(20.7562719040651,18.5823977293319,-7.5509085411294));
#96868=CARTESIAN_POINT('Ctrl Pts',(20.7392273814701,18.5299798548734,-7.5543973484465));
#96869=CARTESIAN_POINT('Ctrl Pts',(20.7082838776819,18.4461021504203,-7.55995445463637));
#96870=CARTESIAN_POINT('Ctrl Pts',(20.6956311008092,18.4142132088306,-7.56206118425963));
#96871=CARTESIAN_POINT('Ctrl Pts',(20.6779792588378,18.3726978719752,-7.56479756475719));
#96872=CARTESIAN_POINT('Ctrl Pts',(20.6736739859594,18.3627838414531,-7.56545055379049));
#96873=CARTESIAN_POINT('Ctrl Pts',(20.6664969221183,18.3465971843096,-7.56651603476649));
#96874=CARTESIAN_POINT('Ctrl Pts',(20.6636701020753,18.3403049439217,-7.5669300560485));
#96875=CARTESIAN_POINT('Ctrl Pts',(20.6581378197626,18.3281498766367,-7.56772956918661));
#96876=CARTESIAN_POINT('Ctrl Pts',(20.6554361936147,18.3222853972975,-7.56811518736254));
#96877=CARTESIAN_POINT('Ctrl Pts',(20.649135079636,18.3087704782615,-7.56900361702094));
#96878=CARTESIAN_POINT('Ctrl Pts',(20.6455164912051,18.3011290255409,-7.56950576239384));
#96879=CARTESIAN_POINT('Ctrl Pts',(20.6356589069633,18.2806309267153,-7.57085240739178));
#96880=CARTESIAN_POINT('Ctrl Pts',(20.6293352837622,18.2678152948676,-7.5716939653678));
#96881=CARTESIAN_POINT('Ctrl Pts',(20.5701090635873,18.1507871592397,-7.57937783534059));
#96882=CARTESIAN_POINT('Ctrl Pts',(20.5087886474078,18.0510524646779,-7.58590326270512));
#96883=CARTESIAN_POINT('Ctrl Pts',(20.3430433535936,17.8256474079191,-7.60121970882826));
#96884=CARTESIAN_POINT('Ctrl Pts',(20.2317349114003,17.7060081278881,-7.60982722065062));
#96885=CARTESIAN_POINT('Ctrl Pts',(20.0832288320186,17.5793394470836,-7.62103684117124));
#96886=CARTESIAN_POINT('Ctrl Pts',(20.0581507781137,17.5589228043075,-7.62292306799144));
#96887=CARTESIAN_POINT('Ctrl Pts',(20.0269084398209,17.5346560594328,-7.62527854330196));
#96888=CARTESIAN_POINT('Ctrl Pts',(20.0211776913712,17.5302517058625,-7.62571083106226));
#96889=CARTESIAN_POINT('Ctrl Pts',(20.0121553637404,17.5233908229729,-7.62639196177655));
#96890=CARTESIAN_POINT('Ctrl Pts',(20.0088789361461,17.5209143318292,-7.62663942471207));
#96891=CARTESIAN_POINT('Ctrl Pts',(20.0027392654977,17.5163016676524,-7.62710339668077));
#96892=CARTESIAN_POINT('Ctrl Pts',(19.9998778149962,17.5141632022144,-7.62731974131291));
#96893=CARTESIAN_POINT('Ctrl Pts',(19.9933309874139,17.5092962976818,-7.62781495791823));
#96894=CARTESIAN_POINT('Ctrl Pts',(19.9896421621321,17.5065725928903,-7.62809415311311));
#96895=CARTESIAN_POINT('Ctrl Pts',(19.9782674078456,17.4982308227799,-7.62895549994657));
#96896=CARTESIAN_POINT('Ctrl Pts',(19.9705525307129,17.492652692943,-7.6295403037076));
#96897=CARTESIAN_POINT('Ctrl Pts',(19.8652496884133,17.4175913779459,-7.63752762654764));
#96898=CARTESIAN_POINT('Ctrl Pts',(19.7619835706889,17.3564694739561,-7.64540854906931));
#96899=CARTESIAN_POINT('Ctrl Pts',(19.5560347535918,17.2570785883419,-7.66051581876532));
#96900=CARTESIAN_POINT('Ctrl Pts',(19.4544369281335,17.2173791409806,-7.66771430848045));
#96901=CARTESIAN_POINT('Ctrl Pts',(19.2785324977121,17.1638581666769,-7.67952731461302));
#96902=CARTESIAN_POINT('Ctrl Pts',(19.2057218935698,17.1458641883269,-7.68424212820552));
#96903=CARTESIAN_POINT('Ctrl Pts',(19.1136428664124,17.1282341578661,-7.68998531474084));
#96904=CARTESIAN_POINT('Ctrl Pts',(19.0951362961006,17.124945621375,-7.69112888288112));
#96905=CARTESIAN_POINT('Ctrl Pts',(19.0681485823209,17.120519944509,-7.69278138706911));
#96906=CARTESIAN_POINT('Ctrl Pts',(19.0597008573032,17.1191871277819,-7.69329650913612));
#96907=CARTESIAN_POINT('Ctrl Pts',(19.0448691569094,17.1169391233765,-7.69419721569517));
#96908=CARTESIAN_POINT('Ctrl Pts',(19.0384886876958,17.116001854842,-7.69458349531606));
#96909=CARTESIAN_POINT('Ctrl Pts',(19.0260863014067,17.1142378443043,-7.69533206077629));
#96910=CARTESIAN_POINT('Ctrl Pts',(19.0200649169497,17.1134078543475,-7.69569444584988));
#96911=CARTESIAN_POINT('Ctrl Pts',(19.0056543965734,17.1114847084589,-7.69655925733277));
#96912=CARTESIAN_POINT('Ctrl Pts',(18.9972620770168,17.1104158782485,-7.69706091240715));
#96913=CARTESIAN_POINT('Ctrl Pts',(18.9669110287855,17.1067351758464,-7.69886816321529));
#96914=CARTESIAN_POINT('Ctrl Pts',(18.9449176328586,17.1044170313075,-7.7001645191002));
#96915=CARTESIAN_POINT('Ctrl Pts',(18.7380956070199,17.0858892411994,-7.71224140454963));
#96916=CARTESIAN_POINT('Ctrl Pts',(18.5519309717436,17.0936976127733,-7.72216589755605));
#96917=CARTESIAN_POINT('Ctrl Pts',(18.2613168852555,17.1445429407069,-7.73824897429961));
#96918=CARTESIAN_POINT('Ctrl Pts',(18.1551181761788,17.1717443709271,-7.7442837374116));
#96919=CARTESIAN_POINT('Ctrl Pts',(18.0403470630171,17.2108315624758,-7.75143990705116));
#96920=CARTESIAN_POINT('Ctrl Pts',(18.0292119362402,17.2147279878865,-7.75214107073281));
#96921=CARTESIAN_POINT('Ctrl Pts',(18.0134014140985,17.2204092047715,-7.75314722591709));
#96922=CARTESIAN_POINT('Ctrl Pts',(18.0086986522564,17.2221179044894,-7.75344784341923));
#96923=CARTESIAN_POINT('Ctrl Pts',(18.000594465435,17.2250950424322,-7.75396828200413));
#96924=CARTESIAN_POINT('Ctrl Pts',(17.9971901293249,17.2263556003775,-7.75418763399487));
#96925=CARTESIAN_POINT('Ctrl Pts',(17.9905875590405,17.2288197307567,-7.75461450451461));
#96926=CARTESIAN_POINT('Ctrl Pts',(17.9873889907919,17.2300222924787,-7.75482195672569));
#96927=CARTESIAN_POINT('Ctrl Pts',(17.9787494943091,17.233294369617,-7.75538404826525));
#96928=CARTESIAN_POINT('Ctrl Pts',(17.9733142149168,17.235378573378,-7.75573955416039));
#96929=CARTESIAN_POINT('Ctrl Pts',(17.9530711626596,17.243236863244,-7.75707044175574));
#96930=CARTESIAN_POINT('Ctrl Pts',(17.938320393228,17.2491550672372,-7.7580539427589));
#96931=CARTESIAN_POINT('Ctrl Pts',(17.8094457286009,17.3025537630838,-7.76675864107124));
#96932=CARTESIAN_POINT('Ctrl Pts',(17.6996273306895,17.3597747062125,-7.77493784328568));
#96933=CARTESIAN_POINT('Ctrl Pts',(17.4545089122284,17.5161443843451,-7.79415109477477));
#96934=CARTESIAN_POINT('Ctrl Pts',(17.324696423208,17.6224417721401,-7.80506921525835));
#96935=CARTESIAN_POINT('Ctrl Pts',(17.1939623569774,17.7582692823488,-7.81664814540657));
#96936=CARTESIAN_POINT('Ctrl Pts',(17.1794268297673,17.7738344596634,-7.81794607724562));
#96937=CARTESIAN_POINT('Ctrl Pts',(17.1590898627573,17.7962816739177,-7.81977786442136));
#96938=CARTESIAN_POINT('Ctrl Pts',(17.1530939813725,17.8029850687184,-7.82031994395172));
#96939=CARTESIAN_POINT('Ctrl Pts',(17.1428230046997,17.814616340643,-7.82125211385718));
#96940=CARTESIAN_POINT('Ctrl Pts',(17.1385276706298,17.8195261043826,-7.82164304948772));
#96941=CARTESIAN_POINT('Ctrl Pts',(17.1303462138068,17.8289655748825,-7.82238983293753));
#96942=CARTESIAN_POINT('Ctrl Pts',(17.1264564239609,17.8334920071229,-7.82274583095637));
#96943=CARTESIAN_POINT('Ctrl Pts',(17.1163900847981,17.8453066129552,-7.82366963190904));
#96944=CARTESIAN_POINT('Ctrl Pts',(17.1102435908696,17.8526203058302,-7.82423619624352));
#96945=CARTESIAN_POINT('Ctrl Pts',(17.0894465542836,17.8777095004407,-7.82616202302315));
#96946=CARTESIAN_POINT('Ctrl Pts',(17.0750363886521,17.8956827798896,-7.82751155488038));
#96947=CARTESIAN_POINT('Ctrl Pts',(16.9537660001987,18.0521032357074,-7.83901211222878));
#96948=CARTESIAN_POINT('Ctrl Pts',(16.8641494981791,18.203061196504,-7.848418175652));
#96949=CARTESIAN_POINT('Ctrl Pts',(16.7766288646635,18.403352548604,-7.86031011670247));
#96950=CARTESIAN_POINT('Ctrl Pts',(16.7603898995266,18.4438903486588,-7.86269366584045));
#96951=CARTESIAN_POINT('Ctrl Pts',(16.7454194594376,18.48488951688,-7.86510585860832));
#96952=CARTESIAN_POINT('',(16.6156461087368,19.2092594235966,-6.88905704663753));
#96953=CARTESIAN_POINT('Ctrl Pts',(16.743090251011,18.4840590306076,-7.64456001983877));
#96954=CARTESIAN_POINT('Ctrl Pts',(16.7690655518128,18.4111456296853,-7.63988948018787));
#96955=CARTESIAN_POINT('Ctrl Pts',(17.0725682250524,17.6922648295445,-7.59282700497648));
#96956=CARTESIAN_POINT('Ctrl Pts',(18.4531255372358,16.7235436104772,-7.50337259420462));
#96957=CARTESIAN_POINT('Ctrl Pts',(20.6735251555922,17.6284160608558,-7.3761967875232));
#96958=CARTESIAN_POINT('Ctrl Pts',(21.1145308242001,19.9852110491624,-7.24902098084175));
#96959=CARTESIAN_POINT('Ctrl Pts',(19.3715472140107,21.6317154528194,-7.12184517416032));
#96960=CARTESIAN_POINT('Ctrl Pts',(17.1752234436464,21.0898253692303,-7.00185719609225));
#96961=CARTESIAN_POINT('Ctrl Pts',(16.6208560614913,19.7934638448055,-6.92426115358465));
#96962=CARTESIAN_POINT('Ctrl Pts',(16.6156461087368,19.2092594235966,-6.88905704663753));
#96963=CARTESIAN_POINT('Ctrl Pts',(16.6170007608246,19.2092051933703,-6.88983560272607));
#96964=CARTESIAN_POINT('Ctrl Pts',(16.6170691234831,19.1285704923251,-6.88542652681705));
#96965=CARTESIAN_POINT('Ctrl Pts',(16.621744409621,19.0480107499138,-6.88096271700477));
#96966=CARTESIAN_POINT('Ctrl Pts',(16.6337263173979,18.944349549339,-6.8749294996215));
#96967=CARTESIAN_POINT('Ctrl Pts',(16.6368467594814,18.9208273159821,-6.87354087664655));
#96968=CARTESIAN_POINT('Ctrl Pts',(16.6412443064366,18.8914720729822,-6.87177780667558));
#96969=CARTESIAN_POINT('Ctrl Pts',(16.6421517369496,18.8855843710229,-6.87142267176195));
#96970=CARTESIAN_POINT('Ctrl Pts',(16.6437164847236,18.8757088423748,-6.87082432682732));
#96971=CARTESIAN_POINT('Ctrl Pts',(16.6443603995873,18.8717188858875,-6.87058184750745));
#96972=CARTESIAN_POINT('Ctrl Pts',(16.6455600505918,18.8644183406169,-6.87013679264496));
#96973=CARTESIAN_POINT('Ctrl Pts',(16.6461122450045,18.8611071720033,-6.86993441614739));
#96974=CARTESIAN_POINT('Ctrl Pts',(16.647268751021,18.8542725486385,-6.86951558516495));
#96975=CARTESIAN_POINT('Ctrl Pts',(16.6478741076568,18.8507493363769,-6.86929906988327));
#96976=CARTESIAN_POINT('Ctrl Pts',(16.6492807993464,18.8426847537831,-6.86880208190678));
#96977=CARTESIAN_POINT('Ctrl Pts',(16.6500880489582,18.8381444709462,-6.86852127706985));
#96978=CARTESIAN_POINT('Ctrl Pts',(16.6526310873336,18.8241077074899,-6.8676501046972));
#96979=CARTESIAN_POINT('Ctrl Pts',(16.6544169762281,18.8146205911576,-6.86705699836012));
#96980=CARTESIAN_POINT('Ctrl Pts',(16.6735179717447,18.7168347401309,-6.86090160543583));
#96981=CARTESIAN_POINT('Ctrl Pts',(16.6963792374528,18.6297226697183,-6.85506651331012));
#96982=CARTESIAN_POINT('Ctrl Pts',(16.7313173629578,18.5244202611044,-6.84777452238905));
#96983=CARTESIAN_POINT('Ctrl Pts',(16.7382219241471,18.5046012268794,-6.8463911615787));
#96984=CARTESIAN_POINT('Ctrl Pts',(16.7454194487812,18.4848895460645,-6.84500598950246));
#96985=CARTESIAN_POINT('Origin',(18.734,19.211,0.));
#96986=CARTESIAN_POINT('',(16.7454194503114,18.4848895418737,-6.04247203357104));
#96987=CARTESIAN_POINT('',(16.7454195730112,18.484889205839,-6.26710634208694));
#96988=CARTESIAN_POINT('',(16.7454194503191,18.4848895418526,0.));
#96989=CARTESIAN_POINT('Ctrl Pts',(16.7454195730112,18.484889205839,-6.26710634208694));
#96990=CARTESIAN_POINT('Ctrl Pts',(16.7157171128003,18.5662345480153,-6.27277683141834));
#96991=CARTESIAN_POINT('Ctrl Pts',(16.6910043038225,18.6494072568333,-6.27836337269697));
#96992=CARTESIAN_POINT('Ctrl Pts',(16.6614520778875,18.7771761929411,-6.28658111049015));
#96993=CARTESIAN_POINT('Ctrl Pts',(16.6528139479689,18.8207141214286,-6.28932034142043));
#96994=CARTESIAN_POINT('Ctrl Pts',(16.643614442751,18.8761611018695,-6.29273463347285));
#96995=CARTESIAN_POINT('Ctrl Pts',(16.6417764797029,18.8878442857266,-6.2934499418142));
#96996=CARTESIAN_POINT('Ctrl Pts',(16.6389885134331,18.9065880907435,-6.29459110135969));
#96997=CARTESIAN_POINT('Ctrl Pts',(16.6379760966145,18.9136390447423,-6.29501892187042));
#96998=CARTESIAN_POINT('Ctrl Pts',(16.6361227659987,18.9270264690196,-6.29582849659302));
#96999=CARTESIAN_POINT('Ctrl Pts',(16.6352749264759,18.9333618859301,-6.29621046570273));
#97000=CARTESIAN_POINT('Ctrl Pts',(16.633414069615,18.9477627967033,-6.2970761417738));
#97001=CARTESIAN_POINT('Ctrl Pts',(16.6324187831995,18.9558305109566,-6.29755928406061));
#97002=CARTESIAN_POINT('Ctrl Pts',(16.6299653952527,18.976706278146,-6.29880483450005));
#97003=CARTESIAN_POINT('Ctrl Pts',(16.6285777510808,18.9895223920608,-6.2995650214894));
#97004=CARTESIAN_POINT('Ctrl Pts',(16.6203967172453,19.0721247124333,-6.30443699776595));
#97005=CARTESIAN_POINT('Ctrl Pts',(16.6169563815465,19.142203345731,-6.30844165782057));
#97006=CARTESIAN_POINT('Ctrl Pts',(16.6171212273729,19.404716566235,-6.32314064332877));
#97007=CARTESIAN_POINT('Ctrl Pts',(16.6434647832249,19.5961655962577,-6.33317497168615));
#97008=CARTESIAN_POINT('Ctrl Pts',(16.7087052272871,19.8293426842463,-6.34683369412467));
#97009=CARTESIAN_POINT('Ctrl Pts',(16.7238020860671,19.8767853212513,-6.34969719296323));
#97010=CARTESIAN_POINT('Ctrl Pts',(16.7431845120058,19.9310025697894,-6.3531151035776));
#97011=CARTESIAN_POINT('Ctrl Pts',(16.745854488552,19.9383427175655,-6.35358097284039));
#97012=CARTESIAN_POINT('Ctrl Pts',(16.7501831752621,19.9500409657708,-6.35432872032372));
#97013=CARTESIAN_POINT('Ctrl Pts',(16.7518158006495,19.9544087315157,-6.35460908603248));
#97014=CARTESIAN_POINT('Ctrl Pts',(16.7547310332478,19.9621299809108,-6.35510686137764));
#97015=CARTESIAN_POINT('Ctrl Pts',(16.7560077573438,19.9654856385674,-6.35532391746722));
#97016=CARTESIAN_POINT('Ctrl Pts',(16.7587298594131,19.9725858335179,-6.35578473757404));
#97017=CARTESIAN_POINT('Ctrl Pts',(16.7601773291796,19.9763294543171,-6.3560286205799));
#97018=CARTESIAN_POINT('Ctrl Pts',(16.7641078966439,19.9864098411805,-6.35668773924526));
#97019=CARTESIAN_POINT('Ctrl Pts',(16.7666108960728,19.9927387232977,-6.35710414401619));
#97020=CARTESIAN_POINT('Ctrl Pts',(16.7791207440013,20.0239294846929,-6.35916870416381));
#97021=CARTESIAN_POINT('Ctrl Pts',(16.7895680738967,20.04861063857,-6.36084133192827));
#97022=CARTESIAN_POINT('Ctrl Pts',(16.8210382317118,20.1191931594763,-6.36572419259452));
#97023=CARTESIAN_POINT('Ctrl Pts',(16.8432373509301,20.1645478312475,-6.36898503169949));
#97024=CARTESIAN_POINT('Ctrl Pts',(16.9295817032383,20.3260626903425,-6.38094756479307));
#97025=CARTESIAN_POINT('Ctrl Pts',(17.0029893298191,20.4369262419257,-6.3898157700923));
#97026=CARTESIAN_POINT('Ctrl Pts',(17.1511163185503,20.6205484644966,-6.4051416947578));
#97027=CARTESIAN_POINT('Ctrl Pts',(17.2217357974137,20.6960623176748,-6.41168263632886));
#97028=CARTESIAN_POINT('Ctrl Pts',(17.307910781157,20.7756583472694,-6.41884328657374));
#97029=CARTESIAN_POINT('Ctrl Pts',(17.3183213353504,20.7850839041021,-6.41969609490092));
#97030=CARTESIAN_POINT('Ctrl Pts',(17.3350950524069,20.7999695466006,-6.42105098750275));
#97031=CARTESIAN_POINT('Ctrl Pts',(17.3413980605066,20.8054965078987,-6.42155587251278));
#97032=CARTESIAN_POINT('Ctrl Pts',(17.3526049402554,20.8152064172839,-6.4224461732826));
#97033=CARTESIAN_POINT('Ctrl Pts',(17.3574953667403,20.8194046556701,-6.42283222174498));
#97034=CARTESIAN_POINT('Ctrl Pts',(17.367682200866,20.8280691602798,-6.42363132400555));
#97035=CARTESIAN_POINT('Ctrl Pts',(17.3729815193615,20.8325318974578,-6.42404422991631));
#97036=CARTESIAN_POINT('Ctrl Pts',(17.3867089423316,20.8439775246914,-6.42510670644005));
#97037=CARTESIAN_POINT('Ctrl Pts',(17.3951695301738,20.8509212694798,-6.42575467924603));
#97038=CARTESIAN_POINT('Ctrl Pts',(17.4313068445597,20.8801136921761,-6.42849388356384));
#97039=CARTESIAN_POINT('Ctrl Pts',(17.4594881412675,20.9017305266963,-6.43055977652761));
#97040=CARTESIAN_POINT('Ctrl Pts',(17.5349317069356,20.9566416643685,-6.43592258394742));
#97041=CARTESIAN_POINT('Ctrl Pts',(17.5830376528115,20.9887277618309,-6.43917556783512));
#97042=CARTESIAN_POINT('Ctrl Pts',(17.7707936119587,21.1031382717155,-6.45137508646922));
#97043=CARTESIAN_POINT('Ctrl Pts',(17.918402403406,21.1712930695367,-6.45992612162854));
#97044=CARTESIAN_POINT('Ctrl Pts',(18.0929235931255,21.2287165275406,-6.47018706747939));
#97045=CARTESIAN_POINT('Ctrl Pts',(18.1136180628487,21.235175176664,-6.47140682939451));
#97046=CARTESIAN_POINT('Ctrl Pts',(18.1746823789171,21.2532086898565,-6.4750245016199));
#97047=CARTESIAN_POINT('Ctrl Pts',(18.2152992908394,21.2639007717696,-6.47745423736939));
#97048=CARTESIAN_POINT('Ctrl Pts',(18.2634493062217,21.2750558024442,-6.48039067042102));
#97049=CARTESIAN_POINT('Ctrl Pts',(18.2707032256743,21.2766961069424,-6.480834536319));
#97050=CARTESIAN_POINT('Ctrl Pts',(18.2824592935057,21.2792894302036,-6.48155651000256));
#97051=CARTESIAN_POINT('Ctrl Pts',(18.2869562422889,21.2802660666255,-6.48183329998524));
#97052=CARTESIAN_POINT('Ctrl Pts',(18.2949512390077,21.2819751225672,-6.48232655440146));
#97053=CARTESIAN_POINT('Ctrl Pts',(18.2984479937798,21.282713354323,-6.48254268280818));
#97054=CARTESIAN_POINT('Ctrl Pts',(18.305956854378,21.2842787671131,-6.48300765605414));
#97055=CARTESIAN_POINT('Ctrl Pts',(18.3099694368348,21.285103146307,-6.48325665137753));
#97056=CARTESIAN_POINT('Ctrl Pts',(18.3210209192156,21.2873402469347,-6.48394382674732));
#97057=CARTESIAN_POINT('Ctrl Pts',(18.3280645758112,21.2887288009247,-6.48438334857316));
#97058=CARTESIAN_POINT('Ctrl Pts',(18.3661876257942,21.2960429496807,-6.48677008586415));
#97059=CARTESIAN_POINT('Ctrl Pts',(18.3973880696127,21.3013067249018,-6.48875163643175));
#97060=CARTESIAN_POINT('Ctrl Pts',(18.5904538319102,21.3294442273624,-6.50113882603053));
#97061=CARTESIAN_POINT('Ctrl Pts',(18.7543963181856,21.3342040052771,-6.51214905143024));
#97062=CARTESIAN_POINT('Ctrl Pts',(19.033863009623,21.3099216097585,-6.53047401432928));
#97063=CARTESIAN_POINT('Ctrl Pts',(19.1494470995104,21.2901347497806,-6.53793075640742));
#97064=CARTESIAN_POINT('Ctrl Pts',(19.2766584604555,21.2573174411523,-6.54595261245501));
#97065=CARTESIAN_POINT('Ctrl Pts',(19.2904615824294,21.2536071080057,-6.54682078078264));
#97066=CARTESIAN_POINT('Ctrl Pts',(19.3123692542439,21.2474796831419,-6.5481953353323));
#97067=CARTESIAN_POINT('Ctrl Pts',(19.3204985392718,21.2451533769057,-6.54870465125274));
#97068=CARTESIAN_POINT('Ctrl Pts',(19.3348107027257,21.2409648249728,-6.54960009375852));
#97069=CARTESIAN_POINT('Ctrl Pts',(19.3409993664486,21.2391228911732,-6.54998687676749));
#97070=CARTESIAN_POINT('Ctrl Pts',(19.3537815742112,21.235254771121,-6.55078493332448));
#97071=CARTESIAN_POINT('Ctrl Pts',(19.3603738437984,21.2332246135568,-6.55119607164699));
#97072=CARTESIAN_POINT('Ctrl Pts',(19.3772687685316,21.2279311049686,-6.55224866142945));
#97073=CARTESIAN_POINT('Ctrl Pts',(19.3875566512589,21.2246209923689,-6.55288857227804));
#97074=CARTESIAN_POINT('Ctrl Pts',(19.4303800397828,21.2104798528851,-6.55554828537603));
#97075=CARTESIAN_POINT('Ctrl Pts',(19.4626763936725,21.1989375622901,-6.55754458038087));
#97076=CARTESIAN_POINT('Ctrl Pts',(19.5460742144948,21.1668265463782,-6.56268602732294));
#97077=CARTESIAN_POINT('Ctrl Pts',(19.5966794961533,21.1450389708372,-6.56579184308038));
#97078=CARTESIAN_POINT('Ctrl Pts',(19.7450263109169,21.0741869426091,-6.57493321228813));
#97079=CARTESIAN_POINT('Ctrl Pts',(19.8398773419618,21.019501030057,-6.580820026276));
#97080=CARTESIAN_POINT('Ctrl Pts',(19.9655515286581,20.9334453563047,-6.58911251296097));
#97081=CARTESIAN_POINT('Ctrl Pts',(20.0002738703543,20.9080820452341,-6.59146252736311));
#97082=CARTESIAN_POINT('Ctrl Pts',(20.0938178827419,20.8352818488065,-6.59802444682895));
#97083=CARTESIAN_POINT('Ctrl Pts',(20.1509039538893,20.7857307108622,-6.60229314793768));
#97084=CARTESIAN_POINT('Ctrl Pts',(20.2120398661685,20.7266441799308,-6.60733214094506));
#97085=CARTESIAN_POINT('Ctrl Pts',(20.2188216099872,20.7200009625788,-6.60789801861905));
#97086=CARTESIAN_POINT('Ctrl Pts',(20.2288085888273,20.710085474823,-6.60874207325033));
#97087=CARTESIAN_POINT('Ctrl Pts',(20.2320483621695,20.7068479474044,-6.60901758015181));
#97088=CARTESIAN_POINT('Ctrl Pts',(20.2377958807759,20.7010670141663,-6.6095094278243));
#97089=CARTESIAN_POINT('Ctrl Pts',(20.2403077206295,20.6985277504256,-6.60972543983958));
#97090=CARTESIAN_POINT('Ctrl Pts',(20.2456965520776,20.6930524388014,-6.61019116686551));
#97091=CARTESIAN_POINT('Ctrl Pts',(20.2485713798898,20.6901144078383,-6.61044103764561));
#97092=CARTESIAN_POINT('Ctrl Pts',(20.2564885481728,20.6819758975532,-6.61113304425547));
#97093=CARTESIAN_POINT('Ctrl Pts',(20.2615127264865,20.6767579395753,-6.61157655262607));
#97094=CARTESIAN_POINT('Ctrl Pts',(20.2889782033874,20.6479385614255,-6.6140246560007));
#97095=CARTESIAN_POINT('Ctrl Pts',(20.3108980520053,20.6238488617113,-6.61606566205947));
#97096=CARTESIAN_POINT('Ctrl Pts',(20.4389310805625,20.4764497057564,-6.6284723389654));
#97097=CARTESIAN_POINT('Ctrl Pts',(20.5310958998833,20.3417516120002,-6.63942741728655));
#97098=CARTESIAN_POINT('Ctrl Pts',(20.6613735314984,20.0944946623868,-6.6576827096116));
#97099=CARTESIAN_POINT('Ctrl Pts',(20.707181537781,19.9868182593872,-6.66512286385159));
#97100=CARTESIAN_POINT('Ctrl Pts',(20.7483642124681,19.8623294105699,-6.67312928268045));
#97101=CARTESIAN_POINT('Ctrl Pts',(20.752714704693,19.8487179143778,-6.67399725043238));
#97102=CARTESIAN_POINT('Ctrl Pts',(20.7594193994893,19.8269843620647,-6.67537154843671));
#97103=CARTESIAN_POINT('Ctrl Pts',(20.761863274943,19.81889063121,-6.67588080668667));
#97104=CARTESIAN_POINT('Ctrl Pts',(20.7660879240262,19.8045902274833,-6.67677618211034));
#97105=CARTESIAN_POINT('Ctrl Pts',(20.7678888987527,19.7983896816427,-6.67716295539817));
#97106=CARTESIAN_POINT('Ctrl Pts',(20.7715552247178,19.7855479002266,-6.67796102475101));
#97107=CARTESIAN_POINT('Ctrl Pts',(20.7734165419068,19.7789055852503,-6.67837218542874));
#97108=CARTESIAN_POINT('Ctrl Pts',(20.7781109614756,19.761832284549,-6.6794249004468));
#97109=CARTESIAN_POINT('Ctrl Pts',(20.7808967265067,19.7513884030041,-6.68006491345573));
#97110=CARTESIAN_POINT('Ctrl Pts',(20.7921897754932,19.7077099083396,-6.68272561932695));
#97111=CARTESIAN_POINT('Ctrl Pts',(20.7999688588139,19.674291221598,-6.68472278253884));
#97112=CARTESIAN_POINT('Ctrl Pts',(20.8181178131451,19.5867374798301,-6.68986697093002));
#97113=CARTESIAN_POINT('Ctrl Pts',(20.8271923872874,19.5323595930676,-6.69297460489443));
#97114=CARTESIAN_POINT('Ctrl Pts',(20.8479100000104,19.3692099757152,-6.70211914628175));
#97115=CARTESIAN_POINT('Ctrl Pts',(20.8532599550459,19.2598263349008,-6.70800732475787));
#97116=CARTESIAN_POINT('Ctrl Pts',(20.848826170494,19.1046941267489,-6.71645682681221));
#97117=CARTESIAN_POINT('Ctrl Pts',(20.8460283027936,19.0589247591212,-6.71896350962539));
#97118=CARTESIAN_POINT('Ctrl Pts',(20.8396436606771,18.9908615083874,-6.72275449525831));
#97119=CARTESIAN_POINT('Ctrl Pts',(20.83718274372,18.9684747894264,-6.72401170976417));
#97120=CARTESIAN_POINT('Ctrl Pts',(20.8337106790109,18.940941797381,-6.7255751164233));
#97121=CARTESIAN_POINT('Ctrl Pts',(20.8330369115128,18.9357539069997,-6.72587045500963));
#97122=CARTESIAN_POINT('Ctrl Pts',(20.8261932842122,18.8845460752896,-6.72879354682361));
#97123=CARTESIAN_POINT('Ctrl Pts',(20.8185306896726,18.8387420129144,-6.73147120945726));
#97124=CARTESIAN_POINT('Ctrl Pts',(20.8078579641483,18.7857226787476,-6.7346827493522));
#97125=CARTESIAN_POINT('Ctrl Pts',(20.8063058918322,18.7782229880204,-6.7351396651536));
#97126=CARTESIAN_POINT('Ctrl Pts',(20.8037527147901,18.7662146260185,-6.73587574119485));
#97127=CARTESIAN_POINT('Ctrl Pts',(20.8027774739496,18.7617004433096,-6.7361534623518));
#97128=CARTESIAN_POINT('Ctrl Pts',(20.8010190847327,18.7536883424341,-6.73664824517833));
#97129=CARTESIAN_POINT('Ctrl Pts',(20.8002418150537,18.7501891816113,-6.73686496796004));
#97130=CARTESIAN_POINT('Ctrl Pts',(20.7985697843028,18.7427512200483,-6.73732701225702));
#97131=CARTESIAN_POINT('Ctrl Pts',(20.797672650753,18.7388130623515,-6.73757246254138));
#97132=CARTESIAN_POINT('Ctrl Pts',(20.7952079244809,18.7281348237989,-6.73824015774943));
#97133=CARTESIAN_POINT('Ctrl Pts',(20.7936185610992,18.7213998916957,-6.73866362349529));
#97134=CARTESIAN_POINT('Ctrl Pts',(20.7853877115994,18.6872710681241,-6.74082096752433));
#97135=CARTESIAN_POINT('Ctrl Pts',(20.7782329354768,18.6600053871329,-6.74258198050917));
#97136=CARTESIAN_POINT('Ctrl Pts',(20.7556732807536,18.5805330752112,-6.74780920330726));
#97137=CARTESIAN_POINT('Ctrl Pts',(20.7387974357248,18.5287699578381,-6.75133417465667));
#97138=CARTESIAN_POINT('Ctrl Pts',(20.6713613069466,18.3461326208481,-6.76407932120529));
#97139=CARTESIAN_POINT('Ctrl Pts',(20.6098122617615,18.2196888925553,-6.77345467276722));
#97140=CARTESIAN_POINT('Ctrl Pts',(20.488640376356,18.0230836128615,-6.78836844067434));
#97141=CARTESIAN_POINT('Ctrl Pts',(20.4361602898219,17.9490323646912,-6.79408348275205));
#97142=CARTESIAN_POINT('Ctrl Pts',(20.3704427794626,17.867894412056,-6.80045431513944));
#97143=CARTESIAN_POINT('Ctrl Pts',(20.3616955804012,17.8573070132729,-6.80128804321739));
#97144=CARTESIAN_POINT('Ctrl Pts',(20.3475024048885,17.8404644303002,-6.80261846712928));
#97145=CARTESIAN_POINT('Ctrl Pts',(20.3421217297589,17.8341549601622,-6.80311780715638));
#97146=CARTESIAN_POINT('Ctrl Pts',(20.332502297046,17.8230083693917,-6.80400171080897));
#97147=CARTESIAN_POINT('Ctrl Pts',(20.3282783324153,17.8181586736077,-6.80438687758631));
#97148=CARTESIAN_POINT('Ctrl Pts',(20.3194315792848,17.8080943482046,-6.80518747776021));
#97149=CARTESIAN_POINT('Ctrl Pts',(20.3148050051731,17.80288313772,-6.80560274676184));
#97150=CARTESIAN_POINT('Ctrl Pts',(20.3027233509827,17.7894093794559,-6.80667839989021));
#97151=CARTESIAN_POINT('Ctrl Pts',(20.2952286401199,17.7811825344619,-6.80733710883089));
#97152=CARTESIAN_POINT('Ctrl Pts',(20.2624018629158,17.7457148782648,-6.81018592005663));
#97153=CARTESIAN_POINT('Ctrl Pts',(20.2364182363267,17.7190843072423,-6.81234803407614));
#97154=CARTESIAN_POINT('Ctrl Pts',(20.1655286855355,17.6501611737876,-6.81802236803161));
#97155=CARTESIAN_POINT('Ctrl Pts',(20.1194528596114,17.6091218999448,-6.82148366464681));
#97156=CARTESIAN_POINT('Ctrl Pts',(19.9571443547057,17.4768052867368,-6.83306940748254));
#97157=CARTESIAN_POINT('Ctrl Pts',(19.8331917225542,17.3957072764406,-6.84090300188289));
#97158=CARTESIAN_POINT('Ctrl Pts',(19.6393241600402,17.2960551869303,-6.85300994561398));
#97159=CARTESIAN_POINT('Ctrl Pts',(19.5752822611494,17.2670690594853,-6.85699439089739));
#97160=CARTESIAN_POINT('Ctrl Pts',(19.5012184820893,17.2378927087841,-6.86171342787288));
#97161=CARTESIAN_POINT('Ctrl Pts',(19.4924887560628,17.2345204575932,-6.86227136346605));
#97162=CARTESIAN_POINT('Ctrl Pts',(19.479478689503,17.2295936160018,-6.86310581070273));
#97163=CARTESIAN_POINT('Ctrl Pts',(19.4752150921646,17.2279947248406,-6.86337973981385));
#97164=CARTESIAN_POINT('Ctrl Pts',(19.4676002881612,17.2251670871743,-6.86386986829252));
#97165=CARTESIAN_POINT('Ctrl Pts',(19.464251101507,17.223933048699,-6.8640857478525));
#97166=CARTESIAN_POINT('Ctrl Pts',(19.4570211516786,17.2212898553458,-6.8645524503365));
#97167=CARTESIAN_POINT('Ctrl Pts',(19.4531394379694,17.2198836011928,-6.8648034357204));
#97168=CARTESIAN_POINT('Ctrl Pts',(19.4423586530324,17.2160136125355,-6.86550160666222));
#97169=CARTESIAN_POINT('Ctrl Pts',(19.4354509463233,17.2135743483709,-6.86595020445473));
#97170=CARTESIAN_POINT('Ctrl Pts',(19.3966033626951,17.2000827722967,-6.86847947658194));
#97171=CARTESIAN_POINT('Ctrl Pts',(19.3644169640888,17.1897614032853,-6.87059940516158));
#97172=CARTESIAN_POINT('Ctrl Pts',(19.2627751015612,17.1598312027444,-6.87734018874641));
#97173=CARTESIAN_POINT('Ctrl Pts',(19.1925582436769,17.1430011032718,-6.88206224799451));
#97174=CARTESIAN_POINT('Ctrl Pts',(19.1178327585342,17.1290835051586,-6.88707254751238));
#97175=CARTESIAN_POINT('Ctrl Pts',(19.1140388472069,17.1283876134826,-6.88732689190765));
#97176=CARTESIAN_POINT('Ctrl Pts',(18.9198653551403,17.0933199307972,-6.90034199432428));
#97177=CARTESIAN_POINT('Ctrl Pts',(18.725624994819,17.0851881656656,-6.91312367423729));
#97178=CARTESIAN_POINT('Ctrl Pts',(18.5118451743411,17.1055817086332,-6.92631837047566));
#97179=CARTESIAN_POINT('Ctrl Pts',(18.4907599493683,17.107913392808,-6.92761176153798));
#97180=CARTESIAN_POINT('Ctrl Pts',(18.461464000176,17.1115995505289,-6.92939820220442));
#97181=CARTESIAN_POINT('Ctrl Pts',(18.4532213852937,17.112686036112,-6.92989965952864));
#97182=CARTESIAN_POINT('Ctrl Pts',(18.439001869435,17.1146456444008,-6.93076277146269));
#97183=CARTESIAN_POINT('Ctrl Pts',(18.4330219560837,17.1154958364316,-6.93112514639025));
#97184=CARTESIAN_POINT('Ctrl Pts',(18.4206434725494,17.1173098233883,-6.93187405227898));
#97185=CARTESIAN_POINT('Ctrl Pts',(18.4142455115715,17.1182773863933,-6.93226045977063));
#97186=CARTESIAN_POINT('Ctrl Pts',(18.3992670317528,17.1206128745989,-6.93316356009079));
#97187=CARTESIAN_POINT('Ctrl Pts',(18.3906902582332,17.1220043277417,-6.93367950166247));
#97188=CARTESIAN_POINT('Ctrl Pts',(18.3628466393357,17.1266976499274,-6.93535079193471));
#97189=CARTESIAN_POINT('Ctrl Pts',(18.3436165531952,17.1302136327904,-6.93649934323863));
#97190=CARTESIAN_POINT('Ctrl Pts',(18.2453589231027,17.1495889630137,-6.9423423322874));
#97191=CARTESIAN_POINT('Ctrl Pts',(18.1672306245918,17.1696866760889,-6.94689956594685));
#97192=CARTESIAN_POINT('Ctrl Pts',(17.9590495531097,17.2361177755839,-6.95901426384232));
#97193=CARTESIAN_POINT('Ctrl Pts',(17.8320833022347,17.2907778884386,-6.96635672375421));
#97194=CARTESIAN_POINT('Ctrl Pts',(17.6378519725247,17.3979384419581,-6.97858082056443));
#97195=CARTESIAN_POINT('Ctrl Pts',(17.5668516874556,17.4428104892378,-6.98329659776018));
#97196=CARTESIAN_POINT('Ctrl Pts',(17.4909173473504,17.4973703412839,-6.9888371237247));
#97197=CARTESIAN_POINT('Ctrl Pts',(17.4831624783123,17.5030226655329,-6.98940904968154));
#97198=CARTESIAN_POINT('Ctrl Pts',(17.4717473791631,17.5114622734323,-6.99026041382681));
#97199=CARTESIAN_POINT('Ctrl Pts',(17.4680572509929,17.5142091707707,-6.99053711437982));
#97200=CARTESIAN_POINT('Ctrl Pts',(17.4616350699228,17.5190223941911,-6.99102132398669));
#97201=CARTESIAN_POINT('Ctrl Pts',(17.4588990429345,17.5210833502882,-6.99122845620957));
#97202=CARTESIAN_POINT('Ctrl Pts',(17.4530089302522,17.5255426202666,-6.99167621348503));
#97203=CARTESIAN_POINT('Ctrl Pts',(17.4498566198019,17.5279431149931,-6.99191698836922));
#97204=CARTESIAN_POINT('Ctrl Pts',(17.4415027435178,17.5343417510787,-6.99255805600139));
#97205=CARTESIAN_POINT('Ctrl Pts',(17.43631304118,17.5383552092597,-6.9929594065589));
#97206=CARTESIAN_POINT('Ctrl Pts',(17.4247881020536,17.547353945514,-6.99385746926857));
#97207=CARTESIAN_POINT('Ctrl Pts',(17.4184625488946,17.5523513939098,-6.99435498162914));
#97208=CARTESIAN_POINT('Ctrl Pts',(17.3994038955279,17.5675861227047,-6.99586756640451));
#97209=CARTESIAN_POINT('Ctrl Pts',(17.3867609144634,17.5779345554961,-6.99688951071415));
#97210=CARTESIAN_POINT('Ctrl Pts',(17.3401742285271,17.6169754966851,-7.00072079354399));
#97211=CARTESIAN_POINT('Ctrl Pts',(17.307018604272,17.6465870132565,-7.00357916107475));
#97212=CARTESIAN_POINT('Ctrl Pts',(17.226167502462,17.7235054878837,-7.01083888461658));
#97213=CARTESIAN_POINT('Ctrl Pts',(17.1797448443081,17.7720805639972,-7.01527737022366));
#97214=CARTESIAN_POINT('Ctrl Pts',(17.02753038308,17.947328282661,-7.03061698230959));
#97215=CARTESIAN_POINT('Ctrl Pts',(16.9342592505177,18.0841203921432,-7.04140633576255));
#97216=CARTESIAN_POINT('Ctrl Pts',(16.846879536144,18.2513007538768,-7.0530243892142));
#97217=CARTESIAN_POINT('Ctrl Pts',(16.8362948863819,18.2724044211339,-7.05446608172364));
#97218=CARTESIAN_POINT('Ctrl Pts',(16.8218844196206,18.3023768133364,-7.05647961300132));
#97219=CARTESIAN_POINT('Ctrl Pts',(16.8177631848946,18.3111008049072,-7.05706168934745));
#97220=CARTESIAN_POINT('Ctrl Pts',(16.8111821268346,18.3252820697487,-7.05800151106406));
#97221=CARTESIAN_POINT('Ctrl Pts',(16.8086855895395,18.330722062443,-7.05836052248939));
#97222=CARTESIAN_POINT('Ctrl Pts',(16.8035223705421,18.3420998394459,-7.05910828502606));
#97223=CARTESIAN_POINT('Ctrl Pts',(16.8008599314519,18.3480394889209,-7.05949688706339));
#97224=CARTESIAN_POINT('Ctrl Pts',(16.7946166550279,18.3621415395365,-7.06041540283663));
#97225=CARTESIAN_POINT('Ctrl Pts',(16.7910598711285,18.3703145035281,-7.06094448868439));
#97226=CARTESIAN_POINT('Ctrl Pts',(16.7793656291721,18.3976568086257,-7.06270391232643));
#97227=CARTESIAN_POINT('Ctrl Pts',(16.771459252064,18.4169241038271,-7.0639263982704));
#97228=CARTESIAN_POINT('Ctrl Pts',(16.7574991989216,18.4524265643442,-7.06614908213932));
#97229=CARTESIAN_POINT('Ctrl Pts',(16.7513592056384,18.4686224831075,-7.0671518274129));
#97230=CARTESIAN_POINT('Ctrl Pts',(16.7454194586292,18.4848895190942,-7.06814843723424));
#97231=CARTESIAN_POINT('Ctrl Pts',(16.7454194487812,18.4848895460645,-6.84500598950246));
#97232=CARTESIAN_POINT('Ctrl Pts',(16.7542717826021,18.4606458806915,-6.84330234745308));
#97233=CARTESIAN_POINT('Ctrl Pts',(16.7635672791046,18.4365646067694,-6.841595978446));
#97234=CARTESIAN_POINT('Ctrl Pts',(16.7883633738557,18.3756663207375,-6.83725152870356));
#97235=CARTESIAN_POINT('Ctrl Pts',(16.8044693734147,18.3391078640125,-6.83461588640926));
#97236=CARTESIAN_POINT('Ctrl Pts',(16.8668107437039,18.2078026951508,-6.82507743024927));
#97237=CARTESIAN_POINT('Ctrl Pts',(16.9190749575734,18.1160785924445,-6.81828421870596));
#97238=CARTESIAN_POINT('Ctrl Pts',(16.997360786519,17.9998107107914,-6.80956858496383));
#97239=CARTESIAN_POINT('Ctrl Pts',(17.017465563447,17.9714819466072,-6.8074349426178));
#97240=CARTESIAN_POINT('Ctrl Pts',(17.0447590019611,17.9349624880055,-6.80466927237634));
#97241=CARTESIAN_POINT('Ctrl Pts',(17.0513256322042,17.9263156573252,-6.80401327697482));
#97242=CARTESIAN_POINT('Ctrl Pts',(17.0621791624435,17.9122499016628,-6.80294414765039));
#97243=CARTESIAN_POINT('Ctrl Pts',(17.0664265223505,17.9068008475623,-6.80252946412771));
#97244=CARTESIAN_POINT('Ctrl Pts',(17.0746921769782,17.8963030071988,-6.80172953693702));
#97245=CARTESIAN_POINT('Ctrl Pts',(17.0787070239505,17.8912516151607,-6.80134416241328));
#97246=CARTESIAN_POINT('Ctrl Pts',(17.0880193242055,17.8796444299269,-6.80045752546651));
#97247=CARTESIAN_POINT('Ctrl Pts',(17.0933329815551,17.8731017315299,-6.79995692052343));
#97248=CARTESIAN_POINT('Ctrl Pts',(17.1077031384188,17.8556221388518,-6.79861712840315));
#97249=CARTESIAN_POINT('Ctrl Pts',(17.1168309339031,17.8447442205895,-6.79778083566769));
#97250=CARTESIAN_POINT('Ctrl Pts',(17.2242910857525,17.7192660218938,-6.78810147157151));
#97251=CARTESIAN_POINT('Ctrl Pts',(17.3345065385012,17.6154068130451,-6.77981373551478));
#97252=CARTESIAN_POINT('Ctrl Pts',(17.5448992440378,17.4558646820692,-6.76546513667802));
#97253=CARTESIAN_POINT('Ctrl Pts',(17.6402645547854,17.3949054109157,-6.75937827347752));
#97254=CARTESIAN_POINT('Ctrl Pts',(17.7804115104198,17.320378466526,-6.75039410020573));
#97255=CARTESIAN_POINT('Ctrl Pts',(17.8214750746974,17.3002204776161,-6.74775612581664));
#97256=CARTESIAN_POINT('Ctrl Pts',(17.8709182998608,17.2779062333554,-6.74453601841656));
#97257=CARTESIAN_POINT('Ctrl Pts',(17.8787018428705,17.2744498228436,-6.74402783233774));
#97258=CARTESIAN_POINT('Ctrl Pts',(17.8905418444945,17.2692773788094,-6.74325257622915));
#97259=CARTESIAN_POINT('Ctrl Pts',(17.8945832588591,17.2675268379475,-6.74298756255724));
#97260=CARTESIAN_POINT('Ctrl Pts',(17.9019055365098,17.2643822894027,-6.74250664980463));
#97261=CARTESIAN_POINT('Ctrl Pts',(17.9051844790447,17.2629839478799,-6.74229101863273));
#97262=CARTESIAN_POINT('Ctrl Pts',(17.9123080012485,17.2599672841148,-6.74182194653694));
#97263=CARTESIAN_POINT('Ctrl Pts',(17.9161537854684,17.2583520624674,-6.74156832750422));
#97264=CARTESIAN_POINT('Ctrl Pts',(17.9267613282122,17.2539337502809,-6.74086779275596));
#97265=CARTESIAN_POINT('Ctrl Pts',(17.933532815508,17.2511543780254,-6.74041948361966));
#97266=CARTESIAN_POINT('Ctrl Pts',(17.9681041072299,17.2371735674588,-6.73812552826431));
#97267=CARTESIAN_POINT('Ctrl Pts',(17.9961236412471,17.2265288938429,-6.7362494315757));
#97268=CARTESIAN_POINT('Ctrl Pts',(18.1901404732436,17.1574983883093,-6.72318893195346));
#97269=CARTESIAN_POINT('Ctrl Pts',(18.3626269434429,17.1194129446676,-6.71129873582195));
#97270=CARTESIAN_POINT('Ctrl Pts',(18.6346556991437,17.0940979638633,-6.69352822761822));
#97271=CARTESIAN_POINT('Ctrl Pts',(18.7319873364915,17.0917680736615,-6.687345065227));
#97272=CARTESIAN_POINT('Ctrl Pts',(18.8507355155976,17.0971104927864,-6.68004189407997));
#97273=CARTESIAN_POINT('Ctrl Pts',(18.872308998039,17.0984123202289,-6.67872443613411));
#97274=CARTESIAN_POINT('Ctrl Pts',(18.9028802793707,17.1007274360927,-6.67687014940629));
#97275=CARTESIAN_POINT('Ctrl Pts',(18.9118967832209,17.1014683976694,-6.67632481908893));
#97276=CARTESIAN_POINT('Ctrl Pts',(18.9274159536034,17.1028439454771,-6.67538881309296));
#97277=CARTESIAN_POINT('Ctrl Pts',(18.9339208869162,17.1034508732203,-6.67499727370422));
#97278=CARTESIAN_POINT('Ctrl Pts',(18.9463517558567,17.1046687772882,-6.67425052366811));
#97279=CARTESIAN_POINT('Ctrl Pts',(18.9522781159087,17.1052746728933,-6.67389515711057));
#97280=CARTESIAN_POINT('Ctrl Pts',(18.9676413680116,17.1069109273403,-6.67297554674825));
#97281=CARTESIAN_POINT('Ctrl Pts',(18.9770740948524,17.107979766287,-6.67241251892353));
#97282=CARTESIAN_POINT('Ctrl Pts',(19.0090051611747,17.1118156396605,-6.67051175500974));
#97283=CARTESIAN_POINT('Ctrl Pts',(19.0314666218217,17.1148806129644,-6.66918340357585));
#97284=CARTESIAN_POINT('Ctrl Pts',(19.2313636942161,17.1454355377504,-6.65742898485418));
#97285=CARTESIAN_POINT('Ctrl Pts',(19.404676806609,17.195032170277,-6.64779521464117));
#97286=CARTESIAN_POINT('Ctrl Pts',(19.6470153661258,17.2991475469224,-6.63343394423946));
#97287=CARTESIAN_POINT('Ctrl Pts',(19.7223109119337,17.336962601843,-6.62881653874044));
#97288=CARTESIAN_POINT('Ctrl Pts',(19.8272525208583,17.3977530694884,-6.62188710606429));
#97289=CARTESIAN_POINT('Ctrl Pts',(19.8588597232794,17.4171896058946,-6.61973081920961));
#97290=CARTESIAN_POINT('Ctrl Pts',(19.8962461114954,17.4415566759158,-6.61707543990428));
#97291=CARTESIAN_POINT('Ctrl Pts',(19.9025324118179,17.4457018100329,-6.61662530105815));
#97292=CARTESIAN_POINT('Ctrl Pts',(19.9122680213522,17.4521961776536,-6.61592225292707));
#97293=CARTESIAN_POINT('Ctrl Pts',(19.915732796055,17.4545222706566,-6.61567087382351));
#97294=CARTESIAN_POINT('Ctrl Pts',(19.9221442361277,17.4588541783392,-6.61520348087342));
#97295=CARTESIAN_POINT('Ctrl Pts',(19.9250927217109,17.46085719614,-6.61498765563757));
#97296=CARTESIAN_POINT('Ctrl Pts',(19.9317454213994,17.4654012249909,-6.6144986967956));
#97297=CARTESIAN_POINT('Ctrl Pts',(19.935446594759,17.4679465708481,-6.61422527205207));
#97298=CARTESIAN_POINT('Ctrl Pts',(19.9463423611838,17.4754909242637,-6.61341628429759));
#97299=CARTESIAN_POINT('Ctrl Pts',(19.9535139529155,17.4805227637334,-6.61287856085702));
#97300=CARTESIAN_POINT('Ctrl Pts',(20.0049966928034,17.5171238217646,-6.60898162470858));
#97301=CARTESIAN_POINT('Ctrl Pts',(20.0481037410525,17.5503436940706,-6.60552146289336));
#97302=CARTESIAN_POINT('Ctrl Pts',(20.2180186132341,17.6920472974389,-6.59121261856002));
#97303=CARTESIAN_POINT('Ctrl Pts',(20.3330781890264,17.8136866714715,-6.57998094787372));
#97304=CARTESIAN_POINT('Ctrl Pts',(20.4685097855369,17.9957749917055,-6.56533809923714));
#97305=CARTESIAN_POINT('Ctrl Pts',(20.5022877663718,18.0454720353527,-6.56152228729835));
#97306=CARTESIAN_POINT('Ctrl Pts',(20.5531251358018,18.1275771059215,-6.55550870807867));
#97307=CARTESIAN_POINT('Ctrl Pts',(20.5715361753906,18.1591052849395,-6.55326417240459));
#97308=CARTESIAN_POINT('Ctrl Pts',(20.594449000166,18.2007818531165,-6.5503782671967));
#97309=CARTESIAN_POINT('Ctrl Pts',(20.5996985063427,18.2105099814582,-6.54971025202415));
#97310=CARTESIAN_POINT('Ctrl Pts',(20.6081250907205,18.2264226922063,-6.54862653089586));
#97311=CARTESIAN_POINT('Ctrl Pts',(20.611348271691,18.232582502577,-6.54820919337355));
#97312=CARTESIAN_POINT('Ctrl Pts',(20.6174971544572,18.2444758668491,-6.54740752543332));
#97313=CARTESIAN_POINT('Ctrl Pts',(20.6204271601951,18.2502070974958,-6.54702304632916));
#97314=CARTESIAN_POINT('Ctrl Pts',(20.6270881511519,18.2633842489653,-6.54614320696507));
#97315=CARTESIAN_POINT('Ctrl Pts',(20.630801443708,18.2708390319669,-6.54564847142312));
#97316=CARTESIAN_POINT('Ctrl Pts',(20.6405752572889,18.2907545002039,-6.54433468192988));
#97317=CARTESIAN_POINT('Ctrl Pts',(20.6465576615999,18.3032532311985,-6.54351834672962));
#97318=CARTESIAN_POINT('Ctrl Pts',(20.6927450726799,18.4022341383204,-6.53711580671033));
#97319=CARTESIAN_POINT('Ctrl Pts',(20.7271898048286,18.4912902204123,-6.5317346905494));
#97320=CARTESIAN_POINT('Ctrl Pts',(20.7967396199892,18.7149466265282,-6.51880067871141));
#97321=CARTESIAN_POINT('Ctrl Pts',(20.8248222289333,18.8512449395767,-6.51141816111785));
#97322=CARTESIAN_POINT('Ctrl Pts',(20.8447997532398,19.040965656807,-6.50085289854419));
#97323=CARTESIAN_POINT('Ctrl Pts',(20.8483359065685,19.0928043126347,-6.49793397667051));
#97324=CARTESIAN_POINT('Ctrl Pts',(20.8508174969009,19.1720241999118,-6.49335590827038));
#97325=CARTESIAN_POINT('Ctrl Pts',(20.8511441638215,19.1993441915293,-6.49175579928983));
#97326=CARTESIAN_POINT('Ctrl Pts',(20.8508913970721,19.2335106195167,-6.48971962733981));
#97327=CARTESIAN_POINT('Ctrl Pts',(20.8508074859012,19.2403594906786,-6.48930970074442));
#97328=CARTESIAN_POINT('Ctrl Pts',(20.8506215274288,19.2512305543346,-6.48865606439309));
#97329=CARTESIAN_POINT('Ctrl Pts',(20.8505412462194,19.2552531389646,-6.4884135560312));
#97330=CARTESIAN_POINT('Ctrl Pts',(20.8503676775473,19.2628625857655,-6.48795354559231));
#97331=CARTESIAN_POINT('Ctrl Pts',(20.850276738111,19.2664494487498,-6.48773617604299));
#97332=CARTESIAN_POINT('Ctrl Pts',(20.8500471308375,19.2746798377041,-6.4872361893731));
#97333=CARTESIAN_POINT('Ctrl Pts',(20.8499022964849,19.2793231471537,-6.48695323076861));
#97334=CARTESIAN_POINT('Ctrl Pts',(20.8494750150797,19.2917127346766,-6.48619593355269));
#97335=CARTESIAN_POINT('Ctrl Pts',(20.8491653073926,19.2994579174424,-6.4857201318927));
#97336=CARTESIAN_POINT('Ctrl Pts',(20.8466146950027,19.3555286809475,-6.48225915387325));
#97337=CARTESIAN_POINT('Ctrl Pts',(20.8427605623458,19.4037627607391,-6.47919366098141));
#97338=CARTESIAN_POINT('Ctrl Pts',(20.8363724581257,19.4595552149184,-6.47557653274864));
#97339=CARTESIAN_POINT('Ctrl Pts',(20.835443900775,19.4672872938789,-6.47507364404561));
#97340=CARTESIAN_POINT('Ctrl Pts',(20.8135613229882,19.6413832073111,-6.46371677511084));
#97341=CARTESIAN_POINT('Ctrl Pts',(20.7729588608621,19.8046828863509,-6.45243043119019));
#97342=CARTESIAN_POINT('Ctrl Pts',(20.6927142930439,20.016336967326,-6.4378402413365));
#97343=CARTESIAN_POINT('Ctrl Pts',(20.669649319687,20.0702973883572,-6.43411711356651));
#97344=CARTESIAN_POINT('Ctrl Pts',(20.6289065285392,20.1556196158572,-6.42823223849908));
#97345=CARTESIAN_POINT('Ctrl Pts',(20.6126202391513,20.1876080150737,-6.42602616881911));
#97346=CARTESIAN_POINT('Ctrl Pts',(20.5902955315046,20.2288293608739,-6.42318188884288));
#97347=CARTESIAN_POINT('Ctrl Pts',(20.5849881747801,20.2384495082936,-6.42251797734894));
#97348=CARTESIAN_POINT('Ctrl Pts',(20.5762078322756,20.2540759454207,-6.4214392388114));
#97349=CARTESIAN_POINT('Ctrl Pts',(20.5727798390621,20.2601071587089,-6.42102280835963));
#97350=CARTESIAN_POINT('Ctrl Pts',(20.566111590863,20.2717061873592,-6.42022174937132));
#97351=CARTESIAN_POINT('Ctrl Pts',(20.5628754514984,20.2772762688906,-6.41983697818318));
#97352=CARTESIAN_POINT('Ctrl Pts',(20.5553804521501,20.2900422442813,-6.41895488215932));
#97353=CARTESIAN_POINT('Ctrl Pts',(20.5511042652016,20.2972278807256,-6.41845819292656));
#97354=CARTESIAN_POINT('Ctrl Pts',(20.539570289496,20.3163506654378,-6.41713576716577));
#97355=CARTESIAN_POINT('Ctrl Pts',(20.5322366493738,20.3282417512292,-6.4163128071395));
#97356=CARTESIAN_POINT('Ctrl Pts',(20.4714597550209,20.4246391378215,-6.40963398814145));
#97357=CARTESIAN_POINT('Ctrl Pts',(20.4122054460579,20.5053401891908,-6.40400493477306));
#97358=CARTESIAN_POINT('Ctrl Pts',(20.2361477277666,20.7126004429819,-6.38901948579182));
#97359=CARTESIAN_POINT('Ctrl Pts',(20.1092982871116,20.8295779733223,-6.37998267350489));
#97360=CARTESIAN_POINT('Ctrl Pts',(19.9372872114692,20.9532354276985,-6.36791331017267));
#97361=CARTESIAN_POINT('Ctrl Pts',(19.9042045042924,20.9756261225481,-6.365596850404));
#97362=CARTESIAN_POINT('Ctrl Pts',(19.8640240857614,21.0011937552643,-6.36276398877022));
#97363=CARTESIAN_POINT('Ctrl Pts',(19.8575149910715,21.0052859795811,-6.36230448079656));
#97364=CARTESIAN_POINT('Ctrl Pts',(19.8474096033598,21.0115626229168,-6.36158994396203));
#97365=CARTESIAN_POINT('Ctrl Pts',(19.8438287692874,21.0137719783861,-6.36133652680632));
#97366=CARTESIAN_POINT('Ctrl Pts',(19.8372045120686,21.0178318935702,-6.36086727086378));
#97367=CARTESIAN_POINT('Ctrl Pts',(19.8341629956337,21.019685453459,-6.36065163302646));
#97368=CARTESIAN_POINT('Ctrl Pts',(19.8273126405839,21.0238365220129,-6.36016555465843));
#97369=CARTESIAN_POINT('Ctrl Pts',(19.823501255424,21.0261296921151,-6.35989483812831));
#97370=CARTESIAN_POINT('Ctrl Pts',(19.8137316770894,21.0319658312249,-6.35920028003406));
#97371=CARTESIAN_POINT('Ctrl Pts',(19.8077633105948,21.0354915463709,-6.35877535810323));
#97372=CARTESIAN_POINT('Ctrl Pts',(19.7728187316377,21.0559036334383,-6.35628441180358));
#97373=CARTESIAN_POINT('Ctrl Pts',(19.7434635709076,21.0721278251695,-6.35417977705838));
#97374=CARTESIAN_POINT('Ctrl Pts',(19.6975154986552,21.0961158477308,-6.35088121460067));
#97375=CARTESIAN_POINT('Ctrl Pts',(19.6811848393107,21.1043738984421,-6.34970802781307));
#97376=CARTESIAN_POINT('Ctrl Pts',(19.6425620540246,21.1232798543988,-6.3469347502455));
#97377=CARTESIAN_POINT('Ctrl Pts',(19.6201866552675,21.1337512561645,-6.34532916655376));
#97378=CARTESIAN_POINT('Ctrl Pts',(19.5566233451991,21.1621528575067,-6.34078013147681));
#97379=CARTESIAN_POINT('Ctrl Pts',(19.5150409727976,21.17916703077,-6.33781845401844));
#97380=CARTESIAN_POINT('Ctrl Pts',(19.3704829516139,21.2330125310946,-6.32762833885687));
#97381=CARTESIAN_POINT('Ctrl Pts',(19.2652049043434,21.2631866484315,-6.32039830780838));
#97382=CARTESIAN_POINT('Ctrl Pts',(19.1041214859697,21.2961211436827,-6.30983047334516));
#97383=CARTESIAN_POINT('Ctrl Pts',(19.0497689864349,21.3050417532998,-6.30634427344008));
#97384=CARTESIAN_POINT('Ctrl Pts',(18.9611055016932,21.3160623291872,-6.300790834217));
#97385=CARTESIAN_POINT('Ctrl Pts',(18.9269852360094,21.3194641882862,-6.29868522734318));
#97386=CARTESIAN_POINT('Ctrl Pts',(18.8820200895347,21.3228465439308,-6.29595006980075));
#97387=CARTESIAN_POINT('Ctrl Pts',(18.8712382214932,21.3235746020818,-6.2952972070506));
#97388=CARTESIAN_POINT('Ctrl Pts',(18.853565907974,21.3246320798939,-6.29423187936506));
#97389=CARTESIAN_POINT('Ctrl Pts',(18.8466786887468,21.3250104281578,-6.29381788593897));
#97390=CARTESIAN_POINT('Ctrl Pts',(18.8333408036691,21.3256777761247,-6.2930183901391));
#97391=CARTESIAN_POINT('Ctrl Pts',(18.826890431207,21.3259709362838,-6.29263276163655));
#97392=CARTESIAN_POINT('Ctrl Pts',(18.8119899302177,21.3265798431543,-6.29174425608576));
#97393=CARTESIAN_POINT('Ctrl Pts',(18.803539013247,21.3268744837012,-6.29124204551304));
#97394=CARTESIAN_POINT('Ctrl Pts',(18.780798330885,21.327530944038,-6.28989511001955));
#97395=CARTESIAN_POINT('Ctrl Pts',(18.766506135588,21.3277986883303,-6.28905332875827));
#97396=CARTESIAN_POINT('Ctrl Pts',(18.6350479473451,21.3289296343791,-6.28135182955752));
#97397=CARTESIAN_POINT('Ctrl Pts',(18.5179952710973,21.3202094958374,-6.27481074064599));
#97398=CARTESIAN_POINT('Ctrl Pts',(18.2404054607923,21.2761651782157,-6.25942582748462));
#97399=CARTESIAN_POINT('Ctrl Pts',(18.0821083834066,21.2317839446089,-6.25076841785113));
#97400=CARTESIAN_POINT('Ctrl Pts',(17.9016686478125,21.1577631798093,-6.23955361856694));
#97401=CARTESIAN_POINT('Ctrl Pts',(17.8730712644509,21.1452863897801,-6.23773209066369));
#97402=CARTESIAN_POINT('Ctrl Pts',(17.8382749421488,21.1291805739933,-6.2354486451909));
#97403=CARTESIAN_POINT('Ctrl Pts',(17.8318034794302,21.1261453022322,-6.23502107246662));
#97404=CARTESIAN_POINT('Ctrl Pts',(17.8216539555023,21.121322072134,-6.2343457361428));
#97405=CARTESIAN_POINT('Ctrl Pts',(17.8179654230808,21.1195560975331,-6.23409931402452));
#97406=CARTESIAN_POINT('Ctrl Pts',(17.8110620447559,21.116226315056,-6.23363621153203));
#97407=CARTESIAN_POINT('Ctrl Pts',(17.8078460352514,21.1146650476691,-6.23341968899333));
#97408=CARTESIAN_POINT('Ctrl Pts',(17.8004896490396,21.1110707094039,-6.23292262777543));
#97409=CARTESIAN_POINT('Ctrl Pts',(17.7963519644209,21.1090322538171,-6.23264175658664));
#97410=CARTESIAN_POINT('Ctrl Pts',(17.7855282348213,21.1036558472467,-6.23190369962673));
#97411=CARTESIAN_POINT('Ctrl Pts',(17.7788532122828,21.1002960211633,-6.23144519783144));
#97412=CARTESIAN_POINT('Ctrl Pts',(17.7341725928776,21.0775090411018,-6.22835435280912));
#97413=CARTESIAN_POINT('Ctrl Pts',(17.6967469833069,21.0569730377007,-6.22565941268588));
#97414=CARTESIAN_POINT('Ctrl Pts',(17.6537632117779,21.0316672866917,-6.22246029349298));
#97415=CARTESIAN_POINT('Ctrl Pts',(17.6475745373744,21.0279811775343,-6.2219971112341));
#97416=CARTESIAN_POINT('Ctrl Pts',(17.5067332065525,20.9431162113054,-6.21139884241179));
#97417=CARTESIAN_POINT('Ctrl Pts',(17.381520401944,20.8472189954507,-6.2008255891468));
#97418=CARTESIAN_POINT('Ctrl Pts',(17.199636874156,20.6726489938476,-6.18444646102177));
#97419=CARTESIAN_POINT('Ctrl Pts',(17.1356824216191,20.6024284344092,-6.17842083494831));
#97420=CARTESIAN_POINT('Ctrl Pts',(17.0633767519725,20.5114468083211,-6.17128275661141));
#97421=CARTESIAN_POINT('Ctrl Pts',(17.0503589550626,20.4945485273957,-6.1699827097655));
#97422=CARTESIAN_POINT('Ctrl Pts',(17.0322147355866,20.4702445753607,-6.16814848369047));
#97423=CARTESIAN_POINT('Ctrl Pts',(17.0268770668331,20.4629989144223,-6.1676060504374));
#97424=CARTESIAN_POINT('Ctrl Pts',(17.0177495690939,20.4504418205807,-6.16667346354058));
#97425=CARTESIAN_POINT('Ctrl Pts',(17.0139378254337,20.4451465412564,-6.16628246263704));
#97426=CARTESIAN_POINT('Ctrl Pts',(17.0066870509714,20.4349749098116,-6.16553568459262));
#97427=CARTESIAN_POINT('Ctrl Pts',(17.0032440432675,20.430101481866,-6.16517975662665));
#97428=CARTESIAN_POINT('Ctrl Pts',(16.9943461642458,20.4173932482778,-6.1642564187872));
#97429=CARTESIAN_POINT('Ctrl Pts',(16.9889235640272,20.4095359297471,-6.16369024500889));
#97430=CARTESIAN_POINT('Ctrl Pts',(16.9706219475502,20.3826294503584,-6.16176718777194));
#97431=CARTESIAN_POINT('Ctrl Pts',(16.9579999310821,20.3634068469764,-6.16041999637991));
#97432=CARTESIAN_POINT('Ctrl Pts',(16.8517988254439,20.1957782501648,-6.14888904460162));
#97433=CARTESIAN_POINT('Ctrl Pts',(16.7766910280836,20.0364803167671,-6.13945578366972));
#97434=CARTESIAN_POINT('Ctrl Pts',(16.6950139619086,19.7870198790295,-6.12517347561472));
#97435=CARTESIAN_POINT('Ctrl Pts',(16.6730620310302,19.7027268103163,-6.12040912916544));
#97436=CARTESIAN_POINT('Ctrl Pts',(16.6490998650406,19.5802038588514,-6.1132812613151));
#97437=CARTESIAN_POINT('Ctrl Pts',(16.6428359520119,19.5428924331231,-6.11108386833566));
#97438=CARTESIAN_POINT('Ctrl Pts',(16.6365221765392,19.4979374778731,-6.10838292032738));
#97439=CARTESIAN_POINT('Ctrl Pts',(16.6355092976289,19.4904335417496,-6.10793029751026));
#97440=CARTESIAN_POINT('Ctrl Pts',(16.6339995005659,19.4787767622308,-6.10722420240243));
#97441=CARTESIAN_POINT('Ctrl Pts',(16.6334745843629,19.4746275205329,-6.10697228172458));
#97442=CARTESIAN_POINT('Ctrl Pts',(16.6325251661749,19.4669398822551,-6.10650439881619));
#97443=CARTESIAN_POINT('Ctrl Pts',(16.6320973021977,19.4634019590237,-6.10628862849065));
#97444=CARTESIAN_POINT('Ctrl Pts',(16.6311517266828,19.4554140134578,-6.10580045824318));
#97445=CARTESIAN_POINT('Ctrl Pts',(16.6306392094336,19.4509634439275,-6.10552777130201));
#97446=CARTESIAN_POINT('Ctrl Pts',(16.6291723816807,19.4378600444509,-6.10472293921759));
#97447=CARTESIAN_POINT('Ctrl Pts',(16.6282573256438,19.4292030385308,-6.10418866596148));
#97448=CARTESIAN_POINT('Ctrl Pts',(16.6221408158919,19.3677111227551,-6.10037676936774));
#97449=CARTESIAN_POINT('Ctrl Pts',(16.6188755557929,19.3147070485057,-6.09700299463916));
#97450=CARTESIAN_POINT('Ctrl Pts',(16.6172125017524,19.2452051771546,-6.09251063184672));
#97451=CARTESIAN_POINT('Ctrl Pts',(16.6170107020447,19.2287651447115,-6.09144296094795));
#97452=CARTESIAN_POINT('Ctrl Pts',(16.6169886659552,19.1935499070994,-6.0891472088716));
#97453=CARTESIAN_POINT('Ctrl Pts',(16.6172266779166,19.1747760437117,-6.08791797418893));
#97454=CARTESIAN_POINT('Ctrl Pts',(16.6217705573637,18.9999111347366,-6.07643128804281));
#97455=CARTESIAN_POINT('Ctrl Pts',(16.6430861467256,18.8447196224014,-6.06600971984951));
#97456=CARTESIAN_POINT('Ctrl Pts',(16.6824574159065,18.6886158924888,-6.05574886267654));
#97457=CARTESIAN_POINT('Ctrl Pts',(16.6836494631439,18.6839565419554,-6.05544275861447));
#97458=CARTESIAN_POINT('Ctrl Pts',(16.7007616129654,18.6180070985914,-6.05111241008373));
#97459=CARTESIAN_POINT('Ctrl Pts',(16.7194091022808,18.5574529387656,-6.04716616922773));
#97460=CARTESIAN_POINT('Ctrl Pts',(16.7422893639867,18.4935052270817,-6.04302901175127));
#97461=CARTESIAN_POINT('Ctrl Pts',(16.7438474130825,18.4891948409118,-6.04275028930809));
#97462=CARTESIAN_POINT('Ctrl Pts',(16.7454194503114,18.4848895418737,-6.04247203357104));
#97463=CARTESIAN_POINT('Origin',(18.734,19.211,0.));
#97464=CARTESIAN_POINT('',(16.745419381199,18.4848897311503,-5.24452701096004));
#97465=CARTESIAN_POINT('',(16.7454194503191,18.4848895418526,-5.46434828430915));
#97466=CARTESIAN_POINT('',(16.7454194503191,18.4848895418526,0.));
#97467=CARTESIAN_POINT('',(16.6170006442152,19.2093484532524,-5.51218499391188));
#97468=CARTESIAN_POINT('Ctrl Pts',(16.7454194503191,18.4848895418527,-5.46434828430915));
#97469=CARTESIAN_POINT('Ctrl Pts',(16.7446923999496,18.4868806965141,-5.4644758422322));
#97470=CARTESIAN_POINT('Ctrl Pts',(16.7439683437551,18.4888729333669,-5.46460357631697));
#97471=CARTESIAN_POINT('Ctrl Pts',(16.7420339915519,18.4942202967959,-5.46494672233998));
#97472=CARTESIAN_POINT('Ctrl Pts',(16.7408292055697,18.4975773302596,-5.46516246031084));
#97473=CARTESIAN_POINT('Ctrl Pts',(16.7382405876864,18.5048480337378,-5.46563039949849));
#97474=CARTESIAN_POINT('Ctrl Pts',(16.7368598003935,18.5087626799101,-5.46588277144038));
#97475=CARTESIAN_POINT('Ctrl Pts',(16.7330402093437,18.5196939195587,-5.46658863297378));
#97476=CARTESIAN_POINT('Ctrl Pts',(16.7306268379231,18.5267192459324,-5.46704358502534));
#97477=CARTESIAN_POINT('Ctrl Pts',(16.7169221932686,18.5673074602492,-5.46967895501753));
#97478=CARTESIAN_POINT('Ctrl Pts',(16.70643819295,18.6011346529457,-5.47190251098958));
#97479=CARTESIAN_POINT('Ctrl Pts',(16.6756286877856,18.7101405100038,-5.47911945319092));
#97480=CARTESIAN_POINT('Ctrl Pts',(16.6586012281405,18.7861812344539,-5.48422947167187));
#97481=CARTESIAN_POINT('Ctrl Pts',(16.6267248929344,18.977447016726,-5.497026588454));
#97482=CARTESIAN_POINT('Ctrl Pts',(16.617091182629,19.0932937524003,-5.50471798017525));
#97483=CARTESIAN_POINT('Ctrl Pts',(16.6170006442152,19.2093484532524,-5.51218499391188));
#97484=CARTESIAN_POINT('Ctrl Pts',(16.6170006421798,19.2093510643075,-5.51218516190835));
#97485=CARTESIAN_POINT('Ctrl Pts',(16.6169350228221,19.2935970047459,-5.517605582707));
#97486=CARTESIAN_POINT('Ctrl Pts',(16.6218981977752,19.3777818118907,-5.52290047725799));
#97487=CARTESIAN_POINT('Ctrl Pts',(16.6330988038497,19.471789986764,-5.52867286592509));
#97488=CARTESIAN_POINT('Ctrl Pts',(16.6344059037781,19.4821123205625,-5.52930484381016));
#97489=CARTESIAN_POINT('Ctrl Pts',(16.636738347915,19.4995022617998,-5.53036650859551));
#97490=CARTESIAN_POINT('Ctrl Pts',(16.6377234400716,19.5065749966085,-5.53079745786133));
#97491=CARTESIAN_POINT('Ctrl Pts',(16.6396009364873,19.5195732790937,-5.53158794109212));
#97492=CARTESIAN_POINT('Ctrl Pts',(16.6404827460144,19.5255002610929,-5.53194780640628));
#97493=CARTESIAN_POINT('Ctrl Pts',(16.6423536689177,19.5377188184431,-5.53268850407761));
#97494=CARTESIAN_POINT('Ctrl Pts',(16.6433460333441,19.5440098402922,-5.53306922932213));
#97495=CARTESIAN_POINT('Ctrl Pts',(16.6456303020622,19.5580780255571,-5.53391922565105));
#97496=CARTESIAN_POINT('Ctrl Pts',(16.6469372945572,19.5658526697254,-5.53438801268315));
#97497=CARTESIAN_POINT('Ctrl Pts',(16.6503587999105,19.5855324378407,-5.53557231933836));
#97498=CARTESIAN_POINT('Ctrl Pts',(16.6525319505521,19.5974271806305,-5.53628597239032));
#97499=CARTESIAN_POINT('Ctrl Pts',(16.6655166081195,19.6652087964251,-5.54034126659226));
#97500=CARTESIAN_POINT('Ctrl Pts',(16.6784773190028,19.720663137167,-5.5436137078366));
#97501=CARTESIAN_POINT('Ctrl Pts',(16.7044778513509,19.8146348024952,-5.54912152047655));
#97502=CARTESIAN_POINT('Ctrl Pts',(16.7164193736241,19.8534202410136,-5.55138376998296));
#97503=CARTESIAN_POINT('Ctrl Pts',(16.7740763462376,20.0231741252782,-5.56128903855644));
#97504=CARTESIAN_POINT('Ctrl Pts',(16.8314807496511,20.1498001938405,-5.56866564273553));
#97505=CARTESIAN_POINT('Ctrl Pts',(16.9272998012879,20.3156803760131,-5.5792670548473));
#97506=CARTESIAN_POINT('Ctrl Pts',(16.955449295854,20.3604524660741,-5.58223563216153));
#97507=CARTESIAN_POINT('Ctrl Pts',(17.0008241867492,20.4269584435849,-5.58688419654007));
#97508=CARTESIAN_POINT('Ctrl Pts',(17.0168505965829,20.4494874230843,-5.58850295395942));
#97509=CARTESIAN_POINT('Ctrl Pts',(17.0374075367327,20.4772188974816,-5.59056000568632));
#97510=CARTESIAN_POINT('Ctrl Pts',(17.0415292359698,20.4827228442926,-5.59097151644611));
#97511=CARTESIAN_POINT('Ctrl Pts',(17.0481085688684,20.4914199772946,-5.5916271016444));
#97512=CARTESIAN_POINT('Ctrl Pts',(17.0505486724653,20.4946264499519,-5.59186996237869));
#97513=CARTESIAN_POINT('Ctrl Pts',(17.0551780844881,20.5006739279624,-5.59233023868622));
#97514=CARTESIAN_POINT('Ctrl Pts',(17.0573654641445,20.5035163429982,-5.59254751940847));
#97515=CARTESIAN_POINT('Ctrl Pts',(17.0623961945627,20.5100193232251,-5.59304677427222));
#97516=CARTESIAN_POINT('Ctrl Pts',(17.0652443490526,20.5136761151391,-5.59332908639859));
#97517=CARTESIAN_POINT('Ctrl Pts',(17.0728655611403,20.5233951038866,-5.59408353521667));
#97518=CARTESIAN_POINT('Ctrl Pts',(17.0776597391594,20.5294405442933,-5.59455711801425));
#97519=CARTESIAN_POINT('Ctrl Pts',(17.1122279307319,20.5725447872489,-5.59796386322302));
#97520=CARTESIAN_POINT('Ctrl Pts',(17.1432073900363,20.608614740661,-5.60097459101504));
#97521=CARTESIAN_POINT('Ctrl Pts',(17.1951783807622,20.6651573822001,-5.6059183148775));
#97522=CARTESIAN_POINT('Ctrl Pts',(17.2154292583923,20.686292669097,-5.60782052074561));
#97523=CARTESIAN_POINT('Ctrl Pts',(17.2868157387307,20.7577692559931,-5.61442594194357));
#97524=CARTESIAN_POINT('Ctrl Pts',(17.3400677892033,20.8059263580313,-5.61918105526391));
#97525=CARTESIAN_POINT('Ctrl Pts',(17.4767036864319,20.9174100614128,-5.63082310362648));
#97526=CARTESIAN_POINT('Ctrl Pts',(17.5625427734562,20.9774431558819,-5.63766787015467));
#97527=CARTESIAN_POINT('Ctrl Pts',(17.6871080699928,21.0514698403135,-5.64685779627215));
#97528=CARTESIAN_POINT('Ctrl Pts',(17.7223220099948,21.0710591191976,-5.6493812006332));
#97529=CARTESIAN_POINT('Ctrl Pts',(17.7742766688073,21.0980488708036,-5.65299758058682));
#97530=CARTESIAN_POINT('Ctrl Pts',(17.7905864472094,21.1062554483016,-5.65411804418506));
#97531=CARTESIAN_POINT('Ctrl Pts',(17.8200118227736,21.120587405612,-5.65611352202763));
#97532=CARTESIAN_POINT('Ctrl Pts',(17.83308777644,21.1267911236725,-5.65699120926473));
#97533=CARTESIAN_POINT('Ctrl Pts',(17.8531817375395,21.1360732154926,-5.65832641127633));
#97534=CARTESIAN_POINT('Ctrl Pts',(17.8601543557683,21.1392482954628,-5.65878725732571));
#97535=CARTESIAN_POINT('Ctrl Pts',(17.872950307635,21.1449914503523,-5.65962853019147));
#97536=CARTESIAN_POINT('Ctrl Pts',(17.878768256399,21.1475712403278,-5.66000935620905));
#97537=CARTESIAN_POINT('Ctrl Pts',(17.8913115781374,21.1530656392479,-5.66082684493576));
#97538=CARTESIAN_POINT('Ctrl Pts',(17.8980406479681,21.1559716417756,-5.6612632095029));
#97539=CARTESIAN_POINT('Ctrl Pts',(17.9162253257146,21.1637130330821,-5.6624366333298));
#97540=CARTESIAN_POINT('Ctrl Pts',(17.9277087764944,21.1684825874829,-5.66317145057699));
#97541=CARTESIAN_POINT('Ctrl Pts',(17.9825479372701,21.1906951074065,-5.6666520442154));
#97542=CARTESIAN_POINT('Ctrl Pts',(18.0264332470636,21.206801264651,-5.66935264452889));
#97543=CARTESIAN_POINT('Ctrl Pts',(18.2543902931222,21.2819971200523,-5.68301461480048));
#97544=CARTESIAN_POINT('Ctrl Pts',(18.4453739919648,21.3171209258884,-5.69315886758305));
#97545=CARTESIAN_POINT('Ctrl Pts',(18.6897804587139,21.3281613038901,-5.706714952772));
#97546=CARTESIAN_POINT('Ctrl Pts',(18.7411570699376,21.3286107812708,-5.70960274343206));
#97547=CARTESIAN_POINT('Ctrl Pts',(18.8196003149383,21.3264424644324,-5.71413655144819));
#97548=CARTESIAN_POINT('Ctrl Pts',(18.8466868366006,21.3251725933766,-5.71572488545301));
#97549=CARTESIAN_POINT('Ctrl Pts',(18.880557488857,21.3229319552709,-5.71774786777438));
#97550=CARTESIAN_POINT('Ctrl Pts',(18.8873726251609,21.3224479667229,-5.71815678419441));
#97551=CARTESIAN_POINT('Ctrl Pts',(18.8981932883466,21.3216268550834,-5.71880917781701));
#97552=CARTESIAN_POINT('Ctrl Pts',(18.902200471189,21.3213112941483,-5.71905146144865));
#97553=CARTESIAN_POINT('Ctrl Pts',(18.9097837904224,21.3206923803924,-5.71951130382944));
#97554=CARTESIAN_POINT('Ctrl Pts',(18.9133600632854,21.3203913453468,-5.71972873153826));
#97555=CARTESIAN_POINT('Ctrl Pts',(18.9215704941605,21.3196791966192,-5.72022919158013));
#97556=CARTESIAN_POINT('Ctrl Pts',(18.9262040716622,21.319261899864,-5.72051256765587));
#97557=CARTESIAN_POINT('Ctrl Pts',(18.9385770418966,21.3181064703368,-5.7212717060231));
#97558=CARTESIAN_POINT('Ctrl Pts',(18.9463137228883,21.3173409795743,-5.72174894236395));
#97559=CARTESIAN_POINT('Ctrl Pts',(19.0026924205808,21.3114489320931,-5.72524443535702));
#97560=CARTESIAN_POINT('Ctrl Pts',(19.0511441512915,21.304680992576,-5.7283447803929));
#97561=CARTESIAN_POINT('Ctrl Pts',(19.2504330645577,21.269767563705,-5.74138160112831));
#97562=CARTESIAN_POINT('Ctrl Pts',(19.3982263174172,21.2269446504282,-5.7516915156213));
#97563=CARTESIAN_POINT('Ctrl Pts',(19.6311631791648,21.1310225334437,-5.76808693086142));
#97564=CARTESIAN_POINT('Ctrl Pts',(19.7195108098392,21.0872093152235,-5.77435330579763));
#97565=CARTESIAN_POINT('Ctrl Pts',(19.8232681037661,21.0263945574511,-5.78174347041408));
#97566=CARTESIAN_POINT('Ctrl Pts',(19.841868960817,21.0151033291436,-5.78307001482165));
#97567=CARTESIAN_POINT('Ctrl Pts',(19.8679739231567,20.9987008781262,-5.78493475864143));
#97568=CARTESIAN_POINT('Ctrl Pts',(19.8756238356116,20.9938253728339,-5.78548159014019));
#97569=CARTESIAN_POINT('Ctrl Pts',(19.8887327029067,20.9853517479328,-5.78641937018984));
#97570=CARTESIAN_POINT('Ctrl Pts',(19.894206715364,20.9817772642732,-5.78681119100015));
#97571=CARTESIAN_POINT('Ctrl Pts',(19.9046328341177,20.9748999964293,-5.78755793698989));
#97572=CARTESIAN_POINT('Ctrl Pts',(19.9095877321843,20.9716015775211,-5.78791302068994));
#97573=CARTESIAN_POINT('Ctrl Pts',(19.9223859275535,20.9630038485013,-5.78883074298802));
#97574=CARTESIAN_POINT('Ctrl Pts',(19.930207767615,20.9576727166509,-5.78939217576493));
#97575=CARTESIAN_POINT('Ctrl Pts',(19.9565036081274,20.9394907711702,-5.7912817371614));
#97576=CARTESIAN_POINT('Ctrl Pts',(19.9748087767351,20.9263976374844,-5.79260063350919));
#97577=CARTESIAN_POINT('Ctrl Pts',(20.138770260746,20.8051228485415,-5.80445696454059));
#97578=CARTESIAN_POINT('Ctrl Pts',(20.270161527352,20.6789309431317,-5.81418241168746));
#97579=CARTESIAN_POINT('Ctrl Pts',(20.4358105302999,20.4729048502185,-5.82858160045585));
#97580=CARTESIAN_POINT('Ctrl Pts',(20.4839171255178,20.405299303186,-5.83313262327671));
#97581=CARTESIAN_POINT('Ctrl Pts',(20.5474539765932,20.3038977391938,-5.83997218089297));
#97582=CARTESIAN_POINT('Ctrl Pts',(20.5661595705515,20.2722406573064,-5.84210956695578));
#97583=CARTESIAN_POINT('Ctrl Pts',(20.5876810783615,20.2335516440555,-5.84474398796897));
#97584=CARTESIAN_POINT('Ctrl Pts',(20.5912969814934,20.2269691549152,-5.84519296543809));
#97585=CARTESIAN_POINT('Ctrl Pts',(20.5968654300036,20.2167031220242,-5.84589458873561));
#97586=CARTESIAN_POINT('Ctrl Pts',(20.5988422903456,20.2130327396858,-5.84614571435808));
#97587=CARTESIAN_POINT('Ctrl Pts',(20.6024894826581,20.2062129230567,-5.84661287935017));
#97588=CARTESIAN_POINT('Ctrl Pts',(20.6041627056437,20.2030651001051,-5.8468287316553));
#97589=CARTESIAN_POINT('Ctrl Pts',(20.6079289510642,20.1959363000461,-5.84731806575701));
#97590=CARTESIAN_POINT('Ctrl Pts',(20.6100172313672,20.1919528915984,-5.8475918406436));
#97591=CARTESIAN_POINT('Ctrl Pts',(20.6161479708735,20.1801672878839,-5.84840280394313));
#97592=CARTESIAN_POINT('Ctrl Pts',(20.6201545053846,20.1723466553952,-5.84894216823161));
#97593=CARTESIAN_POINT('Ctrl Pts',(20.6489204465247,20.1153243465001,-5.85288248004627));
#97594=CARTESIAN_POINT('Ctrl Pts',(20.6717978310808,20.0652021296956,-5.85638687731439));
#97595=CARTESIAN_POINT('Ctrl Pts',(20.7564685845423,19.8587359217368,-5.87082506437484));
#97596=CARTESIAN_POINT('Ctrl Pts',(20.8014990086526,19.6961767047059,-5.88214040023727));
#97597=CARTESIAN_POINT('Ctrl Pts',(20.838952647047,19.4504510447495,-5.89816375150085));
#97598=CARTESIAN_POINT('Ctrl Pts',(20.8465329400232,19.370278524744,-5.90323925098005));
#97599=CARTESIAN_POINT('Ctrl Pts',(20.8502581499253,19.2703449460948,-5.90937017786263));
#97600=CARTESIAN_POINT('Ctrl Pts',(20.8507155673185,19.2508199314504,-5.91055901552437));
#97601=CARTESIAN_POINT('Ctrl Pts',(20.8509860039086,19.2226058436378,-5.9122643639514));
#97602=CARTESIAN_POINT('Ctrl Pts',(20.8510158033641,19.2139203031908,-5.91278763002537));
#97603=CARTESIAN_POINT('Ctrl Pts',(20.8509745295113,19.1987646703921,-5.91369776713135));
#97604=CARTESIAN_POINT('Ctrl Pts',(20.850927248219,19.1922946777547,-5.91408537814049));
#97605=CARTESIAN_POINT('Ctrl Pts',(20.8507784687399,19.1797845197975,-5.91483308798317));
#97606=CARTESIAN_POINT('Ctrl Pts',(20.8506807770335,19.1737443799408,-5.91519330221259));
#97607=CARTESIAN_POINT('Ctrl Pts',(20.8503871358699,19.1593892832168,-5.91604754545429));
#97608=CARTESIAN_POINT('Ctrl Pts',(20.8501680357624,19.1510748601889,-5.91654084616701));
#97609=CARTESIAN_POINT('Ctrl Pts',(20.8492155476901,19.1215405081676,-5.91828807443887));
#97610=CARTESIAN_POINT('Ctrl Pts',(20.8482119193869,19.1003301215115,-5.91953355375152));
#97611=CARTESIAN_POINT('Ctrl Pts',(20.8348468506118,18.8861753481645,-5.93202434393746));
#97612=CARTESIAN_POINT('Ctrl Pts',(20.7964311119478,18.6957800196862,-5.94232524204041));
#97613=CARTESIAN_POINT('Ctrl Pts',(20.7079197406423,18.4422456443887,-5.95699095690298));
#97614=CARTESIAN_POINT('Ctrl Pts',(20.6793748141262,18.3726340348035,-5.96114001020319));
#97615=CARTESIAN_POINT('Ctrl Pts',(20.6323507349037,18.2733673017251,-5.96743216391842));
#97616=CARTESIAN_POINT('Ctrl Pts',(20.6167445704538,18.2424117700734,-5.96945054876323));
#97617=CARTESIAN_POINT('Ctrl Pts',(20.5969027965435,18.2053476455521,-5.97195291795997));
#97618=CARTESIAN_POINT('Ctrl Pts',(20.5933850240021,18.1988583022872,-5.97239429007523));
#97619=CARTESIAN_POINT('Ctrl Pts',(20.5878410500989,18.1887576082805,-5.97308657874437));
#97620=CARTESIAN_POINT('Ctrl Pts',(20.5858380291481,18.1851335079134,-5.97333603970697));
#97621=CARTESIAN_POINT('Ctrl Pts',(20.58208935195,18.1783977158511,-5.97380172914152));
#97622=CARTESIAN_POINT('Ctrl Pts',(20.5803464574785,18.1752845524217,-5.97401778077037));
#97623=CARTESIAN_POINT('Ctrl Pts',(20.5763697942239,18.168223361461,-5.97450967737042));
#97624=CARTESIAN_POINT('Ctrl Pts',(20.5741312109305,18.1642781161047,-5.97478582866334));
#97625=CARTESIAN_POINT('Ctrl Pts',(20.5682967111223,18.1540720438649,-5.97550357216521));
#97626=CARTESIAN_POINT('Ctrl Pts',(20.5646814488057,18.1478224238316,-5.97594636771421));
#97627=CARTESIAN_POINT('Ctrl Pts',(20.5417965212058,18.1087245957527,-5.97873661985179));
#97628=CARTESIAN_POINT('Ctrl Pts',(20.521676651128,18.0763850411015,-5.98113391110635));
#97629=CARTESIAN_POINT('Ctrl Pts',(20.4932674544053,18.0333545240416,-5.98442854375312));
#97630=CARTESIAN_POINT('Ctrl Pts',(20.4857305261716,18.0221724293492,-5.98529459231634));
#97631=CARTESIAN_POINT('Ctrl Pts',(20.4776250015664,18.0103911879699,-5.98621700962352));
#97632=CARTESIAN_POINT('Ctrl Pts',(20.4771621814781,18.009719318946,-5.98626964852478));
#97633=CARTESIAN_POINT('Ctrl Pts',(20.463734896018,17.9902512277851,-5.98779591518946));
#97634=CARTESIAN_POINT('Ctrl Pts',(20.4504678796014,17.9716661703838,-5.98927998968137));
#97635=CARTESIAN_POINT('Ctrl Pts',(20.4097693768218,17.9165611363241,-5.99375469302987));
#97636=CARTESIAN_POINT('Ctrl Pts',(20.3814543577333,17.8807109619743,-5.9967659934363));
#97637=CARTESIAN_POINT('Ctrl Pts',(20.2814846348372,17.7622287298823,-6.00700641737681));
#97638=CARTESIAN_POINT('Ctrl Pts',(20.2045912957222,17.6842349245166,-6.01423699864965));
#97639=CARTESIAN_POINT('Ctrl Pts',(20.080434069921,17.576424703056,-6.02480598858788));
#97640=CARTESIAN_POINT('Ctrl Pts',(20.0374614790086,17.5419553336429,-6.02829278990761));
#97641=CARTESIAN_POINT('Ctrl Pts',(19.9656280397148,17.488804606175,-6.03384707504526));
#97642=CARTESIAN_POINT('Ctrl Pts',(19.9375730048731,17.4690824242569,-6.03595294098667));
#97643=CARTESIAN_POINT('Ctrl Pts',(19.9000608485796,17.4440512515222,-6.03868838078686));
#97644=CARTESIAN_POINT('Ctrl Pts',(19.8910258522233,17.4381218410713,-6.03934127274135));
#97645=CARTESIAN_POINT('Ctrl Pts',(19.8761502341641,17.4285215514451,-6.04040663591698));
#97646=CARTESIAN_POINT('Ctrl Pts',(19.8703364549321,17.4248096294325,-6.04082063582467));
#97647=CARTESIAN_POINT('Ctrl Pts',(19.8590454247469,17.4176780869468,-6.04162013573756));
#97648=CARTESIAN_POINT('Ctrl Pts',(19.8535704733016,17.4142549851697,-6.04200576191569));
#97649=CARTESIAN_POINT('Ctrl Pts',(19.8408898465981,17.4064071469845,-6.04289425009978));
#97650=CARTESIAN_POINT('Ctrl Pts',(19.8336731207864,17.4020004067881,-6.04339644571447));
#97651=CARTESIAN_POINT('Ctrl Pts',(19.8141869496983,17.3902612902263,-6.04474331443113));
#97652=CARTESIAN_POINT('Ctrl Pts',(19.8018691952349,17.3830096574772,-6.04558504433651));
#97653=CARTESIAN_POINT('Ctrl Pts',(19.6879717255663,17.3175008274633,-6.05328243071551));
#97654=CARTESIAN_POINT('Ctrl Pts',(19.5817897989261,17.2676372147659,-6.0598198657114));
#97655=CARTESIAN_POINT('Ctrl Pts',(19.3186488425677,17.1697625834431,-6.0751882390939));
#97656=CARTESIAN_POINT('Ctrl Pts',(19.1592049339455,17.1306988251208,-6.08383348734822));
#97657=CARTESIAN_POINT('Ctrl Pts',(18.965647465654,17.1064765451146,-6.09504684896966));
#97658=CARTESIAN_POINT('Ctrl Pts',(18.9343371089752,17.10326559435,-6.09688396807863));
#97659=CARTESIAN_POINT('Ctrl Pts',(18.895824122615,17.1001818348265,-6.09918477932821));
#97660=CARTESIAN_POINT('Ctrl Pts',(18.8886767441527,17.0996460565407,-6.09961350528181));
#97661=CARTESIAN_POINT('Ctrl Pts',(18.877443026798,17.0988613072369,-6.10029025902922));
#97662=CARTESIAN_POINT('Ctrl Pts',(18.8733583749534,17.0985878711574,-6.10053693595945));
#97663=CARTESIAN_POINT('Ctrl Pts',(18.8657059629365,17.0980978926574,-6.10100024967099));
#97664=CARTESIAN_POINT('Ctrl Pts',(18.8621384387727,17.0978785373947,-6.10121672700388));
#97665=CARTESIAN_POINT('Ctrl Pts',(18.8539725124614,17.0973971966867,-6.10171332906332));
#97666=CARTESIAN_POINT('Ctrl Pts',(18.8493738138443,17.097141183505,-6.10199378399335));
#97667=CARTESIAN_POINT('Ctrl Pts',(18.8351628252793,17.0963965577087,-6.10286281490277));
#97668=CARTESIAN_POINT('Ctrl Pts',(18.825548167811,17.0959584967884,-6.10345411067238));
#97669=CARTESIAN_POINT('Ctrl Pts',(18.7294013803014,17.0922346823894,-6.10939821466919));
#97670=CARTESIAN_POINT('Ctrl Pts',(18.642757057258,17.094196071647,-6.11500401293072));
#97671=CARTESIAN_POINT('Ctrl Pts',(18.4300124818302,17.1120979616639,-6.12902164966085));
#97672=CARTESIAN_POINT('Ctrl Pts',(18.3047409103902,17.1340940355241,-6.13748303995429));
#97673=CARTESIAN_POINT('Ctrl Pts',(18.0889892910458,17.1923444314256,-6.1519472826074));
#97674=CARTESIAN_POINT('Ctrl Pts',(17.9976065264711,17.2238567469128,-6.15804196483319));
#97675=CARTESIAN_POINT('Ctrl Pts',(17.8952172280175,17.2672031287852,-6.16482089800075));
#97676=CARTESIAN_POINT('Ctrl Pts',(17.8818109407093,17.2730431792278,-6.16570765742976));
#97677=CARTESIAN_POINT('Ctrl Pts',(17.8614116592003,17.2821821395861,-6.16705592614929));
#97678=CARTESIAN_POINT('Ctrl Pts',(17.854374640313,17.2853811435752,-6.16752083979656));
#97679=CARTESIAN_POINT('Ctrl Pts',(17.8415803469013,17.2912821545212,-6.16836582331309));
#97680=CARTESIAN_POINT('Ctrl Pts',(17.8358174497876,17.2939716873904,-6.16874631704546));
#97681=CARTESIAN_POINT('Ctrl Pts',(17.8233758159176,17.299846592923,-6.16956757408814));
#97682=CARTESIAN_POINT('Ctrl Pts',(17.8167014675494,17.3030411025095,-6.17000801513585));
#97683=CARTESIAN_POINT('Ctrl Pts',(17.7985847191415,17.3118292690789,-6.1712032885805));
#97684=CARTESIAN_POINT('Ctrl Pts',(17.7871757129363,17.317491353878,-6.17195573327384));
#97685=CARTESIAN_POINT('Ctrl Pts',(17.7311353669005,17.3459363325564,-6.1756512359713));
#97686=CARTESIAN_POINT('Ctrl Pts',(17.6872695017149,17.3701969683445,-6.17854192764237));
#97687=CARTESIAN_POINT('Ctrl Pts',(17.495479817139,17.4853439641728,-6.19124129427989));
#97688=CARTESIAN_POINT('Ctrl Pts',(17.3582178149021,17.5926538521584,-6.20043477883872));
#97689=CARTESIAN_POINT('Ctrl Pts',(17.1912971852306,17.7599007014551,-6.21342102395247));
#97690=CARTESIAN_POINT('Ctrl Pts',(17.1489970496455,17.8062275459842,-6.21691351441275));
#97691=CARTESIAN_POINT('Ctrl Pts',(17.0889997154134,17.8781010873936,-6.2222987706409));
#97692=CARTESIAN_POINT('Ctrl Pts',(17.069704840534,17.9022728158016,-6.22410479523322));
#97693=CARTESIAN_POINT('Ctrl Pts',(17.0466234996822,17.9325242042836,-6.22637096767601));
#97694=CARTESIAN_POINT('Ctrl Pts',(17.0423282334413,17.9382131187843,-6.22679738284875));
#97695=CARTESIAN_POINT('Ctrl Pts',(17.0356167567508,17.9471961988009,-6.22747129638371));
#97696=CARTESIAN_POINT('Ctrl Pts',(17.0331811649679,17.9504759111282,-6.22771746265424));
#97697=CARTESIAN_POINT('Ctrl Pts',(17.0286315569541,17.9566395018317,-6.22818035429558));
#97698=CARTESIAN_POINT('Ctrl Pts',(17.0265153490006,17.9595216934266,-6.22839692345473));
#97699=CARTESIAN_POINT('Ctrl Pts',(17.0216819493963,17.96613967337,-6.22889445122355));
#97700=CARTESIAN_POINT('Ctrl Pts',(17.0189696844426,17.9698789925934,-6.22917574468107));
#97701=CARTESIAN_POINT('Ctrl Pts',(17.0106032963251,17.9814932751574,-6.23004991216945));
#97702=CARTESIAN_POINT('Ctrl Pts',(17.0049911059434,17.9893980923637,-6.23064555170152));
#97703=CARTESIAN_POINT('Ctrl Pts',(16.942141687169,18.079222742175,-6.23741892762844));
#97704=CARTESIAN_POINT('Ctrl Pts',(16.8907261962258,18.1650492762821,-6.2439318518382));
#97705=CARTESIAN_POINT('Ctrl Pts',(16.8076114310492,18.3290878318613,-6.25604811786295));
#97706=CARTESIAN_POINT('Ctrl Pts',(16.774176965914,18.4061320945035,-6.26161627532157));
#97707=CARTESIAN_POINT('Ctrl Pts',(16.7454195730112,18.484889205839,-6.26710634208694));
#97708=CARTESIAN_POINT('',(16.617000284924,19.2120983478179,-5.28730622481232));
#97709=CARTESIAN_POINT('Ctrl Pts',(16.7454194503114,18.4848895418737,-6.04247203357104));
#97710=CARTESIAN_POINT('Ctrl Pts',(16.7481387459572,18.4774422749056,-6.0419907093376));
#97711=CARTESIAN_POINT('Ctrl Pts',(16.750899896563,18.4700102295166,-6.04151078181624));
#97712=CARTESIAN_POINT('Ctrl Pts',(16.75653554949,18.4550981841722,-6.04054860862168));
#97713=CARTESIAN_POINT('Ctrl Pts',(16.7594108865832,18.4476186771125,-6.04006640307945));
#97714=CARTESIAN_POINT('Ctrl Pts',(16.7646516664199,18.4342137728658,-6.03920284167889));
#97715=CARTESIAN_POINT('Ctrl Pts',(16.7670015473001,18.4282824327406,-6.0388209688949));
#97716=CARTESIAN_POINT('Ctrl Pts',(16.772057849224,18.4156863902265,-6.03801046316236));
#97717=CARTESIAN_POINT('Ctrl Pts',(16.7747715031624,18.4090246637072,-6.03758207989412));
#97718=CARTESIAN_POINT('Ctrl Pts',(16.7821570484165,18.3911551801844,-6.0364336365191));
#97719=CARTESIAN_POINT('Ctrl Pts',(16.7868915427081,18.3799734655095,-6.03571570389965));
#97720=CARTESIAN_POINT('Ctrl Pts',(16.8108499540655,18.3247185221913,-6.03217069704112));
#97721=CARTESIAN_POINT('Ctrl Pts',(16.8314761708487,18.2812664059025,-6.02939191354512));
#97722=CARTESIAN_POINT('Ctrl Pts',(16.9305768783373,18.089634205546,-6.01711723884615));
#97723=CARTESIAN_POINT('Ctrl Pts',(17.0250011761165,17.9503966729864,-6.00819925148187));
#97724=CARTESIAN_POINT('Ctrl Pts',(17.1995518208954,17.7491852038798,-5.99361572799738));
#97725=CARTESIAN_POINT('Ctrl Pts',(17.2693672178715,17.6792430339765,-5.98812308154839));
#97726=CARTESIAN_POINT('Ctrl Pts',(17.3511068478608,17.608068459226,-5.98170194445832));
#97727=CARTESIAN_POINT('Ctrl Pts',(17.3584620215311,17.6017522700469,-5.98112420622296));
#97728=CARTESIAN_POINT('Ctrl Pts',(17.3693853989644,17.5925015196791,-5.98026582349408));
#97729=CARTESIAN_POINT('Ctrl Pts',(17.3729203611462,17.5895276579816,-5.97998798233413));
#97730=CARTESIAN_POINT('Ctrl Pts',(17.3792087466636,17.5842724734305,-5.97949356993484));
#97731=CARTESIAN_POINT('Ctrl Pts',(17.3819582460405,17.5819865313151,-5.97927734067681));
#97732=CARTESIAN_POINT('Ctrl Pts',(17.3878614400866,17.5771038387136,-5.97881295987964));
#97733=CARTESIAN_POINT('Ctrl Pts',(17.3910168158717,17.5745092866599,-5.97856466208833));
#97734=CARTESIAN_POINT('Ctrl Pts',(17.3996985526611,17.5674126255078,-5.97788132970049));
#97735=CARTESIAN_POINT('Ctrl Pts',(17.4052401142961,17.5629293180289,-5.97744497757514));
#97736=CARTESIAN_POINT('Ctrl Pts',(17.4349421976595,17.5391465285037,-5.97510571392364));
#97737=CARTESIAN_POINT('Ctrl Pts',(17.4594994156479,17.520351239543,-5.97317002985472));
#97738=CARTESIAN_POINT('Ctrl Pts',(17.5350662199068,17.4650969832626,-5.96723066083318));
#97739=CARTESIAN_POINT('Ctrl Pts',(17.5872900516001,17.4303611403505,-5.96314954571131));
#97740=CARTESIAN_POINT('Ctrl Pts',(17.7561737873169,17.3285443011583,-5.95019052796835));
#97741=CARTESIAN_POINT('Ctrl Pts',(17.8777423238762,17.2702239827259,-5.94122487589165));
#97742=CARTESIAN_POINT('Ctrl Pts',(18.0423575416279,17.2097535817557,-5.92993142637269));
#97743=CARTESIAN_POINT('Ctrl Pts',(18.0810894552583,17.1967843569459,-5.92732948001112));
#97744=CARTESIAN_POINT('Ctrl Pts',(18.1665837488862,17.1708825180933,-5.92171050301941));
#97745=CARTESIAN_POINT('Ctrl Pts',(18.2134653624909,17.1584199558639,-5.91870889039176));
#97746=CARTESIAN_POINT('Ctrl Pts',(18.2730119751691,17.1447624420808,-5.91499302062857));
#97747=CARTESIAN_POINT('Ctrl Pts',(18.285312165364,17.1420565878713,-5.91423055232542));
#97748=CARTESIAN_POINT('Ctrl Pts',(18.3048443022585,17.1379421974862,-5.9130276817962));
#97749=CARTESIAN_POINT('Ctrl Pts',(18.3120605692159,17.1364614044675,-5.91258497417978));
#97750=CARTESIAN_POINT('Ctrl Pts',(18.3255226960721,17.1337720971466,-5.91176220923687));
#97751=CARTESIAN_POINT('Ctrl Pts',(18.3317665392016,17.1325540149916,-5.91138185021932));
#97752=CARTESIAN_POINT('Ctrl Pts',(18.3456487636471,17.1299106960005,-5.91053890480252));
#97753=CARTESIAN_POINT('Ctrl Pts',(18.3532897163211,17.1284993262035,-5.91007676503983));
#97754=CARTESIAN_POINT('Ctrl Pts',(18.3755207663398,17.1245194462317,-5.90873738689269));
#97755=CARTESIAN_POINT('Ctrl Pts',(18.3901304558915,17.1220619407117,-5.90786367991764));
#97756=CARTESIAN_POINT('Ctrl Pts',(18.5067614704049,17.1037001210185,-5.90093807258743));
#97757=CARTESIAN_POINT('Ctrl Pts',(18.6098026989704,17.095124488636,-5.89512919840169));
#97758=CARTESIAN_POINT('Ctrl Pts',(18.8727052488065,17.0925251235231,-5.88065401520009));
#97759=CARTESIAN_POINT('Ctrl Pts',(19.0319913542557,17.1090085141082,-5.87222578061524));
#97760=CARTESIAN_POINT('Ctrl Pts',(19.2353088264538,17.1536389295898,-5.86047071503921));
#97761=CARTESIAN_POINT('Ctrl Pts',(19.2823439802619,17.165672836828,-5.8576758031864));
#97762=CARTESIAN_POINT('Ctrl Pts',(19.3363658020341,17.1814915286654,-5.8543339314129));
#97763=CARTESIAN_POINT('Ctrl Pts',(19.3437994995484,17.1837127088499,-5.85387113669538));
#97764=CARTESIAN_POINT('Ctrl Pts',(19.3556664474398,17.187329713356,-5.85312739536322));
#97765=CARTESIAN_POINT('Ctrl Pts',(19.3601076814325,17.1886993865335,-5.85284793585835));
#97766=CARTESIAN_POINT('Ctrl Pts',(19.3679697945519,17.1911524374952,-5.85235118897157));
#97767=CARTESIAN_POINT('Ctrl Pts',(19.3713924719027,17.1922299009648,-5.85213425011283));
#97768=CARTESIAN_POINT('Ctrl Pts',(19.3786459951136,17.1945336056696,-5.85167302430903));
#97769=CARTESIAN_POINT('Ctrl Pts',(19.3824760305682,17.1957620449101,-5.85142861507782));
#97770=CARTESIAN_POINT('Ctrl Pts',(19.3928137013193,17.1991102540189,-5.85076661869547));
#97771=CARTESIAN_POINT('Ctrl Pts',(19.3993145303316,17.2012506584647,-5.85034784518591));
#97772=CARTESIAN_POINT('Ctrl Pts',(19.431653329498,17.2120723375531,-5.84825266677946));
#97773=CARTESIAN_POINT('Ctrl Pts',(19.457331041608,17.2212201104345,-5.84655092681761));
#97774=CARTESIAN_POINT('Ctrl Pts',(19.5312425868864,17.249171022534,-5.84155577196845));
#97775=CARTESIAN_POINT('Ctrl Pts',(19.5789706385791,17.2692501247554,-5.83820915534393));
#97776=CARTESIAN_POINT('Ctrl Pts',(19.7513078878802,17.3493095465325,-5.82578780410558));
#97777=CARTESIAN_POINT('Ctrl Pts',(19.870706575776,17.4197130606724,-5.81654184700792));
#97778=CARTESIAN_POINT('Ctrl Pts',(20.0148091271497,17.5249309954341,-5.80498856794566));
#97779=CARTESIAN_POINT('Ctrl Pts',(20.0465534845629,17.5495234445017,-5.80241358872893));
#97780=CARTESIAN_POINT('Ctrl Pts',(20.1232167681151,17.6124840916443,-5.79612663753694));
#97781=CARTESIAN_POINT('Ctrl Pts',(20.1672677610612,17.6518589082214,-5.79245355201825));
#97782=CARTESIAN_POINT('Ctrl Pts',(20.2183872880876,17.7015521064076,-5.78811254465629));
#97783=CARTESIAN_POINT('Ctrl Pts',(20.2270825420895,17.7101525404416,-5.78737120593893));
#97784=CARTESIAN_POINT('Ctrl Pts',(20.2412898268673,17.7244505710342,-5.7861548676292));
#97785=CARTESIAN_POINT('Ctrl Pts',(20.246845164355,17.7301045484943,-5.78567795439805));
#97786=CARTESIAN_POINT('Ctrl Pts',(20.2568089909155,17.7403598738999,-5.78482016717834));
#97787=CARTESIAN_POINT('Ctrl Pts',(20.2612286863542,17.7449501562836,-5.78443880469588));
#97788=CARTESIAN_POINT('Ctrl Pts',(20.2706328865916,17.7548060083681,-5.78362543565624));
#97789=CARTESIAN_POINT('Ctrl Pts',(20.275611211643,17.760077381952,-5.78319369936979));
#97790=CARTESIAN_POINT('Ctrl Pts',(20.2890312644421,17.7744344515728,-5.78202662437894));
#97791=CARTESIAN_POINT('Ctrl Pts',(20.2974204768281,17.7835690101393,-5.78129353597302));
#97792=CARTESIAN_POINT('Ctrl Pts',(20.340155954464,17.8309301009973,-5.7775399555737));
#97793=CARTESIAN_POINT('Ctrl Pts',(20.3731839859538,17.8703261531367,-5.77457504135118));
#97794=CARTESIAN_POINT('Ctrl Pts',(20.5101843382777,18.0463824950438,-5.76191407953999));
#97795=CARTESIAN_POINT('Ctrl Pts',(20.5987432446707,18.1941924898872,-5.75281366859313));
#97796=CARTESIAN_POINT('Ctrl Pts',(20.7054257676578,18.4341850744421,-5.7383892691483));
#97797=CARTESIAN_POINT('Ctrl Pts',(20.7369711235795,18.5195786335076,-5.73330266197395));
#97798=CARTESIAN_POINT('Ctrl Pts',(20.7656831956612,18.6159825792187,-5.7273429922418));
#97799=CARTESIAN_POINT('Ctrl Pts',(20.7683774113313,18.6252604001434,-5.72676724776813));
#97800=CARTESIAN_POINT('Ctrl Pts',(20.7722640454593,18.6389947899297,-5.72591127197865));
#97801=CARTESIAN_POINT('Ctrl Pts',(20.7735055953079,18.6434374878978,-5.72563382137693));
#97802=CARTESIAN_POINT('Ctrl Pts',(20.7756835520062,18.6513304060546,-5.72513983980062));
#97803=CARTESIAN_POINT('Ctrl Pts',(20.7766257500082,18.6547789772849,-5.72492364859528));
#97804=CARTESIAN_POINT('Ctrl Pts',(20.7786269781943,18.6621774035352,-5.72445905031546));
#97805=CARTESIAN_POINT('Ctrl Pts',(20.7796832846299,18.6661278859382,-5.72421049542671));
#97806=CARTESIAN_POINT('Ctrl Pts',(20.7825542626137,18.6769910934836,-5.72352574716372));
#97807=CARTESIAN_POINT('Ctrl Pts',(20.7843453647729,18.6839099119624,-5.7230882273483));
#97808=CARTESIAN_POINT('Ctrl Pts',(20.7937636187623,18.7210660196281,-5.72073160698858));
#97809=CARTESIAN_POINT('Ctrl Pts',(20.8007565531057,18.7514582917134,-5.71877916700626));
#97810=CARTESIAN_POINT('Ctrl Pts',(20.8402826141576,18.9424582106662,-5.70640108722148));
#97811=CARTESIAN_POINT('Ctrl Pts',(20.8547462483627,19.106232430254,-5.69536328678664));
#97812=CARTESIAN_POINT('Ctrl Pts',(20.8469094631331,19.3871548150377,-5.67700409845332));
#97813=CARTESIAN_POINT('Ctrl Pts',(20.8339245839354,19.5038165535752,-5.66953962372299));
#97814=CARTESIAN_POINT('Ctrl Pts',(20.8085934887767,19.6328473343383,-5.66151057450884));
#97815=CARTESIAN_POINT('Ctrl Pts',(20.8056978483035,19.6468455669499,-5.66064231466571));
#97816=CARTESIAN_POINT('Ctrl Pts',(20.8008639227089,19.6690764416345,-5.65926764311523));
#97817=CARTESIAN_POINT('Ctrl Pts',(20.7990177406086,19.6773284631985,-5.65875830093279));
#97818=CARTESIAN_POINT('Ctrl Pts',(20.7956746885879,19.6918619037429,-5.65786282793587));
#97819=CARTESIAN_POINT('Ctrl Pts',(20.7941984389958,19.6981479091894,-5.65747604055645));
#97820=CARTESIAN_POINT('Ctrl Pts',(20.7910857781054,19.7111346590859,-5.6566779899948));
#97821=CARTESIAN_POINT('Ctrl Pts',(20.7894453299547,19.7178343644634,-5.65626686196399));
#97822=CARTESIAN_POINT('Ctrl Pts',(20.7851508707941,19.735009426156,-5.65521432959913));
#97823=CARTESIAN_POINT('Ctrl Pts',(20.7824493233422,19.7454727773353,-5.65457446554711));
#97824=CARTESIAN_POINT('Ctrl Pts',(20.7708431511412,19.789043547507,-5.6519152064258));
#97825=CARTESIAN_POINT('Ctrl Pts',(20.7612147880594,19.8219539790205,-5.64991930836331));
#97826=CARTESIAN_POINT('Ctrl Pts',(20.7340521654916,19.9070687127684,-5.64477911447693));
#97827=CARTESIAN_POINT('Ctrl Pts',(20.7152728911656,19.958849378079,-5.64167412969972));
#97828=CARTESIAN_POINT('Ctrl Pts',(20.653248441427,20.1110680065081,-5.63253421050392));
#97829=CARTESIAN_POINT('Ctrl Pts',(20.6042227374268,20.2089502977855,-5.62664802033573));
#97830=CARTESIAN_POINT('Ctrl Pts',(20.5264181760491,20.3382332752665,-5.61843315478145));
#97831=CARTESIAN_POINT('Ctrl Pts',(20.5039342831632,20.3732178105307,-5.61616062172462));
#97832=CARTESIAN_POINT('Ctrl Pts',(20.4369304437737,20.4710166000365,-5.60960323066978));
#97833=CARTESIAN_POINT('Ctrl Pts',(20.3899992829037,20.5320895511261,-5.60525798762717));
#97834=CARTESIAN_POINT('Ctrl Pts',(20.3336585315451,20.5976765936093,-5.60013372390642));
#97835=CARTESIAN_POINT('Ctrl Pts',(20.3274149299025,20.6048465648511,-5.59956702044052));
#97836=CARTESIAN_POINT('Ctrl Pts',(20.3180905126134,20.6154099298794,-5.59872196749233));
#97837=CARTESIAN_POINT('Ctrl Pts',(20.3150465321186,20.6188358802308,-5.59844629724577));
#97838=CARTESIAN_POINT('Ctrl Pts',(20.3096102484778,20.6249144615225,-5.59795427094486));
#97839=CARTESIAN_POINT('Ctrl Pts',(20.3072223324559,20.6275709484679,-5.59773824457235));
#97840=CARTESIAN_POINT('Ctrl Pts',(20.3020731900988,20.6332701404373,-5.59727261555843));
#97841=CARTESIAN_POINT('Ctrl Pts',(20.2993098662797,20.6363108095255,-5.59702285782825));
#97842=CARTESIAN_POINT('Ctrl Pts',(20.2916560429199,20.6446837175715,-5.59633147546365));
#97843=CARTESIAN_POINT('Ctrl Pts',(20.2867470854828,20.6499989003185,-5.59588848227961));
#97844=CARTESIAN_POINT('Ctrl Pts',(20.2596754155538,20.679010987308,-5.59344841529768));
#97845=CARTESIAN_POINT('Ctrl Pts',(20.2369986983407,20.7022197618821,-5.59141520590624));
#97846=CARTESIAN_POINT('Ctrl Pts',(20.0973928107142,20.8386812953483,-5.5790111528113));
#97847=CARTESIAN_POINT('Ctrl Pts',(19.968255172241,20.9386575017609,-5.56804893308317));
#97848=CARTESIAN_POINT('Ctrl Pts',(19.728948641116,21.0832755103828,-5.54978480276311));
#97849=CARTESIAN_POINT('Ctrl Pts',(19.6241156750034,21.1353285270644,-5.54234267676032));
#97850=CARTESIAN_POINT('Ctrl Pts',(19.5022235686276,21.1837457544456,-5.53433426640732));
#97851=CARTESIAN_POINT('Ctrl Pts',(19.4888876628176,21.1888872301853,-5.53346612303993));
#97852=CARTESIAN_POINT('Ctrl Pts',(19.4675807721743,21.1968549148413,-5.53209160046514));
#97853=CARTESIAN_POINT('Ctrl Pts',(19.459643334353,21.19976902798,-5.53158229177042));
#97854=CARTESIAN_POINT('Ctrl Pts',(19.4456140739619,21.2048244909252,-5.53068685772781));
#97855=CARTESIAN_POINT('Ctrl Pts',(19.4395295542947,21.206985656342,-5.53030007599484));
#97856=CARTESIAN_POINT('Ctrl Pts',(19.4269247980111,21.2113979111854,-5.52950201801098));
#97857=CARTESIAN_POINT('Ctrl Pts',(19.4204032490313,21.2136450409956,-5.52909087700565));
#97858=CARTESIAN_POINT('Ctrl Pts',(19.4036360509998,21.2193309873075,-5.52803827195416));
#97859=CARTESIAN_POINT('Ctrl Pts',(19.393374761598,21.2227233223537,-5.52739834860778));
#97860=CARTESIAN_POINT('Ctrl Pts',(19.3504470337057,21.2365512891226,-5.52473851341847));
#97861=CARTESIAN_POINT('Ctrl Pts',(19.3175543633144,21.2462713508712,-5.52274211157902));
#97862=CARTESIAN_POINT('Ctrl Pts',(19.2312560196539,21.2695089060162,-5.51760032715994));
#97863=CARTESIAN_POINT('Ctrl Pts',(19.1775324155649,21.2817491654307,-5.51449428753932));
#97864=CARTESIAN_POINT('Ctrl Pts',(19.0159315959175,21.3119890790746,-5.50535252786758));
#97865=CARTESIAN_POINT('Ctrl Pts',(18.9070745915923,21.3237438574571,-5.49946554599749));
#97866=CARTESIAN_POINT('Ctrl Pts',(18.7544583728296,21.3283451322055,-5.4911528179407));
#97867=CARTESIAN_POINT('Ctrl Pts',(18.7110908096744,21.3283199868743,-5.48878260171933));
#97868=CARTESIAN_POINT('Ctrl Pts',(18.6387100488214,21.3260539736983,-5.48477284606716));
#97869=CARTESIAN_POINT('Ctrl Pts',(18.6096869456578,21.3245466974369,-5.48315047434824));
#97870=CARTESIAN_POINT('Ctrl Pts',(18.5332573432183,21.3189977555048,-5.47881926008128));
#97871=CARTESIAN_POINT('Ctrl Pts',(18.4859430695756,21.3139548650726,-5.47607812533323));
#97872=CARTESIAN_POINT('Ctrl Pts',(18.4312003475133,21.3062472256842,-5.4727957736598));
#97873=CARTESIAN_POINT('Ctrl Pts',(18.4235638822542,21.3051294083639,-5.47233536967439));
#97874=CARTESIAN_POINT('Ctrl Pts',(18.4113506801935,21.3032733824279,-5.47159474472915));
#97875=CARTESIAN_POINT('Ctrl Pts',(18.4067698783917,21.3025618415347,-5.47131599126218));
#97876=CARTESIAN_POINT('Ctrl Pts',(18.3986490664127,21.3012730960857,-5.47082004350714));
#97877=CARTESIAN_POINT('Ctrl Pts',(18.3951081433952,21.3007019343047,-5.4706031938287));
#97878=CARTESIAN_POINT('Ctrl Pts',(18.3875926898239,21.2994700640224,-5.47014164207863));
#97879=CARTESIAN_POINT('Ctrl Pts',(18.3836186510041,21.2988070175452,-5.46989681511304));
#97880=CARTESIAN_POINT('Ctrl Pts',(18.3728689604189,21.2969819348036,-5.46923253297554));
#97881=CARTESIAN_POINT('Ctrl Pts',(18.3660971053576,21.295798243762,-5.46881187767169));
#97882=CARTESIAN_POINT('Ctrl Pts',(18.3321408619236,21.2896922465556,-5.46669201364089));
#97883=CARTESIAN_POINT('Ctrl Pts',(18.3050502688105,21.2842713718476,-5.46496676294433));
#97884=CARTESIAN_POINT('Ctrl Pts',(18.2265010432086,21.2669482138806,-5.45988011483574));
#97885=CARTESIAN_POINT('Ctrl Pts',(18.1753740442127,21.2536489017205,-5.45646335510192));
#97886=CARTESIAN_POINT('Ctrl Pts',(17.9780722831651,21.1943647012517,-5.44298866395169));
#97887=CARTESIAN_POINT('Ctrl Pts',(17.8365445792823,21.134471771628,-5.4327334595869));
#97888=CARTESIAN_POINT('Ctrl Pts',(17.6322552498939,21.0205186968665,-5.41770817525264));
#97889=CARTESIAN_POINT('Ctrl Pts',(17.5640878427914,20.9772127971188,-5.41264265204407));
#97890=CARTESIAN_POINT('Ctrl Pts',(17.4877036590849,20.9223190532456,-5.40690620733465));
#97891=CARTESIAN_POINT('Ctrl Pts',(17.4769290416364,20.9144201154912,-5.4060954528015));
#97892=CARTESIAN_POINT('Ctrl Pts',(17.4596772741709,20.9015198998366,-5.40479455543923));
#97893=CARTESIAN_POINT('Ctrl Pts',(17.4531532173695,20.8965822328406,-5.40430195153289));
#97894=CARTESIAN_POINT('Ctrl Pts',(17.441718210477,20.8878230359064,-5.40343733933386));
#97895=CARTESIAN_POINT('Ctrl Pts',(17.4367952091402,20.8840174682685,-5.40306470919026));
#97896=CARTESIAN_POINT('Ctrl Pts',(17.4265682941923,20.8760396008408,-5.40228975137037));
#97897=CARTESIAN_POINT('Ctrl Pts',(17.4212674012888,20.8718635294994,-5.40188757923018));
#97898=CARTESIAN_POINT('Ctrl Pts',(17.4076769412024,20.8610511803134,-5.40085516116281));
#97899=CARTESIAN_POINT('Ctrl Pts',(17.3994171083664,20.8543777002046,-5.40022641091924));
#97900=CARTESIAN_POINT('Ctrl Pts',(17.3815475914323,20.8397165552935,-5.3988631276667));
#97901=CARTESIAN_POINT('Ctrl Pts',(17.3719576744701,20.8317053551647,-5.39812956455156));
#97902=CARTESIAN_POINT('Ctrl Pts',(17.3443504457775,20.8082247831513,-5.39601157332466));
#97903=CARTESIAN_POINT('Ctrl Pts',(17.3265214507323,20.7925363064579,-5.39463596498888));
#97904=CARTESIAN_POINT('Ctrl Pts',(17.2657170197186,20.7371891588786,-5.38991166384915));
#97905=CARTESIAN_POINT('Ctrl Pts',(17.2241217530004,20.6960510723948,-5.38662221562829));
#97906=CARTESIAN_POINT('Ctrl Pts',(17.0705752943577,20.5310620699904,-5.37412313596597));
#97907=CARTESIAN_POINT('Ctrl Pts',(16.9717272268921,20.3958769292234,-5.36533455581101));
#97908=CARTESIAN_POINT('Ctrl Pts',(16.8619590343551,20.2011327200551,-5.35279638020422));
#97909=CARTESIAN_POINT('Ctrl Pts',(16.8361298907681,20.1506744272087,-5.3495523903727));
#97910=CARTESIAN_POINT('Ctrl Pts',(16.8086457512731,20.0912149151449,-5.34566616102009));
#97911=CARTESIAN_POINT('Ctrl Pts',(16.8049839540475,20.083160746777,-5.34513842711246));
#97912=CARTESIAN_POINT('Ctrl Pts',(16.7995317710099,20.0709662878449,-5.34433707457302));
#97913=CARTESIAN_POINT('Ctrl Pts',(16.7977039031392,20.0668427248148,-5.34406569607154));
#97914=CARTESIAN_POINT('Ctrl Pts',(16.7944546135634,20.0594488255301,-5.34357832025268));
#97915=CARTESIAN_POINT('Ctrl Pts',(16.7930282644025,20.0561807125852,-5.34336262825377));
#97916=CARTESIAN_POINT('Ctrl Pts',(16.7899560464386,20.0490927195048,-5.34289422821695));
#97917=CARTESIAN_POINT('Ctrl Pts',(16.7883131984231,20.0452716400236,-5.34264134642966));
#97918=CARTESIAN_POINT('Ctrl Pts',(16.7837528404042,20.0345780232952,-5.34193265037776));
#97919=CARTESIAN_POINT('Ctrl Pts',(16.7808604447694,20.0276949356661,-5.34147535494318));
#97920=CARTESIAN_POINT('Ctrl Pts',(16.764222646662,19.9875077471839,-5.3387994386588));
#97921=CARTESIAN_POINT('Ctrl Pts',(16.7512937136483,19.9538745029651,-5.33653614540452));
#97922=CARTESIAN_POINT('Ctrl Pts',(16.7123940719146,19.8444196762135,-5.32913131005087));
#97923=CARTESIAN_POINT('Ctrl Pts',(16.6898690219549,19.7674511146764,-5.32386679432088));
#97924=CARTESIAN_POINT('Ctrl Pts',(16.6354601235266,19.5329093389116,-5.30797072274112));
#97925=CARTESIAN_POINT('Ctrl Pts',(16.6170836488932,19.3727774115619,-5.2973580198773));
#97926=CARTESIAN_POINT('Ctrl Pts',(16.617000284924,19.2120983478179,-5.28730622481232));
#97927=CARTESIAN_POINT('Ctrl Pts',(16.6170002837517,19.2120960860112,-5.28730608331776));
#97928=CARTESIAN_POINT('Ctrl Pts',(16.6169868618999,19.1861728863881,-5.28568437508849));
#97929=CARTESIAN_POINT('Ctrl Pts',(16.6174495936717,19.160250559852,-5.28407668349347));
#97930=CARTESIAN_POINT('Ctrl Pts',(16.619026332341,19.1167355687962,-5.28140090887606));
#97931=CARTESIAN_POINT('Ctrl Pts',(16.6198840725551,19.0991372597741,-5.28032509221211));
#97932=CARTESIAN_POINT('Ctrl Pts',(16.6214584305574,19.0734384407885,-5.27876299621345));
#97933=CARTESIAN_POINT('Ctrl Pts',(16.6220021625087,19.0653284430094,-5.27827133051497));
#97934=CARTESIAN_POINT('Ctrl Pts',(16.62304733721,19.050977982414,-5.27740358656125));
#97935=CARTESIAN_POINT('Ctrl Pts',(16.6235297763263,19.0447362728896,-5.27702691609314));
#97936=CARTESIAN_POINT('Ctrl Pts',(16.6245388687024,19.0323936384307,-5.27628353155207));
#97937=CARTESIAN_POINT('Ctrl Pts',(16.6250643196937,19.0262926790796,-5.27591678345692));
#97938=CARTESIAN_POINT('Ctrl Pts',(16.6261638693465,19.0141427830512,-5.27518779097605));
#97939=CARTESIAN_POINT('Ctrl Pts',(16.6267375529903,19.0080938685996,-5.27482553722127));
#97940=CARTESIAN_POINT('Ctrl Pts',(16.6281714449769,18.9936373475952,-5.2739613605212));
#97941=CARTESIAN_POINT('Ctrl Pts',(16.6290559777756,18.9852322160711,-5.27346020631224));
#97942=CARTESIAN_POINT('Ctrl Pts',(16.6319011555824,18.9596681197253,-5.27193970990869));
#97943=CARTESIAN_POINT('Ctrl Pts',(16.634021488887,18.9425273855968,-5.27092538153886));
#97944=CARTESIAN_POINT('Ctrl Pts',(16.6419662052317,18.8841728758714,-5.26748807325364));
#97945=CARTESIAN_POINT('Ctrl Pts',(16.6487962821945,18.8431044315344,-5.26509633856523));
#97946=CARTESIAN_POINT('Ctrl Pts',(16.6780901108046,18.6942360310667,-5.25649241599256));
#97947=CARTESIAN_POINT('Ctrl Pts',(16.7077221576858,18.5881302047764,-5.25049678412355));
#97948=CARTESIAN_POINT('Ctrl Pts',(16.745419381199,18.4848897311503,-5.24452701096005));
#97949=CARTESIAN_POINT('Origin',(18.734,19.211,0.));
#97950=CARTESIAN_POINT('',(16.7454194484637,18.4848895469342,-4.44630497835508));
#97951=CARTESIAN_POINT('',(16.7454194645813,18.4848895027932,-4.66702131702538));
#97952=CARTESIAN_POINT('',(16.7454194503191,18.4848895418526,0.));
#97953=CARTESIAN_POINT('Ctrl Pts',(16.7454194645813,18.4848895027932,-4.66702131702538));
#97954=CARTESIAN_POINT('Ctrl Pts',(16.6988234574177,18.6125008143362,-4.67446195852453));
#97955=CARTESIAN_POINT('Ctrl Pts',(16.66461025224,18.744325088795,-4.68169548026336));
#97956=CARTESIAN_POINT('Ctrl Pts',(16.6370543938698,18.9176173124031,-4.69152882229505));
#97957=CARTESIAN_POINT('Ctrl Pts',(16.6319381925939,18.9568542403389,-4.69377779250457));
#97958=CARTESIAN_POINT('Ctrl Pts',(16.6263939805864,19.0112165310485,-4.69695244130703));
#97959=CARTESIAN_POINT('Ctrl Pts',(16.6250239202028,19.0262395182405,-4.69783592543835));
#97960=CARTESIAN_POINT('Ctrl Pts',(16.6229323256568,19.0522443093919,-4.69937786513208));
#97961=CARTESIAN_POINT('Ctrl Pts',(16.6221356455648,19.0632196503181,-4.70003252474882));
#97962=CARTESIAN_POINT('Ctrl Pts',(16.6211102620339,19.0790544965181,-4.70098327938888));
#97963=CARTESIAN_POINT('Ctrl Pts',(16.6208126722696,19.0839095694667,-4.701275631674));
#97964=CARTESIAN_POINT('Ctrl Pts',(16.6203235174211,19.0923671963612,-4.70178645165111));
#97965=CARTESIAN_POINT('Ctrl Pts',(16.6201244222695,19.0959693221627,-4.70200449766765));
#97966=CARTESIAN_POINT('Ctrl Pts',(16.6197264096915,19.1035206041751,-4.70246264082655));
#97967=CARTESIAN_POINT('Ctrl Pts',(16.6195293494629,19.10746979848,-4.70270283607585));
#97968=CARTESIAN_POINT('Ctrl Pts',(16.6190357978279,19.1179506865753,-4.70334183187577));
#97969=CARTESIAN_POINT('Ctrl Pts',(16.6187585034882,19.1244831805591,-4.70374168383773));
#97970=CARTESIAN_POINT('Ctrl Pts',(16.6177066684856,19.1523033179473,-4.70545097380983));
#97971=CARTESIAN_POINT('Ctrl Pts',(16.6172232245839,19.1735998901574,-4.70677546541417));
#97972=CARTESIAN_POINT('Ctrl Pts',(16.6170218767773,19.200073104592,-4.70843882601727));
#97973=CARTESIAN_POINT('Ctrl Pts',(16.6170014935553,19.2052471239773,-4.70876472284575));
#97974=CARTESIAN_POINT('Ctrl Pts',(16.6169868171449,19.2589278692597,-4.71215391036776));
#97975=CARTESIAN_POINT('Ctrl Pts',(16.6186407108918,19.3074176155505,-4.71528275379712));
#97976=CARTESIAN_POINT('Ctrl Pts',(16.6353861331744,19.5516577913175,-4.73125346316285));
#97977=CARTESIAN_POINT('Ctrl Pts',(16.6759975066366,19.7447399354121,-4.74444610218463));
#97978=CARTESIAN_POINT('Ctrl Pts',(16.7587957145083,19.9742314962044,-4.75978159654064));
#97979=CARTESIAN_POINT('Ctrl Pts',(16.7764544915404,20.0184468654001,-4.76272638402557));
#97980=CARTESIAN_POINT('Ctrl Pts',(16.8006203653444,20.0734898657946,-4.7663823368788));
#97981=CARTESIAN_POINT('Ctrl Pts',(16.8057522324957,20.0849028195151,-4.76713986251815));
#97982=CARTESIAN_POINT('Ctrl Pts',(16.8140577645003,20.1029443951343,-4.76833669134979));
#97983=CARTESIAN_POINT('Ctrl Pts',(16.8171652094914,20.1096030156214,-4.76877826123794));
#97984=CARTESIAN_POINT('Ctrl Pts',(16.823028055914,20.1219970985968,-4.76959995815116));
#97985=CARTESIAN_POINT('Ctrl Pts',(16.8257747608685,20.1277365613108,-4.76998038042889));
#97986=CARTESIAN_POINT('Ctrl Pts',(16.8319433128508,20.1404784015904,-4.77082477432642));
#97987=CARTESIAN_POINT('Ctrl Pts',(16.8353780471961,20.1474744646648,-4.77128829154419));
#97988=CARTESIAN_POINT('Ctrl Pts',(16.8455036889344,20.1678142453384,-4.77263567946622));
#97989=CARTESIAN_POINT('Ctrl Pts',(16.8522972737284,20.1811065322949,-4.77351595259198));
#97990=CARTESIAN_POINT('Ctrl Pts',(16.9092402101685,20.289671584962,-4.78070597854901));
#97991=CARTESIAN_POINT('Ctrl Pts',(16.9664529731369,20.3810694934547,-4.78674993048902));
#97992=CARTESIAN_POINT('Ctrl Pts',(17.1097563341115,20.5753316980448,-4.80001601635743));
#97993=CARTESIAN_POINT('Ctrl Pts',(17.1991453836981,20.6751676246587,-4.80713510492787));
#97994=CARTESIAN_POINT('Ctrl Pts',(17.3094007822207,20.7770381047402,-4.81548127362692));
#97995=CARTESIAN_POINT('Ctrl Pts',(17.3215822631169,20.7880334155392,-4.81639837091414));
#97996=CARTESIAN_POINT('Ctrl Pts',(17.373692197529,20.8339810742921,-4.8203064141723));
#97997=CARTESIAN_POINT('Ctrl Pts',(17.4147963007586,20.8675643603935,-4.82335196781879));
#97998=CARTESIAN_POINT('Ctrl Pts',(17.4640569638761,20.904815056129,-4.82701707430932));
#97999=CARTESIAN_POINT('Ctrl Pts',(17.4710316282704,20.910021967337,-4.82753635032579));
#98000=CARTESIAN_POINT('Ctrl Pts',(17.481644252569,20.9178433290356,-4.8283273311095));
#98001=CARTESIAN_POINT('Ctrl Pts',(17.4852588266247,20.9204895580453,-4.82859688115313));
#98002=CARTESIAN_POINT('Ctrl Pts',(17.4917639171662,20.9252202935484,-4.82908230549878));
#98003=CARTESIAN_POINT('Ctrl Pts',(17.4946513198195,20.9273089899384,-4.82929788489472));
#98004=CARTESIAN_POINT('Ctrl Pts',(17.5009390504933,20.9318332832327,-4.82976760082909));
#98005=CARTESIAN_POINT('Ctrl Pts',(17.5043412822405,20.9342660650693,-4.83002191959921));
#98006=CARTESIAN_POINT('Ctrl Pts',(17.5139239269522,20.9410753531651,-4.83073862393211));
#98007=CARTESIAN_POINT('Ctrl Pts',(17.5201205743176,20.9454287496401,-4.8312025441027));
#98008=CARTESIAN_POINT('Ctrl Pts',(17.5574253897987,20.9713390609635,-4.83399751539601));
#98009=CARTESIAN_POINT('Ctrl Pts',(17.5890816778356,20.9920904097943,-4.83637790462689));
#98010=CARTESIAN_POINT('Ctrl Pts',(17.6953709858567,21.0577606335277,-4.84435490029763));
#98011=CARTESIAN_POINT('Ctrl Pts',(17.7722173269281,21.0989214065626,-4.85009463079852));
#98012=CARTESIAN_POINT('Ctrl Pts',(18.0107243942808,21.2083222871105,-4.86743182627381));
#98013=CARTESIAN_POINT('Ctrl Pts',(18.1785701436342,21.2613524066277,-4.87894125133019));
#98014=CARTESIAN_POINT('Ctrl Pts',(18.3736794421063,21.2972375609875,-4.89115214668771));
#98015=CARTESIAN_POINT('Ctrl Pts',(18.3963683895905,21.3010294319637,-4.89255631343321));
#98016=CARTESIAN_POINT('Ctrl Pts',(18.4285569776615,21.3058710512096,-4.89452676420059));
#98017=CARTESIAN_POINT('Ctrl Pts',(18.4380082189428,21.3072273329269,-4.89510270707347));
#98018=CARTESIAN_POINT('Ctrl Pts',(18.4533806355021,21.3093272811114,-4.89603530195001));
#98019=CARTESIAN_POINT('Ctrl Pts',(18.4592962704175,21.3101099229136,-4.89639318218107));
#98020=CARTESIAN_POINT('Ctrl Pts',(18.4716866219836,21.3116958983636,-4.89714069867419));
#98021=CARTESIAN_POINT('Ctrl Pts',(18.4781619108412,21.312494334823,-4.89753017659066));
#98022=CARTESIAN_POINT('Ctrl Pts',(18.4935764075615,21.3143227198565,-4.89845457704296));
#98023=CARTESIAN_POINT('Ctrl Pts',(18.5025187409409,21.3153256397661,-4.89898864230417));
#98024=CARTESIAN_POINT('Ctrl Pts',(18.5326722001821,21.318512939129,-4.9007822924993));
#98025=CARTESIAN_POINT('Ctrl Pts',(18.5539102921976,21.3204339092809,-4.90203359417181));
#98026=CARTESIAN_POINT('Ctrl Pts',(18.6697208013014,21.3291470229912,-4.90879675696166));
#98027=CARTESIAN_POINT('Ctrl Pts',(18.7646440373952,21.3299012721082,-4.91411544545084));
#98028=CARTESIAN_POINT('Ctrl Pts',(19.0284622397008,21.3142581753223,-4.92865689622046));
#98029=CARTESIAN_POINT('Ctrl Pts',(19.1957807525193,21.2839568251217,-4.9375737220549));
#98030=CARTESIAN_POINT('Ctrl Pts',(19.3942231775491,21.2227794841407,-4.94941672400651));
#98031=CARTESIAN_POINT('Ctrl Pts',(19.4304520589743,21.2105263083619,-4.95163553070747));
#98032=CARTESIAN_POINT('Ctrl Pts',(19.4731095581262,21.1947989623043,-4.9543379330653));
#98033=CARTESIAN_POINT('Ctrl Pts',(19.4798795018202,21.1922634926047,-4.95476954671575));
#98034=CARTESIAN_POINT('Ctrl Pts',(19.4908786137344,21.188079757111,-4.95547544488958));
#98035=CARTESIAN_POINT('Ctrl Pts',(19.4951157652467,21.1864524527102,-4.95574850559991));
#98036=CARTESIAN_POINT('Ctrl Pts',(19.502674395544,21.1835215854793,-4.95623769310054));
#98037=CARTESIAN_POINT('Ctrl Pts',(19.5059978417334,21.1822232404395,-4.9564535050126));
#98038=CARTESIAN_POINT('Ctrl Pts',(19.5131693283762,21.1794006928996,-4.95692076825145));
#98039=CARTESIAN_POINT('Ctrl Pts',(19.5170161318849,21.1778736275167,-4.95717238581413));
#98040=CARTESIAN_POINT('Ctrl Pts',(19.5277027373964,21.1735950470494,-4.95787406001067));
#98041=CARTESIAN_POINT('Ctrl Pts',(19.5345326039404,21.1708190988973,-4.95832555166087));
#98042=CARTESIAN_POINT('Ctrl Pts',(19.5732605924124,21.1548421791802,-4.9609024645476));
#98043=CARTESIAN_POINT('Ctrl Pts',(19.6048445963251,21.1408989949771,-4.96306886047731));
#98044=CARTESIAN_POINT('Ctrl Pts',(19.7036377744781,21.0943665572877,-4.97002075292179));
#98045=CARTESIAN_POINT('Ctrl Pts',(19.7694682536341,21.0589910621757,-4.97491417818913));
#98046=CARTESIAN_POINT('Ctrl Pts',(19.9991769554074,20.9194189890758,-4.99264212121274));
#98047=CARTESIAN_POINT('Ctrl Pts',(20.1504570886518,20.7962599464977,-5.00546980764393));
#98048=CARTESIAN_POINT('Ctrl Pts',(20.2972438308747,20.6387269067766,-5.01869840151999));
#98049=CARTESIAN_POINT('Ctrl Pts',(20.31141526599,20.6230540090637,-5.01998660102361));
#98050=CARTESIAN_POINT('Ctrl Pts',(20.3308238122341,20.6009322278203,-5.02176706530472));
#98051=CARTESIAN_POINT('Ctrl Pts',(20.3362608343112,20.5946611243915,-5.02226766467881));
#98052=CARTESIAN_POINT('Ctrl Pts',(20.3455882459795,20.5837741120739,-5.02312969880941));
#98053=CARTESIAN_POINT('Ctrl Pts',(20.3494960018881,20.5791732735355,-5.02349184969312));
#98054=CARTESIAN_POINT('Ctrl Pts',(20.3575532343649,20.569604355026,-5.02424066262373));
#98055=CARTESIAN_POINT('Ctrl Pts',(20.3616997154676,20.564633826415,-5.02462719957479));
#98056=CARTESIAN_POINT('Ctrl Pts',(20.3713673559584,20.5529362412866,-5.02553124212869));
#98057=CARTESIAN_POINT('Ctrl Pts',(20.3768699878682,20.5461939710943,-5.02604799180047));
#98058=CARTESIAN_POINT('Ctrl Pts',(20.3946453041218,20.5241379567078,-5.02772461082035));
#98059=CARTESIAN_POINT('Ctrl Pts',(20.4067468875821,20.5086871764136,-5.02887762130791));
#98060=CARTESIAN_POINT('Ctrl Pts',(20.4678027198295,20.4284601815563,-5.03475909175496));
#98061=CARTESIAN_POINT('Ctrl Pts',(20.5132187216919,20.3610712973861,-5.03934822491166));
#98062=CARTESIAN_POINT('Ctrl Pts',(20.6406813700746,20.1462423227603,-5.05319189609479));
#98063=CARTESIAN_POINT('Ctrl Pts',(20.7090724430763,19.9915082600914,-5.0620626918143));
#98064=CARTESIAN_POINT('Ctrl Pts',(20.7741263764752,19.7788629866068,-5.07456389136168));
#98065=CARTESIAN_POINT('Ctrl Pts',(20.7878981153823,19.7268347526823,-5.07765029257518));
#98066=CARTESIAN_POINT('Ctrl Pts',(20.8015844539561,19.6658184894189,-5.08136102593395));
#98067=CARTESIAN_POINT('Ctrl Pts',(20.8034438411121,19.6572818785142,-5.08188223772846));
#98068=CARTESIAN_POINT('Ctrl Pts',(20.8061780396652,19.6443443242729,-5.0826755933476));
#98069=CARTESIAN_POINT('Ctrl Pts',(20.8070918134197,19.6399515866976,-5.08294556303785));
#98070=CARTESIAN_POINT('Ctrl Pts',(20.8087063952332,19.6320642198032,-5.08343143358339));
#98071=CARTESIAN_POINT('Ctrl Pts',(20.8094123481887,19.6285706985794,-5.08364703714067));
#98072=CARTESIAN_POINT('Ctrl Pts',(20.8109265117657,19.6209789179596,-5.08411644344029));
#98073=CARTESIAN_POINT('Ctrl Pts',(20.8117314055249,19.6168800983621,-5.08437042643753));
#98074=CARTESIAN_POINT('Ctrl Pts',(20.8139566794485,19.6053680830238,-5.08508525680834));
#98075=CARTESIAN_POINT('Ctrl Pts',(20.8153495340956,19.5979497205955,-5.08554762620798));
#98076=CARTESIAN_POINT('Ctrl Pts',(20.8234096700197,19.5537183734045,-5.08831411978127));
#98077=CARTESIAN_POINT('Ctrl Pts',(20.8291393770273,19.5167437584401,-5.09066644425214));
#98078=CARTESIAN_POINT('Ctrl Pts',(20.8447218636128,19.3949394702345,-5.0985036897849));
#98079=CARTESIAN_POINT('Ctrl Pts',(20.8504223412073,19.3096666831819,-5.10412669952517));
#98080=CARTESIAN_POINT('Ctrl Pts',(20.852074192631,19.0465236464045,-5.1215109985812));
#98081=CARTESIAN_POINT('Ctrl Pts',(20.8307946317997,18.8692875652443,-5.13319192669085));
#98082=CARTESIAN_POINT('Ctrl Pts',(20.7820564236979,18.6746472374158,-5.14554011528105));
#98083=CARTESIAN_POINT('Ctrl Pts',(20.776157785983,18.652608522954,-5.14693256727195));
#98084=CARTESIAN_POINT('Ctrl Pts',(20.7672950736057,18.6215165718268,-5.1488895816805));
#98085=CARTESIAN_POINT('Ctrl Pts',(20.7646245401782,18.6123819666164,-5.14946362526579));
#98086=CARTESIAN_POINT('Ctrl Pts',(20.7601810820551,18.5975550048967,-5.15039398496426));
#98087=CARTESIAN_POINT('Ctrl Pts',(20.7584455711271,18.5918516575419,-5.15075151766503));
#98088=CARTESIAN_POINT('Ctrl Pts',(20.7547588473058,18.5799173496861,-5.1514989748786));
#98089=CARTESIAN_POINT('Ctrl Pts',(20.7528028505029,18.5736879235679,-5.15188873811846));
#98090=CARTESIAN_POINT('Ctrl Pts',(20.7480744607896,18.5588692421862,-5.15281502934689));
#98091=CARTESIAN_POINT('Ctrl Pts',(20.7452758833745,18.5502884262482,-5.15335069059783));
#98092=CARTESIAN_POINT('Ctrl Pts',(20.7356303210785,18.5213430995984,-5.1551554123184));
#98093=CARTESIAN_POINT('Ctrl Pts',(20.7285280991241,18.5010645843888,-5.15641604732768));
#98094=CARTESIAN_POINT('Ctrl Pts',(20.6593418037715,18.3127605060513,-5.16809653375303));
#98095=CARTESIAN_POINT('Ctrl Pts',(20.5764785248977,18.1531459692136,-5.17772287233326));
#98096=CARTESIAN_POINT('Ctrl Pts',(20.40570003958,17.9065028038249,-5.19404858118146));
#98097=CARTESIAN_POINT('Ctrl Pts',(20.328531478131,17.8132322136214,-5.20067729948763));
#98098=CARTESIAN_POINT('Ctrl Pts',(20.2371952744552,17.720301187994,-5.2083999392276));
#98099=CARTESIAN_POINT('Ctrl Pts',(20.2305008150659,17.7135807920984,-5.2089653677263));
#98100=CARTESIAN_POINT('Ctrl Pts',(20.2205084800376,17.7036836751694,-5.20980887927629));
#98101=CARTESIAN_POINT('Ctrl Pts',(20.2172449913798,17.7004721919251,-5.21008429725847));
#98102=CARTESIAN_POINT('Ctrl Pts',(20.2114172864118,17.6947744499762,-5.21057604772473));
#98103=CARTESIAN_POINT('Ctrl Pts',(20.2088571714755,17.6922840686129,-5.21079205195714));
#98104=CARTESIAN_POINT('Ctrl Pts',(20.2033362946632,17.6869406972459,-5.21125783251008));
#98105=CARTESIAN_POINT('Ctrl Pts',(20.2003735633168,17.6840898922113,-5.21150776497149));
#98106=CARTESIAN_POINT('Ctrl Pts',(20.1921650037943,17.6762373610213,-5.21220011231284));
#98107=CARTESIAN_POINT('Ctrl Pts',(20.1869018216996,17.671253972469,-5.21264390191453));
#98108=CARTESIAN_POINT('Ctrl Pts',(20.1578012249538,17.6439824317191,-5.21509640628565));
#98109=CARTESIAN_POINT('Ctrl Pts',(20.1334778715711,17.6222220409873,-5.21714168342497));
#98110=CARTESIAN_POINT('Ctrl Pts',(19.9849903831066,17.4954366051412,-5.22954980491163));
#98111=CARTESIAN_POINT('Ctrl Pts',(19.8495662594593,17.4044434511716,-5.24050098099606));
#98112=CARTESIAN_POINT('Ctrl Pts',(19.6012509177667,17.2762614295174,-5.25875414881715));
#98113=CARTESIAN_POINT('Ctrl Pts',(19.493169104198,17.2313516544784,-5.26619577951411));
#98114=CARTESIAN_POINT('Ctrl Pts',(19.3683366318617,17.191220430012,-5.27420198193072));
#98115=CARTESIAN_POINT('Ctrl Pts',(19.3547126667837,17.1869920269941,-5.27506842393795));
#98116=CARTESIAN_POINT('Ctrl Pts',(19.3329541855649,17.1804793179396,-5.27644077026794));
#98117=CARTESIAN_POINT('Ctrl Pts',(19.3248471184224,17.1781055013691,-5.27694958966385));
#98118=CARTESIAN_POINT('Ctrl Pts',(19.3105198097889,17.1740032933581,-5.27784445474815));
#98119=CARTESIAN_POINT('Ctrl Pts',(19.3043055045365,17.1722547224147,-5.27823115419692));
#98120=CARTESIAN_POINT('Ctrl Pts',(19.2914317294757,17.1686957888675,-5.27902932161128));
#98121=CARTESIAN_POINT('Ctrl Pts',(19.2847712036161,17.1668895071848,-5.2794406529545));
#98122=CARTESIAN_POINT('Ctrl Pts',(19.2676433850478,17.1623343721844,-5.28049432387994));
#98123=CARTESIAN_POINT('Ctrl Pts',(19.2571635494368,17.1596331327328,-5.28113511663186));
#98124=CARTESIAN_POINT('Ctrl Pts',(19.2132658537066,17.1486765245523,-5.28380341199279));
#98125=CARTESIAN_POINT('Ctrl Pts',(19.1796687738439,17.1411561850023,-5.2858072132766));
#98126=CARTESIAN_POINT('Ctrl Pts',(19.0915961329795,17.1236861415526,-5.29097237850196));
#98127=CARTESIAN_POINT('Ctrl Pts',(19.036886377878,17.1150480365207,-5.29409392857891));
#98128=CARTESIAN_POINT('Ctrl Pts',(18.8730906016543,17.095734913275,-5.30326273946136));
#98129=CARTESIAN_POINT('Ctrl Pts',(18.7634487630281,17.0913712090237,-5.3091613544561));
#98130=CARTESIAN_POINT('Ctrl Pts',(18.5936323344809,17.0977960734939,-5.31841466959183));
#98131=CARTESIAN_POINT('Ctrl Pts',(18.5334302117375,17.1026582291857,-5.32172055381736));
#98132=CARTESIAN_POINT('Ctrl Pts',(18.4157446272804,17.1172493075713,-5.32836359578313));
#98133=CARTESIAN_POINT('Ctrl Pts',(18.3582935058201,17.1267922885538,-5.33169277155115));
#98134=CARTESIAN_POINT('Ctrl Pts',(18.2925983050441,17.1405090374674,-5.33567393163575));
#98135=CARTESIAN_POINT('Ctrl Pts',(18.2838939502995,17.1423838393813,-5.33620499030984));
#98136=CARTESIAN_POINT('Ctrl Pts',(18.2707867154551,17.1452936057689,-5.33701041681783));
#98137=CARTESIAN_POINT('Ctrl Pts',(18.2663747752304,17.1462878887279,-5.33728251052522));
#98138=CARTESIAN_POINT('Ctrl Pts',(18.2584890838033,17.148091594195,-5.33777065477873));
#98139=CARTESIAN_POINT('Ctrl Pts',(18.2550141624138,17.1488956647912,-5.33798639594007));
#98140=CARTESIAN_POINT('Ctrl Pts',(18.2474999580234,17.1506544134868,-5.33845430438067));
#98141=CARTESIAN_POINT('Ctrl Pts',(18.2434615014439,17.1516121765294,-5.33870664218224));
#98142=CARTESIAN_POINT('Ctrl Pts',(18.2322055765157,17.1543166262999,-5.33941231404738));
#98143=CARTESIAN_POINT('Ctrl Pts',(18.2249945255667,17.1560894018634,-5.33986710932274));
#98144=CARTESIAN_POINT('Ctrl Pts',(18.1834902308312,17.1665247459197,-5.34249979479707));
#98145=CARTESIAN_POINT('Ctrl Pts',(18.1494111881358,17.1760072109599,-5.3447207224182));
#98146=CARTESIAN_POINT('Ctrl Pts',(18.0412567969326,17.2090418452874,-5.35192534350078));
#98147=CARTESIAN_POINT('Ctrl Pts',(17.9682370295545,17.2358202525296,-5.35702525829945));
#98148=CARTESIAN_POINT('Ctrl Pts',(17.7268424049412,17.3397473451085,-5.37436991876636));
#98149=CARTESIAN_POINT('Ctrl Pts',(17.5671202279576,17.4349449970406,-5.38658847261831));
#98150=CARTESIAN_POINT('Ctrl Pts',(17.4024246351647,17.5650334089522,-5.39952828948029));
#98151=CARTESIAN_POINT('Ctrl Pts',(17.3833124394935,17.580680348512,-5.40103764730808));
#98152=CARTESIAN_POINT('Ctrl Pts',(17.3569790414246,17.603020217905,-5.40312909352447));
#98153=CARTESIAN_POINT('Ctrl Pts',(17.3495246306124,17.6094339986604,-5.40372249904741));
#98154=CARTESIAN_POINT('Ctrl Pts',(17.337579317074,17.6198574814043,-5.40467570042938));
#98155=CARTESIAN_POINT('Ctrl Pts',(17.3330604201126,17.6238347493549,-5.40503683318622));
#98156=CARTESIAN_POINT('Ctrl Pts',(17.3240070515465,17.6318717826441,-5.40576145854981));
#98157=CARTESIAN_POINT('Ctrl Pts',(17.3194729994174,17.6359319356438,-5.40612492990108));
#98158=CARTESIAN_POINT('Ctrl Pts',(17.3087575434609,17.6456110004192,-5.40698532677446));
#98159=CARTESIAN_POINT('Ctrl Pts',(17.3025917338053,17.6512470841663,-5.40748152144987));
#98160=CARTESIAN_POINT('Ctrl Pts',(17.2833844706732,17.6690140031828,-5.4090308788075));
#98161=CARTESIAN_POINT('Ctrl Pts',(17.2704624312886,17.6812732132746,-5.41007855568076));
#98162=CARTESIAN_POINT('Ctrl Pts',(17.2407218398731,17.7102101273218,-5.41250363177934));
#98163=CARTESIAN_POINT('Ctrl Pts',(17.2240252300558,17.7270100529576,-5.4138756822937));
#98164=CARTESIAN_POINT('Ctrl Pts',(17.1672501941593,17.786086938513,-5.4185839250987));
#98165=CARTESIAN_POINT('Ctrl Pts',(17.1286356377501,17.8297367398963,-5.42186133841043));
#98166=CARTESIAN_POINT('Ctrl Pts',(16.9872885638627,18.0034625625894,-5.43428376472812));
#98167=CARTESIAN_POINT('Ctrl Pts',(16.8981704334622,18.1438211181074,-5.4430137233738));
#98168=CARTESIAN_POINT('Ctrl Pts',(16.8011345781242,18.3454955232621,-5.45555189605258));
#98169=CARTESIAN_POINT('Ctrl Pts',(16.7781056627413,18.3988775980773,-5.45887555300619));
#98170=CARTESIAN_POINT('Ctrl Pts',(16.7541175175169,18.4614444156118,-5.46285056196539));
#98171=CARTESIAN_POINT('Ctrl Pts',(16.7509837343203,18.4697748639589,-5.46338140995003));
#98172=CARTESIAN_POINT('Ctrl Pts',(16.7470710655027,18.4803782241668,-5.46405941616438));
#98173=CARTESIAN_POINT('Ctrl Pts',(16.7462433354765,18.4826331881799,-5.46420373713071));
#98174=CARTESIAN_POINT('Ctrl Pts',(16.7454194503191,18.4848895418527,-5.46434828430915));
#98175=CARTESIAN_POINT('Ctrl Pts',(16.745419381199,18.4848897311503,-5.24452701096005));
#98176=CARTESIAN_POINT('Ctrl Pts',(16.7665875207388,18.4269170597383,-5.24117480144515));
#98177=CARTESIAN_POINT('Ctrl Pts',(16.79029877288,18.369848040943,-5.23782816810057));
#98178=CARTESIAN_POINT('Ctrl Pts',(16.8430672123269,18.2570645705659,-5.23098482960947));
#98179=CARTESIAN_POINT('Ctrl Pts',(16.8721437363652,18.2014903584518,-5.2274929886192));
#98180=CARTESIAN_POINT('Ctrl Pts',(16.9191780061591,18.1205568161515,-5.22210863810526));
#98181=CARTESIAN_POINT('Ctrl Pts',(16.9352983715831,18.0941663366885,-5.22030283547618));
#98182=CARTESIAN_POINT('Ctrl Pts',(16.9558380197945,18.062139789975,-5.21803691042424));
#98183=CARTESIAN_POINT('Ctrl Pts',(16.9597163424726,18.0561591844035,-5.21761051195919));
#98184=CARTESIAN_POINT('Ctrl Pts',(16.9658647108679,18.0467821133109,-5.21693661899035));
#98185=CARTESIAN_POINT('Ctrl Pts',(16.9681145521063,18.043372374158,-5.21669045644307));
#98186=CARTESIAN_POINT('Ctrl Pts',(16.9723521719804,18.0369903254211,-5.21622756791302));
#98187=CARTESIAN_POINT('Ctrl Pts',(16.9743376167164,18.0340165327635,-5.21601099811852));
#98188=CARTESIAN_POINT('Ctrl Pts',(16.9789053705259,18.0272123578381,-5.2155134637109));
#98189=CARTESIAN_POINT('Ctrl Pts',(16.9814926820828,18.0233853992743,-5.21523216421622));
#98190=CARTESIAN_POINT('Ctrl Pts',(16.9895487919404,18.0115530536154,-5.21435795951966));
#98191=CARTESIAN_POINT('Ctrl Pts',(16.9950599823976,18.0035768755451,-5.21376228848335));
#98192=CARTESIAN_POINT('Ctrl Pts',(17.0573285124062,17.9147681396608,-5.20706090758718));
#98193=CARTESIAN_POINT('Ctrl Pts',(17.1196150883644,17.8379737651375,-5.20062764360413));
#98194=CARTESIAN_POINT('Ctrl Pts',(17.3015407181285,17.6432341265288,-5.18307319300389));
#98195=CARTESIAN_POINT('Ctrl Pts',(17.4302426694658,17.5346758175266,-5.17192748994837));
#98196=CARTESIAN_POINT('Ctrl Pts',(17.5967906923591,17.4250996310605,-5.15940133723881));
#98197=CARTESIAN_POINT('Ctrl Pts',(17.6235431133017,17.4083434034479,-5.15743871782998));
#98198=CARTESIAN_POINT('Ctrl Pts',(17.6638283057349,17.3843483036585,-5.15455519500633));
#98199=CARTESIAN_POINT('Ctrl Pts',(17.6770802748512,17.3766487280465,-5.15361788718658));
#98200=CARTESIAN_POINT('Ctrl Pts',(17.7013526899396,17.3628964935241,-5.15192118788303));
#98201=CARTESIAN_POINT('Ctrl Pts',(17.7123455761262,17.356796859432,-5.15116013442713));
#98202=CARTESIAN_POINT('Ctrl Pts',(17.7297375581182,17.3473481835301,-5.14996745028875));
#98203=CARTESIAN_POINT('Ctrl Pts',(17.7361004399357,17.3439334197088,-5.14953347939301));
#98204=CARTESIAN_POINT('Ctrl Pts',(17.7425268617009,17.340526792826,-5.14909753542998));
#98205=CARTESIAN_POINT('Ctrl Pts',(17.7425729937549,17.3405023405487,-5.14909440612938));
#98206=CARTESIAN_POINT('Ctrl Pts',(17.7426668839292,17.3404525785478,-5.14908803747501));
#98207=CARTESIAN_POINT('Ctrl Pts',(17.7427146431582,17.340427268393,-5.14908479805474));
#98208=CARTESIAN_POINT('Ctrl Pts',(17.7428118470402,17.3403757596561,-5.14907820516147));
#98209=CARTESIAN_POINT('Ctrl Pts',(17.7428612926054,17.3403495607585,-5.14907485163596));
#98210=CARTESIAN_POINT('Ctrl Pts',(17.742961930683,17.3402962424479,-5.14906802638801));
#98211=CARTESIAN_POINT('Ctrl Pts',(17.7430131240878,17.3402691227423,-5.1490645546151));
#98212=CARTESIAN_POINT('Ctrl Pts',(17.7431173215902,17.3402139295943,-5.14905748857992));
#98213=CARTESIAN_POINT('Ctrl Pts',(17.7431703265441,17.3401858558916,-5.14905389427035));
#98214=CARTESIAN_POINT('Ctrl Pts',(17.7432782132587,17.3401287203199,-5.14904657871138));
#98215=CARTESIAN_POINT('Ctrl Pts',(17.7433330958113,17.3400996582391,-5.14904285741986));
#98216=CARTESIAN_POINT('Ctrl Pts',(17.7434448062837,17.3400405102367,-5.14903528328347));
#98217=CARTESIAN_POINT('Ctrl Pts',(17.7435016349047,17.3400104241665,-5.14903143040346));
#98218=CARTESIAN_POINT('Ctrl Pts',(17.7436173084945,17.3399491912835,-5.14902358831549));
#98219=CARTESIAN_POINT('Ctrl Pts',(17.7436761541978,17.3399180443209,-5.14901959907105));
#98220=CARTESIAN_POINT('Ctrl Pts',(17.7437959355934,17.3398546514006,-5.14901147930244));
#98221=CARTESIAN_POINT('Ctrl Pts',(17.7438568718533,17.3398224053991,-5.14900734875409));
#98222=CARTESIAN_POINT('Ctrl Pts',(17.7439809105642,17.3397567748556,-5.14899894125579));
#98223=CARTESIAN_POINT('Ctrl Pts',(17.7440440136382,17.3397233902593,-5.14899466427896));
#98224=CARTESIAN_POINT('Ctrl Pts',(17.7441724649142,17.3396554416007,-5.14898595862013));
#98225=CARTESIAN_POINT('Ctrl Pts',(17.744237813652,17.3396208775503,-5.14898152991829));
#98226=CARTESIAN_POINT('Ctrl Pts',(17.7443708400812,17.3395505265439,-5.14897251517862));
#98227=CARTESIAN_POINT('Ctrl Pts',(17.744438515141,17.3395147412968,-5.14896792933687));
#98228=CARTESIAN_POINT('Ctrl Pts',(17.744565124291,17.3394478016433,-5.14895935045504));
#98229=CARTESIAN_POINT('Ctrl Pts',(17.7446240592246,17.3394166456558,-5.14895535729448));
#98230=CARTESIAN_POINT('Ctrl Pts',(17.7447516801295,17.3393491865018,-5.14894671071834));
#98231=CARTESIAN_POINT('Ctrl Pts',(17.7448203677342,17.3393128837474,-5.14894205726322));
#98232=CARTESIAN_POINT('Ctrl Pts',(17.7449690904234,17.3392342913453,-5.14893198216726));
#98233=CARTESIAN_POINT('Ctrl Pts',(17.7450491271088,17.339192002581,-5.14892656051443));
#98234=CARTESIAN_POINT('Ctrl Pts',(17.7452223978501,17.3391004662097,-5.14891482401745));
#98235=CARTESIAN_POINT('Ctrl Pts',(17.7453156336344,17.3390512200324,-5.1489085091869));
#98236=CARTESIAN_POINT('Ctrl Pts',(17.7455174426764,17.3389446458661,-5.14889484179935));
#98237=CARTESIAN_POINT('Ctrl Pts',(17.7456260177007,17.3388873201143,-5.14888748929952));
#98238=CARTESIAN_POINT('Ctrl Pts',(17.7458609758868,17.3387632923568,-5.14887157982363));
#98239=CARTESIAN_POINT('Ctrl Pts',(17.7459873605098,17.3386965938638,-5.14886302298758));
#98240=CARTESIAN_POINT('Ctrl Pts',(17.7462732875681,17.3385457351152,-5.14884366643892));
#98241=CARTESIAN_POINT('Ctrl Pts',(17.7464328340597,17.3384615824252,-5.14883286699294));
#98242=CARTESIAN_POINT('Ctrl Pts',(17.7523042951661,17.3353656433259,-5.14843549068378));
#98243=CARTESIAN_POINT('Ctrl Pts',(17.7580299971857,17.3323799607537,-5.1480498414139));
#98244=CARTESIAN_POINT('Ctrl Pts',(17.7712868462962,17.3255441073084,-5.14716118409919));
#98245=CARTESIAN_POINT('Ctrl Pts',(17.778827618023,17.32171276311,-5.14665884326033));
#98246=CARTESIAN_POINT('Ctrl Pts',(17.7991802184313,17.3115249366375,-5.14531132764273));
#98247=CARTESIAN_POINT('Ctrl Pts',(17.812033972748,17.3052528499592,-5.14446910053862));
#98248=CARTESIAN_POINT('Ctrl Pts',(17.9304952002776,17.2489278558678,-5.13678484693071));
#98249=CARTESIAN_POINT('Ctrl Pts',(18.0400203632305,17.2075667989625,-5.13025966790724));
#98250=CARTESIAN_POINT('Ctrl Pts',(18.3090877065854,17.1306900886076,-5.11494053939293));
#98251=CARTESIAN_POINT('Ctrl Pts',(18.4703869809401,17.1041692002194,-5.10633029852664));
#98252=CARTESIAN_POINT('Ctrl Pts',(18.6653452635767,17.094867431543,-5.09512044645868));
#98253=CARTESIAN_POINT('Ctrl Pts',(18.6976101780815,17.0940668302937,-5.09323781104055));
#98254=CARTESIAN_POINT('Ctrl Pts',(18.7371021607656,17.0939899493437,-5.09088633191333));
#98255=CARTESIAN_POINT('Ctrl Pts',(18.7443254861544,17.0940128581174,-5.09045430113954));
#98256=CARTESIAN_POINT('Ctrl Pts',(18.7556544325444,17.0941067703038,-5.08977348621681));
#98257=CARTESIAN_POINT('Ctrl Pts',(18.7597602832643,17.0941527529058,-5.08952607997421));
#98258=CARTESIAN_POINT('Ctrl Pts',(18.7674380386202,17.0942610789131,-5.08906215587487));
#98259=CARTESIAN_POINT('Ctrl Pts',(18.7710099280465,17.0943205185864,-5.08884580206336));
#98260=CARTESIAN_POINT('Ctrl Pts',(18.7791676957407,17.094476926914,-5.08835048726969));
#98261=CARTESIAN_POINT('Ctrl Pts',(18.7837534045061,17.0945797587744,-5.0880712025695));
#98262=CARTESIAN_POINT('Ctrl Pts',(18.7978632819704,17.0949420473855,-5.08720931090085));
#98263=CARTESIAN_POINT('Ctrl Pts',(18.8073859086107,17.0952508943102,-5.08662404703951));
#98264=CARTESIAN_POINT('Ctrl Pts',(18.9364096869498,17.1003076005152,-5.07864861266085));
#98265=CARTESIAN_POINT('Ctrl Pts',(19.0552882197228,17.1151089398747,-5.07078164892295));
#98266=CARTESIAN_POINT('Ctrl Pts',(19.2788793356495,17.1624222177002,-5.05568351915807));
#98267=CARTESIAN_POINT('Ctrl Pts',(19.3836001930243,17.1931824943587,-5.04848024951828));
#98268=CARTESIAN_POINT('Ctrl Pts',(19.5556501469808,17.2585113818391,-5.0366556210673));
#98269=CARTESIAN_POINT('Ctrl Pts',(19.6243475460686,17.2888646867418,-5.03193409089951));
#98270=CARTESIAN_POINT('Ctrl Pts',(19.708070742436,17.3313114693982,-5.02618365548227));
#98271=CARTESIAN_POINT('Ctrl Pts',(19.7247332835523,17.3400402516219,-5.02503922766813));
#98272=CARTESIAN_POINT('Ctrl Pts',(19.7488019286374,17.3530604888887,-5.02338571789685));
#98273=CARTESIAN_POINT('Ctrl Pts',(19.7563014877007,17.3571764234655,-5.02287043932883));
#98274=CARTESIAN_POINT('Ctrl Pts',(19.7694108074949,17.3644748708633,-5.02196955231988));
#98275=CARTESIAN_POINT('Ctrl Pts',(19.7750313188752,17.3676377492855,-5.02158324789162));
#98276=CARTESIAN_POINT('Ctrl Pts',(19.7859201083961,17.3738309763772,-5.02083470200891));
#98277=CARTESIAN_POINT('Ctrl Pts',(19.7911899575873,17.3768584213403,-5.02047236100222));
#98278=CARTESIAN_POINT('Ctrl Pts',(19.8037616516294,17.3841528441756,-5.01960776236391));
#98279=CARTESIAN_POINT('Ctrl Pts',(19.8110511444346,17.3884409865613,-5.01910627519593));
#98280=CARTESIAN_POINT('Ctrl Pts',(19.8372915207901,17.404089651508,-5.01730026724312));
#98281=CARTESIAN_POINT('Ctrl Pts',(19.8560903810793,17.4157032506496,-5.01600496945837));
#98282=CARTESIAN_POINT('Ctrl Pts',(20.0311433128968,17.5276718041231,-5.00391919883066));
#98283=CARTESIAN_POINT('Ctrl Pts',(20.1737328988905,17.647878196273,-4.99398659812591));
#98284=CARTESIAN_POINT('Ctrl Pts',(20.3527446000026,17.8443378473788,-4.97949718431949));
#98285=CARTESIAN_POINT('Ctrl Pts',(20.4032656567957,17.9065270474114,-4.97509387528752));
#98286=CARTESIAN_POINT('Ctrl Pts',(20.471224497983,18.0006129825604,-4.96845483110276));
#98287=CARTESIAN_POINT('Ctrl Pts',(20.4915597355171,18.030335307369,-4.96636025628068));
#98288=CARTESIAN_POINT('Ctrl Pts',(20.5151824692052,18.0668261768349,-4.96377332146848));
#98289=CARTESIAN_POINT('Ctrl Pts',(20.5192059279987,18.0731140140186,-4.96332702094746));
#98290=CARTESIAN_POINT('Ctrl Pts',(20.5254190716096,18.0829379416076,-4.96262868255573));
#98291=CARTESIAN_POINT('Ctrl Pts',(20.5276317792475,18.0864594993949,-4.9623781420078));
#98292=CARTESIAN_POINT('Ctrl Pts',(20.5317223383541,18.0930124732045,-4.96191150004868));
#98293=CARTESIAN_POINT('Ctrl Pts',(20.533602913083,18.0960421216454,-4.9616955821236));
#98294=CARTESIAN_POINT('Ctrl Pts',(20.5378451174003,18.102915102167,-4.96120536747651));
#98295=CARTESIAN_POINT('Ctrl Pts',(20.5402021108608,18.1067612204667,-4.96093077309707));
#98296=CARTESIAN_POINT('Ctrl Pts',(20.5462565717578,18.1167120774044,-4.96021969315446));
#98297=CARTESIAN_POINT('Ctrl Pts',(20.5499354570135,18.1228279768035,-4.95978204020591));
#98298=CARTESIAN_POINT('Ctrl Pts',(20.5723483664446,18.1605181182324,-4.95708172966992));
#98299=CARTESIAN_POINT('Ctrl Pts',(20.5902881255627,18.1925546551957,-4.95477276410428));
#98300=CARTESIAN_POINT('Ctrl Pts',(20.6867179057959,18.3757769882834,-4.94155887217023));
#98301=CARTESIAN_POINT('Ctrl Pts',(20.7475683513684,18.5355370038938,-4.93006551996235));
#98302=CARTESIAN_POINT('Ctrl Pts',(20.8116277076602,18.7935427779359,-4.91278865236797));
#98303=CARTESIAN_POINT('Ctrl Pts',(20.8283436779442,18.8876793428476,-4.90672137332949));
#98304=CARTESIAN_POINT('Ctrl Pts',(20.8409557532101,19.0039140454517,-4.89953959306726));
#98305=CARTESIAN_POINT('Ctrl Pts',(20.8429418773827,19.0252276953234,-4.89823491581578));
#98306=CARTESIAN_POINT('Ctrl Pts',(20.8453044512104,19.0555531311161,-4.89639535169131));
#98307=CARTESIAN_POINT('Ctrl Pts',(20.8459470553223,19.0645423126358,-4.89585214530947));
#98308=CARTESIAN_POINT('Ctrl Pts',(20.8469560512532,19.0800483917354,-4.8949186465579));
#98309=CARTESIAN_POINT('Ctrl Pts',(20.847349737989,19.0865633307368,-4.89452750254457));
#98310=CARTESIAN_POINT('Ctrl Pts',(20.8480455106944,19.0990350450933,-4.89378073458804));
#98311=CARTESIAN_POINT('Ctrl Pts',(20.8483525640714,19.1049914704365,-4.89342495845663));
#98312=CARTESIAN_POINT('Ctrl Pts',(20.8490849377019,19.1204706260673,-4.89250262626724));
#98313=CARTESIAN_POINT('Ctrl Pts',(20.8494711244829,19.1299951406741,-4.89193730086953));
#98314=CARTESIAN_POINT('Ctrl Pts',(20.8505663603021,19.1624148244431,-4.89002026407437));
#98315=CARTESIAN_POINT('Ctrl Pts',(20.850968170873,19.1853192558791,-4.88867816123748));
#98316=CARTESIAN_POINT('Ctrl Pts',(20.8512295742387,19.3848382571626,-4.87708342181251));
#98317=CARTESIAN_POINT('Ctrl Pts',(20.8293614529549,19.5607825552394,-4.86759302040801));
#98318=CARTESIAN_POINT('Ctrl Pts',(20.7646769708164,19.8155434887637,-4.85328878113131));
#98319=CARTESIAN_POINT('Ctrl Pts',(20.7383771692414,19.8977252753808,-4.84856657343219));
#98320=CARTESIAN_POINT('Ctrl Pts',(20.6935117427131,20.0131335107421,-4.84149554083877));
#98321=CARTESIAN_POINT('Ctrl Pts',(20.6789483766716,20.0478272567555,-4.83930983386104));
#98322=CARTESIAN_POINT('Ctrl Pts',(20.6603586337361,20.0890026029904,-4.836621838883));
#98323=CARTESIAN_POINT('Ctrl Pts',(20.6572108952173,20.0958762654956,-4.83616991645551));
#98324=CARTESIAN_POINT('Ctrl Pts',(20.652265838085,20.1065236707714,-4.8354646804091));
#98325=CARTESIAN_POINT('Ctrl Pts',(20.6504940099607,20.1103092791512,-4.83521291234682));
#98326=CARTESIAN_POINT('Ctrl Pts',(20.6471906365745,20.1173130199926,-4.83474516789243));
#98327=CARTESIAN_POINT('Ctrl Pts',(20.6456621714024,20.120532541435,-4.83452938247815));
#98328=CARTESIAN_POINT('Ctrl Pts',(20.6421925724225,20.1277934375356,-4.83404099175021));
#98329=CARTESIAN_POINT('Ctrl Pts',(20.6402467370215,20.1318324914427,-4.83376809826387));
#98330=CARTESIAN_POINT('Ctrl Pts',(20.6344781805794,20.1437098897379,-4.8329621038197));
#98331=CARTESIAN_POINT('Ctrl Pts',(20.6306198923733,20.1515307177956,-4.83242686573392));
#98332=CARTESIAN_POINT('Ctrl Pts',(20.6028090913762,20.2070367399427,-4.82859708356805));
#98333=CARTESIAN_POINT('Ctrl Pts',(20.577111425047,20.2538210993135,-4.82520541176137));
#98334=CARTESIAN_POINT('Ctrl Pts',(20.5406308104231,20.3146682419944,-4.82062024070629));
#98335=CARTESIAN_POINT('Ctrl Pts',(20.5313973760414,20.3296425353914,-4.81947726141034));
#98336=CARTESIAN_POINT('Ctrl Pts',(20.4960066704448,20.385467713749,-4.81516533013202));
#98337=CARTESIAN_POINT('Ctrl Pts',(20.4686350205583,20.4255299603789,-4.81196761137516));
#98338=CARTESIAN_POINT('Ctrl Pts',(20.3751395296935,20.5527580454857,-4.80153801841995));
#98339=CARTESIAN_POINT('Ctrl Pts',(20.303627718832,20.6357546801402,-4.79430521590294));
#98340=CARTESIAN_POINT('Ctrl Pts',(20.1869268522954,20.751690994199,-4.78373156033375));
#98341=CARTESIAN_POINT('Ctrl Pts',(20.1463327189766,20.7889867837565,-4.78024233014644));
#98342=CARTESIAN_POINT('Ctrl Pts',(20.0781788860306,20.8468633414559,-4.77468462939269));
#98343=CARTESIAN_POINT('Ctrl Pts',(20.0514942736566,20.8684301809681,-4.77257771781605));
#98344=CARTESIAN_POINT('Ctrl Pts',(20.0157271242064,20.8959277144478,-4.76984113922598));
#98345=CARTESIAN_POINT('Ctrl Pts',(20.0071077823162,20.9024497938846,-4.76918812982322));
#98346=CARTESIAN_POINT('Ctrl Pts',(19.9929062907476,20.9130257148125,-4.76812262418186));
#98347=CARTESIAN_POINT('Ctrl Pts',(19.9873536859432,20.9171187304674,-4.76770859846668));
#98348=CARTESIAN_POINT('Ctrl Pts',(19.9765651570821,20.9249902332771,-4.76690908268898));
#98349=CARTESIAN_POINT('Ctrl Pts',(19.9713317637717,20.9287720445831,-4.76652346627546));
#98350=CARTESIAN_POINT('Ctrl Pts',(19.9592058922682,20.9374504051987,-4.7656350491395));
#98351=CARTESIAN_POINT('Ctrl Pts',(19.9523011899901,20.9423297472438,-4.765132914467));
#98352=CARTESIAN_POINT('Ctrl Pts',(19.9336483463962,20.9553443003065,-4.76378631694572));
#98353=CARTESIAN_POINT('Ctrl Pts',(19.921846633497,20.9634022321439,-4.76294479541847));
#98354=CARTESIAN_POINT('Ctrl Pts',(19.8128225316931,21.0362338476429,-4.75526374040295));
#98355=CARTESIAN_POINT('Ctrl Pts',(19.7104705091745,21.0929796120467,-4.74874081363296));
#98356=CARTESIAN_POINT('Ctrl Pts',(19.4555786090185,21.2078722561001,-4.73343476668945));
#98357=CARTESIAN_POINT('Ctrl Pts',(19.3000126966134,21.2574096046306,-4.72483473246113));
#98358=CARTESIAN_POINT('Ctrl Pts',(19.1084258281255,21.2948788713808,-4.7136257228041));
#98359=CARTESIAN_POINT('Ctrl Pts',(19.076383470885,21.3003824802869,-4.7117296331103));
#98360=CARTESIAN_POINT('Ctrl Pts',(19.0370676313179,21.3062067735073,-4.70936318475707));
#98361=CARTESIAN_POINT('Ctrl Pts',(19.0299008343908,21.307230928516,-4.70893019429197));
#98362=CARTESIAN_POINT('Ctrl Pts',(19.0186577337376,21.3087787929985,-4.70824820021469));
#98363=CARTESIAN_POINT('Ctrl Pts',(19.0145848403025,21.3093274378569,-4.70800058240478));
#98364=CARTESIAN_POINT('Ctrl Pts',(19.0069690724334,21.3103307610446,-4.7075364795854));
#98365=CARTESIAN_POINT('Ctrl Pts',(19.0034266360555,21.3107883335948,-4.70732015994906));
#98366=CARTESIAN_POINT('Ctrl Pts',(18.9953378506481,21.3118123471456,-4.70682521104011));
#98367=CARTESIAN_POINT('Ctrl Pts',(18.9907908261307,21.3123729942122,-4.70654625989907));
#98368=CARTESIAN_POINT('Ctrl Pts',(18.9768095662562,21.3140508239046,-4.70568639707687));
#98369=CARTESIAN_POINT('Ctrl Pts',(18.9673697532037,21.3151192466088,-4.70510284624257));
#98370=CARTESIAN_POINT('Ctrl Pts',(18.8825210037021,21.3241446574914,-4.69983274965195));
#98371=CARTESIAN_POINT('Ctrl Pts',(18.806750143018,21.3281073919894,-4.69495152712518));
#98372=CARTESIAN_POINT('Ctrl Pts',(18.5460074647156,21.3277304198091,-4.67789871868947));
#98373=CARTESIAN_POINT('Ctrl Pts',(18.3618681058443,21.3032300477396,-4.66550124996916));
#98374=CARTESIAN_POINT('Ctrl Pts',(18.1318241503516,21.2412487702261,-4.65047365059779));
#98375=CARTESIAN_POINT('Ctrl Pts',(18.0809342985178,21.2254557108729,-4.64717204928174));
#98376=CARTESIAN_POINT('Ctrl Pts',(18.0188621994328,21.2035923301053,-4.64317035481114));
#98377=CARTESIAN_POINT('Ctrl Pts',(18.0070708973072,21.1993209896954,-4.64241130097009));
#98378=CARTESIAN_POINT('Ctrl Pts',(17.9884946120081,21.1924044842425,-4.64121706921076));
#98379=CARTESIAN_POINT('Ctrl Pts',(17.981684267272,21.1898287076082,-4.64077958751628));
#98380=CARTESIAN_POINT('Ctrl Pts',(17.968942133346,21.1849341479904,-4.63996165543386));
#98381=CARTESIAN_POINT('Ctrl Pts',(17.9630072727639,21.182623639504,-4.63958093314989));
#98382=CARTESIAN_POINT('Ctrl Pts',(17.9497500548354,21.1773934404949,-4.63873098376972));
#98383=CARTESIAN_POINT('Ctrl Pts',(17.9424333721073,21.1744595528021,-4.63826224048039));
#98384=CARTESIAN_POINT('Ctrl Pts',(17.9239381160256,21.1669230259619,-4.6370781191557));
#98385=CARTESIAN_POINT('Ctrl Pts',(17.9127821716643,21.1622653399452,-4.63636460666203));
#98386=CARTESIAN_POINT('Ctrl Pts',(17.8493618896023,21.135146671232,-4.63231159546641));
#98387=CARTESIAN_POINT('Ctrl Pts',(17.7979770661027,21.110680735478,-4.62904120317594));
#98388=CARTESIAN_POINT('Ctrl Pts',(17.7238770586398,21.0716616270324,-4.62431038000907));
#98389=CARTESIAN_POINT('Ctrl Pts',(17.7003571279539,21.0586992529641,-4.62280634098087));
#98390=CARTESIAN_POINT('Ctrl Pts',(17.5767140742856,20.987456731641,-4.61486880108734));
#98391=CARTESIAN_POINT('Ctrl Pts',(17.4812555646195,20.9214798729665,-4.60864386096608));
#98392=CARTESIAN_POINT('Ctrl Pts',(17.3297827366213,20.7972750668102,-4.59796498357712));
#98393=CARTESIAN_POINT('Ctrl Pts',(17.2708254705386,20.7430616847505,-4.59356323704014));
#98394=CARTESIAN_POINT('Ctrl Pts',(17.1900057768913,20.6598157038647,-4.58692631778353));
#98395=CARTESIAN_POINT('Ctrl Pts',(17.1655927649907,20.6333513989536,-4.58483220143466));
#98396=CARTESIAN_POINT('Ctrl Pts',(17.1369482569954,20.6006655889278,-4.5822457752747));
#98397=CARTESIAN_POINT('Ctrl Pts',(17.1320583328928,20.5950258705332,-4.58179950377347));
#98398=CARTESIAN_POINT('Ctrl Pts',(17.1244905668321,20.5862038690185,-4.58110120099635));
#98399=CARTESIAN_POINT('Ctrl Pts',(17.1217920484444,20.5830392913752,-4.58085066679607));
#98400=CARTESIAN_POINT('Ctrl Pts',(17.1167971345355,20.5771466275252,-4.58038403048547));
#98401=CARTESIAN_POINT('Ctrl Pts',(17.1144983004347,20.5744206835985,-4.58016811182235));
#98402=CARTESIAN_POINT('Ctrl Pts',(17.1093069070463,20.5682331057692,-4.57967788750414));
#98403=CARTESIAN_POINT('Ctrl Pts',(17.1064185330244,20.5647680440806,-4.57940328414158));
#98404=CARTESIAN_POINT('Ctrl Pts',(17.0978965100615,20.5544778343176,-4.57858763695095));
#98405=CARTESIAN_POINT('Ctrl Pts',(17.0922946412651,20.5476266606343,-4.57804438040996));
#98406=CARTESIAN_POINT('Ctrl Pts',(17.0511025773865,20.4965985139932,-4.57399795859996));
#98407=CARTESIAN_POINT('Ctrl Pts',(17.0172611142355,20.4510458272492,-4.57038509503549));
#98408=CARTESIAN_POINT('Ctrl Pts',(16.9504036025297,20.3530615930658,-4.56270240111715));
#98409=CARTESIAN_POINT('Ctrl Pts',(16.9177751785404,20.3004253513025,-4.5586247818669));
#98410=CARTESIAN_POINT('Ctrl Pts',(16.8338945767296,20.1508408274315,-4.54729667242138));
#98411=CARTESIAN_POINT('Ctrl Pts',(16.7877886618243,20.0512179998227,-4.5400480933186));
#98412=CARTESIAN_POINT('Ctrl Pts',(16.7303166545563,19.8965707557044,-4.52944127355711));
#98413=CARTESIAN_POINT('Ctrl Pts',(16.7130722627021,19.8439345326445,-4.52593476936327));
#98414=CARTESIAN_POINT('Ctrl Pts',(16.6884846754667,19.7575720160236,-4.52035278720549));
#98415=CARTESIAN_POINT('Ctrl Pts',(16.6798675391327,19.7242387002014,-4.51823844816655));
#98416=CARTESIAN_POINT('Ctrl Pts',(16.669614456483,19.6801678230864,-4.51549378176146));
#98417=CARTESIAN_POINT('Ctrl Pts',(16.6672430079269,19.6696083961618,-4.51483993910782));
#98418=CARTESIAN_POINT('Ctrl Pts',(16.6634921046976,19.6522863917352,-4.51377342232846));
#98419=CARTESIAN_POINT('Ctrl Pts',(16.6620645837058,19.6455345285478,-4.51335921312024));
#98420=CARTESIAN_POINT('Ctrl Pts',(16.659365641462,19.6324533808418,-4.51255958342342));
#98421=CARTESIAN_POINT('Ctrl Pts',(16.6580901071821,19.6261250319783,-4.51217403532362));
#98422=CARTESIAN_POINT('Ctrl Pts',(16.6552123724927,19.6115026288507,-4.51128611878298));
#98423=CARTESIAN_POINT('Ctrl Pts',(16.6536308208072,19.6032045861708,-4.51078441398248));
#98424=CARTESIAN_POINT('Ctrl Pts',(16.6495122711541,19.5808694072398,-4.50943973006159));
#98425=CARTESIAN_POINT('Ctrl Pts',(16.6470673798197,19.5668155755174,-4.50859967904288));
#98426=CARTESIAN_POINT('Ctrl Pts',(16.6261906884124,19.4391846390304,-4.50102301574524));
#98427=CARTESIAN_POINT('Ctrl Pts',(16.616903709544,19.3242992233257,-4.49459281375611));
#98428=CARTESIAN_POINT('Ctrl Pts',(16.6171578058469,19.0229639434196,-4.47808639068802));
#98429=CARTESIAN_POINT('Ctrl Pts',(16.6418924517422,18.837581013522,-4.46831880596789));
#98430=CARTESIAN_POINT('Ctrl Pts',(16.6942562459747,18.6441344240756,-4.45654184871822));
#98431=CARTESIAN_POINT('Ctrl Pts',(16.6981093691122,18.6304481264809,-4.4556994591094));
#98432=CARTESIAN_POINT('Ctrl Pts',(16.703660730018,18.6114648710771,-4.45451691988771));
#98433=CARTESIAN_POINT('Ctrl Pts',(16.7052425224818,18.6061338843476,-4.45418327483423));
#98434=CARTESIAN_POINT('Ctrl Pts',(16.70781564271,18.5975855526895,-4.45364567388351));
#98435=CARTESIAN_POINT('Ctrl Pts',(16.7087936865955,18.5943641904044,-4.453442490537));
#98436=CARTESIAN_POINT('Ctrl Pts',(16.710853077047,18.58763896931,-4.45301703896373));
#98437=CARTESIAN_POINT('Ctrl Pts',(16.7119358439217,18.5841355853084,-4.45279468524881));
#98438=CARTESIAN_POINT('Ctrl Pts',(16.7145777265398,18.5756656159272,-4.45225539030026));
#98439=CARTESIAN_POINT('Ctrl Pts',(16.7161460645308,18.5707019507145,-4.45193791291718));
#98440=CARTESIAN_POINT('Ctrl Pts',(16.7216994279354,18.5533490422127,-4.45082311741977));
#98441=CARTESIAN_POINT('Ctrl Pts',(16.7257802848631,18.5409910963517,-4.45002045320262));
#98442=CARTESIAN_POINT('Ctrl Pts',(16.7349633441649,18.5140200780063,-4.4482506304145));
#98443=CARTESIAN_POINT('Ctrl Pts',(16.7401119397152,18.4994250885034,-4.44728123638518));
#98444=CARTESIAN_POINT('Ctrl Pts',(16.7454194484637,18.4848895469342,-4.44630497835508));
#98445=CARTESIAN_POINT('Origin',(18.734,19.211,0.));
#98446=CARTESIAN_POINT('',(16.7454194503191,18.4848895418526,-3.64442446310682));
#98447=CARTESIAN_POINT('',(16.7454195180457,18.4848893563717,-3.86819359339412));
#98448=CARTESIAN_POINT('',(16.7454194503191,18.4848895418526,0.));
#98449=CARTESIAN_POINT('',(16.6170009085985,19.2129458556375,-3.91098515007265));
#98450=CARTESIAN_POINT('Ctrl Pts',(16.7454195180457,18.4848893563717,-3.86819359339412));
#98451=CARTESIAN_POINT('Ctrl Pts',(16.7340081750488,18.5161413069603,-3.8702730290524));
#98452=CARTESIAN_POINT('Ctrl Pts',(16.7233298318036,18.5476724487867,-3.87233003188037));
#98453=CARTESIAN_POINT('Ctrl Pts',(16.7086937641219,18.5945001653747,-3.87532603712808));
#98454=CARTESIAN_POINT('Ctrl Pts',(16.7041601162795,18.6095954250907,-3.87628295790638));
#98455=CARTESIAN_POINT('Ctrl Pts',(16.6975600380691,18.6324963820482,-3.87772162915976));
#98456=CARTESIAN_POINT('Ctrl Pts',(16.6953690628555,18.6402653335688,-3.87820742758997));
#98457=CARTESIAN_POINT('Ctrl Pts',(16.6915244728498,18.6542024625253,-3.87907494690955));
#98458=CARTESIAN_POINT('Ctrl Pts',(16.6898542408526,18.6603659168837,-3.87945720403082));
#98459=CARTESIAN_POINT('Ctrl Pts',(16.6863713151664,18.6734528050941,-3.88026595029803));
#98460=CARTESIAN_POINT('Ctrl Pts',(16.6845657869426,18.6803780762302,-3.88069220305471));
#98461=CARTESIAN_POINT('Ctrl Pts',(16.6809624124013,18.6944919467194,-3.8815574851934));
#98462=CARTESIAN_POINT('Ctrl Pts',(16.6791671199493,18.7016810995306,-3.88199642733997));
#98463=CARTESIAN_POINT('Ctrl Pts',(16.6747876940511,18.7196184016077,-3.88308720594793));
#98464=CARTESIAN_POINT('Ctrl Pts',(16.6722499112019,18.7303777216631,-3.88373755764843));
#98465=CARTESIAN_POINT('Ctrl Pts',(16.6345655721988,18.8959395700599,-3.89368676514654));
#98466=CARTESIAN_POINT('Ctrl Pts',(16.6168549648216,19.0541908608747,-3.90236290972166));
#98467=CARTESIAN_POINT('Ctrl Pts',(16.6170008943792,19.2129459703939,-3.91098517963697));
#98468=CARTESIAN_POINT('Ctrl Pts',(16.6170008942726,19.2129458543872,-3.91098517333644));
#98469=CARTESIAN_POINT('Ctrl Pts',(16.6171322461988,19.3558506431979,-3.91874658439979));
#98470=CARTESIAN_POINT('Ctrl Pts',(16.6317330804654,19.4983603027047,-3.9264424920887));
#98471=CARTESIAN_POINT('Ctrl Pts',(16.6625404319245,19.6478517853169,-3.93541363481339));
#98472=CARTESIAN_POINT('Ctrl Pts',(16.6645760626826,19.6573953229992,-3.9359904216043));
#98473=CARTESIAN_POINT('Ctrl Pts',(16.667882870474,19.6723895637183,-3.93690353184972));
#98474=CARTESIAN_POINT('Ctrl Pts',(16.6691098355725,19.677850007725,-3.93723750276904));
#98475=CARTESIAN_POINT('Ctrl Pts',(16.6714750781768,19.6881844490039,-3.93787242471626));
#98476=CARTESIAN_POINT('Ctrl Pts',(16.672609019639,19.6930594117202,-3.93817313382037));
#98477=CARTESIAN_POINT('Ctrl Pts',(16.6745952748942,19.7014634122482,-3.9386936798716));
#98478=CARTESIAN_POINT('Ctrl Pts',(16.6754394073226,19.7049943994331,-3.93891304719644));
#98479=CARTESIAN_POINT('Ctrl Pts',(16.6770956004237,19.7118442524171,-3.93933990619326));
#98480=CARTESIAN_POINT('Ctrl Pts',(16.6779066143187,19.7151633298341,-3.93954733136033));
#98481=CARTESIAN_POINT('Ctrl Pts',(16.6801205703334,19.7241297588524,-3.94010925993164));
#98482=CARTESIAN_POINT('Ctrl Pts',(16.6815387556165,19.7297732640509,-3.94046462903048));
#98483=CARTESIAN_POINT('Ctrl Pts',(16.6869136883268,19.7507951311197,-3.94179448535118));
#98484=CARTESIAN_POINT('Ctrl Pts',(16.6910200422985,19.7661342261252,-3.94277707608856));
#98485=CARTESIAN_POINT('Ctrl Pts',(16.7288547857979,19.9013557404675,-3.95153871836391));
#98486=CARTESIAN_POINT('Ctrl Pts',(16.7729252523116,20.0180801875818,-3.9597825681384));
#98487=CARTESIAN_POINT('Ctrl Pts',(16.8578682281151,20.1942980367638,-3.9727093888281));
#98488=CARTESIAN_POINT('Ctrl Pts',(16.8919540277664,20.256759487364,-3.97739845763347));
#98489=CARTESIAN_POINT('Ctrl Pts',(16.9780398811445,20.3971934664044,-3.98810073468003));
#98490=CARTESIAN_POINT('Ctrl Pts',(17.0322035681162,20.4736732727662,-3.99404894940884));
#98491=CARTESIAN_POINT('Ctrl Pts',(17.1051790273315,20.5634489711676,-4.00116199014754));
#98492=CARTESIAN_POINT('Ctrl Pts',(17.1193657657752,20.5803547123202,-4.00250801876747));
#98493=CARTESIAN_POINT('Ctrl Pts',(17.1384738220318,20.6024150554793,-4.00427384397666));
#98494=CARTESIAN_POINT('Ctrl Pts',(17.1431600971169,20.6077705776276,-4.00470327820077));
#98495=CARTESIAN_POINT('Ctrl Pts',(17.1524783184886,20.6183118042884,-4.00555006100294));
#98496=CARTESIAN_POINT('Ctrl Pts',(17.1571089823927,20.6234985182166,-4.00596745535447));
#98497=CARTESIAN_POINT('Ctrl Pts',(17.1660753099207,20.6334424744123,-4.00676916200921));
#98498=CARTESIAN_POINT('Ctrl Pts',(17.1704072744565,20.6382029346986,-4.00715362337432));
#98499=CARTESIAN_POINT('Ctrl Pts',(17.1803927715502,20.6490761124179,-4.0080333239212));
#98500=CARTESIAN_POINT('Ctrl Pts',(17.1860608137048,20.6551754062277,-4.00852793905558));
#98501=CARTESIAN_POINT('Ctrl Pts',(17.2012520071404,20.6713302323593,-4.00984119673477));
#98502=CARTESIAN_POINT('Ctrl Pts',(17.2108381953051,20.6813261296286,-4.01065712406613));
#98503=CARTESIAN_POINT('Ctrl Pts',(17.2870189358343,20.7592181323684,-4.01704365034278));
#98504=CARTESIAN_POINT('Ctrl Pts',(17.3580261300918,20.8226552851848,-4.02241038038099));
#98505=CARTESIAN_POINT('Ctrl Pts',(17.5136072429533,20.9438454160643,-4.03330208248319));
#98506=CARTESIAN_POINT('Ctrl Pts',(17.5985800042946,21.0006741303751,-4.03879512597839));
#98507=CARTESIAN_POINT('Ctrl Pts',(17.7562767918343,21.0903720710094,-4.04868788914964));
#98508=CARTESIAN_POINT('Ctrl Pts',(17.8273763185593,21.1256836791062,-4.0530528508949));
#98509=CARTESIAN_POINT('Ctrl Pts',(17.9331536559171,21.1710033043791,-4.05963688937138));
#98510=CARTESIAN_POINT('Ctrl Pts',(17.9663737481862,21.1842504697453,-4.06171725231584));
#98511=CARTESIAN_POINT('Ctrl Pts',(18.006866278449,21.1992204449077,-4.06428632694957));
#98512=CARTESIAN_POINT('Ctrl Pts',(18.0138348289917,21.2017551605717,-4.06472962638129));
#98513=CARTESIAN_POINT('Ctrl Pts',(18.0247533666434,21.2056618000905,-4.06542624786626));
#98514=CARTESIAN_POINT('Ctrl Pts',(18.0286944239498,21.2070587484757,-4.06567810941549));
#98515=CARTESIAN_POINT('Ctrl Pts',(18.0360021530273,21.2096247038287,-4.06614593869295));
#98516=CARTESIAN_POINT('Ctrl Pts',(18.0393676478146,21.2107968886484,-4.06636171487551));
#98517=CARTESIAN_POINT('Ctrl Pts',(18.0469717687189,21.2134238541343,-4.06684997055104));
#98518=CARTESIAN_POINT('Ctrl Pts',(18.0512120393213,21.214873669192,-4.06712273751009));
#98519=CARTESIAN_POINT('Ctrl Pts',(18.0637085721378,21.2191021610163,-4.0679280196735));
#98520=CARTESIAN_POINT('Ctrl Pts',(18.0719773023564,21.2218433129306,-4.06846266647874));
#98521=CARTESIAN_POINT('Ctrl Pts',(18.13086385684,21.2409621156783,-4.07228183069476));
#98522=CARTESIAN_POINT('Ctrl Pts',(18.1820620815793,21.2554761929898,-4.07566289750783));
#98523=CARTESIAN_POINT('Ctrl Pts',(18.376777782,21.3028290671957,-4.08861272684905));
#98524=CARTESIAN_POINT('Ctrl Pts',(18.5230453918307,21.3226005527415,-4.09849088632015));
#98525=CARTESIAN_POINT('Ctrl Pts',(18.7441911936846,21.3292698233333,-4.11289961213195));
#98526=CARTESIAN_POINT('Ctrl Pts',(18.8182691080562,21.3276179320866,-4.1176449942125));
#98527=CARTESIAN_POINT('Ctrl Pts',(18.9199296651094,21.3200038347833,-4.12402275749862));
#98528=CARTESIAN_POINT('Ctrl Pts',(18.9477017627737,21.3173709756192,-4.12575149575042));
#98529=CARTESIAN_POINT('Ctrl Pts',(18.9955496772923,21.3118787499455,-4.12870704764698));
#98530=CARTESIAN_POINT('Ctrl Pts',(19.0156508714278,21.309278481786,-4.12994170526012));
#98531=CARTESIAN_POINT('Ctrl Pts',(19.0445448247617,21.3051180828043,-4.13170687365948));
#98532=CARTESIAN_POINT('Ctrl Pts',(19.0533694336168,21.3037904342281,-4.13224469362501));
#98533=CARTESIAN_POINT('Ctrl Pts',(19.0686176354473,21.3013976725245,-4.13317184880509));
#98534=CARTESIAN_POINT('Ctrl Pts',(19.0750451444487,21.3003586580972,-4.13356200521672));
#98535=CARTESIAN_POINT('Ctrl Pts',(19.0873697610949,21.2983079814154,-4.13430888466098));
#98536=CARTESIAN_POINT('Ctrl Pts',(19.09326756453,21.2973009407909,-4.13466575028568));
#98537=CARTESIAN_POINT('Ctrl Pts',(19.108652110581,21.2946068818921,-4.13559526060995));
#98538=CARTESIAN_POINT('Ctrl Pts',(19.1181318136601,21.292880062979,-4.13616663572549));
#98539=CARTESIAN_POINT('Ctrl Pts',(19.1507198924043,21.2867136658793,-4.1381263592517));
#98540=CARTESIAN_POINT('Ctrl Pts',(19.1737663623093,21.2819534768419,-4.13950450052636));
#98541=CARTESIAN_POINT('Ctrl Pts',(19.3593649103863,21.2403804833745,-4.15055065895701));
#98542=CARTESIAN_POINT('Ctrl Pts',(19.5171301284544,21.1848745094007,-4.15955243294578));
#98543=CARTESIAN_POINT('Ctrl Pts',(19.7800786349565,21.0558148292426,-4.17547157093414));
#98544=CARTESIAN_POINT('Ctrl Pts',(19.8881758113895,20.9901827729904,-4.18235474788397));
#98545=CARTESIAN_POINT('Ctrl Pts',(19.999326516399,20.9082857073215,-4.19050259357584));
#98546=CARTESIAN_POINT('Ctrl Pts',(20.0088253297347,20.901162811534,-4.19120818886398));
#98547=CARTESIAN_POINT('Ctrl Pts',(20.0222515206398,20.8909173150772,-4.19221960688322));
#98548=CARTESIAN_POINT('Ctrl Pts',(20.0262286844835,20.8878599201322,-4.19252099295881));
#98549=CARTESIAN_POINT('Ctrl Pts',(20.0330668742742,20.8825643723634,-4.19304233376008));
#98550=CARTESIAN_POINT('Ctrl Pts',(20.0359331056542,20.8803329155817,-4.1932618149417));
#98551=CARTESIAN_POINT('Ctrl Pts',(20.0414816864101,20.8759901777714,-4.19368859086692));
#98552=CARTESIAN_POINT('Ctrl Pts',(20.0441646780786,20.8738797816756,-4.19389581772906));
#98553=CARTESIAN_POINT('Ctrl Pts',(20.0513947480816,20.8681643702373,-4.19445655064975));
#98554=CARTESIAN_POINT('Ctrl Pts',(20.0559320882067,20.864547164312,-4.19481091601459));
#98555=CARTESIAN_POINT('Ctrl Pts',(20.0727469664247,20.8510287597202,-4.19613317986286));
#98556=CARTESIAN_POINT('Ctrl Pts',(20.0849282545491,20.8410093834432,-4.19710906595625));
#98557=CARTESIAN_POINT('Ctrl Pts',(20.1966283633912,20.7470214721884,-4.20621672860228));
#98558=CARTESIAN_POINT('Ctrl Pts',(20.2883046428404,20.6541821483913,-4.21485581174275));
#98559=CARTESIAN_POINT('Ctrl Pts',(20.4727946800734,20.4292433853559,-4.23407494658443));
#98560=CARTESIAN_POINT('Ctrl Pts',(20.5602584382964,20.2937384948187,-4.24454512065337));
#98561=CARTESIAN_POINT('Ctrl Pts',(20.6409846290793,20.1305388023696,-4.25572787711943));
#98562=CARTESIAN_POINT('Ctrl Pts',(20.6501331131048,20.1113199039178,-4.25702508976319));
#98563=CARTESIAN_POINT('Ctrl Pts',(20.6627321948377,20.0837897614468,-4.25885604748058));
#98564=CARTESIAN_POINT('Ctrl Pts',(20.6664218245012,20.075589927758,-4.25939800661627));
#98565=CARTESIAN_POINT('Ctrl Pts',(20.6726978320906,20.0614012380509,-4.26033003459456));
#98566=CARTESIAN_POINT('Ctrl Pts',(20.6753089555614,20.0554235254695,-4.26072094801069));
#98567=CARTESIAN_POINT('Ctrl Pts',(20.6802562481001,20.0439533239268,-4.26146773334372));
#98568=CARTESIAN_POINT('Ctrl Pts',(20.6825968959646,20.0384628458548,-4.26182375524728));
#98569=CARTESIAN_POINT('Ctrl Pts',(20.6886244241814,20.024156607944,-4.2627477141079));
#98570=CARTESIAN_POINT('Ctrl Pts',(20.6922749185422,20.0153255911684,-4.26331441161118));
#98571=CARTESIAN_POINT('Ctrl Pts',(20.7045260611332,19.9851106327014,-4.26524118247259));
#98572=CARTESIAN_POINT('Ctrl Pts',(20.7128374213022,19.9636106235572,-4.26659151209585));
#98573=CARTESIAN_POINT('Ctrl Pts',(20.7811160665671,19.7780295815631,-4.27808140086563));
#98574=CARTESIAN_POINT('Ctrl Pts',(20.8209119827372,19.6072472051742,-4.287477931127));
#98575=CARTESIAN_POINT('Ctrl Pts',(20.8484770077298,19.3464321839502,-4.30174639421038));
#98576=CARTESIAN_POINT('Ctrl Pts',(20.852268116943,19.2588816240947,-4.30653795327146));
#98577=CARTESIAN_POINT('Ctrl Pts',(20.8499178595543,19.1334000458307,-4.31370249473699));
#98578=CARTESIAN_POINT('Ctrl Pts',(20.8481861880695,19.0954729462956,-4.31590739121543));
#98579=CARTESIAN_POINT('Ctrl Pts',(20.8448868890886,19.0500559339576,-4.31861665567595));
#98580=CARTESIAN_POINT('Ctrl Pts',(20.8442971302259,19.0424993497234,-4.31906972587955));
#98581=CARTESIAN_POINT('Ctrl Pts',(20.8433188658876,19.0307767279496,-4.31977636972615));
#98582=CARTESIAN_POINT('Ctrl Pts',(20.8429585606805,19.026608312511,-4.32002838788244));
#98583=CARTESIAN_POINT('Ctrl Pts',(20.8422684943924,19.0188915537733,-4.32049635942624));
#98584=CARTESIAN_POINT('Ctrl Pts',(20.8419421300191,19.015342964681,-4.32071212031728));
#98585=CARTESIAN_POINT('Ctrl Pts',(20.8411854477312,19.0073371894712,-4.32120015061534));
#98586=CARTESIAN_POINT('Ctrl Pts',(20.8407499494864,19.0028805607125,-4.32147270630836));
#98587=CARTESIAN_POINT('Ctrl Pts',(20.839427181919,18.9897738881274,-4.32227680003598));
#98588=CARTESIAN_POINT('Ctrl Pts',(20.83850076606,18.9811280124874,-4.32281046046641));
#98589=CARTESIAN_POINT('Ctrl Pts',(20.8315639091146,18.9199493667243,-4.32660842497082));
#98590=CARTESIAN_POINT('Ctrl Pts',(20.8236409165926,18.8676566565923,-4.32996810931569));
#98591=CARTESIAN_POINT('Ctrl Pts',(20.8132706188509,18.8130931702028,-4.33355650421712));
#98592=CARTESIAN_POINT('Ctrl Pts',(20.812766315121,18.8104669069373,-4.33372942581347));
#98593=CARTESIAN_POINT('Ctrl Pts',(20.8067039977719,18.7792160284454,-4.3357894640278));
#98594=CARTESIAN_POINT('Ctrl Pts',(20.8005602739575,18.7507090062411,-4.33769236429479));
#98595=CARTESIAN_POINT('Ctrl Pts',(20.7880170342882,18.6978360920448,-4.34125654432872));
#98596=CARTESIAN_POINT('Ctrl Pts',(20.7817674845587,18.6734393333877,-4.34291514306212));
#98597=CARTESIAN_POINT('Ctrl Pts',(20.7465826732987,18.5456179040197,-4.35166346588616));
#98598=CARTESIAN_POINT('Ctrl Pts',(20.7102414995577,18.4443876011478,-4.35878402065841));
#98599=CARTESIAN_POINT('Ctrl Pts',(20.6407861833358,18.2891647883661,-4.36977755715366));
#98600=CARTESIAN_POINT('Ctrl Pts',(20.6126715314603,18.2331410343518,-4.37376458546057));
#98601=CARTESIAN_POINT('Ctrl Pts',(20.5637633782404,18.145603349821,-4.38001455570823));
#98602=CARTESIAN_POINT('Ctrl Pts',(20.5445429626296,18.1132575403375,-4.38232895660014));
#98603=CARTESIAN_POINT('Ctrl Pts',(20.5185082980585,18.0719899184099,-4.38529025175654));
#98604=CARTESIAN_POINT('Ctrl Pts',(20.512472055782,18.0625876236719,-4.38596554896999));
#98605=CARTESIAN_POINT('Ctrl Pts',(20.5025451948745,18.0473911350403,-4.38705811331711));
#98606=CARTESIAN_POINT('Ctrl Pts',(20.4986999221598,18.0415677088988,-4.38747706243136));
#98607=CARTESIAN_POINT('Ctrl Pts',(20.4912573891632,18.030416759211,-4.38827984590693));
#98608=CARTESIAN_POINT('Ctrl Pts',(20.487664526282,18.0250864066603,-4.38866383953559));
#98609=CARTESIAN_POINT('Ctrl Pts',(20.479393289368,18.0129350281893,-4.38953982885042));
#98610=CARTESIAN_POINT('Ctrl Pts',(20.4746990886027,18.0061248624226,-4.39003121841804));
#98611=CARTESIAN_POINT('Ctrl Pts',(20.462145872562,17.9881396307921,-4.39133026000814));
#98612=CARTESIAN_POINT('Ctrl Pts',(20.4542183099843,17.9770127154291,-4.39213529052361));
#98613=CARTESIAN_POINT('Ctrl Pts',(20.3944973525776,17.894884035786,-4.39808918978787));
#98614=CARTESIAN_POINT('Ctrl Pts',(20.3384320159953,17.8270876937509,-4.40306565206366));
#98615=CARTESIAN_POINT('Ctrl Pts',(20.1821105229613,17.6603728977585,-4.41573245651121));
#98616=CARTESIAN_POINT('Ctrl Pts',(20.0759332990415,17.5676248728425,-4.42321230087426));
#98617=CARTESIAN_POINT('Ctrl Pts',(19.9155053660955,17.4534734912241,-4.43408033940308));
#98618=CARTESIAN_POINT('Ctrl Pts',(19.8683851125068,17.4226980431254,-4.4372302225456));
#98619=CARTESIAN_POINT('Ctrl Pts',(19.7953661861868,17.3790553924104,-4.44213516135802));
#98620=CARTESIAN_POINT('Ctrl Pts',(19.7703356638665,17.3647802318397,-4.44382064940801));
#98621=CARTESIAN_POINT('Ctrl Pts',(19.7388996908033,17.347692675444,-4.44595232855252));
#98622=CARTESIAN_POINT('Ctrl Pts',(19.7327600182035,17.3443945255417,-4.44636935391955));
#98623=CARTESIAN_POINT('Ctrl Pts',(19.7230269849404,17.3392278380903,-4.44703172217683));
#98624=CARTESIAN_POINT('Ctrl Pts',(19.7194442929704,17.3373391587965,-4.44727580810125));
#98625=CARTESIAN_POINT('Ctrl Pts',(19.7126825838023,17.3337993627254,-4.44773702893828));
#98626=CARTESIAN_POINT('Ctrl Pts',(19.7095047877348,17.3321460299382,-4.44795402099435));
#98627=CARTESIAN_POINT('Ctrl Pts',(19.702236843303,17.3283880978882,-4.44845082138741));
#98628=CARTESIAN_POINT('Ctrl Pts',(19.6981440273503,17.326288761559,-4.44873095591609));
#98629=CARTESIAN_POINT('Ctrl Pts',(19.6872745368124,17.3207581226272,-4.44947583675153));
#98630=CARTESIAN_POINT('Ctrl Pts',(19.6804862522674,17.3173499616336,-4.44994197293745));
#98631=CARTESIAN_POINT('Ctrl Pts',(19.6332336414111,17.2939436231039,-4.45319243317525));
#98632=CARTESIAN_POINT('Ctrl Pts',(19.5921601536008,17.2752090031939,-4.45604673137148));
#98633=CARTESIAN_POINT('Ctrl Pts',(19.5449269394488,17.2554634273718,-4.45933637506048));
#98634=CARTESIAN_POINT('Ctrl Pts',(19.5393209490136,17.2531481271879,-4.45972693248499));
#98635=CARTESIAN_POINT('Ctrl Pts',(19.387862631515,17.1913557007781,-4.4702805362724));
#98636=CARTESIAN_POINT('Ctrl Pts',(19.2358348502079,17.148316087859,-4.48087220131182));
#98637=CARTESIAN_POINT('Ctrl Pts',(18.978823441679,17.1056831256988,-4.49778517428951));
#98638=CARTESIAN_POINT('Ctrl Pts',(18.8761078637002,17.096263969277,-4.50430452206001));
#98639=CARTESIAN_POINT('Ctrl Pts',(18.7582955570908,17.0940876284215,-4.51149025665462));
#98640=CARTESIAN_POINT('Ctrl Pts',(18.7434878028228,17.0939694706699,-4.51238838544493));
#98641=CARTESIAN_POINT('Ctrl Pts',(18.7209110826764,17.0940262088427,-4.51375028545251));
#98642=CARTESIAN_POINT('Ctrl Pts',(18.7131425261603,17.0940884948827,-4.51421756807006));
#98643=CARTESIAN_POINT('Ctrl Pts',(18.699013597531,17.0942795605143,-4.51506504378658));
#98644=CARTESIAN_POINT('Ctrl Pts',(18.692653155287,17.0943942485446,-4.515445673544));
#98645=CARTESIAN_POINT('Ctrl Pts',(18.6789275077052,17.0947036354405,-4.51626520199385));
#98646=CARTESIAN_POINT('Ctrl Pts',(18.6715625897929,17.0949081177874,-4.51670378934812));
#98647=CARTESIAN_POINT('Ctrl Pts',(18.6516069464671,17.0955664481011,-4.51788911792633));
#98648=CARTESIAN_POINT('Ctrl Pts',(18.6390188360181,17.0960942534991,-4.51863353825995));
#98649=CARTESIAN_POINT('Ctrl Pts',(18.5779507759758,17.0992011129832,-4.52222980213252));
#98650=CARTESIAN_POINT('Ctrl Pts',(18.5295623668543,17.1033350158927,-4.52503267155569));
#98651=CARTESIAN_POINT('Ctrl Pts',(18.4408421035346,17.1139991568736,-4.53011151238128));
#98652=CARTESIAN_POINT('Ctrl Pts',(18.4004761606625,17.1200394114944,-4.53239919674766));
#98653=CARTESIAN_POINT('Ctrl Pts',(18.227968545886,17.1509761437617,-4.54212597035447));
#98654=CARTESIAN_POINT('Ctrl Pts',(18.098194736733,17.1872616053873,-4.54929580651753));
#98655=CARTESIAN_POINT('Ctrl Pts',(17.9142086261841,17.258164688025,-4.56013212125728));
#98656=CARTESIAN_POINT('Ctrl Pts',(17.8567132255139,17.2833095637553,-4.56362566858367));
#98657=CARTESIAN_POINT('Ctrl Pts',(17.7726608238646,17.3246085167745,-4.56901239852279));
#98658=CARTESIAN_POINT('Ctrl Pts',(17.7452021941251,17.3388556381815,-4.57081878414247));
#98659=CARTESIAN_POINT('Ctrl Pts',(17.7118128689337,17.3571193971365,-4.57308535888627));
#98660=CARTESIAN_POINT('Ctrl Pts',(17.7055759509998,17.3605719974185,-4.57351180114141));
#98661=CARTESIAN_POINT('Ctrl Pts',(17.6957925319521,17.366052590725,-4.5741857479662));
#98662=CARTESIAN_POINT('Ctrl Pts',(17.6922341938586,17.3680594979201,-4.57443192022489));
#98663=CARTESIAN_POINT('Ctrl Pts',(17.6855723082155,17.3718422686238,-4.5748948167894));
#98664=CARTESIAN_POINT('Ctrl Pts',(17.6824674432624,17.3736156996364,-4.5751113848455));
#98665=CARTESIAN_POINT('Ctrl Pts',(17.675361824098,17.3776981835285,-4.57560890163939));
#98666=CARTESIAN_POINT('Ctrl Pts',(17.6713641360052,17.3800124638946,-4.57589018517003));
#98667=CARTESIAN_POINT('Ctrl Pts',(17.6590006650335,17.3872238628522,-4.57676429174669));
#98668=CARTESIAN_POINT('Ctrl Pts',(17.6506610583673,17.3921652911963,-4.57735987974959));
#98669=CARTESIAN_POINT('Ctrl Pts',(17.5601869776788,17.4466164563788,-4.58388406151157));
#98670=CARTESIAN_POINT('Ctrl Pts',(17.4814826859414,17.5015900641994,-4.59012179372017));
#98671=CARTESIAN_POINT('Ctrl Pts',(17.308064530617,17.6411421040318,-4.604774816402));
#98672=CARTESIAN_POINT('Ctrl Pts',(17.2166673270677,17.7292942996406,-4.61320495666886));
#98673=CARTESIAN_POINT('Ctrl Pts',(17.0955488135574,17.8691493858251,-4.62512680547077));
#98674=CARTESIAN_POINT('Ctrl Pts',(17.0592295958338,17.9147629789104,-4.62882514702687));
#98675=CARTESIAN_POINT('Ctrl Pts',(17.0037574688616,17.9906615633833,-4.63467551381041));
#98676=CARTESIAN_POINT('Ctrl Pts',(16.983410959526,18.0200325898984,-4.63687121838472));
#98677=CARTESIAN_POINT('Ctrl Pts',(16.9578007194851,18.0590775099832,-4.6397042674692));
#98678=CARTESIAN_POINT('Ctrl Pts',(16.9518562191603,18.068295813163,-4.640367061492));
#98679=CARTESIAN_POINT('Ctrl Pts',(16.9422715080927,18.0834158210239,-4.64144444340265));
#98680=CARTESIAN_POINT('Ctrl Pts',(16.9385882291837,18.0892898572344,-4.64186062706176));
#98681=CARTESIAN_POINT('Ctrl Pts',(16.9315377437401,18.1006575615209,-4.64266152292562));
#98682=CARTESIAN_POINT('Ctrl Pts',(16.9281666356074,18.1061487080187,-4.64304637612918));
#98683=CARTESIAN_POINT('Ctrl Pts',(16.9204736954179,18.11880889329,-4.6439290981769));
#98684=CARTESIAN_POINT('Ctrl Pts',(16.9161691912069,18.1259883757944,-4.64442632840094));
#98685=CARTESIAN_POINT('Ctrl Pts',(16.9047787772147,18.1452445090098,-4.64575114876464));
#98686=CARTESIAN_POINT('Ctrl Pts',(16.8977698294048,18.157366371503,-4.64657594628487));
#98687=CARTESIAN_POINT('Ctrl Pts',(16.8410107609327,18.2578170897637,-4.65333770409752));
#98688=CARTESIAN_POINT('Ctrl Pts',(16.7975405588004,18.3495508932622,-4.65904108803465));
#98689=CARTESIAN_POINT('Ctrl Pts',(16.7555368256109,18.4576181896615,-4.66542626409794));
#98690=CARTESIAN_POINT('Ctrl Pts',(16.7504072005036,18.4712297160127,-4.6662248549002));
#98691=CARTESIAN_POINT('Ctrl Pts',(16.7454194645813,18.4848895027932,-4.66702131702538));
#98692=CARTESIAN_POINT('',(16.6170000029932,19.2108919596605,-3.68920542541543));
#98693=CARTESIAN_POINT('Ctrl Pts',(16.7454194484637,18.4848895469342,-4.44630497835508));
#98694=CARTESIAN_POINT('Ctrl Pts',(16.7620249656267,18.4394124320693,-4.44325057557546));
#98695=CARTESIAN_POINT('Ctrl Pts',(16.7801860430651,18.3945172195639,-4.44012925146104));
#98696=CARTESIAN_POINT('Ctrl Pts',(16.8760920383706,18.1790053847587,-4.42474708365561));
#98697=CARTESIAN_POINT('Ctrl Pts',(16.9747456858919,18.0185744946775,-4.41214842973718));
#98698=CARTESIAN_POINT('Ctrl Pts',(17.1286539258257,17.8298074633418,-4.39674509051351));
#98699=CARTESIAN_POINT('Ctrl Pts',(17.1657754124566,17.7877988861886,-4.39326452647925));
#98700=CARTESIAN_POINT('Ctrl Pts',(17.2128424242685,17.7386164181891,-4.38912059089443));
#98701=CARTESIAN_POINT('Ctrl Pts',(17.2212358030051,17.7299941675128,-4.38839135421871));
#98702=CARTESIAN_POINT('Ctrl Pts',(17.2352366312937,17.7158547796949,-4.38719075325615));
#98703=CARTESIAN_POINT('Ctrl Pts',(17.2408020484296,17.7102965831959,-4.38671755965911));
#98704=CARTESIAN_POINT('Ctrl Pts',(17.2509287316874,17.700295145678,-4.3858637871393));
#98705=CARTESIAN_POINT('Ctrl Pts',(17.2554792919944,17.6958412422664,-4.38548273971838));
#98706=CARTESIAN_POINT('Ctrl Pts',(17.2652853260212,17.6863297393664,-4.38466714671523));
#98707=CARTESIAN_POINT('Ctrl Pts',(17.2705469932532,17.6812786213472,-4.38423288667315));
#98708=CARTESIAN_POINT('Ctrl Pts',(17.2849676783071,17.6675774925376,-4.38305175984437));
#98709=CARTESIAN_POINT('Ctrl Pts',(17.2941780629657,17.6589817959136,-4.38230723793986));
#98710=CARTESIAN_POINT('Ctrl Pts',(17.3433130964687,17.6139398315135,-4.37838616825592));
#98711=CARTESIAN_POINT('Ctrl Pts',(17.384548059278,17.5789487052456,-4.37527146450083));
#98712=CARTESIAN_POINT('Ctrl Pts',(17.5775417212019,17.4274997805049,-4.36137520083457));
#98713=CARTESIAN_POINT('Ctrl Pts',(17.7432942790343,17.3303710424829,-4.3513511588659));
#98714=CARTESIAN_POINT('Ctrl Pts',(17.9351029415774,17.2504576574925,-4.33980018026887));
#98715=CARTESIAN_POINT('Ctrl Pts',(17.9504506366743,17.2442734908208,-4.33887557450857));
#98716=CARTESIAN_POINT('Ctrl Pts',(18.0154339535036,17.2189706350912,-4.33495322615693));
#98717=CARTESIAN_POINT('Ctrl Pts',(18.0657043652678,17.201547814133,-4.3319007851306));
#98718=CARTESIAN_POINT('Ctrl Pts',(18.1249045926734,17.1834971859942,-4.32822792186033));
#98719=CARTESIAN_POINT('Ctrl Pts',(18.1332520143669,17.1810081951184,-4.32770825126156));
#98720=CARTESIAN_POINT('Ctrl Pts',(18.1459165545096,17.1773169022518,-4.32691678638023));
#98721=CARTESIAN_POINT('Ctrl Pts',(18.1502226383851,17.1760766421942,-4.32664715077164));
#98722=CARTESIAN_POINT('Ctrl Pts',(18.1579603176427,17.1738745779117,-4.32616163556875));
#98723=CARTESIAN_POINT('Ctrl Pts',(18.1613904299153,17.1729077594677,-4.32594605136858));
#98724=CARTESIAN_POINT('Ctrl Pts',(18.1688504977366,17.1708253690799,-4.32547639907788));
#98725=CARTESIAN_POINT('Ctrl Pts',(18.1728812693288,17.1697130887721,-4.3252221491604));
#98726=CARTESIAN_POINT('Ctrl Pts',(18.1842164963819,17.1666212745397,-4.32450582909725));
#98727=CARTESIAN_POINT('Ctrl Pts',(18.1915282239849,17.1646689802918,-4.32404222692731));
#98728=CARTESIAN_POINT('Ctrl Pts',(18.2353814299639,17.1532113429672,-4.32125312542023));
#98729=CARTESIAN_POINT('Ctrl Pts',(18.2721590049323,17.1446464187521,-4.31887852361217));
#98730=CARTESIAN_POINT('Ctrl Pts',(18.3941221173814,17.1196615511405,-4.31093048639852));
#98731=CARTESIAN_POINT('Ctrl Pts',(18.4800854786699,17.1074936442186,-4.30521497620494));
#98732=CARTESIAN_POINT('Ctrl Pts',(18.7418157171605,17.0867258582925,-4.28786815532137));
#98733=CARTESIAN_POINT('Ctrl Pts',(18.9181716279832,17.0947046239889,-4.27632337620133));
#98734=CARTESIAN_POINT('Ctrl Pts',(19.1141662431538,17.1282878346254,-4.26408405820796));
#98735=CARTESIAN_POINT('Ctrl Pts',(19.1367362449317,17.1325342392916,-4.26268222168468));
#98736=CARTESIAN_POINT('Ctrl Pts',(19.1685805826328,17.1390637654035,-4.26071444352681));
#98737=CARTESIAN_POINT('Ctrl Pts',(19.1779148116963,17.1410435541648,-4.26013887850158));
#98738=CARTESIAN_POINT('Ctrl Pts',(19.1930631128783,17.1443636867127,-4.2592067284491));
#98739=CARTESIAN_POINT('Ctrl Pts',(19.1988853884152,17.1456656034013,-4.25884891751254));
#98740=CARTESIAN_POINT('Ctrl Pts',(19.2110640073146,17.1484429677316,-4.25810141360815));
#98741=CARTESIAN_POINT('Ctrl Pts',(19.2174191975524,17.1499232281783,-4.25771187956592));
#98742=CARTESIAN_POINT('Ctrl Pts',(19.2325268223556,17.1535158391959,-4.25678710590187));
#98743=CARTESIAN_POINT('Ctrl Pts',(19.2412728705851,17.1556546997766,-4.25625272542227));
#98744=CARTESIAN_POINT('Ctrl Pts',(19.2707158970647,17.1630544256209,-4.25445689210552));
#98745=CARTESIAN_POINT('Ctrl Pts',(19.2913472681243,17.1685727426381,-4.2532037504682));
#98746=CARTESIAN_POINT('Ctrl Pts',(19.4033610469702,17.2003570717855,-4.24642344852745));
#98747=CARTESIAN_POINT('Ctrl Pts',(19.4929830863256,17.2324457495615,-4.24109060896725));
#98748=CARTESIAN_POINT('Ctrl Pts',(19.7363290492884,17.3385540063705,-4.22648541345346));
#98749=CARTESIAN_POINT('Ctrl Pts',(19.88369455115,17.4252486076997,-4.21752248432758));
#98750=CARTESIAN_POINT('Ctrl Pts',(20.0485716662607,17.5511900349048,-4.20567642017467));
#98751=CARTESIAN_POINT('Ctrl Pts',(20.0774798263531,17.5745008812832,-4.20352010454318));
#98752=CARTESIAN_POINT('Ctrl Pts',(20.1112138078694,17.6031995039757,-4.2008871101654));
#98753=CARTESIAN_POINT('Ctrl Pts',(20.1166458737412,17.6078684732283,-4.20045940457657));
#98754=CARTESIAN_POINT('Ctrl Pts',(20.1254659337047,17.615527664116,-4.19975863979839));
#98755=CARTESIAN_POINT('Ctrl Pts',(20.1288682832835,17.6185013687127,-4.19948677509155));
#98756=CARTESIAN_POINT('Ctrl Pts',(20.1349389071423,17.6238415647845,-4.19899887720807));
#98757=CARTESIAN_POINT('Ctrl Pts',(20.1376107447251,17.6262039257234,-4.19878315211469));
#98758=CARTESIAN_POINT('Ctrl Pts',(20.1433811713299,17.6313320083437,-4.19831508772185));
#98759=CARTESIAN_POINT('Ctrl Pts',(20.1464775521571,17.6341000621692,-4.19806257687245));
#98760=CARTESIAN_POINT('Ctrl Pts',(20.155096855643,17.6418511668158,-4.19735594333158));
#98761=CARTESIAN_POINT('Ctrl Pts',(20.160601626241,17.6468541851759,-4.19690035309468));
#98762=CARTESIAN_POINT('Ctrl Pts',(20.1922823378131,17.6759536021983,-4.19425401833392));
#98763=CARTESIAN_POINT('Ctrl Pts',(20.2178722324698,17.7006763021852,-4.19201972357592));
#98764=CARTESIAN_POINT('Ctrl Pts',(20.2978737025376,17.7819629654504,-4.18475230362379));
#98765=CARTESIAN_POINT('Ctrl Pts',(20.3497657938878,17.8409098421037,-4.17960085634584));
#98766=CARTESIAN_POINT('Ctrl Pts',(20.5145155982759,18.0504681821764,-4.16200639681164));
#98767=CARTESIAN_POINT('Ctrl Pts',(20.6105696632863,18.2132099644645,-4.14960154753646));
#98768=CARTESIAN_POINT('Ctrl Pts',(20.6923613731792,18.4066450944228,-4.13668937275581));
#98769=CARTESIAN_POINT('Ctrl Pts',(20.7005562747561,18.4268937849937,-4.13535698179561));
#98770=CARTESIAN_POINT('Ctrl Pts',(20.7114731241142,18.4551164841424,-4.13352578843577));
#98771=CARTESIAN_POINT('Ctrl Pts',(20.7144628545145,18.4629848054826,-4.13301801878129));
#98772=CARTESIAN_POINT('Ctrl Pts',(20.7195266870702,18.476554915179,-4.13214696532309));
#98773=CARTESIAN_POINT('Ctrl Pts',(20.7216233343735,18.482248128969,-4.13178293017799));
#98774=CARTESIAN_POINT('Ctrl Pts',(20.7259001319133,18.4940170641886,-4.13103327082618));
#98775=CARTESIAN_POINT('Ctrl Pts',(20.7280770281984,18.5000939071883,-4.13064775833854));
#98776=CARTESIAN_POINT('Ctrl Pts',(20.733086308776,18.5142814531294,-4.12975131614767));
#98777=CARTESIAN_POINT('Ctrl Pts',(20.7358971970614,18.522399666566,-4.12924110468477));
#98778=CARTESIAN_POINT('Ctrl Pts',(20.7447680635358,18.548533347581,-4.12760727508147));
#98779=CARTESIAN_POINT('Ctrl Pts',(20.7506349745345,18.5666137142693,-4.1264900305016));
#98780=CARTESIAN_POINT('Ctrl Pts',(20.7788920163266,18.6578631287926,-4.120913651131));
#98781=CARTESIAN_POINT('Ctrl Pts',(20.7975483763162,18.732132953823,-4.11657752005548));
#98782=CARTESIAN_POINT('Ctrl Pts',(20.8330984319958,18.9151157095607,-4.10621809926495));
#98783=CARTESIAN_POINT('Ctrl Pts',(20.8456247103672,19.0244426514256,-4.1003042143357));
#98784=CARTESIAN_POINT('Ctrl Pts',(20.8521450700533,19.20417631853,-4.09050918107038));
#98785=CARTESIAN_POINT('Ctrl Pts',(20.8512132815947,19.2741813194231,-4.08667312437598));
#98786=CARTESIAN_POINT('Ctrl Pts',(20.8437778763291,19.3922927393893,-4.07998901581291));
#98787=CARTESIAN_POINT('Ctrl Pts',(20.8390840555645,19.4404560576827,-4.07720291383589));
#98788=CARTESIAN_POINT('Ctrl Pts',(20.8317294531977,19.4960968759273,-4.07387081254261));
#98789=CARTESIAN_POINT('Ctrl Pts',(20.830671497921,19.5037758752394,-4.07340842477671));
#98790=CARTESIAN_POINT('Ctrl Pts',(20.828912092067,19.5160473874809,-4.07266521383919));
#98791=CARTESIAN_POINT('Ctrl Pts',(20.8282376436474,19.5206437841873,-4.07238587442976));
#98792=CARTESIAN_POINT('Ctrl Pts',(20.8270154825512,19.5287861923158,-4.0718892636066));
#98793=CARTESIAN_POINT('Ctrl Pts',(20.8264738777351,19.532333074951,-4.07167234005033));
#98794=CARTESIAN_POINT('Ctrl Pts',(20.8253058135114,19.5398543477503,-4.07121105941479));
#98795=CARTESIAN_POINT('Ctrl Pts',(20.8246770502732,19.543828271783,-4.07096657960802));
#98796=CARTESIAN_POINT('Ctrl Pts',(20.8229472865175,19.554562436088,-4.07030419714244));
#98797=CARTESIAN_POINT('Ctrl Pts',(20.8218248108308,19.5613190969023,-4.06988510580349));
#98798=CARTESIAN_POINT('Ctrl Pts',(20.8160616767009,19.5949980782503,-4.06778578079572));
#98799=CARTESIAN_POINT('Ctrl Pts',(20.810933198114,19.6218329052306,-4.0660800940292));
#98800=CARTESIAN_POINT('Ctrl Pts',(20.7945516614194,19.6993786360622,-4.06106963058264));
#98801=CARTESIAN_POINT('Ctrl Pts',(20.7819501487824,19.7497822407039,-4.05771129351724));
#98802=CARTESIAN_POINT('Ctrl Pts',(20.728915616357,19.932986079694,-4.04524289270576));
#98803=CARTESIAN_POINT('Ctrl Pts',(20.6773010160004,20.0621977215373,-4.03596170781975));
#98804=CARTESIAN_POINT('Ctrl Pts',(20.5694994528494,20.2701183092783,-4.02080213828596));
#98805=CARTESIAN_POINT('Ctrl Pts',(20.5199100817507,20.3517538662043,-4.01477697040225));
#98806=CARTESIAN_POINT('Ctrl Pts',(20.45699767181,20.441105702491,-4.00810821764091));
#98807=CARTESIAN_POINT('Ctrl Pts',(20.4489088808851,20.4523575475894,-4.00726685070598));
#98808=CARTESIAN_POINT('Ctrl Pts',(20.4357824552206,20.4702437568369,-4.00592662479235));
#98809=CARTESIAN_POINT('Ctrl Pts',(20.4308152354769,20.4769290753352,-4.00542505943387));
#98810=CARTESIAN_POINT('Ctrl Pts',(20.4219393547239,20.4887289094744,-4.00453859377909));
#98811=CARTESIAN_POINT('Ctrl Pts',(20.4180466000976,20.4938552067366,-4.00415307848769));
#98812=CARTESIAN_POINT('Ctrl Pts',(20.4099010132332,20.5044810098667,-4.0033531060857));
#98813=CARTESIAN_POINT('Ctrl Pts',(20.4056443449131,20.5099774882321,-4.00293880665209));
#98814=CARTESIAN_POINT('Ctrl Pts',(20.3945498387777,20.5241585614896,-4.0018685547175));
#98815=CARTESIAN_POINT('Ctrl Pts',(20.3876708670395,20.5328108205002,-4.00121424552423));
#98816=CARTESIAN_POINT('Ctrl Pts',(20.3577877663349,20.5697988685039,-3.99841088458837));
#98817=CARTESIAN_POINT('Ctrl Pts',(20.3341199286135,20.5975920540963,-3.99628870474889));
#98818=CARTESIAN_POINT('Ctrl Pts',(20.2696433376916,20.6694561365765,-3.99074445329885));
#98819=CARTESIAN_POINT('Ctrl Pts',(20.227657142821,20.7124272886774,-3.98737030902173));
#98820=CARTESIAN_POINT('Ctrl Pts',(20.0622964968734,20.8678549193019,-3.97479975202564));
#98821=CARTESIAN_POINT('Ctrl Pts',(19.927618280039,20.9673620826633,-3.96601316266627));
#98822=CARTESIAN_POINT('Ctrl Pts',(19.7353992324203,21.0769713672813,-3.95357996357705));
#98823=CARTESIAN_POINT('Ctrl Pts',(19.6871154652365,21.1020894746051,-3.9504601531847));
#98824=CARTESIAN_POINT('Ctrl Pts',(19.6300004002602,21.1290586639559,-3.94671222584627));
#98825=CARTESIAN_POINT('Ctrl Pts',(19.6220551633231,21.1327501857783,-3.94618958994098));
#98826=CARTESIAN_POINT('Ctrl Pts',(19.6100019587384,21.138259646859,-3.94539448762135));
#98827=CARTESIAN_POINT('Ctrl Pts',(19.6059106294689,21.1401140535201,-3.94512420967365));
#98828=CARTESIAN_POINT('Ctrl Pts',(19.5985621659807,21.1434166132796,-3.94463801075401));
#98829=CARTESIAN_POINT('Ctrl Pts',(19.5953072507833,21.1448695730536,-3.9444223888364));
#98830=CARTESIAN_POINT('Ctrl Pts',(19.5882336157606,21.1480057679612,-3.94395320716877));
#98831=CARTESIAN_POINT('Ctrl Pts',(19.5844136345005,21.1496859118929,-3.94369946860464));
#98832=CARTESIAN_POINT('Ctrl Pts',(19.5736871819762,21.1543659293477,-3.94298600125315));
#98833=CARTESIAN_POINT('Ctrl Pts',(19.5667697172808,21.1573402305329,-3.94252475956089));
#98834=CARTESIAN_POINT('Ctrl Pts',(19.5256767420092,21.1747498014775,-3.93977873585652));
#98835=CARTESIAN_POINT('Ctrl Pts',(19.4911446417989,21.1883206491528,-3.93744656293871));
#98836=CARTESIAN_POINT('Ctrl Pts',(19.3771474976469,21.2296967447004,-3.92970862206491));
#98837=CARTESIAN_POINT('Ctrl Pts',(19.2963809359632,21.2536700894198,-3.92416829951151));
#98838=CARTESIAN_POINT('Ctrl Pts',(19.0395605479547,21.31351114945,-3.90674952948735));
#98839=CARTESIAN_POINT('Ctrl Pts',(18.8602027372249,21.3318532059096,-3.8949453656144));
#98840=CARTESIAN_POINT('Ctrl Pts',(18.6579996993966,21.3267567728553,-3.88249941011351));
#98841=CARTESIAN_POINT('Ctrl Pts',(18.6353504317566,21.325821763873,-3.88111599049576));
#98842=CARTESIAN_POINT('Ctrl Pts',(18.6032427359117,21.3239793300108,-3.87916934217481));
#98843=CARTESIAN_POINT('Ctrl Pts',(18.5937692830264,21.3233717622078,-3.87859676825141));
#98844=CARTESIAN_POINT('Ctrl Pts',(18.5783578798885,21.3222792373476,-3.87766813725326));
#98845=CARTESIAN_POINT('Ctrl Pts',(18.5724174028572,21.3218329050486,-3.87731087257365));
#98846=CARTESIAN_POINT('Ctrl Pts',(18.5599662039822,21.3208445249716,-3.87656345565097));
#98847=CARTESIAN_POINT('Ctrl Pts',(18.553455939165,21.3202974008616,-3.87617346696461));
#98848=CARTESIAN_POINT('Ctrl Pts',(18.5379367816161,21.3189207907336,-3.87524568980076));
#98849=CARTESIAN_POINT('Ctrl Pts',(18.5289304209558,21.3180636718499,-3.87470877550605));
#98850=CARTESIAN_POINT('Ctrl Pts',(18.4984286699317,21.3149634549216,-3.87289532596846));
#98851=CARTESIAN_POINT('Ctrl Pts',(18.4769617861304,21.3124488998514,-3.87162732920009));
#98852=CARTESIAN_POINT('Ctrl Pts',(18.3591357262543,21.2968145935176,-3.86470776720767));
#98853=CARTESIAN_POINT('Ctrl Pts',(18.263724968455,21.2773954969086,-3.8592599985852));
#98854=CARTESIAN_POINT('Ctrl Pts',(18.0202879377967,21.2101056222789,-3.84537888154959));
#98855=CARTESIAN_POINT('Ctrl Pts',(17.8756193290227,21.1523869789401,-3.83716565171484));
#98856=CARTESIAN_POINT('Ctrl Pts',(17.6957476336115,21.0565557328634,-3.82565615901801));
#98857=CARTESIAN_POINT('Ctrl Pts',(17.6537198992097,21.0322737453101,-3.82286191755898));
#98858=CARTESIAN_POINT('Ctrl Pts',(17.6054139183755,21.0021040126113,-3.81948067198155));
#98859=CARTESIAN_POINT('Ctrl Pts',(17.5982876030213,20.9975938188672,-3.81897739486701));
#98860=CARTESIAN_POINT('Ctrl Pts',(17.5875083648538,20.9906811636917,-3.81820903904099));
#98861=CARTESIAN_POINT('Ctrl Pts',(17.5838355254244,20.9883097069714,-3.8179459734449));
#98862=CARTESIAN_POINT('Ctrl Pts',(17.5773397178244,20.984086965744,-3.81747842453225));
#98863=CARTESIAN_POINT('Ctrl Pts',(17.5745138062785,20.9822402894084,-3.81727425011606));
#98864=CARTESIAN_POINT('Ctrl Pts',(17.5716708396979,20.9803727486796,-3.81706805653115));
#98865=CARTESIAN_POINT('Ctrl Pts',(17.5716493924919,20.980358659482,-3.81706650097145));
#98866=CARTESIAN_POINT('Ctrl Pts',(17.5716069177775,20.9803307556911,-3.81706342020347));
#98867=CARTESIAN_POINT('Ctrl Pts',(17.5715858903259,20.9803169411565,-3.81706189500105));
#98868=CARTESIAN_POINT('Ctrl Pts',(17.5715442301954,20.9802895703806,-3.81705887314492));
#98869=CARTESIAN_POINT('Ctrl Pts',(17.5715235974604,20.9802760141222,-3.81705737648873));
#98870=CARTESIAN_POINT('Ctrl Pts',(17.5714827032911,20.9802491445358,-3.8170544100272));
#98871=CARTESIAN_POINT('Ctrl Pts',(17.5714624419069,20.980235831259,-3.81705294022697));
#98872=CARTESIAN_POINT('Ctrl Pts',(17.5714222691765,20.9802094337192,-3.81705002593934));
#98873=CARTESIAN_POINT('Ctrl Pts',(17.5714023576909,20.9801963493816,-3.81704858144319));
#98874=CARTESIAN_POINT('Ctrl Pts',(17.5713628642758,20.9801703963112,-3.81704571628188));
#98875=CARTESIAN_POINT('Ctrl Pts',(17.5713432824778,20.9801575276808,-3.81704429562755));
#98876=CARTESIAN_POINT('Ctrl Pts',(17.5713044297303,20.9801319937775,-3.81704147679644));
#98877=CARTESIAN_POINT('Ctrl Pts',(17.5712851588656,20.980119328575,-3.817040078627));
#98878=CARTESIAN_POINT('Ctrl Pts',(17.5712469104831,20.9800941900686,-3.81703730349935));
#98879=CARTESIAN_POINT('Ctrl Pts',(17.5712279329782,20.9800817167869,-3.81703592654319));
#98880=CARTESIAN_POINT('Ctrl Pts',(17.5711902553968,20.9800569516996,-3.81703319269038));
#98881=CARTESIAN_POINT('Ctrl Pts',(17.5711715550792,20.9800446597483,-3.81703183577725));
#98882=CARTESIAN_POINT('Ctrl Pts',(17.5711344159396,20.9800202468866,-3.81702914085743));
#98883=CARTESIAN_POINT('Ctrl Pts',(17.5711159772758,20.980008126092,-3.81702780286318));
#98884=CARTESIAN_POINT('Ctrl Pts',(17.5710793469747,20.9799840460674,-3.81702514473397));
#98885=CARTESIAN_POINT('Ctrl Pts',(17.5710611554,20.9799720868896,-3.81702382460445));
#98886=CARTESIAN_POINT('Ctrl Pts',(17.5710250065701,20.9799483217773,-3.81702120128523));
#98887=CARTESIAN_POINT('Ctrl Pts',(17.5710070488909,20.9799365155744,-3.81701989806558));
#98888=CARTESIAN_POINT('Ctrl Pts',(17.5709713539729,20.9799130473178,-3.81701730756133));
#98889=CARTESIAN_POINT('Ctrl Pts',(17.5709536169827,20.979901385437,-3.81701602029553));
#98890=CARTESIAN_POINT('Ctrl Pts',(17.5709183522129,20.9798781984695,-3.81701346088627));
#98891=CARTESIAN_POINT('Ctrl Pts',(17.5709008241268,20.9798666731902,-3.81701218872128));
#98892=CARTESIAN_POINT('Ctrl Pts',(17.5708659653909,20.9798437517102,-3.81700965866119));
#98893=CARTESIAN_POINT('Ctrl Pts',(17.5708486347621,20.9798323555316,-3.8170084007683));
#98894=CARTESIAN_POINT('Ctrl Pts',(17.5708141596542,20.9798096848559,-3.8170058984352));
#98895=CARTESIAN_POINT('Ctrl Pts',(17.5707970154369,20.9797984105388,-3.81700465401463));
#98896=CARTESIAN_POINT('Ctrl Pts',(17.5707629036413,20.9797759773548,-3.81700217793771));
#98897=CARTESIAN_POINT('Ctrl Pts',(17.5707459358579,20.9797648183603,-3.81700094626705));
#98898=CARTESIAN_POINT('Ctrl Pts',(17.5707121667196,20.9797426091284,-3.81699849495055));
#98899=CARTESIAN_POINT('Ctrl Pts',(17.5706953655069,20.9797315589912,-3.81699727531558));
#98900=CARTESIAN_POINT('Ctrl Pts',(17.5706619203325,20.9797095614578,-3.81699484740584));
#98901=CARTESIAN_POINT('Ctrl Pts',(17.5706452764654,20.9796986141304,-3.81699363913847));
#98902=CARTESIAN_POINT('Ctrl Pts',(17.5706121369901,20.9796768163209,-3.81699123331268));
#98903=CARTESIAN_POINT('Ctrl Pts',(17.5705956415121,20.9796659659306,-3.81699003576421));
#98904=CARTESIAN_POINT('Ctrl Pts',(17.5705627911449,20.979644356968,-3.8169876508208));
#98905=CARTESIAN_POINT('Ctrl Pts',(17.5705464359826,20.9796335982216,-3.8169864634065));
#98906=CARTESIAN_POINT('Ctrl Pts',(17.5705138573104,20.979612166685,-3.816984098084));
#98907=CARTESIAN_POINT('Ctrl Pts',(17.5704976341029,20.9796014940989,-3.81698292019817));
#98908=CARTESIAN_POINT('Ctrl Pts',(17.5669721938763,20.9772821813513,-3.81672695004972));
#98909=CARTESIAN_POINT('Ctrl Pts',(17.5634698905235,20.9749631250476,-3.81647145549824));
#98910=CARTESIAN_POINT('Ctrl Pts',(17.5533724216286,20.968233754693,-3.81573140954562));
#98911=CARTESIAN_POINT('Ctrl Pts',(17.5467952015199,20.9637968248909,-3.8152451176077));
#98912=CARTESIAN_POINT('Ctrl Pts',(17.5031594114367,20.9340022629206,-3.81199132894857));
#98913=CARTESIAN_POINT('Ctrl Pts',(17.4668935509768,20.9075099297967,-3.80915427221634));
#98914=CARTESIAN_POINT('Ctrl Pts',(17.3375093174381,20.8065307137936,-3.79861576237224));
#98915=CARTESIAN_POINT('Ctrl Pts',(17.2498869211711,20.7253682148947,-3.79066785675721));
#98916=CARTESIAN_POINT('Ctrl Pts',(17.0706999415654,20.528822475985,-3.77314902005174));
#98917=CARTESIAN_POINT('Ctrl Pts',(16.9833620424435,20.4103768616343,-3.7636919082579));
#98918=CARTESIAN_POINT('Ctrl Pts',(16.9017534031063,20.271549022565,-3.75385956517648));
#98919=CARTESIAN_POINT('Ctrl Pts',(16.8946602014013,20.2591989038074,-3.75299453283563));
#98920=CARTESIAN_POINT('Ctrl Pts',(16.8835622998991,20.2394165316241,-3.75162399002801));
#98921=CARTESIAN_POINT('Ctrl Pts',(16.8794765893048,20.2320304436593,-3.75111557640561));
#98922=CARTESIAN_POINT('Ctrl Pts',(16.8723447231156,20.2189535157891,-3.75022118303641));
#98923=CARTESIAN_POINT('Ctrl Pts',(16.8692802351493,20.213272847058,-3.74983455170444));
#98924=CARTESIAN_POINT('Ctrl Pts',(16.8629918195743,20.2014872791555,-3.74903629270852));
#98925=CARTESIAN_POINT('Ctrl Pts',(16.8597716754549,20.195380439971,-3.74862480281219));
#98926=CARTESIAN_POINT('Ctrl Pts',(16.8515748731151,20.1796495893643,-3.74757024385822));
#98927=CARTESIAN_POINT('Ctrl Pts',(16.846642079434,20.1700028527513,-3.74692872674609));
#98928=CARTESIAN_POINT('Ctrl Pts',(16.8262991591984,20.129454598265,-3.74425336103823));
#98929=CARTESIAN_POINT('Ctrl Pts',(16.8115716784683,20.0982152478476,-3.74224337432153));
#98930=CARTESIAN_POINT('Ctrl Pts',(16.7751408963554,20.0157681730833,-3.7370586361944));
#98931=CARTESIAN_POINT('Ctrl Pts',(16.7546789088779,19.9640401575799,-3.73392409547238));
#98932=CARTESIAN_POINT('Ctrl Pts',(16.7027485980965,19.8159559085773,-3.72520196171289));
#98933=CARTESIAN_POINT('Ctrl Pts',(16.676126623379,19.7180621230921,-3.71973258579423));
#98934=CARTESIAN_POINT('Ctrl Pts',(16.6333093437204,19.4998588572485,-3.70764141857151));
#98935=CARTESIAN_POINT('Ctrl Pts',(16.620235005192,19.3793155006776,-3.70102399953171));
#98936=CARTESIAN_POINT('Ctrl Pts',(16.6172719227627,19.2468288732992,-3.69321427594124));
#98937=CARTESIAN_POINT('Ctrl Pts',(16.6171084252312,19.2353209518181,-3.69253143385636));
#98938=CARTESIAN_POINT('Ctrl Pts',(16.6170172121696,19.2202502263473,-3.69163065589168));
#98939=CARTESIAN_POINT('Ctrl Pts',(16.6170046437703,19.2166878770101,-3.6914172562726));
#98940=CARTESIAN_POINT('Ctrl Pts',(16.6170002821712,19.2123438082719,-3.69115642739275));
#98941=CARTESIAN_POINT('Ctrl Pts',(16.6169999302848,19.2115620757113,-3.69110946645803));
#98942=CARTESIAN_POINT('Ctrl Pts',(16.6170000113955,19.2107803447323,-3.69106248172613));
#98943=CARTESIAN_POINT('Ctrl Pts',(16.6170000023184,19.210900923828,-3.6890562790225));
#98944=CARTESIAN_POINT('Ctrl Pts',(16.6170002492315,19.2056250329456,-3.68873698393553));
#98945=CARTESIAN_POINT('Ctrl Pts',(16.6170202186042,19.2003491960952,-3.68841768884857));
#98946=CARTESIAN_POINT('Ctrl Pts',(16.6170599094811,19.1950735078034,-3.6880983937616));
#98947=CARTESIAN_POINT('Ctrl Pts',(16.6176052825337,19.1225828384795,-3.68371111511931));
#98948=CARTESIAN_POINT('Ctrl Pts',(16.6218794874508,19.0499787438806,-3.67932383647702));
#98949=CARTESIAN_POINT('Ctrl Pts',(16.6298970753153,18.9776764428242,-3.67493655783472));
#98950=CARTESIAN_POINT('Ctrl Pts',(16.6379042320844,18.9054682089865,-3.67055498715876));
#98951=CARTESIAN_POINT('Ctrl Pts',(16.6496450608728,18.8335614651472,-3.66617341648279));
#98952=CARTESIAN_POINT('Ctrl Pts',(16.6650821233697,18.7623711781888,-3.66179184580682));
#98953=CARTESIAN_POINT('Ctrl Pts',(16.6805014135,18.6912628511164,-3.65741531954139));
#98954=CARTESIAN_POINT('Ctrl Pts',(16.699608383448,18.620869811639,-3.65303879327595));
#98955=CARTESIAN_POINT('Ctrl Pts',(16.7223140614303,18.5515997538967,-3.64866226701052));
#98956=CARTESIAN_POINT('Ctrl Pts',(16.7296427208095,18.5292416169249,-3.64724966570929));
#98957=CARTESIAN_POINT('Ctrl Pts',(16.7373458914714,18.5070003955267,-3.64583706440805));
#98958=CARTESIAN_POINT('Ctrl Pts',(16.7454194503191,18.4848895418526,-3.64442446310682));
#98959=CARTESIAN_POINT('Origin',(18.734,19.211,0.));
#98960=CARTESIAN_POINT('',(16.747777019274,18.4857290362168,-2.84456321874111));
#98961=CARTESIAN_POINT('',(16.7454194666968,18.4848894969994,-3.06515441818778));
#98962=CARTESIAN_POINT('',(16.7454194503191,18.4848895418526,0.));
#98963=CARTESIAN_POINT('Ctrl Pts',(16.7454194666968,18.4848894969994,-3.06515441818778));
#98964=CARTESIAN_POINT('Ctrl Pts',(16.6929878099064,18.6284827539369,-3.07512667887767));
#98965=CARTESIAN_POINT('Ctrl Pts',(16.6562469357021,18.7773756907385,-3.08537382465129));
#98966=CARTESIAN_POINT('Ctrl Pts',(16.6280919214672,18.9868385248522,-3.09899374936203));
#98967=CARTESIAN_POINT('Ctrl Pts',(16.6227108915773,19.0449985907553,-3.1026987833764));
#98968=CARTESIAN_POINT('Ctrl Pts',(16.6179213236954,19.1390322893946,-3.10855847142046));
#98969=CARTESIAN_POINT('Ctrl Pts',(16.6170073709064,19.1747954552044,-3.11075697795693));
#98970=CARTESIAN_POINT('Ctrl Pts',(16.6169977968628,19.2215398079568,-3.11359306368755));
#98971=CARTESIAN_POINT('Ctrl Pts',(16.6170808697603,19.2325132230707,-3.11425616031307));
#98972=CARTESIAN_POINT('Ctrl Pts',(16.617355670962,19.2504191432636,-3.1153339095973));
#98973=CARTESIAN_POINT('Ctrl Pts',(16.6174961453267,19.2573521244129,-3.11575016009385));
#98974=CARTESIAN_POINT('Ctrl Pts',(16.6178328490843,19.2707252061193,-3.11655110005955));
#98975=CARTESIAN_POINT('Ctrl Pts',(16.6180244187625,19.277165337481,-3.11693593097546));
#98976=CARTESIAN_POINT('Ctrl Pts',(16.6185373490306,19.2921125355497,-3.11782710282682));
#98977=CARTESIAN_POINT('Ctrl Pts',(16.6188806300209,19.3006187761529,-3.11833275166139));
#98978=CARTESIAN_POINT('Ctrl Pts',(16.6201365681075,19.3276865230197,-3.11993714976034));
#98979=CARTESIAN_POINT('Ctrl Pts',(16.6212423395125,19.3462385078596,-3.12102984838258));
#98980=CARTESIAN_POINT('Ctrl Pts',(16.6243860789557,19.3894039111221,-3.1235575311596));
#98981=CARTESIAN_POINT('Ctrl Pts',(16.6266107585169,19.4140012503967,-3.12498671235796));
#98982=CARTESIAN_POINT('Ctrl Pts',(16.6359173822974,19.500081504802,-3.12995531109658));
#98983=CARTESIAN_POINT('Ctrl Pts',(16.6452643348431,19.5612898374677,-3.13342814759911));
#98984=CARTESIAN_POINT('Ctrl Pts',(16.6848813491744,19.761466335755,-3.14471622121767));
#98985=CARTESIAN_POINT('Ctrl Pts',(16.7264585002196,19.8977860910206,-3.15226965910077));
#98986=CARTESIAN_POINT('Ctrl Pts',(16.8104677901499,20.0983446659418,-3.16430892628748));
#98987=CARTESIAN_POINT('Ctrl Pts',(16.843234173352,20.1661747264976,-3.16856359966033));
#98988=CARTESIAN_POINT('Ctrl Pts',(16.8841143625527,20.2404183467846,-3.17358676593651));
#98989=CARTESIAN_POINT('Ctrl Pts',(16.8887460408186,20.2486978475829,-3.17415226598364));
#98990=CARTESIAN_POINT('Ctrl Pts',(16.8956954201968,20.260926777631,-3.17499586404308));
#98991=CARTESIAN_POINT('Ctrl Pts',(16.8979706121172,20.2649003996768,-3.17527129619235));
#98992=CARTESIAN_POINT('Ctrl Pts',(16.9020434239784,20.2719603482061,-3.17576306214405));
#98993=CARTESIAN_POINT('Ctrl Pts',(16.9038359804333,20.2750495374494,-3.1759790676145));
#98994=CARTESIAN_POINT('Ctrl Pts',(16.9077088521027,20.2816850829863,-3.17644483962914));
#98995=CARTESIAN_POINT('Ctrl Pts',(16.9097916527238,20.2852298678033,-3.17669476225511));
#98996=CARTESIAN_POINT('Ctrl Pts',(16.9155744449446,20.2950064697784,-3.17738705526196));
#98997=CARTESIAN_POINT('Ctrl Pts',(16.9192960918719,20.3012253198887,-3.17783080001669));
#98998=CARTESIAN_POINT('Ctrl Pts',(16.9399457208506,20.3353320402637,-3.18028260193025));
#98999=CARTESIAN_POINT('Ctrl Pts',(16.9574836888723,20.362843226496,-3.18232719728519));
#99000=CARTESIAN_POINT('Ctrl Pts',(17.0662162861242,20.5250148758663,-3.1947350877816));
#99001=CARTESIAN_POINT('Ctrl Pts',(17.1720438520995,20.6492039298558,-3.20568688624845));
#99002=CARTESIAN_POINT('Ctrl Pts',(17.3764983259566,20.8396550051589,-3.22393798224768));
#99003=CARTESIAN_POINT('Ctrl Pts',(17.4684036692153,20.9120589788882,-3.23137710151106));
#99004=CARTESIAN_POINT('Ctrl Pts',(17.5777443358775,20.9844052032281,-3.23938255686668));
#99005=CARTESIAN_POINT('Ctrl Pts',(17.5897407225571,20.9921692500584,-3.2402505119227));
#99006=CARTESIAN_POINT('Ctrl Pts',(17.608958800475,21.004332868292,-3.24162479368793));
#99007=CARTESIAN_POINT('Ctrl Pts',(17.6161296672528,21.0088115584032,-3.24213404828691));
#99008=CARTESIAN_POINT('Ctrl Pts',(17.6288239822849,21.0166346969632,-3.24302941946336));
#99009=CARTESIAN_POINT('Ctrl Pts',(17.6343362260356,21.0199970355623,-3.24341619213557));
#99010=CARTESIAN_POINT('Ctrl Pts',(17.6457691799304,21.026899299525,-3.24421426229817));
#99011=CARTESIAN_POINT('Ctrl Pts',(17.6516919886846,21.0304356141779,-3.24462542439077));
#99012=CARTESIAN_POINT('Ctrl Pts',(17.6669394893455,21.0394385955014,-3.24567814733697));
#99013=CARTESIAN_POINT('Ctrl Pts',(17.6762890277062,21.0448629546849,-3.24631816681371));
#99014=CARTESIAN_POINT('Ctrl Pts',(17.7154849602121,21.0672039394384,-3.24897893555428));
#99015=CARTESIAN_POINT('Ctrl Pts',(17.7456997772362,21.083465972287,-3.25097615374836));
#99016=CARTESIAN_POINT('Ctrl Pts',(17.8254447987032,21.1239175083262,-3.25612051576821));
#99017=CARTESIAN_POINT('Ctrl Pts',(17.8755487132813,21.1469204480803,-3.25922826489179));
#99018=CARTESIAN_POINT('Ctrl Pts',(18.0275780243382,21.209653112275,-3.26837300717717));
#99019=CARTESIAN_POINT('Ctrl Pts',(18.1317424662785,21.2434696842161,-3.27426127206076));
#99020=CARTESIAN_POINT('Ctrl Pts',(18.2827868088843,21.2798675645777,-3.28272016865566));
#99021=CARTESIAN_POINT('Ctrl Pts',(18.3278592402491,21.2891856953231,-3.28523622204361));
#99022=CARTESIAN_POINT('Ctrl Pts',(18.3949987144338,21.300798223752,-3.28901509046505));
#99023=CARTESIAN_POINT('Ctrl Pts',(18.4168566471958,21.3042268233531,-3.29025018981404));
#99024=CARTESIAN_POINT('Ctrl Pts',(18.4897453002247,21.3144921709329,-3.29439629947441));
#99025=CARTESIAN_POINT('Ctrl Pts',(18.5409674567388,21.3198094231568,-3.29735448844211));
#99026=CARTESIAN_POINT('Ctrl Pts',(18.6009478783508,21.3238324055423,-3.30092248011162));
#99027=CARTESIAN_POINT('Ctrl Pts',(18.6095713038437,21.3243577867427,-3.30143795753021));
#99028=CARTESIAN_POINT('Ctrl Pts',(18.622656661426,21.3250746449514,-3.30222427639916));
#99029=CARTESIAN_POINT('Ctrl Pts',(18.6271165012822,21.3253048172704,-3.30249300097944));
#99030=CARTESIAN_POINT('Ctrl Pts',(18.6351357008699,21.3256932506871,-3.30297755066702));
#99031=CARTESIAN_POINT('Ctrl Pts',(18.6386947577369,21.3258566392622,-3.30319308557753));
#99032=CARTESIAN_POINT('Ctrl Pts',(18.646443745119,21.3261927777671,-3.30366342433517));
#99033=CARTESIAN_POINT('Ctrl Pts',(18.6506337280332,21.3263620609441,-3.30391841435706));
#99034=CARTESIAN_POINT('Ctrl Pts',(18.6624420011046,21.3268039998604,-3.30463887000105));
#99035=CARTESIAN_POINT('Ctrl Pts',(18.6700612102549,21.3270479531758,-3.30510589555819));
#99036=CARTESIAN_POINT('Ctrl Pts',(18.7164059381543,21.3282812987535,-3.30795906396363));
#99037=CARTESIAN_POINT('Ctrl Pts',(18.7551486955895,21.3282486730973,-3.31039691276878));
#99038=CARTESIAN_POINT('Ctrl Pts',(18.8845059450356,21.3245891696571,-3.31866548505668));
#99039=CARTESIAN_POINT('Ctrl Pts',(18.97488229698,21.3162042498079,-3.3246500656955));
#99040=CARTESIAN_POINT('Ctrl Pts',(19.130734388154,21.2915758828464,-3.33507696129625));
#99041=CARTESIAN_POINT('Ctrl Pts',(19.196498625389,21.2779518004067,-3.33951152027783));
#99042=CARTESIAN_POINT('Ctrl Pts',(19.3726434450192,21.2326312034525,-3.35138282706485));
#99043=CARTESIAN_POINT('Ctrl Pts',(19.4812852787277,21.1950439273391,-3.35868683075174));
#99044=CARTESIAN_POINT('Ctrl Pts',(19.5994118731489,21.1430855619597,-3.36656623016451));
#99045=CARTESIAN_POINT('Ctrl Pts',(19.6124062756236,21.1372125426555,-3.36743235935875));
#99046=CARTESIAN_POINT('Ctrl Pts',(19.6330013126163,21.1276525432891,-3.36880430551127));
#99047=CARTESIAN_POINT('Ctrl Pts',(19.6406407598762,21.1240506704065,-3.36931303489598));
#99048=CARTESIAN_POINT('Ctrl Pts',(19.6540808124361,21.1176153176316,-3.37020779533655));
#99049=CARTESIAN_POINT('Ctrl Pts',(19.659890357605,21.1148008609008,-3.37059447967014));
#99050=CARTESIAN_POINT('Ctrl Pts',(19.6718842843063,21.1089224698088,-3.37139266734787));
#99051=CARTESIAN_POINT('Ctrl Pts',(19.6780667449575,21.1058547741063,-3.37180403381585));
#99052=CARTESIAN_POINT('Ctrl Pts',(19.6939072246733,21.0978980620105,-3.37285790143912));
#99053=CARTESIAN_POINT('Ctrl Pts',(19.7035430228559,21.0929650660462,-3.37349885463178));
#99054=CARTESIAN_POINT('Ctrl Pts',(19.743680942859,21.0720265769892,-3.3761687142773));
#99055=CARTESIAN_POINT('Ctrl Pts',(19.773828973,21.0553512226515,-3.37817388393533));
#99056=CARTESIAN_POINT('Ctrl Pts',(19.8513820324026,21.0099489752026,-3.38334337695911));
#99057=CARTESIAN_POINT('Ctrl Pts',(19.898090490426,20.9800828150596,-3.38646779892359));
#99058=CARTESIAN_POINT('Ctrl Pts',(20.0335281682329,20.8857921549217,-3.39564161633733));
#99059=CARTESIAN_POINT('Ctrl Pts',(20.1184836985275,20.8162750431441,-3.4015423837091));
#99060=CARTESIAN_POINT('Ctrl Pts',(20.2426868186299,20.6974167549793,-3.4109034341488));
#99061=CARTESIAN_POINT('Ctrl Pts',(20.2857741169622,20.6523767865316,-3.41431572028435));
#99062=CARTESIAN_POINT('Ctrl Pts',(20.3638815131606,20.563162131561,-3.42096827558358));
#99063=CARTESIAN_POINT('Ctrl Pts',(20.3992460553724,20.5193617903362,-3.4241908487252));
#99064=CARTESIAN_POINT('Ctrl Pts',(20.4380912279551,20.4671210567527,-3.42805321900816));
#99065=CARTESIAN_POINT('Ctrl Pts',(20.4433173594533,20.4600000724333,-3.42858009519152));
#99066=CARTESIAN_POINT('Ctrl Pts',(20.451142771871,20.4491962760847,-3.4293803964736));
#99067=CARTESIAN_POINT('Ctrl Pts',(20.4537751790517,20.4455374233911,-3.42965159017405));
#99068=CARTESIAN_POINT('Ctrl Pts',(20.4584690077531,20.4389691996341,-3.43013876793881));
#99069=CARTESIAN_POINT('Ctrl Pts',(20.4605347811103,20.4360630038037,-3.43035444773612));
#99070=CARTESIAN_POINT('Ctrl Pts',(20.4649957423871,20.4297534856831,-3.43082297701288));
#99071=CARTESIAN_POINT('Ctrl Pts',(20.4673882075464,20.4263483616963,-3.43107600108407));
#99072=CARTESIAN_POINT('Ctrl Pts',(20.4740508688877,20.4168059029012,-3.43178548864634));
#99073=CARTESIAN_POINT('Ctrl Pts',(20.4782985653936,20.4106530384743,-3.43224343855026));
#99074=CARTESIAN_POINT('Ctrl Pts',(20.5029238557443,20.3745755774155,-3.43493081986129));
#99075=CARTESIAN_POINT('Ctrl Pts',(20.5225624087132,20.3441565994983,-3.43720536256098));
#99076=CARTESIAN_POINT('Ctrl Pts',(20.5834735755453,20.2442778772683,-3.44466394771567));
#99077=CARTESIAN_POINT('Ctrl Pts',(20.621551733202,20.1729575852527,-3.44997280347107));
#99078=CARTESIAN_POINT('Ctrl Pts',(20.732935031487,19.9321198290709,-3.46749316358894));
#99079=CARTESIAN_POINT('Ctrl Pts',(20.7881876152504,19.7551465797868,-3.47965034010632));
#99080=CARTESIAN_POINT('Ctrl Pts',(20.8235802099429,19.5513478117612,-3.49237241659951));
#99081=CARTESIAN_POINT('Ctrl Pts',(20.8270353053704,19.5294106722129,-3.4937272997619));
#99082=CARTESIAN_POINT('Ctrl Pts',(20.8313312895463,19.4990317271568,-3.49558415685693));
#99083=CARTESIAN_POINT('Ctrl Pts',(20.8324674835906,19.4906337560797,-3.49609542916909));
#99084=CARTESIAN_POINT('Ctrl Pts',(20.8343324616095,19.4761971755608,-3.4969708976316));
#99085=CARTESIAN_POINT('Ctrl Pts',(20.8350856984129,19.4701618805719,-3.49733586248594));
#99086=CARTESIAN_POINT('Ctrl Pts',(20.8365837569957,19.4577227334541,-3.49808599021959));
#99087=CARTESIAN_POINT('Ctrl Pts',(20.837325357055,19.4513185514561,-3.49847104774548));
#99088=CARTESIAN_POINT('Ctrl Pts',(20.8389812154041,19.4364240488768,-3.49936399356953));
#99089=CARTESIAN_POINT('Ctrl Pts',(20.839873384816,19.4279313472028,-3.49987118096662));
#99090=CARTESIAN_POINT('Ctrl Pts',(20.8425578397165,19.4007985576625,-3.5014854649064));
#99091=CARTESIAN_POINT('Ctrl Pts',(20.8441542370115,19.3821396660465,-3.50258640332619));
#99092=CARTESIAN_POINT('Ctrl Pts',(20.8472985949722,19.3385921680564,-3.50513595017191));
#99093=CARTESIAN_POINT('Ctrl Pts',(20.8486548380721,19.3136922688832,-3.50657861369475));
#99094=CARTESIAN_POINT('Ctrl Pts',(20.8518764894577,19.2260578491885,-3.51160944547749));
#99095=CARTESIAN_POINT('Ctrl Pts',(20.8513922858796,19.1632677994925,-3.51512908724445));
#99096=CARTESIAN_POINT('Ctrl Pts',(20.8429335710268,19.0013039643041,-3.52409522285026));
#99097=CARTESIAN_POINT('Ctrl Pts',(20.8307606992863,18.9025064183191,-3.52945117451298));
#99098=CARTESIAN_POINT('Ctrl Pts',(20.7979299445984,18.7345249330378,-3.53877346953323));
#99099=CARTESIAN_POINT('Ctrl Pts',(20.7806006530245,18.6648683175245,-3.54270751075005));
#99100=CARTESIAN_POINT('Ctrl Pts',(20.746278597417,18.5517712854519,-3.54939451847304));
#99101=CARTESIAN_POINT('Ctrl Pts',(20.7313275221603,18.5077719279041,-3.55207382890925));
#99102=CARTESIAN_POINT('Ctrl Pts',(20.7122407784917,18.4571358877466,-3.55528720006793));
#99103=CARTESIAN_POINT('Ctrl Pts',(20.7095001066211,18.4499829159889,-3.55574420043702));
#99104=CARTESIAN_POINT('Ctrl Pts',(20.7050447920928,18.4385410944547,-3.5564803867906));
#99105=CARTESIAN_POINT('Ctrl Pts',(20.7033547993185,18.4342426333353,-3.55675813300646));
#99106=CARTESIAN_POINT('Ctrl Pts',(20.7003282714571,18.4266180917129,-3.55725294406247));
#99107=CARTESIAN_POINT('Ctrl Pts',(20.6989973403463,18.4232898366547,-3.55746966987588));
#99108=CARTESIAN_POINT('Ctrl Pts',(20.6961487975362,18.4162186410653,-3.55793170199208));
#99109=CARTESIAN_POINT('Ctrl Pts',(20.6946289495333,18.4124767168053,-3.55817713696921));
#99110=CARTESIAN_POINT('Ctrl Pts',(20.6904764310727,18.402336382944,-3.55884474831909));
#99111=CARTESIAN_POINT('Ctrl Pts',(20.6878231127795,18.3959465589251,-3.55926814500395));
#99112=CARTESIAN_POINT('Ctrl Pts',(20.6742067489765,18.3636036798431,-3.56142455906846));
#99113=CARTESIAN_POINT('Ctrl Pts',(20.662758277842,18.3378596455277,-3.56318468375243));
#99114=CARTESIAN_POINT('Ctrl Pts',(20.6277132086572,18.2631090341327,-3.56840839404944));
#99115=CARTESIAN_POINT('Ctrl Pts',(20.6027386053463,18.2147760204601,-3.5719306550947));
#99116=CARTESIAN_POINT('Ctrl Pts',(20.5063073786562,18.0445667949262,-3.58473693324005));
#99117=CARTESIAN_POINT('Ctrl Pts',(20.4245498040554,17.9289366811572,-3.59417851851971));
#99118=CARTESIAN_POINT('Ctrl Pts',(20.2729908615203,17.7545465879801,-3.60909205489516));
#99119=CARTESIAN_POINT('Ctrl Pts',(20.2098412776637,17.6905903173306,-3.61474964247142));
#99120=CARTESIAN_POINT('Ctrl Pts',(20.1325788705896,17.6217064082067,-3.62106521154277));
#99121=CARTESIAN_POINT('Ctrl Pts',(20.1222565019068,17.6126818599007,-3.62189756626861));
#99122=CARTESIAN_POINT('Ctrl Pts',(20.1055565795846,17.598365447915,-3.62322622708388));
#99123=CARTESIAN_POINT('Ctrl Pts',(20.0992344913194,17.5930097539416,-3.62372516625509));
#99124=CARTESIAN_POINT('Ctrl Pts',(20.0879503834773,17.5835637626124,-3.62460860917325));
#99125=CARTESIAN_POINT('Ctrl Pts',(20.0830008931566,17.5794587227538,-3.62499371394123));
#99126=CARTESIAN_POINT('Ctrl Pts',(20.0726463945855,17.5709501735711,-3.62579443106882));
#99127=CARTESIAN_POINT('Ctrl Pts',(20.0672381763467,17.5665506788518,-3.62620987780965));
#99128=CARTESIAN_POINT('Ctrl Pts',(20.0531300913197,17.555189336429,-3.62728652046865));
#99129=CARTESIAN_POINT('Ctrl Pts',(20.0443967476758,17.5482692574326,-3.62794603533587));
#99130=CARTESIAN_POINT('Ctrl Pts',(20.0061697385541,17.5184674079985,-3.63080325429072));
#99131=CARTESIAN_POINT('Ctrl Pts',(19.9761273438626,17.4962981800244,-3.63297276085202));
#99132=CARTESIAN_POINT('Ctrl Pts',(19.8946914692653,17.4394681885347,-3.63867130106736));
#99133=CARTESIAN_POINT('Ctrl Pts',(19.8423347859398,17.406249459587,-3.64214884170592));
#99134=CARTESIAN_POINT('Ctrl Pts',(19.7069292251707,17.3284570827204,-3.65078677320553));
#99135=CARTESIAN_POINT('Ctrl Pts',(19.6222240937723,17.2870411500413,-3.65586984781523));
#99136=CARTESIAN_POINT('Ctrl Pts',(19.4210144012457,17.2047908058381,-3.6676944257322));
#99137=CARTESIAN_POINT('Ctrl Pts',(19.3031514036269,17.1682269242903,-3.67444122090718));
#99138=CARTESIAN_POINT('Ctrl Pts',(19.1735739266523,17.1401178492513,-3.68230024978787));
#99139=CARTESIAN_POINT('Ctrl Pts',(19.164335112392,17.1381782993091,-3.68286299825159));
#99140=CARTESIAN_POINT('Ctrl Pts',(19.1506054170072,17.135391701481,-3.68370326877679));
#99141=CARTESIAN_POINT('Ctrl Pts',(19.1461241212043,17.1344972694013,-3.68397815543183));
#99142=CARTESIAN_POINT('Ctrl Pts',(19.1381360136509,17.1329297814439,-3.68446932583529));
#99143=CARTESIAN_POINT('Ctrl Pts',(19.1346303611728,17.1322510819609,-3.68468528434452));
#99144=CARTESIAN_POINT('Ctrl Pts',(19.1270784631141,17.1308088365709,-3.68515138830297));
#99145=CARTESIAN_POINT('Ctrl Pts',(19.1230317608604,17.1300482362757,-3.68540169212611));
#99146=CARTESIAN_POINT('Ctrl Pts',(19.111828676928,17.1279763744941,-3.68609609186472));
#99147=CARTESIAN_POINT('Ctrl Pts',(19.1046677943431,17.1266902062738,-3.68654157567169));
#99148=CARTESIAN_POINT('Ctrl Pts',(19.066176442187,17.1199813922492,-3.68894438159497));
#99149=CARTESIAN_POINT('Ctrl Pts',(19.0347352137866,17.1152285224869,-3.6909362948906));
#99150=CARTESIAN_POINT('Ctrl Pts',(18.841308648286,17.0904307994393,-3.70332086242888));
#99151=CARTESIAN_POINT('Ctrl Pts',(18.6775640440237,17.0884676178542,-3.71431350075406));
#99152=CARTESIAN_POINT('Ctrl Pts',(18.3988741370583,17.117423535812,-3.73261642477663));
#99153=CARTESIAN_POINT('Ctrl Pts',(18.2837148017831,17.1391354212299,-3.74006804206649));
#99154=CARTESIAN_POINT('Ctrl Pts',(18.1571460386678,17.1740579896664,-3.7480851297345));
#99155=CARTESIAN_POINT('Ctrl Pts',(18.1434079507728,17.1779986981607,-3.74895323667806));
#99156=CARTESIAN_POINT('Ctrl Pts',(18.1216071999855,17.1844917844461,-3.75032771271529));
#99157=CARTESIAN_POINT('Ctrl Pts',(18.1135182896523,17.1869538198002,-3.75083701098681));
#99158=CARTESIAN_POINT('Ctrl Pts',(18.0992785984693,17.1913813644741,-3.75173243296299));
#99159=CARTESIAN_POINT('Ctrl Pts',(18.0931216938649,17.193326664526,-3.75211921299655));
#99160=CARTESIAN_POINT('Ctrl Pts',(18.0804059895686,17.1974083211125,-3.75291727346725));
#99161=CARTESIAN_POINT('Ctrl Pts',(18.0738485311375,17.1995486285652,-3.75332841862934));
#99162=CARTESIAN_POINT('Ctrl Pts',(18.0570440056722,17.2051245342603,-3.7543810467283));
#99163=CARTESIAN_POINT('Ctrl Pts',(18.0468124943179,17.208606646809,-3.7550209888335));
#99164=CARTESIAN_POINT('Ctrl Pts',(18.0048404161899,17.223250688442,-3.75764269247529));
#99165=CARTESIAN_POINT('Ctrl Pts',(17.9733404272866,17.2350905323301,-3.75960192765196));
#99166=CARTESIAN_POINT('Ctrl Pts',(17.8921203737892,17.2678489390955,-3.76464272767542));
#99167=CARTESIAN_POINT('Ctrl Pts',(17.8428928722314,17.2899258087789,-3.76768663705855));
#99168=CARTESIAN_POINT('Ctrl Pts',(17.6804852539002,17.3703480737555,-3.77777329623982));
#99169=CARTESIAN_POINT('Ctrl Pts',(17.5717401856394,17.4370086425783,-3.78458694596819));
#99170=CARTESIAN_POINT('Ctrl Pts',(17.3877476745824,17.5740153256638,-3.79713120499452));
#99171=CARTESIAN_POINT('Ctrl Pts',(17.3103836803492,17.6408327664611,-3.80279980053515));
#99172=CARTESIAN_POINT('Ctrl Pts',(17.2312943924323,17.7198062591517,-3.80942140215416));
#99173=CARTESIAN_POINT('Ctrl Pts',(17.2244840392838,17.726700679768,-3.80999890105219));
#99174=CARTESIAN_POINT('Ctrl Pts',(17.2144981910691,17.7369495987166,-3.81085699491019));
#99175=CARTESIAN_POINT('Ctrl Pts',(17.2112858430292,17.7402682338026,-3.8111347892569));
#99176=CARTESIAN_POINT('Ctrl Pts',(17.2056059512423,17.7461746121291,-3.81162915001794));
#99177=CARTESIAN_POINT('Ctrl Pts',(17.2031340762655,17.7487581224133,-3.81184537471628));
#99178=CARTESIAN_POINT('Ctrl Pts',(17.1978517144034,17.7543071232828,-3.81230978154288));
#99179=CARTESIAN_POINT('Ctrl Pts',(17.1950433058677,17.7572744463438,-3.8125581101102));
#99180=CARTESIAN_POINT('Ctrl Pts',(17.1892976395439,17.7633805413353,-3.81306905410891));
#99181=CARTESIAN_POINT('Ctrl Pts',(17.1863613188675,17.7665201657942,-3.81333173768555));
#99182=CARTESIAN_POINT('Ctrl Pts',(17.1729076003644,17.7809935002625,-3.81454243739383));
#99183=CARTESIAN_POINT('Ctrl Pts',(17.1625053222708,17.7924329358648,-3.81549866485058));
#99184=CARTESIAN_POINT('Ctrl Pts',(17.0941973456397,17.8692249567763,-3.82190710789897));
#99185=CARTESIAN_POINT('Ctrl Pts',(17.0402625674082,17.9379864944498,-3.82759171384278));
#99186=CARTESIAN_POINT('Ctrl Pts',(16.9494514006864,18.0697861592552,-3.83812735841573));
#99187=CARTESIAN_POINT('Ctrl Pts',(16.9112865256595,18.1317880314201,-3.84295320018642));
#99188=CARTESIAN_POINT('Ctrl Pts',(16.8741060039446,18.1998096180957,-3.84805125711873));
#99189=CARTESIAN_POINT('Ctrl Pts',(16.8718367035901,18.2039947752084,-3.84836416845396));
#99190=CARTESIAN_POINT('Ctrl Pts',(16.8216173512443,18.2973620733673,-3.85532787399593));
#99191=CARTESIAN_POINT('Ctrl Pts',(16.7801280274345,18.3898340573838,-3.86186882407568));
#99192=CARTESIAN_POINT('Ctrl Pts',(16.7454195180457,18.4848893563717,-3.86819359339412));
#99193=CARTESIAN_POINT('',(16.6170008393112,19.2128851108722,-2.8890562790225));
#99194=CARTESIAN_POINT('Ctrl Pts',(16.7454194503191,18.4848895418526,-3.64442446310682));
#99195=CARTESIAN_POINT('Ctrl Pts',(16.7704138790241,18.4164379251386,-3.6400512785945));
#99196=CARTESIAN_POINT('Ctrl Pts',(16.7989618302365,18.3492371530331,-3.63567809408218));
#99197=CARTESIAN_POINT('Ctrl Pts',(16.8309082930386,18.2836753778236,-3.63130490956986));
#99198=CARTESIAN_POINT('Ctrl Pts',(16.8628484348593,18.2181265747783,-3.62693259034326));
#99199=CARTESIAN_POINT('Ctrl Pts',(16.8981855413773,18.1542165580066,-3.62256027111665));
#99200=CARTESIAN_POINT('Ctrl Pts',(16.9367174473244,18.0923112918029,-3.61818795189004));
#99201=CARTESIAN_POINT('Ctrl Pts',(16.9752544398296,18.0303978535473,-3.61381505547797));
#99202=CARTESIAN_POINT('Ctrl Pts',(17.0169868120812,17.9704900994532,-3.60944215906591));
#99203=CARTESIAN_POINT('Ctrl Pts',(17.0616685471728,17.9129258449978,-3.60506926265384));
#99204=CARTESIAN_POINT('Ctrl Pts',(17.1063995662725,17.8552980970997,-3.60069154293171));
#99205=CARTESIAN_POINT('Ctrl Pts',(17.1540861428344,17.80001938801,-3.59631382320958));
#99206=CARTESIAN_POINT('Ctrl Pts',(17.2044419181706,17.7473944949849,-3.59193610348746));
#99207=CARTESIAN_POINT('Ctrl Pts',(17.2548300009133,17.6947358387262,-3.58755557509504));
#99208=CARTESIAN_POINT('Ctrl Pts',(17.3078903391089,17.6447347170448,-3.58317504670262));
#99209=CARTESIAN_POINT('Ctrl Pts',(17.3633016198,17.597657212333,-3.57879451831021));
#99210=CARTESIAN_POINT('Ctrl Pts',(17.418805685217,17.5505008775831,-3.5744066548387));
#99211=CARTESIAN_POINT('Ctrl Pts',(17.4766681650794,17.5062782200529,-3.5700187913672));
#99212=CARTESIAN_POINT('Ctrl Pts',(17.5365374615874,17.4652129370687,-3.56563092789569));
#99213=CARTESIAN_POINT('Ctrl Pts',(17.5579514560577,17.4505247447224,-3.56406148095718));
#99214=CARTESIAN_POINT('Ctrl Pts',(17.5796219550475,17.4362400645932,-3.56249203401867));
#99215=CARTESIAN_POINT('Ctrl Pts',(17.6015321394765,17.4223676887405,-3.56092258708016));
#99216=CARTESIAN_POINT('Ctrl Pts',(17.6627935078071,17.3835802139256,-3.55653437814988));
#99217=CARTESIAN_POINT('Ctrl Pts',(17.7261694924201,17.3478680068777,-3.5521461692196));
#99218=CARTESIAN_POINT('Ctrl Pts',(17.7913186157339,17.3154681992227,-3.54775796028932));
#99219=CARTESIAN_POINT('Ctrl Pts',(17.8563710469468,17.2831164782542,-3.54337626418867));
#99220=CARTESIAN_POINT('Ctrl Pts',(17.9231909643682,17.2540676104731,-3.53899456808802));
#99221=CARTESIAN_POINT('Ctrl Pts',(17.9914091442163,17.22851473627,-3.53461287198737));
#99222=CARTESIAN_POINT('Ctrl Pts',(18.0595471622739,17.2029918887279,-3.53023632472837));
#99223=CARTESIAN_POINT('Ctrl Pts',(18.1290797293046,17.1809570424211,-3.52585977746936));
#99224=CARTESIAN_POINT('Ctrl Pts',(18.199615869865,17.1625560536202,-3.52148323021035));
#99225=CARTESIAN_POINT('Ctrl Pts',(18.2701072774302,17.1441667344591,-3.51710945849401));
#99226=CARTESIAN_POINT('Ctrl Pts',(18.3416005301142,17.1294068217631,-3.51273568677767));
#99227=CARTESIAN_POINT('Ctrl Pts',(18.4136889989947,17.1183724978786,-3.50836191506134));
#99228=CARTESIAN_POINT('Ctrl Pts',(18.485755531112,17.1073415317759,-3.50398947429842));
#99229=CARTESIAN_POINT('Ctrl Pts',(18.5584164432967,17.1000339766644,-3.49961703353551));
#99230=CARTESIAN_POINT('Ctrl Pts',(18.6312560654053,17.0964946952292,-3.4952445927726));
#99231=CARTESIAN_POINT('Ctrl Pts',(18.704097550031,17.0929553232941,-3.4908720402059));
#99232=CARTESIAN_POINT('Ctrl Pts',(18.7771172717469,17.0931844377533,-3.4864994876392));
#99233=CARTESIAN_POINT('Ctrl Pts',(18.8498972932262,17.0971748375462,-3.4821269350725));
#99234=CARTESIAN_POINT('Ctrl Pts',(18.9227528485569,17.1011693787265,-3.47774984450582));
#99235=CARTESIAN_POINT('Ctrl Pts',(18.9953677242803,17.1089329725837,-3.47337275393914));
#99236=CARTESIAN_POINT('Ctrl Pts',(19.0673276840485,17.120406386921,-3.46899566337246));
#99237=CARTESIAN_POINT('Ctrl Pts',(19.1393269438215,17.1318860673157,-3.46461618231416));
#99238=CARTESIAN_POINT('Ctrl Pts',(19.2106701033895,17.1470795015322,-3.46023670125586));
#99239=CARTESIAN_POINT('Ctrl Pts',(19.2809543980013,17.1658765595918,-3.45585722019757));
#99240=CARTESIAN_POINT('Ctrl Pts',(19.3513632710535,17.1847069353106,-3.45146997653849));
#99241=CARTESIAN_POINT('Ctrl Pts',(19.4207090718562,17.2071535415653,-3.44708273287941));
#99242=CARTESIAN_POINT('Ctrl Pts',(19.4886059995035,17.2330569306693,-3.44269548922033));
#99243=CARTESIAN_POINT('Ctrl Pts',(19.5347693678666,17.2506687392518,-3.43971258627979));
#99244=CARTESIAN_POINT('Ctrl Pts',(19.5802633709747,17.2698774944523,-3.43672968333926));
#99245=CARTESIAN_POINT('Ctrl Pts',(19.6249733426257,17.2906210002371,-3.43374678039872));
#99246=CARTESIAN_POINT('Ctrl Pts',(19.690747087516,17.3211371917541,-3.4293585714646));
#99247=CARTESIAN_POINT('Ctrl Pts',(19.7550796205686,17.3550960250398,-3.42497036253047));
#99248=CARTESIAN_POINT('Ctrl Pts',(19.8175867162744,17.3923387263392,-3.42058215359634));
#99249=CARTESIAN_POINT('Ctrl Pts',(19.8800010410865,17.429526153295,-3.41620045749183));
#99250=CARTESIAN_POINT('Ctrl Pts',(19.9405948958129,17.4699875282328,-3.41181876138732));
#99251=CARTESIAN_POINT('Ctrl Pts',(19.9990060261197,17.513516935613,-3.40743706528282));
#99252=CARTESIAN_POINT('Ctrl Pts',(20.0573485186999,17.5569951924752,-3.40306051801994));
#99253=CARTESIAN_POINT('Ctrl Pts',(20.1135129971337,17.6035340332493,-3.39868397075707));
#99254=CARTESIAN_POINT('Ctrl Pts',(20.1671651917876,17.6528836586929,-3.39430742349419));
#99255=CARTESIAN_POINT('Ctrl Pts',(20.2207833609995,17.7022019873212,-3.38993365177399));
#99256=CARTESIAN_POINT('Ctrl Pts',(20.2718920534962,17.7543272380349,-3.38555988005378));
#99257=CARTESIAN_POINT('Ctrl Pts',(20.3201902946222,17.8089695619402,-3.38118610833357));
#99258=CARTESIAN_POINT('Ctrl Pts',(20.3684738384312,17.8635952580027,-3.3768136675668));
#99259=CARTESIAN_POINT('Ctrl Pts',(20.413948309491,17.9207361453916,-3.37244122680002));
#99260=CARTESIAN_POINT('Ctrl Pts',(20.4563509910177,17.9800669946174,-3.36806878603325));
#99261=CARTESIAN_POINT('Ctrl Pts',(20.4987547567856,18.0393993609393,-3.36369623346269));
#99262=CARTESIAN_POINT('Ctrl Pts',(20.5380862982224,18.10092140666,-3.35932368089214));
#99263=CARTESIAN_POINT('Ctrl Pts',(20.5741254487323,18.1642778148296,-3.35495112832159));
#99264=CARTESIAN_POINT('Ctrl Pts',(20.6102020020315,18.2276999766687,-3.35057403775109));
#99265=CARTESIAN_POINT('Ctrl Pts',(20.6429791031824,18.2929598817764,-3.34619694718059));
#99266=CARTESIAN_POINT('Ctrl Pts',(20.6722823388101,18.3596771616732,-3.3418198566101));
#99267=CARTESIAN_POINT('Ctrl Pts',(20.7016015780223,18.4264308783525,-3.33744037554801));
#99268=CARTESIAN_POINT('Ctrl Pts',(20.7274430033813,18.4946431030975,-3.33306089448592));
#99269=CARTESIAN_POINT('Ctrl Pts',(20.7496812078501,18.5639155632221,-3.32868141342383));
#99270=CARTESIAN_POINT('Ctrl Pts',(20.7719588293866,18.6333108083162,-3.32429416976102));
#99271=CARTESIAN_POINT('Ctrl Pts',(20.7906203524711,18.7037695748855,-3.31990692609822));
#99272=CARTESIAN_POINT('Ctrl Pts',(20.8055910206616,18.7748811594138,-3.31551968243541));
#99273=CARTESIAN_POINT('Ctrl Pts',(20.8157696323556,18.8232301840966,-3.31253677952937));
#99274=CARTESIAN_POINT('Ctrl Pts',(20.8242431499885,18.8718807754378,-3.30955387662333));
#99275=CARTESIAN_POINT('Ctrl Pts',(20.8310018039417,18.9207028517787,-3.30657097371729));
#99276=CARTESIAN_POINT('Ctrl Pts',(20.8409445967654,18.9925259978733,-3.30218276479086));
#99277=CARTESIAN_POINT('Ctrl Pts',(20.8472125720511,19.0650007495843,-3.29779455586443));
#99278=CARTESIAN_POINT('Ctrl Pts',(20.8497312594192,19.1377180928425,-3.29340634693799));
#99279=CARTESIAN_POINT('Ctrl Pts',(20.8522462086376,19.2103275115067,-3.28902465084118));
#99280=CARTESIAN_POINT('Ctrl Pts',(20.8510228997994,19.2831783288738,-3.28464295474436));
#99281=CARTESIAN_POINT('Ctrl Pts',(20.8460383938858,19.355854488202,-3.28026125864754));
#99282=CARTESIAN_POINT('Ctrl Pts',(20.8410597451634,19.4284452472597,-3.27588471139231));
#99283=CARTESIAN_POINT('Ctrl Pts',(20.8323287119824,19.5008612771246,-3.27150816413708));
#99284=CARTESIAN_POINT('Ctrl Pts',(20.8198744021611,19.5726862983432,-3.26713161688185));
#99285=CARTESIAN_POINT('Ctrl Pts',(20.8074279906819,19.6444657691777,-3.26275784516926));
#99286=CARTESIAN_POINT('Ctrl Pts',(20.7912630697951,19.7156545009196,-3.25838407345667));
#99287=CARTESIAN_POINT('Ctrl Pts',(20.7714604446778,19.7858425318062,-3.25401030174408));
#99288=CARTESIAN_POINT('Ctrl Pts',(20.7516638455656,19.8560092042398,-3.24963786098487));
#99289=CARTESIAN_POINT('Ctrl Pts',(20.7282318707952,19.9251753164025,-3.24526542022567));
#99290=CARTESIAN_POINT('Ctrl Pts',(20.7012957832859,19.992943924502,-3.24089297946647));
#99291=CARTESIAN_POINT('Ctrl Pts',(20.6743590070176,20.0607142654529,-3.23652042690343));
#99292=CARTESIAN_POINT('Ctrl Pts',(20.6439181201481,20.1270865838657,-3.2321478743404));
#99293=CARTESIAN_POINT('Ctrl Pts',(20.6101527159991,20.1916834281506,-3.22777532177736));
#99294=CARTESIAN_POINT('Ctrl Pts',(20.5763522688394,20.2563473134783,-3.22339823121425));
#99295=CARTESIAN_POINT('Ctrl Pts',(20.5392206395603,20.3192316172821,-3.21902114065115));
#99296=CARTESIAN_POINT('Ctrl Pts',(20.4989832512063,20.3799837992723,-3.21464405008804));
#99297=CARTESIAN_POINT('Ctrl Pts',(20.4587238877208,20.4407691602846,-3.21026456903327));
#99298=CARTESIAN_POINT('Ctrl Pts',(20.4153556750978,20.4994196929838,-3.20588508797851));
#99299=CARTESIAN_POINT('Ctrl Pts',(20.3691456171873,20.5556143724478,-3.20150560692374));
#99300=CARTESIAN_POINT('Ctrl Pts',(20.322853652258,20.6119086566055,-3.19711836326808));
#99301=CARTESIAN_POINT('Ctrl Pts',(20.2737101085746,20.6657380382375,-3.19273111961242));
#99302=CARTESIAN_POINT('Ctrl Pts',(20.2220198585544,20.716817352984,-3.18834387595676));
#99303=CARTESIAN_POINT('Ctrl Pts',(20.1868754689114,20.7515463655046,-3.18536097298313));
#99304=CARTESIAN_POINT('Ctrl Pts',(20.1505545743034,20.7850048960123,-3.1823780700095));
#99305=CARTESIAN_POINT('Ctrl Pts',(20.1131612647175,20.8171143190642,-3.17939516703586));
#99306=CARTESIAN_POINT('Ctrl Pts',(20.0581512102736,20.8643511411,-3.17500695810766));
#99307=CARTESIAN_POINT('Ctrl Pts',(20.000604149589,20.9088507248998,-3.17061874917945));
#99308=CARTESIAN_POINT('Ctrl Pts',(19.9408236893637,20.9503290611011,-3.16623054025124));
#99309=CARTESIAN_POINT('Ctrl Pts',(19.8811319532539,20.9917458365736,-3.16184884415272));
#99310=CARTESIAN_POINT('Ctrl Pts',(19.8192137908515,21.0301499931512,-3.1574671480542));
#99311=CARTESIAN_POINT('Ctrl Pts',(19.7554066235781,21.0652970391258,-3.15308545195568));
#99312=CARTESIAN_POINT('Ctrl Pts',(19.6916744348053,21.1004027845237,-3.14870890469886));
#99313=CARTESIAN_POINT('Ctrl Pts',(19.6260580710932,21.1322587908208,-3.14433235744203));
#99314=CARTESIAN_POINT('Ctrl Pts',(19.5589233130942,21.1606642089123,-3.13995581018521));
#99315=CARTESIAN_POINT('Ctrl Pts',(19.4918311309836,21.1890516127003,-3.1355820384711));
#99316=CARTESIAN_POINT('Ctrl Pts',(19.423222908347,21.2139925826756,-3.13120826675699));
#99317=CARTESIAN_POINT('Ctrl Pts',(19.3534870964587,21.2353331586775,-3.12683449504287));
#99318=CARTESIAN_POINT('Ctrl Pts',(19.2837725054128,21.2566672406702,-3.12246205428222));
#99319=CARTESIAN_POINT('Ctrl Pts',(19.2129314673179,21.2744029627461,-3.11808961352157));
#99320=CARTESIAN_POINT('Ctrl Pts',(19.1413687992146,21.288435838101,-3.11371717276091));
#99321=CARTESIAN_POINT('Ctrl Pts',(19.0698043012465,21.302469072278,-3.1093446201965));
#99322=CARTESIAN_POINT('Ctrl Pts',(18.9975186103822,21.312799180891,-3.10497206763209));
#99323=CARTESIAN_POINT('Ctrl Pts',(18.9249263141349,21.3193728661152,-3.10059951506768));
#99324=CARTESIAN_POINT('Ctrl Pts',(18.8522586788649,21.3259533737578,-3.09622242450331));
#99325=CARTESIAN_POINT('Ctrl Pts',(18.7792842843306,21.3287696306808,-3.09184533393895));
#99326=CARTESIAN_POINT('Ctrl Pts',(18.7064215783433,21.3278203586178,-3.08746824337459));
#99327=CARTESIAN_POINT('Ctrl Pts',(18.6335190793282,21.3268705681222,-3.08308876231863));
#99328=CARTESIAN_POINT('Ctrl Pts',(18.5607288720058,21.3221511854103,-3.07870928126267));
#99329=CARTESIAN_POINT('Ctrl Pts',(18.4884654116523,21.3137129537635,-3.07432980020672));
#99330=CARTESIAN_POINT('Ctrl Pts',(18.4160738648003,21.3052597654078,-3.06994255654998));
#99331=CARTESIAN_POINT('Ctrl Pts',(18.3442114053975,21.2930746456032,-3.06555531289325));
#99332=CARTESIAN_POINT('Ctrl Pts',(18.2732828331998,21.2772595897456,-3.06116806923651));
#99333=CARTESIAN_POINT('Ctrl Pts',(18.225058238315,21.266506875597,-3.05818516627582));
#99334=CARTESIAN_POINT('Ctrl Pts',(18.1772650979176,21.2540772191558,-3.05520226331512));
#99335=CARTESIAN_POINT('Ctrl Pts',(18.1300258654965,21.2400155851671,-3.05221936035442));
#99336=CARTESIAN_POINT('Ctrl Pts',(18.0605312740272,21.2193292306402,-3.04783115140135));
#99337=CARTESIAN_POINT('Ctrl Pts',(17.9919650333991,21.1950280401746,-3.04344294244829));
#99338=CARTESIAN_POINT('Ctrl Pts',(17.9247302870924,21.1672135700813,-3.03905473349522));
#99339=CARTESIAN_POINT('Ctrl Pts',(17.8575953282952,21.1394403812727,-3.03467303737171));
#99340=CARTESIAN_POINT('Ctrl Pts',(17.791788382932,21.1081644467877,-3.0302913412482));
#99341=CARTESIAN_POINT('Ctrl Pts',(17.7276976696562,21.0735371459235,-3.02590964512469));
#99342=CARTESIAN_POINT('Ctrl Pts',(17.6636822680688,21.0389505348933,-3.02153309784281));
#99343=CARTESIAN_POINT('Ctrl Pts',(17.6013795146524,21.0010206087461,-3.01715655056093));
#99344=CARTESIAN_POINT('Ctrl Pts',(17.5411562818512,20.9599462153173,-3.01278000327905));
#99345=CARTESIAN_POINT('Ctrl Pts',(17.4809712417489,20.918897870672,-3.00840623153985));
#99346=CARTESIAN_POINT('Ctrl Pts',(17.4228635031208,20.8747092865794,-3.00403245980065));
#99347=CARTESIAN_POINT('Ctrl Pts',(17.367172783407,20.8276237533764,-2.99965868806145));
#99348=CARTESIAN_POINT('Ctrl Pts',(17.3114990105668,20.7805525484596,-2.99528624727572));
#99349=CARTESIAN_POINT('Ctrl Pts',(17.2582411645738,20.7305864558404,-2.99091380648998));
#99350=CARTESIAN_POINT('Ctrl Pts',(17.2077062220831,20.6780093058642,-2.98654136570425));
#99351=CARTESIAN_POINT('Ctrl Pts',(17.1571699874092,20.6254308114853,-2.9821688131148));
#99352=CARTESIAN_POINT('Ctrl Pts',(17.1093571273009,20.5702414763594,-2.97779626052535));
#99353=CARTESIAN_POINT('Ctrl Pts',(17.064536865154,20.5127610538767,-2.9734237079359));
#99354=CARTESIAN_POINT('Ctrl Pts',(17.0196700868515,20.4552209760473,-2.96904661734673));
#99355=CARTESIAN_POINT('Ctrl Pts',(16.9778024047636,20.3953854446857,-2.96466952675757));
#99356=CARTESIAN_POINT('Ctrl Pts',(16.9391613915757,20.3336056162827,-2.96029243616841));
#99357=CARTESIAN_POINT('Ctrl Pts',(16.9004992750975,20.2717920476242,-2.95591295508774));
#99358=CARTESIAN_POINT('Ctrl Pts',(16.8650675705241,20.2080324897248,-2.95153347400708));
#99359=CARTESIAN_POINT('Ctrl Pts',(16.8330479475686,20.1427029002621,-2.94715399292642));
#99360=CARTESIAN_POINT('Ctrl Pts',(16.8009715700497,20.0772575145475,-2.94276674924541));
#99361=CARTESIAN_POINT('Ctrl Pts',(16.7723195413297,20.0102369839267,-2.93837950556439));
#99362=CARTESIAN_POINT('Ctrl Pts',(16.7472252098539,19.9420368891101,-2.93399226188338));
#99363=CARTESIAN_POINT('Ctrl Pts',(16.7301634837498,19.8956673996836,-2.93100935914658));
#99364=CARTESIAN_POINT('Ctrl Pts',(16.714745338617,19.8487529982297,-2.92802645640979));
#99365=CARTESIAN_POINT('Ctrl Pts',(16.7009992479662,19.8014209872878,-2.92504355367299));
#99366=CARTESIAN_POINT('Ctrl Pts',(16.6758066766592,19.7146752287267,-2.91957676374651));
#99367=CARTESIAN_POINT('Ctrl Pts',(16.6561521069757,19.6262535084973,-2.91410997382002));
#99368=CARTESIAN_POINT('Ctrl Pts',(16.6422180861875,19.5367873923999,-2.90864318389354));
#99369=CARTESIAN_POINT('Ctrl Pts',(16.6285119268963,19.44878430578,-2.90326579177662));
#99370=CARTESIAN_POINT('Ctrl Pts',(16.6203407792486,19.3597706087752,-2.8978883996597));
#99371=CARTESIAN_POINT('Ctrl Pts',(16.6178326248382,19.2703686811429,-2.89251100754278));
#99372=CARTESIAN_POINT('Ctrl Pts',(16.6172955000023,19.2512231311289,-2.89135943136935));
#99373=CARTESIAN_POINT('Ctrl Pts',(16.6170179137274,19.2320598582303,-2.89020785519593));
#99374=CARTESIAN_POINT('Ctrl Pts',(16.6170008393112,19.2128851108722,-2.8890562790225));
#99375=CARTESIAN_POINT('Ctrl Pts',(16.6180380291883,19.2128841872923,-2.8890562790225));
#99376=CARTESIAN_POINT('Ctrl Pts',(16.6201501796595,18.9660536838257,-2.8742252589287));
#99377=CARTESIAN_POINT('Ctrl Pts',(16.6645220593274,18.718557967196,-2.85939423883491));
#99378=CARTESIAN_POINT('Ctrl Pts',(16.747777019274,18.4857290362168,-2.84456321874111));
#99379=CARTESIAN_POINT('Origin',(18.734,19.211,0.));
#99380=CARTESIAN_POINT('',(16.7454194497489,18.4848895434144,-2.04625067101847));
#99381=CARTESIAN_POINT('',(16.7454194503195,18.4848895418517,-2.26547384646959));
#99382=CARTESIAN_POINT('',(16.7454194503191,18.4848895418526,0.));
#99383=CARTESIAN_POINT('',(16.6170007438825,19.2092252893056,-2.31031846004158));
#99384=CARTESIAN_POINT('Ctrl Pts',(16.7454194503191,18.4848895418526,-2.26547384646965));
#99385=CARTESIAN_POINT('Ctrl Pts',(16.7453677674078,18.4850310845493,-2.26548208690514));
#99386=CARTESIAN_POINT('Ctrl Pts',(16.7453160995444,18.4851726329394,-2.26549032756363));
#99387=CARTESIAN_POINT('Ctrl Pts',(16.71039107295,18.5808843594811,-2.27106239636578));
#99388=CARTESIAN_POINT('Ctrl Pts',(16.6824565881579,18.6788318784946,-2.27671183763777));
#99389=CARTESIAN_POINT('Ctrl Pts',(16.6596923791677,18.7878796593165,-2.28331158252327));
#99390=CARTESIAN_POINT('Ctrl Pts',(16.6577771067251,18.7973801045402,-2.28388912020902));
#99391=CARTESIAN_POINT('Ctrl Pts',(16.6550454939141,18.8114271084375,-2.28474726085886));
#99392=CARTESIAN_POINT('Ctrl Pts',(16.6541786621636,18.8159638803859,-2.28502506276829));
#99393=CARTESIAN_POINT('Ctrl Pts',(16.6526671367138,18.824017703857,-2.28551943186517));
#99394=CARTESIAN_POINT('Ctrl Pts',(16.6520164991973,18.8275335901293,-2.28573565729369));
#99395=CARTESIAN_POINT('Ctrl Pts',(16.6506415073593,18.8350703750618,-2.28620005991831));
#99396=CARTESIAN_POINT('Ctrl Pts',(16.6499198953488,18.839091666524,-2.28644838352347));
#99397=CARTESIAN_POINT('Ctrl Pts',(16.6484629280945,18.847348243196,-2.28695931545769));
#99398=CARTESIAN_POINT('Ctrl Pts',(16.647728823752,18.8515837275005,-2.2872219919196));
#99399=CARTESIAN_POINT('Ctrl Pts',(16.6459036982747,18.8623079735055,-2.28788849722442));
#99400=CARTESIAN_POINT('Ctrl Pts',(16.6448300284559,18.8687995878549,-2.28829325045048));
#99401=CARTESIAN_POINT('Ctrl Pts',(16.6260486277417,18.9857393177545,-2.29560661568504));
#99402=CARTESIAN_POINT('Ctrl Pts',(16.6170944893144,19.0973991701253,-2.30293656026631));
#99403=CARTESIAN_POINT('Ctrl Pts',(16.6170007438825,19.2092252893056,-2.31031846004158));
#99404=CARTESIAN_POINT('Ctrl Pts',(16.6170007453236,19.2092235711201,-2.3103183466202));
#99405=CARTESIAN_POINT('Ctrl Pts',(16.616915726726,19.3105416197922,-2.31700658397897));
#99406=CARTESIAN_POINT('Ctrl Pts',(16.6241043877404,19.4117441614251,-2.32371994782463));
#99407=CARTESIAN_POINT('Ctrl Pts',(16.6510544996473,19.5993334501703,-2.33599024637347));
#99408=CARTESIAN_POINT('Ctrl Pts',(16.6690366514094,19.6857574113246,-2.34157366617144));
#99409=CARTESIAN_POINT('Ctrl Pts',(16.6977848563464,19.7906013373736,-2.34824548702124));
#99410=CARTESIAN_POINT('Ctrl Pts',(16.7034969581734,19.8103056525321,-2.34949514501999));
#99411=CARTESIAN_POINT('Ctrl Pts',(16.7120848616136,19.8383967346214,-2.35127113872248));
#99412=CARTESIAN_POINT('Ctrl Pts',(16.7147281849366,19.8468528368021,-2.35180503175381));
#99413=CARTESIAN_POINT('Ctrl Pts',(16.7194026267877,19.8614834108317,-2.3527275766178));
#99414=CARTESIAN_POINT('Ctrl Pts',(16.7214092264388,19.8676655340124,-2.35311702758627));
#99415=CARTESIAN_POINT('Ctrl Pts',(16.7253221591816,19.8795344444876,-2.35386405145122));
#99416=CARTESIAN_POINT('Ctrl Pts',(16.7272242480617,19.8852225554174,-2.35422175979312));
#99417=CARTESIAN_POINT('Ctrl Pts',(16.7322704291892,19.9001023844301,-2.35515676684877));
#99418=CARTESIAN_POINT('Ctrl Pts',(16.7354536847999,19.9092807470241,-2.35573276596104));
#99419=CARTESIAN_POINT('Ctrl Pts',(16.7467207709941,19.9410591482834,-2.35772473922642));
#99420=CARTESIAN_POINT('Ctrl Pts',(16.75512586698,19.9635439049138,-2.3591300440431));
#99421=CARTESIAN_POINT('Ctrl Pts',(16.8192012734972,20.1264516444741,-2.36929205006344));
#99422=CARTESIAN_POINT('Ctrl Pts',(16.8893769880301,20.2607040579724,-2.37751638336487));
#99423=CARTESIAN_POINT('Ctrl Pts',(17.0104437718363,20.4420686199338,-2.38935807424816));
#99424=CARTESIAN_POINT('Ctrl Pts',(17.0502560833175,20.4959832322531,-2.39299171086651));
#99425=CARTESIAN_POINT('Ctrl Pts',(17.1266257048819,20.5897484999617,-2.39967841622019));
#99426=CARTESIAN_POINT('Ctrl Pts',(17.1622799555692,20.6302585571004,-2.40270475103767));
#99427=CARTESIAN_POINT('Ctrl Pts',(17.2186821763871,20.6896078423788,-2.40743001718127));
#99428=CARTESIAN_POINT('Ctrl Pts',(17.2383225651946,20.7094719213274,-2.40906497406223));
#99429=CARTESIAN_POINT('Ctrl Pts',(17.2632324094003,20.7336877807824,-2.41113480030659));
#99430=CARTESIAN_POINT('Ctrl Pts',(17.2681385286067,20.7384113810998,-2.41154228590584));
#99431=CARTESIAN_POINT('Ctrl Pts',(17.276023810327,20.7459303304026,-2.41219709676157));
#99432=CARTESIAN_POINT('Ctrl Pts',(17.2789884673509,20.748740917077,-2.41244326280438));
#99433=CARTESIAN_POINT('Ctrl Pts',(17.2845632807302,20.7539954577843,-2.41290615429137));
#99434=CARTESIAN_POINT('Ctrl Pts',(17.2871715001504,20.7564413859003,-2.41312272352551));
#99435=CARTESIAN_POINT('Ctrl Pts',(17.2931634827415,20.7620320660284,-2.41362025185677));
#99436=CARTESIAN_POINT('Ctrl Pts',(17.2965513410501,20.765172349279,-2.41390154580439));
#99437=CARTESIAN_POINT('Ctrl Pts',(17.307080934092,20.7748685893667,-2.41477571628584));
#99438=CARTESIAN_POINT('Ctrl Pts',(17.3142573268096,20.7813864871993,-2.41537135834745));
#99439=CARTESIAN_POINT('Ctrl Pts',(17.3958893893346,20.8545112186955,-2.42214262180574));
#99440=CARTESIAN_POINT('Ctrl Pts',(17.4749172679588,20.9158093931919,-2.42865320554723));
#99441=CARTESIAN_POINT('Ctrl Pts',(17.6998425835254,21.0660798275081,-2.44647593700132));
#99442=CARTESIAN_POINT('Ctrl Pts',(17.8526864934017,21.14338380602,-2.45780560408483));
#99443=CARTESIAN_POINT('Ctrl Pts',(18.0407436312296,21.2114861330929,-2.47033978586432));
#99444=CARTESIAN_POINT('Ctrl Pts',(18.0685251761512,21.2208986425922,-2.47215989962421));
#99445=CARTESIAN_POINT('Ctrl Pts',(18.1167827612908,21.2361381544597,-2.47526807927265));
#99446=CARTESIAN_POINT('Ctrl Pts',(18.1371670536833,21.242239067777,-2.4765648267941));
#99447=CARTESIAN_POINT('Ctrl Pts',(18.166291081568,21.25047944537,-2.47839524803608));
#99448=CARTESIAN_POINT('Ctrl Pts',(18.1749573133718,21.2528719603782,-2.47893712926988));
#99449=CARTESIAN_POINT('Ctrl Pts',(18.189937141537,21.2569049716091,-2.47986906540596));
#99450=CARTESIAN_POINT('Ctrl Pts',(18.196243511701,21.2585716123213,-2.48025996444069));
#99451=CARTESIAN_POINT('Ctrl Pts',(18.2083351831741,21.2617074697892,-2.48100675098293));
#99452=CARTESIAN_POINT('Ctrl Pts',(18.2141191829561,21.2631814158332,-2.48136278833935));
#99453=CARTESIAN_POINT('Ctrl Pts',(18.2291803387941,21.2669517130647,-2.48228684940491));
#99454=CARTESIAN_POINT('Ctrl Pts',(18.2384670148812,21.2692097565617,-2.48285363310706));
#99455=CARTESIAN_POINT('Ctrl Pts',(18.2702097351164,21.2767006637273,-2.48478101503239));
#99456=CARTESIAN_POINT('Ctrl Pts',(18.2927363233567,21.2816296315469,-2.48613186100627));
#99457=CARTESIAN_POINT('Ctrl Pts',(18.4864623569375,21.3207130051364,-2.49761503257089));
#99458=CARTESIAN_POINT('Ctrl Pts',(18.6611960902983,21.3339390428514,-2.50700554760839));
#99459=CARTESIAN_POINT('Ctrl Pts',(18.9231250715244,21.3213558236439,-2.52127175192693));
#99460=CARTESIAN_POINT('Ctrl Pts',(19.0103131151477,21.3117185972704,-2.5260677647394));
#99461=CARTESIAN_POINT('Ctrl Pts',(19.134067892197,21.2902011619123,-2.53323830618952));
#99462=CARTESIAN_POINT('Ctrl Pts',(19.1713060297255,21.2826888816811,-2.53544442749617));
#99463=CARTESIAN_POINT('Ctrl Pts',(19.2157074006118,21.272481130113,-2.53815504940848));
#99464=CARTESIAN_POINT('Ctrl Pts',(19.223086241022,21.2707429729266,-2.53860819242691));
#99465=CARTESIAN_POINT('Ctrl Pts',(19.2345230353907,21.2679840055428,-2.53931492556288));
#99466=CARTESIAN_POINT('Ctrl Pts',(19.2385876525667,21.2669907120893,-2.53956695956276));
#99467=CARTESIAN_POINT('Ctrl Pts',(19.2461084882052,21.2651291575041,-2.54003494550051));
#99468=CARTESIAN_POINT('Ctrl Pts',(19.2495654691785,21.2642642172432,-2.54025070484568));
#99469=CARTESIAN_POINT('Ctrl Pts',(19.2573611476283,21.2622928015224,-2.54073871236004));
#99470=CARTESIAN_POINT('Ctrl Pts',(19.2616985029387,21.2611812938295,-2.5410112466961));
#99471=CARTESIAN_POINT('Ctrl Pts',(19.2744470798398,21.2578711578748,-2.54181522036926));
#99472=CARTESIAN_POINT('Ctrl Pts',(19.2828482030478,21.2556344971907,-2.54234878117279));
#99473=CARTESIAN_POINT('Ctrl Pts',(19.3421863819696,21.239444627566,-2.54614281721492));
#99474=CARTESIAN_POINT('Ctrl Pts',(19.3925951488972,21.2236424677904,-2.5494984486381));
#99475=CARTESIAN_POINT('Ctrl Pts',(19.4570269869958,21.2007646504455,-2.55391577498353));
#99476=CARTESIAN_POINT('Ctrl Pts',(19.4716402352252,21.1953936742222,-2.55492638070868));
#99477=CARTESIAN_POINT('Ctrl Pts',(19.6180919115667,21.1397253820128,-2.56513472761021));
#99478=CARTESIAN_POINT('Ctrl Pts',(19.7446502528874,21.0765266625902,-2.57458272746252));
#99479=CARTESIAN_POINT('Ctrl Pts',(19.9499321592801,20.9469515977538,-2.59033250513701));
#99480=CARTESIAN_POINT('Ctrl Pts',(20.0318701673413,20.8865766933043,-2.59676211479777));
#99481=CARTESIAN_POINT('Ctrl Pts',(20.1203930948011,20.8109441717258,-2.60386217551483));
#99482=CARTESIAN_POINT('Ctrl Pts',(20.1315224428851,20.8012321229728,-2.60475802605912));
#99483=CARTESIAN_POINT('Ctrl Pts',(20.1483432162397,20.7862404573462,-2.60611719572834));
#99484=CARTESIAN_POINT('Ctrl Pts',(20.1541085918524,20.7810448470131,-2.60658400468454));
#99485=CARTESIAN_POINT('Ctrl Pts',(20.1645471638488,20.7715333300532,-2.60743098057794));
#99486=CARTESIAN_POINT('Ctrl Pts',(20.1692297071773,20.7672278596677,-2.60781158161727));
#99487=CARTESIAN_POINT('Ctrl Pts',(20.1792983518375,20.7578859195777,-2.60863144837453));
#99488=CARTESIAN_POINT('Ctrl Pts',(20.184677700351,20.7528422700866,-2.60907040059836));
#99489=CARTESIAN_POINT('Ctrl Pts',(20.1991959300207,20.7390868093347,-2.61025768541833));
#99490=CARTESIAN_POINT('Ctrl Pts',(20.2082834975006,20.7303210949628,-2.61100368404767));
#99491=CARTESIAN_POINT('Ctrl Pts',(20.2521491909447,20.6872448001146,-2.61461938551674));
#99492=CARTESIAN_POINT('Ctrl Pts',(20.2858125643751,20.6518171230195,-2.61743945916776));
#99493=CARTESIAN_POINT('Ctrl Pts',(20.3452568888793,20.5847544751773,-2.62253173164243));
#99494=CARTESIAN_POINT('Ctrl Pts',(20.3714063039008,20.5534794077522,-2.62481624401318));
#99495=CARTESIAN_POINT('Ctrl Pts',(20.4697864995513,20.4286609130493,-2.63363530300484));
#99496=CARTESIAN_POINT('Ctrl Pts',(20.5350358570186,20.3298936949913,-2.63997299850123));
#99497=CARTESIAN_POINT('Ctrl Pts',(20.6275059368221,20.1606831698113,-2.65050617048442));
#99498=CARTESIAN_POINT('Ctrl Pts',(20.6598146038472,20.0933260463539,-2.65462747392556));
#99499=CARTESIAN_POINT('Ctrl Pts',(20.701757070452,19.992544824345,-2.66088162903481));
#99500=CARTESIAN_POINT('Ctrl Pts',(20.7142361359487,19.9603628877799,-2.66289150203385));
#99501=CARTESIAN_POINT('Ctrl Pts',(20.728418654839,19.9209560378632,-2.66538441873089));
#99502=CARTESIAN_POINT('Ctrl Pts',(20.7308787908355,19.9140067123074,-2.6658252267002));
#99503=CARTESIAN_POINT('Ctrl Pts',(20.7346633078189,19.9031361556126,-2.6665168226936));
#99504=CARTESIAN_POINT('Ctrl Pts',(20.736012598243,19.8992235719312,-2.6667661598703));
#99505=CARTESIAN_POINT('Ctrl Pts',(20.7385037790302,19.8919304895642,-2.66723174114806));
#99506=CARTESIAN_POINT('Ctrl Pts',(20.7396485991476,19.8885510518587,-2.66744780917107));
#99507=CARTESIAN_POINT('Ctrl Pts',(20.7422303640487,19.8808659629102,-2.66793990345803));
#99508=CARTESIAN_POINT('Ctrl Pts',(20.7436620016921,19.8765585935295,-2.66821623705707));
#99509=CARTESIAN_POINT('Ctrl Pts',(20.7478851138569,19.8637146498074,-2.66904170753367));
#99510=CARTESIAN_POINT('Ctrl Pts',(20.7506360864048,19.8551650055277,-2.66959313536422));
#99511=CARTESIAN_POINT('Ctrl Pts',(20.7714940869043,19.7888979320506,-2.67388080436279));
#99512=CARTESIAN_POINT('Ctrl Pts',(20.7871725011374,19.7304510700462,-2.6777416507676));
#99513=CARTESIAN_POINT('Ctrl Pts',(20.8134037128092,19.6127274994457,-2.68557058491372));
#99514=CARTESIAN_POINT('Ctrl Pts',(20.8239744762868,19.5535068930085,-2.68953441005239));
#99515=CARTESIAN_POINT('Ctrl Pts',(20.8465547164529,19.3860612107819,-2.70069675926838));
#99516=CARTESIAN_POINT('Ctrl Pts',(20.8527615264669,19.2772339121808,-2.70788988127502));
#99517=CARTESIAN_POINT('Ctrl Pts',(20.8490659444797,19.0935944048813,-2.71968984222296));
#99518=CARTESIAN_POINT('Ctrl Pts',(20.8435950501378,19.0189091960864,-2.72439711894139));
#99519=CARTESIAN_POINT('Ctrl Pts',(20.8318167920761,18.9260326723945,-2.73013216987657));
#99520=CARTESIAN_POINT('Ctrl Pts',(20.8292063116425,18.9074341615935,-2.73127477248517));
#99521=CARTESIAN_POINT('Ctrl Pts',(20.8250477688962,18.8804227527477,-2.73292614710874));
#99522=CARTESIAN_POINT('Ctrl Pts',(20.8236957219795,18.8719810018652,-2.73344109325815));
#99523=CARTESIAN_POINT('Ctrl Pts',(20.8212342143084,18.8571866076319,-2.73434159695733));
#99524=CARTESIAN_POINT('Ctrl Pts',(20.8201468027287,18.8508304553537,-2.73472784867144));
#99525=CARTESIAN_POINT('Ctrl Pts',(20.8179778700571,18.8384920235643,-2.73547643613149));
#99526=CARTESIAN_POINT('Ctrl Pts',(20.8168995907418,18.8325092451995,-2.73583887075416));
#99527=CARTESIAN_POINT('Ctrl Pts',(20.8142585491144,18.8182087143678,-2.73670392165712));
#99528=CARTESIAN_POINT('Ctrl Pts',(20.8126716421405,18.8098954842522,-2.7372057656217));
#99529=CARTESIAN_POINT('Ctrl Pts',(20.8067544080408,18.7798758001871,-2.73901441726628));
#99530=CARTESIAN_POINT('Ctrl Pts',(20.8021334856037,18.7582275936779,-2.74031196608073));
#99531=CARTESIAN_POINT('Ctrl Pts',(20.755648006654,18.5560379115105,-2.75237780083063));
#99532=CARTESIAN_POINT('Ctrl Pts',(20.6905881497839,18.381659991534,-2.76229230394082));
#99533=CARTESIAN_POINT('Ctrl Pts',(20.5659759708226,18.1470438304773,-2.77677352323143));
#99534=CARTESIAN_POINT('Ctrl Pts',(20.5243020089875,18.0783237933446,-2.78118953506107));
#99535=CARTESIAN_POINT('Ctrl Pts',(20.4584000975061,17.9824094512677,-2.78784585150284));
#99536=CARTESIAN_POINT('Ctrl Pts',(20.4372152844464,17.953205192522,-2.78994414931373));
#99537=CARTESIAN_POINT('Ctrl Pts',(20.410757542257,17.9186266289342,-2.79253521455693));
#99538=CARTESIAN_POINT('Ctrl Pts',(20.4061875651719,17.9127190100488,-2.79298175051942));
#99539=CARTESIAN_POINT('Ctrl Pts',(20.3990238070851,17.9035589777024,-2.79368037788817));
#99540=CARTESIAN_POINT('Ctrl Pts',(20.3964514867217,17.9002897503417,-2.79393096996523));
#99541=CARTESIAN_POINT('Ctrl Pts',(20.3916563357817,17.8942322954638,-2.79439765784973));
#99542=CARTESIAN_POINT('Ctrl Pts',(20.3894360903565,17.8914420947124,-2.79461356985555));
#99543=CARTESIAN_POINT('Ctrl Pts',(20.3843918867449,17.8851357694261,-2.79510370627398));
#99544=CARTESIAN_POINT('Ctrl Pts',(20.3815637505502,17.8816230689712,-2.79537822793867));
#99545=CARTESIAN_POINT('Ctrl Pts',(20.374233244835,17.8725775006318,-2.79608899700515));
#99546=CARTESIAN_POINT('Ctrl Pts',(20.3697141375818,17.8670583565179,-2.79652641012653));
#99547=CARTESIAN_POINT('Ctrl Pts',(20.3418046051799,17.8333219974645,-2.79922262100264));
#99548=CARTESIAN_POINT('Ctrl Pts',(20.3177140423278,17.8056951269798,-2.8015275691923));
#99549=CARTESIAN_POINT('Ctrl Pts',(20.1775031367678,17.6530880782193,-2.8147528921501));
#99550=CARTESIAN_POINT('Ctrl Pts',(20.0473267844066,17.541878455085,-2.82626398317437));
#99551=CARTESIAN_POINT('Ctrl Pts',(19.8257962925328,17.3947515275174,-2.84354582263158));
#99552=CARTESIAN_POINT('Ctrl Pts',(19.7429007297666,17.3474278332049,-2.84960274492326));
#99553=CARTESIAN_POINT('Ctrl Pts',(19.6378408759582,17.2965240889397,-2.85677366252124));
#99554=CARTESIAN_POINT('Ctrl Pts',(19.6184546381155,17.287491125867,-2.85807719036012));
#99555=CARTESIAN_POINT('Ctrl Pts',(19.5907117025869,17.2750725176694,-2.85991542967627));
#99556=CARTESIAN_POINT('Ctrl Pts',(19.5824656181997,17.2714443145796,-2.86045844438309));
#99557=CARTESIAN_POINT('Ctrl Pts',(19.5682063546996,17.2652787073771,-2.86139171707981));
#99558=CARTESIAN_POINT('Ctrl Pts',(19.5622041891893,17.2627162903526,-2.86178282562564));
#99559=CARTESIAN_POINT('Ctrl Pts',(19.5506935440632,17.2578650238011,-2.86252959604228));
#99560=CARTESIAN_POINT('Ctrl Pts',(19.5451870611022,17.2555716241223,-2.86288540976373));
#99561=CARTESIAN_POINT('Ctrl Pts',(19.5308527615449,17.249672488838,-2.86380799082697));
#99562=CARTESIAN_POINT('Ctrl Pts',(19.5220100821921,17.2461030448116,-2.86437352616462));
#99563=CARTESIAN_POINT('Ctrl Pts',(19.4918251342721,17.2341551040104,-2.86629205257813));
#99564=CARTESIAN_POINT('Ctrl Pts',(19.4703705370113,17.226063434367,-2.86763541446476));
#99565=CARTESIAN_POINT('Ctrl Pts',(19.2828153238359,17.1587860275195,-2.8792146453731));
#99566=CARTESIAN_POINT('Ctrl Pts',(19.1100575384729,17.1202183673649,-2.88869114687395));
#99567=CARTESIAN_POINT('Ctrl Pts',(18.8484807130938,17.0953322329895,-2.90299000891541));
#99568=CARTESIAN_POINT('Ctrl Pts',(18.7620438558293,17.0924233279127,-2.90772244744911));
#99569=CARTESIAN_POINT('Ctrl Pts',(18.6380204629066,17.0958413387308,-2.91480728427978));
#99570=CARTESIAN_POINT('Ctrl Pts',(18.6003990385863,17.0978841436868,-2.91699583607903));
#99571=CARTESIAN_POINT('Ctrl Pts',(18.5553165097138,17.1015407302542,-2.91968698448819));
#99572=CARTESIAN_POINT('Ctrl Pts',(18.547781628787,17.1021925373026,-2.92013907789111));
#99573=CARTESIAN_POINT('Ctrl Pts',(18.5360876768861,17.1032672873211,-2.92084452367938));
#99574=CARTESIAN_POINT('Ctrl Pts',(18.5319260058597,17.1036622064947,-2.92109632903089));
#99575=CARTESIAN_POINT('Ctrl Pts',(18.5242185796754,17.1044166388692,-2.92156410733076));
#99576=CARTESIAN_POINT('Ctrl Pts',(18.5206725524296,17.1047727802453,-2.92177988907489));
#99577=CARTESIAN_POINT('Ctrl Pts',(18.5126684751859,17.1055970814703,-2.92226822596466));
#99578=CARTESIAN_POINT('Ctrl Pts',(18.508211028365,17.1060704447268,-2.92254106900114));
#99579=CARTESIAN_POINT('Ctrl Pts',(18.4950898198076,17.1075060226235,-2.92334677932452));
#99580=CARTESIAN_POINT('Ctrl Pts',(18.486430581789,17.1085075828382,-2.92388178153363));
#99581=CARTESIAN_POINT('Ctrl Pts',(18.4248686020642,17.1160136529679,-2.92770748962769));
#99582=CARTESIAN_POINT('Ctrl Pts',(18.3722263723868,17.1244600833069,-2.93109510204498));
#99583=CARTESIAN_POINT('Ctrl Pts',(18.3023671160317,17.1383919761581,-2.93569881183349));
#99584=CARTESIAN_POINT('Ctrl Pts',(18.2848158633758,17.1421248097532,-2.93686471372105));
#99585=CARTESIAN_POINT('Ctrl Pts',(18.2202688798785,17.1567128526648,-2.94118221444833));
#99586=CARTESIAN_POINT('Ctrl Pts',(18.1736014733933,17.1689499012762,-2.94436187204783));
#99587=CARTESIAN_POINT('Ctrl Pts',(18.0226008043547,17.2141113934183,-2.95477312449557));
#99588=CARTESIAN_POINT('Ctrl Pts',(17.9203860230035,17.2535300296179,-2.96200570030163));
#99589=CARTESIAN_POINT('Ctrl Pts',(17.7533808690013,17.3332880376191,-2.97390169377441));
#99590=CARTESIAN_POINT('Ctrl Pts',(17.6868836071066,17.3695425464847,-2.97866449906579));
#99591=CARTESIAN_POINT('Ctrl Pts',(17.6063837415456,17.4192054866225,-2.98445945731136));
#99592=CARTESIAN_POINT('Ctrl Pts',(17.5904362901477,17.429341199235,-2.98560915438306));
#99593=CARTESIAN_POINT('Ctrl Pts',(17.567455419989,17.4443828391994,-2.98726882635567));
#99594=CARTESIAN_POINT('Ctrl Pts',(17.560313071366,17.4491199113118,-2.98778506296745));
#99595=CARTESIAN_POINT('Ctrl Pts',(17.5478447386553,17.4574988394124,-2.98868705568223));
#99596=CARTESIAN_POINT('Ctrl Pts',(17.5425063070238,17.4611218884662,-2.98907351302871));
#99597=CARTESIAN_POINT('Ctrl Pts',(17.5321751884177,17.4682025355165,-2.98982194281896));
#99598=CARTESIAN_POINT('Ctrl Pts',(17.5271806582596,17.4716573202705,-2.99018401675394));
#99599=CARTESIAN_POINT('Ctrl Pts',(17.5152808157448,17.4799645360757,-2.99104732297116));
#99600=CARTESIAN_POINT('Ctrl Pts',(17.5083894844323,17.4848368864155,-2.9915477900786));
#99601=CARTESIAN_POINT('Ctrl Pts',(17.483652863754,17.5025491384645,-2.99334628428657));
#99602=CARTESIAN_POINT('Ctrl Pts',(17.4659783115253,17.5156258942739,-2.99463518982757));
#99603=CARTESIAN_POINT('Ctrl Pts',(17.3000934569141,17.6424036877317,-3.00677956299877));
#99604=CARTESIAN_POINT('Ctrl Pts',(17.1673451492009,17.7749704581813,-3.0167651179066));
#99605=CARTESIAN_POINT('Ctrl Pts',(17.0054418802403,17.9862258147212,-3.03127849372914));
#99606=CARTESIAN_POINT('Ctrl Pts',(16.9607582039768,18.0518638786354,-3.03564441507471));
#99607=CARTESIAN_POINT('Ctrl Pts',(16.9014072497951,18.1505399432923,-3.04223259077679));
#99608=CARTESIAN_POINT('Ctrl Pts',(16.8837303565891,18.1816926485078,-3.04431616260788));
#99609=CARTESIAN_POINT('Ctrl Pts',(16.8633406653445,18.2198500600563,-3.04689088952553));
#99610=CARTESIAN_POINT('Ctrl Pts',(16.8598628487978,18.2264419851936,-3.0473364915599));
#99611=CARTESIAN_POINT('Ctrl Pts',(16.8544998901505,18.2367384266318,-3.04803397273379));
#99612=CARTESIAN_POINT('Ctrl Pts',(16.8525906877086,18.2404304377289,-3.04828436049649));
#99613=CARTESIAN_POINT('Ctrl Pts',(16.8490636419453,18.2473005427728,-3.04875086669966));
#99614=CARTESIAN_POINT('Ctrl Pts',(16.8474429517466,18.2504771107082,-3.0489668025912));
#99615=CARTESIAN_POINT('Ctrl Pts',(16.8437887964376,18.2576842149565,-3.0494572508952));
#99616=CARTESIAN_POINT('Ctrl Pts',(16.8417602029554,18.2617171497949,-3.04973206217267));
#99617=CARTESIAN_POINT('Ctrl Pts',(16.8357860112669,18.273689350793,-3.05054888666941));
#99618=CARTESIAN_POINT('Ctrl Pts',(16.8318774264879,18.2816468329169,-3.05109312190785));
#99619=CARTESIAN_POINT('Ctrl Pts',(16.8031430489102,18.3410877591387,-3.05516696600248));
#99620=CARTESIAN_POINT('Ctrl Pts',(16.7803635666302,18.3935287064521,-3.05880791823012));
#99621=CARTESIAN_POINT('Ctrl Pts',(16.7548404642287,18.4594679460122,-3.0633885546121));
#99622=CARTESIAN_POINT('Ctrl Pts',(16.7500682834686,18.4721578996777,-3.0642702345555));
#99623=CARTESIAN_POINT('Ctrl Pts',(16.7454194666968,18.4848894969994,-3.06515441818778));
#99624=CARTESIAN_POINT('',(16.6200858900717,19.2101715454936,-2.08900427075732));
#99625=CARTESIAN_POINT('Ctrl Pts',(16.747777019274,18.4857290362168,-2.84456321874111));
#99626=CARTESIAN_POINT('Ctrl Pts',(16.8351531090644,18.241375047072,-2.82899806149126));
#99627=CARTESIAN_POINT('Ctrl Pts',(17.3199691688815,17.3916717671322,-2.77104096868093));
#99628=CARTESIAN_POINT('Ctrl Pts',(19.0938031543631,16.7337290395393,-2.67069194031012));
#99629=CARTESIAN_POINT('Ctrl Pts',(21.0117474691636,18.1726377106278,-2.54351613362868));
#99630=CARTESIAN_POINT('Ctrl Pts',(20.8399998558895,20.5641793786163,-2.41634032694726));
#99631=CARTESIAN_POINT('Ctrl Pts',(18.736128084209,21.7142628689015,-2.28916452026583));
#99632=CARTESIAN_POINT('Ctrl Pts',(16.9296978888421,20.7307616435956,-2.18006983762423));
#99633=CARTESIAN_POINT('Ctrl Pts',(16.6216056483476,19.6158003190927,-2.11336709054313));
#99634=CARTESIAN_POINT('Ctrl Pts',(16.6201761352154,19.2101685860996,-2.0890562790225));
#99635=CARTESIAN_POINT('Ctrl Pts',(16.6170001249202,19.210272736479,-2.08722594468162));
#99636=CARTESIAN_POINT('Ctrl Pts',(16.6170670028706,19.0155969299224,-2.07601658232614));
#99637=CARTESIAN_POINT('Ctrl Pts',(16.6439835858641,18.8218627412699,-2.0657352630804));
#99638=CARTESIAN_POINT('Ctrl Pts',(16.7112838353467,18.5840556965883,-2.0521523543399));
#99639=CARTESIAN_POINT('Ctrl Pts',(16.7274347386544,18.5341438219612,-2.04923738527145));
#99640=CARTESIAN_POINT('Ctrl Pts',(16.7454194497489,18.4848895434144,-2.04625067101847));
#99641=CARTESIAN_POINT('Origin',(18.734,19.211,0.));
#99642=CARTESIAN_POINT('',(16.7454193884829,18.484889711202,-1.2445862186816));
#99643=CARTESIAN_POINT('',(16.7454194504776,18.4848895414187,-1.46829793832533));
#99644=CARTESIAN_POINT('',(16.7454194503191,18.4848895418526,0.));
#99645=CARTESIAN_POINT('Ctrl Pts',(16.7454194504776,18.4848895414187,-1.46829793832533));
#99646=CARTESIAN_POINT('Ctrl Pts',(16.6959068598972,18.6204884347014,-1.47674751206437));
#99647=CARTESIAN_POINT('Ctrl Pts',(16.6603893501654,18.7608044574327,-1.48469151238656));
#99648=CARTESIAN_POINT('Ctrl Pts',(16.6244283767766,19.0058873144864,-1.49816090940912));
#99649=CARTESIAN_POINT('Ctrl Pts',(16.6169334230905,19.1090662019796,-1.50372410772867));
#99650=CARTESIAN_POINT('Ctrl Pts',(16.617039406997,19.2724280285841,-1.51286250500369));
#99651=CARTESIAN_POINT('Ctrl Pts',(16.6196337799328,19.332448106488,-1.51629223384452));
#99652=CARTESIAN_POINT('Ctrl Pts',(16.6255428333359,19.4012045822417,-1.52038547531305));
#99653=CARTESIAN_POINT('Ctrl Pts',(16.6263673812465,19.4101334846522,-1.52092023865661));
#99654=CARTESIAN_POINT('Ctrl Pts',(16.6276944043495,19.4235707244116,-1.52173020007817));
#99655=CARTESIAN_POINT('Ctrl Pts',(16.6281546984081,19.4280832559857,-1.52200308581255));
#99656=CARTESIAN_POINT('Ctrl Pts',(16.6290029478587,19.4361424884885,-1.5224920827716));
#99657=CARTESIAN_POINT('Ctrl Pts',(16.6293853698041,19.4396897193852,-1.52270788010183));
#99658=CARTESIAN_POINT('Ctrl Pts',(16.6302310217689,19.4473519268589,-1.52317525487703));
#99659=CARTESIAN_POINT('Ctrl Pts',(16.6306973520588,19.451466458332,-1.52342699932537));
#99660=CARTESIAN_POINT('Ctrl Pts',(16.6320285811027,19.462911980543,-1.52412937420652));
#99661=CARTESIAN_POINT('Ctrl Pts',(16.6329197472504,19.4702397724419,-1.52458144421862));
#99662=CARTESIAN_POINT('Ctrl Pts',(16.6382144776853,19.5119550436418,-1.52716799118256));
#99663=CARTESIAN_POINT('Ctrl Pts',(16.6434236348418,19.546232805256,-1.52934379516798));
#99664=CARTESIAN_POINT('Ctrl Pts',(16.6625928168378,19.6544150201489,-1.53633889055484));
#99665=CARTESIAN_POINT('Ctrl Pts',(16.6796496685526,19.7277085866481,-1.54126750918516));
#99666=CARTESIAN_POINT('Ctrl Pts',(16.7543348629841,19.9855767587457,-1.55897624798418));
#99667=CARTESIAN_POINT('Ctrl Pts',(16.833285513439,20.163028807161,-1.57174489460041));
#99668=CARTESIAN_POINT('Ctrl Pts',(16.9464403129331,20.3453589893003,-1.58492997915281));
#99669=CARTESIAN_POINT('Ctrl Pts',(16.9579092292772,20.3632332997938,-1.58622483245215));
#99670=CARTESIAN_POINT('Ctrl Pts',(16.9742421772088,20.3878647287892,-1.58801295848453));
#99671=CARTESIAN_POINT('Ctrl Pts',(16.9788797317359,20.3947698390144,-1.58851465949724));
#99672=CARTESIAN_POINT('Ctrl Pts',(16.9869555310392,20.4066425543119,-1.58937807984382));
#99673=CARTESIAN_POINT('Ctrl Pts',(16.9903745393692,20.4116230667551,-1.58974052067012));
#99674=CARTESIAN_POINT('Ctrl Pts',(16.9974994140815,20.4219073361421,-1.59048945997367));
#99675=CARTESIAN_POINT('Ctrl Pts',(17.0012083737823,20.4272088813858,-1.59087583543189));
#99676=CARTESIAN_POINT('Ctrl Pts',(17.0099527897475,20.4395868491681,-1.59177868363988));
#99677=CARTESIAN_POINT('Ctrl Pts',(17.0150076272013,20.4466494870373,-1.59229440641937));
#99678=CARTESIAN_POINT('Ctrl Pts',(17.0315678467597,20.4694891907515,-1.59396423982988));
#99679=CARTESIAN_POINT('Ctrl Pts',(17.0432482868361,20.4851385175056,-1.59511156994434));
#99680=CARTESIAN_POINT('Ctrl Pts',(17.1041455565418,20.5644156735477,-1.6009440164131));
#99681=CARTESIAN_POINT('Ctrl Pts',(17.156746131161,20.6253662046906,-1.60549250894985));
#99682=CARTESIAN_POINT('Ctrl Pts',(17.329516928172,20.8039023620081,-1.61926735349304));
#99683=CARTESIAN_POINT('Ctrl Pts',(17.4602834086994,20.9102790533472,-1.62810921921722));
#99684=CARTESIAN_POINT('Ctrl Pts',(17.6034464149036,21.0008434689676,-1.63762169540562));
#99685=CARTESIAN_POINT('Ctrl Pts',(17.6046578327881,21.0016080870819,-1.63770218047912));
#99686=CARTESIAN_POINT('Ctrl Pts',(17.6514439486952,21.0310720037534,-1.64081033113675));
#99687=CARTESIAN_POINT('Ctrl Pts',(17.6980925138912,21.0580203944255,-1.64389965447141));
#99688=CARTESIAN_POINT('Ctrl Pts',(17.7534414804455,21.0872383539285,-1.64761364329193));
#99689=CARTESIAN_POINT('Ctrl Pts',(17.7611948552407,21.0912700644848,-1.64813498479443));
#99690=CARTESIAN_POINT('Ctrl Pts',(17.7729667913062,21.0972991034811,-1.6489285015261));
#99691=CARTESIAN_POINT('Ctrl Pts',(17.7769672159459,21.0993319055185,-1.64919850135907));
#99692=CARTESIAN_POINT('Ctrl Pts',(17.7841567114073,21.1029565087954,-1.64968440566121));
#99693=CARTESIAN_POINT('Ctrl Pts',(17.7873433637962,21.1045529876125,-1.64990001267127));
#99694=CARTESIAN_POINT('Ctrl Pts',(17.7942731517909,21.1080028720176,-1.65036940213231));
#99695=CARTESIAN_POINT('Ctrl Pts',(17.7980176958408,21.109853225316,-1.6506233647053));
#99696=CARTESIAN_POINT('Ctrl Pts',(17.8085430972304,21.115015617342,-1.65133807963303));
#99697=CARTESIAN_POINT('Ctrl Pts',(17.8153361449886,21.1183024583224,-1.65180035323353));
#99698=CARTESIAN_POINT('Ctrl Pts',(17.8558858092826,21.1376556801787,-1.65456508847729));
#99699=CARTESIAN_POINT('Ctrl Pts',(17.8900434268716,21.1528608466435,-1.65691568048034));
#99700=CARTESIAN_POINT('Ctrl Pts',(18.0033889318725,21.1997609526478,-1.66474435179443));
#99701=CARTESIAN_POINT('Ctrl Pts',(18.0840883256608,21.2275752166946,-1.67036021279631));
#99702=CARTESIAN_POINT('Ctrl Pts',(18.3376409819696,21.298161707302,-1.68774741306462));
#99703=CARTESIAN_POINT('Ctrl Pts',(18.5144113666176,21.3240900869336,-1.69943889571769));
#99704=CARTESIAN_POINT('Ctrl Pts',(18.7151610050707,21.3280389542826,-1.71179548129477));
#99705=CARTESIAN_POINT('Ctrl Pts',(18.7379630520414,21.3281190801895,-1.71318717444918));
#99706=CARTESIAN_POINT('Ctrl Pts',(18.7702766298393,21.3277105461314,-1.71514331801955));
#99707=CARTESIAN_POINT('Ctrl Pts',(18.7797897934904,21.3275261230166,-1.71571723815169));
#99708=CARTESIAN_POINT('Ctrl Pts',(18.7952605951424,21.3271218477167,-1.71664745239659));
#99709=CARTESIAN_POINT('Ctrl Pts',(18.80121903906,21.3269409577818,-1.71700496234333));
#99710=CARTESIAN_POINT('Ctrl Pts',(18.8137023079373,21.3265092003526,-1.71775241537211));
#99711=CARTESIAN_POINT('Ctrl Pts',(18.8202269050533,21.3262533079952,-1.71814219699084));
#99712=CARTESIAN_POINT('Ctrl Pts',(18.8357688326794,21.3255717286431,-1.71906861099234));
#99713=CARTESIAN_POINT('Ctrl Pts',(18.8447848767661,21.3251185410959,-1.71960437601916));
#99714=CARTESIAN_POINT('Ctrl Pts',(18.8752584349786,21.3233913204335,-1.72140982091528));
#99715=CARTESIAN_POINT('Ctrl Pts',(18.8966997974882,21.3218481380876,-1.72267106597266));
#99716=CARTESIAN_POINT('Ctrl Pts',(19.0969130637548,21.3043694531506,-1.73437254793194));
#99717=CARTESIAN_POINT('Ctrl Pts',(19.2729982710574,21.2660886617846,-1.74401575230736));
#99718=CARTESIAN_POINT('Ctrl Pts',(19.555684578965,21.1657470774263,-1.76034091505661));
#99719=CARTESIAN_POINT('Ctrl Pts',(19.6655505568961,21.1158377291937,-1.76695024492803));
#99720=CARTESIAN_POINT('Ctrl Pts',(19.778840346635,21.0522191183713,-1.77465072814509));
#99721=CARTESIAN_POINT('Ctrl Pts',(19.787089422591,21.0475135045075,-1.77521680930884));
#99722=CARTESIAN_POINT('Ctrl Pts',(19.7992700049658,21.0404561488919,-1.77606110946159));
#99723=CARTESIAN_POINT('Ctrl Pts',(19.8032261192575,21.0381468165396,-1.77633665612269));
#99724=CARTESIAN_POINT('Ctrl Pts',(19.8102535521807,21.0340140014688,-1.77682854672267));
#99725=CARTESIAN_POINT('Ctrl Pts',(19.8133277818173,21.032195568109,-1.77704456167691));
#99726=CARTESIAN_POINT('Ctrl Pts',(19.8199297122953,21.0282678814746,-1.77751026300074));
#99727=CARTESIAN_POINT('Ctrl Pts',(19.8234558251876,21.0261561633606,-1.77776010497034));
#99728=CARTESIAN_POINT('Ctrl Pts',(19.833177523092,21.0202955018174,-1.77845195410065));
#99729=CARTESIAN_POINT('Ctrl Pts',(19.8393599879735,21.0165250576118,-1.77889533280146));
#99730=CARTESIAN_POINT('Ctrl Pts',(19.8732142644036,20.9956396039212,-1.78134142065681));
#99731=CARTESIAN_POINT('Ctrl Pts',(19.9005064094762,20.9779211028227,-1.78338047178864));
#99732=CARTESIAN_POINT('Ctrl Pts',(20.0617654452043,20.8678645363204,-1.79578646284055));
#99733=CARTESIAN_POINT('Ctrl Pts',(20.1851285139736,20.760963591564,-1.80674330176059));
#99734=CARTESIAN_POINT('Ctrl Pts',(20.3739337424721,20.5548567574695,-1.82500089877527));
#99735=CARTESIAN_POINT('Ctrl Pts',(20.4455824257093,20.4623301204311,-1.83244165709588));
#99736=CARTESIAN_POINT('Ctrl Pts',(20.5170242067805,20.3523666643615,-1.84044863649234));
#99737=CARTESIAN_POINT('Ctrl Pts',(20.52468770223,20.3403054295805,-1.84131661054526));
#99738=CARTESIAN_POINT('Ctrl Pts',(20.5366901839651,20.3209858463645,-1.84269091606629));
#99739=CARTESIAN_POINT('Ctrl Pts',(20.5411087162168,20.3137776609572,-1.84320017559491));
#99740=CARTESIAN_POINT('Ctrl Pts',(20.5488253311113,20.3010182138872,-1.84409555187577));
#99741=CARTESIAN_POINT('Ctrl Pts',(20.5521413978991,20.295478007028,-1.84448232475353));
#99742=CARTESIAN_POINT('Ctrl Pts',(20.5589476627747,20.2839877031702,-1.84528039192358));
#99743=CARTESIAN_POINT('Ctrl Pts',(20.5624342331843,20.278035538149,-1.84569155083534));
#99744=CARTESIAN_POINT('Ctrl Pts',(20.5713090994871,20.262713411274,-1.8467442585542));
#99745=CARTESIAN_POINT('Ctrl Pts',(20.5766548835802,20.2533189593826,-1.84738426606248));
#99746=CARTESIAN_POINT('Ctrl Pts',(20.5986659935689,20.2139389661409,-1.850044925651));
#99747=CARTESIAN_POINT('Ctrl Pts',(20.6146737328174,20.1835905328897,-1.85204204905034));
#99748=CARTESIAN_POINT('Ctrl Pts',(20.6544539887068,20.1035144393947,-1.8571861135451));
#99749=CARTESIAN_POINT('Ctrl Pts',(20.6770353651403,20.0532231073029,-1.8602936657903));
#99750=CARTESIAN_POINT('Ctrl Pts',(20.7384915575997,19.9006805087424,-1.86943806290884));
#99751=CARTESIAN_POINT('Ctrl Pts',(20.7714348766994,19.7962397931314,-1.87532617814154));
#99752=CARTESIAN_POINT('Ctrl Pts',(20.8065009483781,19.6451877511086,-1.8837687736118));
#99753=CARTESIAN_POINT('Ctrl Pts',(20.8153937493393,19.6003314877986,-1.88626856698705));
#99754=CARTESIAN_POINT('Ctrl Pts',(20.8265370763613,19.5327113081147,-1.89006869277782));
#99755=CARTESIAN_POINT('Ctrl Pts',(20.8298827144741,19.5101407308908,-1.89134240181201));
#99756=CARTESIAN_POINT('Ctrl Pts',(20.8330068333032,19.4864279025798,-1.8926900312721));
#99757=CARTESIAN_POINT('Ctrl Pts',(20.8331500026186,19.4853346173429,-1.89275218508388));
#99758=CARTESIAN_POINT('Ctrl Pts',(20.8397581739754,19.4345645203354,-1.89563948799598));
#99759=CARTESIAN_POINT('Ctrl Pts',(20.8444581568153,19.3846781249981,-1.89852074748396));
#99760=CARTESIAN_POINT('Ctrl Pts',(20.8478413750193,19.3268656945797,-1.90195836270283));
#99761=CARTESIAN_POINT('Ctrl Pts',(20.8482551558296,19.3190525321089,-1.90242502334476));
#99762=CARTESIAN_POINT('Ctrl Pts',(20.8488465800877,19.3065757422154,-1.90317380144847));
#99763=CARTESIAN_POINT('Ctrl Pts',(20.849052133623,19.3019134253639,-1.90345439982381));
#99764=CARTESIAN_POINT('Ctrl Pts',(20.8493885683665,19.2936625649046,-1.9039524395378));
#99765=CARTESIAN_POINT('Ctrl Pts',(20.8495257375652,19.2900743217089,-1.90416952603827));
#99766=CARTESIAN_POINT('Ctrl Pts',(20.849796819096,19.2824766611927,-1.90463024391723));
#99767=CARTESIAN_POINT('Ctrl Pts',(20.8499284627948,19.2784672699049,-1.90487399344614));
#99768=CARTESIAN_POINT('Ctrl Pts',(20.8502524268373,19.2676644023794,-1.9055323819951));
#99769=CARTESIAN_POINT('Ctrl Pts',(20.8504234285035,19.2608704017992,-1.90594818576546));
#99770=CARTESIAN_POINT('Ctrl Pts',(20.8511046952856,19.2273958503391,-1.90800505444492));
#99771=CARTESIAN_POINT('Ctrl Pts',(20.8511431376046,19.2007094233868,-1.90967037746517));
#99772=CARTESIAN_POINT('Ctrl Pts',(20.8498011711394,19.1238747345776,-1.9145252321067));
#99773=CARTESIAN_POINT('Ctrl Pts',(20.8471427593648,19.0737687499926,-1.91776473227241));
#99774=CARTESIAN_POINT('Ctrl Pts',(20.8311335823854,18.8934261565449,-1.92958818445611));
#99775=CARTESIAN_POINT('Ctrl Pts',(20.8074923777699,18.7643968725743,-1.93833645646128));
#99776=CARTESIAN_POINT('Ctrl Pts',(20.7435780671029,18.5369145299891,-1.95370070928406));
#99777=CARTESIAN_POINT('Ctrl Pts',(20.7075330014761,18.4377157463494,-1.96038329006193));
#99778=CARTESIAN_POINT('Ctrl Pts',(20.6584568122342,18.3287565869069,-1.96767812183041));
#99779=CARTESIAN_POINT('Ctrl Pts',(20.6525431892436,18.3159695490272,-1.96853368315175));
#99780=CARTESIAN_POINT('Ctrl Pts',(20.6429021319407,18.2956573636174,-1.96989210251203));
#99781=CARTESIAN_POINT('Ctrl Pts',(20.6392568829303,18.288093880979,-1.97039778420121));
#99782=CARTESIAN_POINT('Ctrl Pts',(20.6327330440303,18.2747610376537,-1.97128900800427));
#99783=CARTESIAN_POINT('Ctrl Pts',(20.6298729306371,18.268982803017,-1.97167518707565));
#99784=CARTESIAN_POINT('Ctrl Pts',(20.6238872568839,18.2570277380775,-1.97247409306763));
#99785=CARTESIAN_POINT('Ctrl Pts',(20.6207577032444,18.2508529845656,-1.97288667440835));
#99786=CARTESIAN_POINT('Ctrl Pts',(20.6126136484626,18.2349779733188,-1.97394733597398));
#99787=CARTESIAN_POINT('Ctrl Pts',(20.6075542423733,18.2253008854613,-1.97459382895316));
#99788=CARTESIAN_POINT('Ctrl Pts',(20.5858312234504,18.1845230029864,-1.97731826079207));
#99789=CARTESIAN_POINT('Ctrl Pts',(20.5684657742618,18.1538011341689,-1.97937120721142));
#99790=CARTESIAN_POINT('Ctrl Pts',(20.5209125952416,18.0743760146279,-1.98469258930912));
#99791=CARTESIAN_POINT('Ctrl Pts',(20.4895012530008,18.0264381528055,-1.98791797766205));
#99792=CARTESIAN_POINT('Ctrl Pts',(20.3658038554172,17.853407971902,-1.99972432972039));
#99793=CARTESIAN_POINT('Ctrl Pts',(20.2617863034488,17.737329348791,-2.00794636938961));
#99794=CARTESIAN_POINT('Ctrl Pts',(20.1334485206014,17.6224418669102,-2.01751895948848));
#99795=CARTESIAN_POINT('Ctrl Pts',(20.1207564696309,17.6113501705525,-2.01846062217564));
#99796=CARTESIAN_POINT('Ctrl Pts',(20.0673758786275,17.5658131618407,-2.02240670428345));
#99797=CARTESIAN_POINT('Ctrl Pts',(20.025529327739,17.532762250327,-2.02546577719365));
#99798=CARTESIAN_POINT('Ctrl Pts',(19.9754439900595,17.4961875274164,-2.02914613715852));
#99799=CARTESIAN_POINT('Ctrl Pts',(19.9683721763111,17.4910900253156,-2.02966621520578));
#99800=CARTESIAN_POINT('Ctrl Pts',(19.957616671921,17.4834377480025,-2.03045818028469));
#99801=CARTESIAN_POINT('Ctrl Pts',(19.9539559186703,17.4808506856397,-2.03072790456617));
#99802=CARTESIAN_POINT('Ctrl Pts',(19.9473699942445,17.4762276925308,-2.03121351427578));
#99803=CARTESIAN_POINT('Ctrl Pts',(19.9444478764161,17.4741875058379,-2.03142910380594));
#99804=CARTESIAN_POINT('Ctrl Pts',(19.9380869924229,17.4697702651024,-2.03189869131741));
#99805=CARTESIAN_POINT('Ctrl Pts',(19.9346463782718,17.467396045927,-2.03215287070863));
#99806=CARTESIAN_POINT('Ctrl Pts',(19.9249615556566,17.4607552264595,-2.03286879681091));
#99807=CARTESIAN_POINT('Ctrl Pts',(19.9187015568244,17.4565119231947,-2.03333207289827));
#99808=CARTESIAN_POINT('Ctrl Pts',(19.8811282478524,17.4313358486846,-2.03611516891385));
#99809=CARTESIAN_POINT('Ctrl Pts',(19.8492856113889,17.4112096487811,-2.03848385080122));
#99810=CARTESIAN_POINT('Ctrl Pts',(19.742700406754,17.3477570119258,-2.04640234122446));
#99811=CARTESIAN_POINT('Ctrl Pts',(19.6658448826362,17.3081562971225,-2.05209315702692));
#99812=CARTESIAN_POINT('Ctrl Pts',(19.4253935060272,17.2023290232827,-2.06944986560032));
#99813=CARTESIAN_POINT('Ctrl Pts',(19.2557187035422,17.1517240442912,-2.08103081022248));
#99814=CARTESIAN_POINT('Ctrl Pts',(19.0590957549896,17.1189848744022,-2.09329913705833));
#99815=CARTESIAN_POINT('Ctrl Pts',(19.0364221906489,17.1155870528465,-2.09469854304351));
#99816=CARTESIAN_POINT('Ctrl Pts',(19.0042455743057,17.1112982950912,-2.09666353364091));
#99817=CARTESIAN_POINT('Ctrl Pts',(18.9947854407372,17.1101023636118,-2.09723870471809));
#99818=CARTESIAN_POINT('Ctrl Pts',(18.9793947879915,17.1082622662116,-2.09817039109011));
#99819=CARTESIAN_POINT('Ctrl Pts',(18.9734691360716,17.1075791878296,-2.0985281298787));
#99820=CARTESIAN_POINT('Ctrl Pts',(18.9610542218372,17.1062012038786,-2.09927562112541));
#99821=CARTESIAN_POINT('Ctrl Pts',(18.9545644652573,17.1055112420284,-2.09966521405193));
#99822=CARTESIAN_POINT('Ctrl Pts',(18.9391085242532,17.103940281024,-2.10059037847836));
#99823=CARTESIAN_POINT('Ctrl Pts',(18.9301396558038,17.1030864805939,-2.1011250888805));
#99824=CARTESIAN_POINT('Ctrl Pts',(18.8998610642644,17.1003990045108,-2.10292320890595));
#99825=CARTESIAN_POINT('Ctrl Pts',(18.8785286466909,17.0988309787259,-2.10417827801084));
#99826=CARTESIAN_POINT('Ctrl Pts',(18.6920726549447,17.0879638122336,-2.11505404151969));
#99827=CARTESIAN_POINT('Ctrl Pts',(18.526409712385,17.09771951267,-2.12401221140242));
#99828=CARTESIAN_POINT('Ctrl Pts',(18.3016027589193,17.1376739193637,-2.13641574453864));
#99829=CARTESIAN_POINT('Ctrl Pts',(18.2401735316896,17.1514409959104,-2.13983910272743));
#99830=CARTESIAN_POINT('Ctrl Pts',(18.1596221228129,17.1733049278557,-2.14447025566488));
#99831=CARTESIAN_POINT('Ctrl Pts',(18.1398730572307,17.178975322293,-2.14561733047005));
#99832=CARTESIAN_POINT('Ctrl Pts',(18.0701940452841,17.2000843253544,-2.14971557967471));
#99833=CARTESIAN_POINT('Ctrl Pts',(18.0207605181586,17.2170820795169,-2.1527166975314));
#99834=CARTESIAN_POINT('Ctrl Pts',(17.963919663373,17.2390110321689,-2.15633246707259));
#99835=CARTESIAN_POINT('Ctrl Pts',(17.9558477430367,17.2421822650977,-2.15684989471024));
#99836=CARTESIAN_POINT('Ctrl Pts',(17.9436426265262,17.2470640973833,-2.15763860723274));
#99837=CARTESIAN_POINT('Ctrl Pts',(17.9394948791528,17.2487383916779,-2.15790775585106));
#99838=CARTESIAN_POINT('Ctrl Pts',(17.9320524889223,17.2517700781387,-2.15839275424732));
#99839=CARTESIAN_POINT('Ctrl Pts',(17.9287559423977,17.2531226533227,-2.15860831140802));
#99840=CARTESIAN_POINT('Ctrl Pts',(17.9215924346766,17.2560829977624,-2.15907832761102));
#99841=CARTESIAN_POINT('Ctrl Pts',(17.9177268745272,17.257693899625,-2.15933297079279));
#99842=CARTESIAN_POINT('Ctrl Pts',(17.9070029859586,17.2622002772095,-2.16004217280865));
#99843=CARTESIAN_POINT('Ctrl Pts',(17.9001551904168,17.2651204429536,-2.16049818997774));
#99844=CARTESIAN_POINT('Ctrl Pts',(17.8601330465235,17.2824374889262,-2.16318129240295));
#99845=CARTESIAN_POINT('Ctrl Pts',(17.8273186912187,17.2976454969852,-2.16545337888392));
#99846=CARTESIAN_POINT('Ctrl Pts',(17.7224518637009,17.3495499852349,-2.17291349038553));
#99847=CARTESIAN_POINT('Ctrl Pts',(17.6521101730921,17.389533982468,-2.17822661167641));
#99848=CARTESIAN_POINT('Ctrl Pts',(17.4293354433018,17.5336298415982,-2.19574502878615));
#99849=CARTESIAN_POINT('Ctrl Pts',(17.2881636943055,17.653660993577,-2.2078955885692));
#99850=CARTESIAN_POINT('Ctrl Pts',(17.1494254195771,17.8069679861631,-2.22061254355502));
#99851=CARTESIAN_POINT('Ctrl Pts',(17.1347790983335,17.8236734113778,-2.22196799819656));
#99852=CARTESIAN_POINT('Ctrl Pts',(17.1149114023867,17.8470671016292,-2.22382550562645));
#99853=CARTESIAN_POINT('Ctrl Pts',(17.1094636043675,17.853560373087,-2.2243368652928));
#99854=CARTESIAN_POINT('Ctrl Pts',(17.1001735352377,17.8647693069741,-2.22521244387439));
#99855=CARTESIAN_POINT('Ctrl Pts',(17.0963123530989,17.8694690953277,-2.22557743192844));
#99856=CARTESIAN_POINT('Ctrl Pts',(17.0884005770431,17.8791842848849,-2.22632757160391));
#99857=CARTESIAN_POINT('Ctrl Pts',(17.084352526464,17.88420168287,-2.22671261802951));
#99858=CARTESIAN_POINT('Ctrl Pts',(17.0749966718327,17.8959069027328,-2.22760547801569));
#99859=CARTESIAN_POINT('Ctrl Pts',(17.0697062578163,17.9026085294009,-2.22811259110002));
#99860=CARTESIAN_POINT('Ctrl Pts',(17.0529469528597,17.9241044909288,-2.22972639706376));
#99861=CARTESIAN_POINT('Ctrl Pts',(17.0416334768823,17.9390192677116,-2.23082693703694));
#99862=CARTESIAN_POINT('Ctrl Pts',(16.9927534729308,18.0052655857988,-2.2356344357632));
#99863=CARTESIAN_POINT('Ctrl Pts',(16.957311731321,18.0581275742994,-2.23925948062348));
#99864=CARTESIAN_POINT('Ctrl Pts',(16.8873536190559,18.1733794162606,-2.24680663626997));
#99865=CARTESIAN_POINT('Ctrl Pts',(16.8534986323758,18.236077063811,-2.25070731916699));
#99866=CARTESIAN_POINT('Ctrl Pts',(16.7941561418751,18.3606179444794,-2.25821639434393));
#99867=CARTESIAN_POINT('Ctrl Pts',(16.7683116637394,18.4221952095568,-2.26182386230899));
#99868=CARTESIAN_POINT('Ctrl Pts',(16.7454194503191,18.4848895418526,-2.26547384646965));
#99869=CARTESIAN_POINT('Ctrl Pts',(16.7454194497489,18.4848895434144,-2.04625067101847));
#99870=CARTESIAN_POINT('Ctrl Pts',(16.748932204389,18.475269250122,-2.04566730916763));
#99871=CARTESIAN_POINT('Ctrl Pts',(16.7525149174804,18.4656740442466,-2.04508120036617));
#99872=CARTESIAN_POINT('Ctrl Pts',(16.7671937061732,18.4272154823377,-2.04271340093804));
#99873=CARTESIAN_POINT('Ctrl Pts',(16.7788510679927,18.3985730221787,-2.04090763423702));
#99874=CARTESIAN_POINT('Ctrl Pts',(16.7939618142308,18.3636561223643,-2.03864174979379));
#99875=CARTESIAN_POINT('Ctrl Pts',(16.7968258179881,18.3571288185766,-2.03821535470679));
#99876=CARTESIAN_POINT('Ctrl Pts',(16.8013829450996,18.3468836841518,-2.03754146625148));
#99877=CARTESIAN_POINT('Ctrl Pts',(16.8030539896864,18.343156008944,-2.03729530481808));
#99878=CARTESIAN_POINT('Ctrl Pts',(16.8062079246755,18.3361745887211,-2.03683241795746));
#99879=CARTESIAN_POINT('Ctrl Pts',(16.8076882727687,18.3329197560843,-2.03661584871557));
#99880=CARTESIAN_POINT('Ctrl Pts',(16.8111000197742,18.3254685176877,-2.03611831500188));
#99881=CARTESIAN_POINT('Ctrl Pts',(16.813036907477,18.3212746848889,-2.03583701564578));
#99882=CARTESIAN_POINT('Ctrl Pts',(16.8190812869896,18.3082988768954,-2.03496280912999));
#99883=CARTESIAN_POINT('Ctrl Pts',(16.823235323755,18.2995388988545,-2.03436713610167));
#99884=CARTESIAN_POINT('Ctrl Pts',(16.8705008587748,18.2016091896507,-2.02764871579488));
#99885=CARTESIAN_POINT('Ctrl Pts',(16.9197543466835,18.1155517304313,-2.02119661547279));
#99886=CARTESIAN_POINT('Ctrl Pts',(17.0685235620562,17.8933376474788,-2.00358053880378));
#99887=CARTESIAN_POINT('Ctrl Pts',(17.1785843751989,17.7650591625204,-1.99239369273905));
#99888=CARTESIAN_POINT('Ctrl Pts',(17.3255714047026,17.6301831975143,-1.97986683303894));
#99889=CARTESIAN_POINT('Ctrl Pts',(17.3489064487713,17.6096977540831,-1.97793714026745));
#99890=CARTESIAN_POINT('Ctrl Pts',(17.3842834551674,17.5799930623691,-1.97509721056029));
#99891=CARTESIAN_POINT('Ctrl Pts',(17.3959866756151,17.5703785493105,-1.97417113595211));
#99892=CARTESIAN_POINT('Ctrl Pts',(17.4148938305261,17.5551827028855,-1.97269609917014));
#99893=CARTESIAN_POINT('Ctrl Pts',(17.4220322072816,17.5495209833677,-1.97214392183847));
#99894=CARTESIAN_POINT('Ctrl Pts',(17.4357163011011,17.5388107870854,-1.97109429581479));
#99895=CARTESIAN_POINT('Ctrl Pts',(17.4422554552983,17.5337542336096,-1.97059653054046));
#99896=CARTESIAN_POINT('Ctrl Pts',(17.4537845048468,17.5249465454373,-1.96972553507797));
#99897=CARTESIAN_POINT('Ctrl Pts',(17.4587616553858,17.5211789646849,-1.96935165785627));
#99898=CARTESIAN_POINT('Ctrl Pts',(17.4686169661866,17.5137870764052,-1.96861550761198));
#99899=CARTESIAN_POINT('Ctrl Pts',(17.4734942099634,17.5101616523759,-1.96825319301647));
#99900=CARTESIAN_POINT('Ctrl Pts',(17.4851946312962,17.5015422952822,-1.96738872132745));
#99901=CARTESIAN_POINT('Ctrl Pts',(17.492032283288,17.4965681154039,-1.96688733417987));
#99902=CARTESIAN_POINT('Ctrl Pts',(17.5168356703837,17.478750681511,-1.96508206434312));
#99903=CARTESIAN_POINT('Ctrl Pts',(17.5349726937722,17.4661474905479,-1.9637873946628));
#99904=CARTESIAN_POINT('Ctrl Pts',(17.7074868914954,17.3502299601347,-1.95169903557469));
#99905=CARTESIAN_POINT('Ctrl Pts',(17.8746285822612,17.2673742462143,-1.94176382026612));
#99906=CARTESIAN_POINT('Ctrl Pts',(18.1261998595004,17.1815483970631,-1.92727297071972));
#99907=CARTESIAN_POINT('Ctrl Pts',(18.2033482274414,17.1600242529721,-1.9228711878646));
#99908=CARTESIAN_POINT('Ctrl Pts',(18.3166925849788,17.1352255324177,-1.91623421921975));
#99909=CARTESIAN_POINT('Ctrl Pts',(18.3520505310455,17.1284296232213,-1.91414009170023));
#99910=CARTESIAN_POINT('Ctrl Pts',(18.3949259879772,17.1213173605547,-1.91155365263428));
#99911=CARTESIAN_POINT('Ctrl Pts',(18.4022961761574,17.1201347990098,-1.91110737977979));
#99912=CARTESIAN_POINT('Ctrl Pts',(18.4137821978192,17.1183541016037,-1.91040907501757));
#99913=CARTESIAN_POINT('Ctrl Pts',(18.417893884448,17.1177290619857,-1.9101585401916));
#99914=CARTESIAN_POINT('Ctrl Pts',(18.4255343849237,17.1165906129626,-1.90969190132036));
#99915=CARTESIAN_POINT('Ctrl Pts',(18.4290626637494,17.1160740021307,-1.90947598071486));
#99916=CARTESIAN_POINT('Ctrl Pts',(18.4370573984633,17.1149240372454,-1.9089857507221));
#99917=CARTESIAN_POINT('Ctrl Pts',(18.4415245611604,17.1142960468752,-1.90871114361393));
#99918=CARTESIAN_POINT('Ctrl Pts',(18.4530650521396,17.1127112918473,-1.90800001530098));
#99919=CARTESIAN_POINT('Ctrl Pts',(18.4601412069207,17.1117760229477,-1.90756232648785));
#99920=CARTESIAN_POINT('Ctrl Pts',(18.503651265195,17.1062489510007,-1.90486145973869));
#99921=CARTESIAN_POINT('Ctrl Pts',(18.540192475817,17.1025703031983,-1.90255195330837));
#99922=CARTESIAN_POINT('Ctrl Pts',(18.7466635844147,17.0871969396967,-1.88933835460756));
#99923=CARTESIAN_POINT('Ctrl Pts',(18.9174228130529,17.0950938248628,-1.87784603500694));
#99924=CARTESIAN_POINT('Ctrl Pts',(19.1795617803202,17.1392175761917,-1.8605700067175));
#99925=CARTESIAN_POINT('Ctrl Pts',(19.2725582170084,17.1614227207803,-1.85450263010928));
#99926=CARTESIAN_POINT('Ctrl Pts',(19.3841840461219,17.1962027757636,-1.84732074178399));
#99927=CARTESIAN_POINT('Ctrl Pts',(19.4045223051533,17.2028797247869,-1.84601605000661));
#99928=CARTESIAN_POINT('Ctrl Pts',(19.4332751879296,17.2128047072667,-1.84417646600841));
#99929=CARTESIAN_POINT('Ctrl Pts',(19.4417752063122,17.2157996397327,-1.84363325417258));
#99930=CARTESIAN_POINT('Ctrl Pts',(19.4563978256583,17.2210570408857,-1.84269974620621));
#99931=CARTESIAN_POINT('Ctrl Pts',(19.4625295138347,17.2232936967456,-1.84230859842226));
#99932=CARTESIAN_POINT('Ctrl Pts',(19.474244484527,17.2276284573484,-1.84156182335729));
#99933=CARTESIAN_POINT('Ctrl Pts',(19.4798294267272,17.2297218669703,-1.84120604388603));
#99934=CARTESIAN_POINT('Ctrl Pts',(19.4943170475591,17.2352222164258,-1.84028370318293));
#99935=CARTESIAN_POINT('Ctrl Pts',(19.5032057587659,17.2386657565024,-1.83971837262315));
#99936=CARTESIAN_POINT('Ctrl Pts',(19.5333738497084,17.2505880191995,-1.83780131862885));
#99937=CARTESIAN_POINT('Ctrl Pts',(19.5545392176772,17.2593521991455,-1.8364592038496));
#99938=CARTESIAN_POINT('Ctrl Pts',(19.7376080157621,17.3386622950578,-1.82486499101896));
#99939=CARTESIAN_POINT('Ctrl Pts',(19.8902343827304,17.4288646997646,-1.81537503189025));
#99940=CARTESIAN_POINT('Ctrl Pts',(20.0980772799964,17.5897608909292,-1.8010709118068));
#99941=CARTESIAN_POINT('Ctrl Pts',(20.1629633828687,17.6466520925966,-1.79634831694525));
#99942=CARTESIAN_POINT('Ctrl Pts',(20.2509187011146,17.733819496642,-1.78927676085419));
#99943=CARTESIAN_POINT('Ctrl Pts',(20.2769298804605,17.7610098014468,-1.78709094393442));
#99944=CARTESIAN_POINT('Ctrl Pts',(20.3072797335607,17.7944771309119,-1.78440282599807));
#99945=CARTESIAN_POINT('Ctrl Pts',(20.31232836727,17.8001046389454,-1.78395089556875));
#99946=CARTESIAN_POINT('Ctrl Pts',(20.3201211746591,17.8088851366176,-1.7832456490346));
#99947=CARTESIAN_POINT('Ctrl Pts',(20.3228863945706,17.812019480023,-1.7829938785437));
#99948=CARTESIAN_POINT('Ctrl Pts',(20.3279921801586,17.8178414909012,-1.78252613341434));
#99949=CARTESIAN_POINT('Ctrl Pts',(20.3303352480225,17.8205268872724,-1.78231034977703));
#99950=CARTESIAN_POINT('Ctrl Pts',(20.3356104915107,17.8266037658478,-1.78182196699511));
#99951=CARTESIAN_POINT('Ctrl Pts',(20.338538664505,17.829998633996,-1.78154907971064));
#99952=CARTESIAN_POINT('Ctrl Pts',(20.3471307456788,17.8400243453229,-1.78074310876765));
#99953=CARTESIAN_POINT('Ctrl Pts',(20.3527644107552,17.8466808200299,-1.78020788809811));
#99954=CARTESIAN_POINT('Ctrl Pts',(20.3925763987801,17.8943145297086,-1.77637830335595));
#99955=CARTESIAN_POINT('Ctrl Pts',(20.4252329226406,17.9365328710557,-1.77298682021617));
#99956=CARTESIAN_POINT('Ctrl Pts',(20.4665200388632,17.9942934607574,-1.76839814780399));
#99957=CARTESIAN_POINT('Ctrl Pts',(20.4766030344262,18.0087790853131,-1.76725143660039));
#99958=CARTESIAN_POINT('Ctrl Pts',(20.5136858735944,18.063500534582,-1.76293908919992));
#99959=CARTESIAN_POINT('Ctrl Pts',(20.5394824044578,18.1045327018757,-1.75974481577322));
#99960=CARTESIAN_POINT('Ctrl Pts',(20.6188535677183,18.2409584592925,-1.7493186861675));
#99961=CARTESIAN_POINT('Ctrl Pts',(20.6664533521603,18.339632643482,-1.74208588986972));
#99962=CARTESIAN_POINT('Ctrl Pts',(20.7262430089122,18.492882337104,-1.73151223758427));
#99963=CARTESIAN_POINT('Ctrl Pts',(20.7442598257454,18.5449809023694,-1.72802300248184));
#99964=CARTESIAN_POINT('Ctrl Pts',(20.7701617750288,18.6305596757276,-1.7224653029267));
#99965=CARTESIAN_POINT('Ctrl Pts',(20.7793001331969,18.6636305401208,-1.72035839656378));
#99966=CARTESIAN_POINT('Ctrl Pts',(20.790255861212,18.707395339042,-1.71762183079164));
#99967=CARTESIAN_POINT('Ctrl Pts',(20.7928002593873,18.7179002940177,-1.71696882869671));
#99968=CARTESIAN_POINT('Ctrl Pts',(20.7968365313947,18.7351407496521,-1.71590333646862));
#99969=CARTESIAN_POINT('Ctrl Pts',(20.7983761102126,18.7418647756417,-1.71548931686118));
#99970=CARTESIAN_POINT('Ctrl Pts',(20.8012930921926,18.7548969865183,-1.71468981394894));
#99971=CARTESIAN_POINT('Ctrl Pts',(20.8026745529531,18.7612041759596,-1.71430420428969));
#99972=CARTESIAN_POINT('Ctrl Pts',(20.8057982328307,18.775784467652,-1.71341580430024));
#99973=CARTESIAN_POINT('Ctrl Pts',(20.8075197986331,18.784061919013,-1.71291367999694));
#99974=CARTESIAN_POINT('Ctrl Pts',(20.8120175446899,18.8063566176257,-1.71156711398095));
#99975=CARTESIAN_POINT('Ctrl Pts',(20.814701499101,18.820392179435,-1.71072561347498));
#99976=CARTESIAN_POINT('Ctrl Pts',(20.8380194479748,18.949398917796,-1.70304550623693));
#99977=CARTESIAN_POINT('Ctrl Pts',(20.8492485377539,19.0658729944758,-1.69652341872511));
#99978=CARTESIAN_POINT('Ctrl Pts',(20.8529860109224,19.3453574992842,-1.68122168989833));
#99979=CARTESIAN_POINT('Ctrl Pts',(20.8364044404087,19.5077109611391,-1.67262493106746));
#99980=CARTESIAN_POINT('Ctrl Pts',(20.7943952495572,19.6983622548763,-1.66141634795089));
#99981=CARTESIAN_POINT('Ctrl Pts',(20.7866510683782,19.7300124087444,-1.65951615396292));
#99982=CARTESIAN_POINT('Ctrl Pts',(20.7762964353091,19.7684645758903,-1.65714514399646));
#99983=CARTESIAN_POINT('Ctrl Pts',(20.7743768275969,19.7754500695405,-1.65671186732123));
#99984=CARTESIAN_POINT('Ctrl Pts',(20.7713118568887,19.786383607601,-1.65602952419425));
#99985=CARTESIAN_POINT('Ctrl Pts',(20.7701907632999,19.7903384787037,-1.65578184594555));
#99986=CARTESIAN_POINT('Ctrl Pts',(20.7680740637434,19.7977234957114,-1.65531769627363));
#99987=CARTESIAN_POINT('Ctrl Pts',(20.7670812934255,19.8011543958,-1.65510139062656));
#99988=CARTESIAN_POINT('Ctrl Pts',(20.764795734403,19.8089788118065,-1.65460656181675));
#99989=CARTESIAN_POINT('Ctrl Pts',(20.7634973726848,19.8133706397177,-1.65432771735529));
#99990=CARTESIAN_POINT('Ctrl Pts',(20.7594643792966,19.8268515555118,-1.65346848953093));
#99991=CARTESIAN_POINT('Ctrl Pts',(20.7566829071503,19.8359263473696,-1.65288547246445));
#99992=CARTESIAN_POINT('Ctrl Pts',(20.73123563527,19.9170003172269,-1.64763729051895));
#99993=CARTESIAN_POINT('Ctrl Pts',(20.7047974379205,19.9877506534473,-1.64277918045029));
#99994=CARTESIAN_POINT('Ctrl Pts',(20.6205212509165,20.1810880772827,-1.62898763264374));
#99995=CARTESIAN_POINT('Ctrl Pts',(20.5546053160047,20.2997760414597,-1.61993439762496));
#99996=CARTESIAN_POINT('Ctrl Pts',(20.4268030116346,20.4854398131255,-1.60532705951748));
#99997=CARTESIAN_POINT('Ctrl Pts',(20.3711298320927,20.5562094215129,-1.59962720805163));
#99998=CARTESIAN_POINT('Ctrl Pts',(20.2972855535347,20.6386754208425,-1.59283220891481));
#99999=CARTESIAN_POINT('Ctrl Pts',(20.2832287132102,20.6539169315409,-1.5915690577714));
#100000=CARTESIAN_POINT('Ctrl Pts',(20.2628224254177,20.6754009534606,-1.58977744489934));
#100001=CARTESIAN_POINT('Ctrl Pts',(20.2566543319473,20.6818133634611,-1.58924124211741));
#100002=CARTESIAN_POINT('Ctrl Pts',(20.2459060944276,20.6928472565524,-1.58831598730404));
#100003=CARTESIAN_POINT('Ctrl Pts',(20.2413447683426,20.6974868250126,-1.58792612317244));
#100004=CARTESIAN_POINT('Ctrl Pts',(20.2325437552783,20.7063566402202,-1.58717919149632));
#100005=CARTESIAN_POINT('Ctrl Pts',(20.2283073700397,20.7105900616215,-1.5868219842864));
#100006=CARTESIAN_POINT('Ctrl Pts',(20.2171856920302,20.7216100308647,-1.58589023947696));
#100007=CARTESIAN_POINT('Ctrl Pts',(20.2102717259589,20.7283675422379,-1.58531698364121));
#100008=CARTESIAN_POINT('Ctrl Pts',(20.1862330012043,20.7515424639579,-1.58334411275167));
#100009=CARTESIAN_POINT('Ctrl Pts',(20.1688783514593,20.7677196139166,-1.58195489215878));
#100010=CARTESIAN_POINT('Ctrl Pts',(20.0307366418845,20.8922151955322,-1.57115672235753));
#100011=CARTESIAN_POINT('Ctrl Pts',(19.8981324675179,20.9866162411614,-1.56237404407504));
#100012=CARTESIAN_POINT('Ctrl Pts',(19.6418803015186,21.1278811990845,-1.54647761837973));
#100013=CARTESIAN_POINT('Ctrl Pts',(19.522174520254,21.1801244835777,-1.53938848268958));
#100014=CARTESIAN_POINT('Ctrl Pts',(19.3871558879411,21.2247571373537,-1.53099654831876));
#100015=CARTESIAN_POINT('Ctrl Pts',(19.3758337498979,21.2283943206682,-1.53028982671437));
#100016=CARTESIAN_POINT('Ctrl Pts',(19.3596897455559,21.2334308496959,-1.52927706824115));
#100017=CARTESIAN_POINT('Ctrl Pts',(19.354892380384,21.2349088048366,-1.52897548389518));
#100018=CARTESIAN_POINT('Ctrl Pts',(19.3466139729639,21.2374269835953,-1.52845390420199));
#100019=CARTESIAN_POINT('Ctrl Pts',(19.3431353897502,21.2384753454774,-1.52823438350641));
#100020=CARTESIAN_POINT('Ctrl Pts',(19.3363837941764,21.240491170953,-1.52780760386014));
#100021=CARTESIAN_POINT('Ctrl Pts',(19.3331111342183,21.2414596762644,-1.52760041314822));
#100022=CARTESIAN_POINT('Ctrl Pts',(19.3242717952368,21.2440523440794,-1.52703996155802));
#100023=CARTESIAN_POINT('Ctrl Pts',(19.3187008095448,21.2456615412687,-1.52668584307665));
#100024=CARTESIAN_POINT('Ctrl Pts',(19.2979796640321,21.2515547824242,-1.5253655730213));
#100025=CARTESIAN_POINT('Ctrl Pts',(19.2827889003846,21.2556925418607,-1.52439146539274));
#100026=CARTESIAN_POINT('Ctrl Pts',(19.1401759622143,21.2928347129148,-1.51519755641148));
#100027=CARTESIAN_POINT('Ctrl Pts',(19.00999319318,21.3140540483049,-1.50645963863266));
#100028=CARTESIAN_POINT('Ctrl Pts',(18.7197366709189,21.333939608509,-1.48724143405048));
#100029=CARTESIAN_POINT('Ctrl Pts',(18.5600264604325,21.3268514654846,-1.47686840382037));
#100030=CARTESIAN_POINT('Ctrl Pts',(18.3815830274096,21.2985689560941,-1.46577185151761));
#100031=CARTESIAN_POINT('Ctrl Pts',(18.3606155230474,21.2949208126232,-1.46447480700474));
#100032=CARTESIAN_POINT('Ctrl Pts',(18.330871935262,21.2892823696761,-1.46264402259855));
#100033=CARTESIAN_POINT('Ctrl Pts',(18.3220485519764,21.2875514327981,-1.46210207166813));
#100034=CARTESIAN_POINT('Ctrl Pts',(18.3068431988327,21.2844677766219,-1.46117003497377));
#100035=CARTESIAN_POINT('Ctrl Pts',(18.3004560133068,21.2831416859263,-1.46077910482167));
#100036=CARTESIAN_POINT('Ctrl Pts',(18.2882362799637,21.2805456832788,-1.46003227186534));
#100037=CARTESIAN_POINT('Ctrl Pts',(18.2824027834691,21.2792805864833,-1.45967621914014));
#100038=CARTESIAN_POINT('Ctrl Pts',(18.2672434705536,21.2759258286182,-1.45875214605874));
#100039=CARTESIAN_POINT('Ctrl Pts',(18.2579262484274,21.2737976447271,-1.45818536554872));
#100040=CARTESIAN_POINT('Ctrl Pts',(18.2261829610988,21.2663205053888,-1.45625813426443));
#100041=CARTESIAN_POINT('Ctrl Pts',(18.2038295148217,21.260668227527,-1.4549074326959));
#100042=CARTESIAN_POINT('Ctrl Pts',(18.013001897462,21.2090848392155,-1.4434214562749));
#100043=CARTESIAN_POINT('Ctrl Pts',(17.8507182639555,21.1428388653696,-1.43402845751925));
#100044=CARTESIAN_POINT('Ctrl Pts',(17.6219897839229,21.0145513908651,-1.41976116469091));
#100045=CARTESIAN_POINT('Ctrl Pts',(17.5483186694448,20.9669959259469,-1.41496681028824));
#100046=CARTESIAN_POINT('Ctrl Pts',(17.4472435950924,20.8924842096476,-1.40779849604375));
#100047=CARTESIAN_POINT('Ctrl Pts',(17.4172897299615,20.8691329421779,-1.40559281767691));
#100048=CARTESIAN_POINT('Ctrl Pts',(17.3821311849691,20.8401707006092,-1.40288268092858));
#100049=CARTESIAN_POINT('Ctrl Pts',(17.3763062231969,20.8353195711646,-1.40242955688775));
#100050=CARTESIAN_POINT('Ctrl Pts',(17.36730672404,20.827742402918,-1.4017228434973));
#100051=CARTESIAN_POINT('Ctrl Pts',(17.3641139352504,20.8250380035354,-1.40147081003788));
#100052=CARTESIAN_POINT('Ctrl Pts',(17.3582169959043,20.8200129966435,-1.40100283890841));
#100053=CARTESIAN_POINT('Ctrl Pts',(17.3555106790074,20.81769502055,-1.40078709390854));
#100054=CARTESIAN_POINT('Ctrl Pts',(17.3494172701478,20.8124492525169,-1.40029912943574));
#100055=CARTESIAN_POINT('Ctrl Pts',(17.3460336263186,20.8095175597626,-1.40002662392805));
#100056=CARTESIAN_POINT('Ctrl Pts',(17.336107282698,20.8008617937674,-1.39922271670995));
#100057=CARTESIAN_POINT('Ctrl Pts',(17.3295906043254,20.795108208351,-1.39868919349516));
#100058=CARTESIAN_POINT('Ctrl Pts',(17.2837281587452,20.7541107583246,-1.39489464216436));
#100059=CARTESIAN_POINT('Ctrl Pts',(17.2456814511811,20.7174481782097,-1.39153841103967));
#100060=CARTESIAN_POINT('Ctrl Pts',(17.195507708285,20.6653423239044,-1.38686501604838));
#100061=CARTESIAN_POINT('Ctrl Pts',(17.1821618851296,20.6510932466922,-1.38559625206619));
#100062=CARTESIAN_POINT('Ctrl Pts',(17.0704045124053,20.5284143929947,-1.37476374100887));
#100063=CARTESIAN_POINT('Ctrl Pts',(16.9832811391905,20.4102161226442,-1.36495842821981));
#100064=CARTESIAN_POINT('Ctrl Pts',(16.8777709031625,20.2307611200807,-1.35150931276999));
#100065=CARTESIAN_POINT('Ctrl Pts',(16.8488256597699,20.1762036238822,-1.34758320436482));
#100066=CARTESIAN_POINT('Ctrl Pts',(16.8063135111892,20.0868420597404,-1.34141720810371));
#100067=CARTESIAN_POINT('Ctrl Pts',(16.7912114292737,20.0528119494022,-1.33912754783615));
#100068=CARTESIAN_POINT('Ctrl Pts',(16.7727688570564,20.0081105854558,-1.33619297680954));
#100069=CARTESIAN_POINT('Ctrl Pts',(16.7686050697038,19.9977881906051,-1.33552028771204));
#100070=CARTESIAN_POINT('Ctrl Pts',(16.7619671077403,19.9809505370373,-1.33443092601528));
#100071=CARTESIAN_POINT('Ctrl Pts',(16.759443395003,19.9744551546148,-1.33401258917509));
#100072=CARTESIAN_POINT('Ctrl Pts',(16.7546526297504,19.961942297938,-1.33321030082237));
#100073=CARTESIAN_POINT('Ctrl Pts',(16.752380836047,19.9559267329135,-1.33282619370624));
#100074=CARTESIAN_POINT('Ctrl Pts',(16.747243154446,19.9421326507232,-1.33194900818436));
#100075=CARTESIAN_POINT('Ctrl Pts',(16.7443954637851,19.9343474329577,-1.33145654214473));
#100076=CARTESIAN_POINT('Ctrl Pts',(16.7369541495323,19.9136274082932,-1.33015265068161));
#100077=CARTESIAN_POINT('Ctrl Pts',(16.7324404233318,19.9006641777291,-1.32934387929097));
#100078=CARTESIAN_POINT('Ctrl Pts',(16.6991412224389,19.8019489358526,-1.32323611985894));
#100079=CARTESIAN_POINT('Ctrl Pts',(16.6757502469573,19.7144696845719,-1.31812043168403));
#100080=CARTESIAN_POINT('Ctrl Pts',(16.6306361030139,19.4886587757842,-1.30537418782824));
#100081=CARTESIAN_POINT('Ctrl Pts',(16.6168948152935,19.3491947907301,-1.29793912363815));
#100082=CARTESIAN_POINT('Ctrl Pts',(16.6170159594101,19.1891094974785,-1.28909419861748));
#100083=CARTESIAN_POINT('Ctrl Pts',(16.6173229666296,19.1688226796989,-1.28796711911386));
#100084=CARTESIAN_POINT('Ctrl Pts',(16.6196735815231,19.0891814573856,-1.28350785079882));
#100085=CARTESIAN_POINT('Ctrl Pts',(16.6239226730702,19.0299246715509,-1.28011460872607));
#100086=CARTESIAN_POINT('Ctrl Pts',(16.6316702819436,18.9620446814946,-1.27606206003484));
#100087=CARTESIAN_POINT('Ctrl Pts',(16.6327408137148,18.9531651309176,-1.27552865258903));
#100088=CARTESIAN_POINT('Ctrl Pts',(16.6344383637347,18.9397981127848,-1.27472036792846));
#100089=CARTESIAN_POINT('Ctrl Pts',(16.6350235911771,18.9353053093828,-1.27444778944549));
#100090=CARTESIAN_POINT('Ctrl Pts',(16.636095341648,18.9272787126149,-1.27395914218773));
#100091=CARTESIAN_POINT('Ctrl Pts',(16.6365763775095,18.9237442393861,-1.27374338568322));
#100092=CARTESIAN_POINT('Ctrl Pts',(16.6376355523321,18.9161063336661,-1.27327586689139));
#100093=CARTESIAN_POINT('Ctrl Pts',(16.638216799053,18.9120034350728,-1.27302393636176));
#100094=CARTESIAN_POINT('Ctrl Pts',(16.6398690473806,18.9005821205774,-1.27232048023154));
#100095=CARTESIAN_POINT('Ctrl Pts',(16.6409663501364,18.8932676544505,-1.27186750771633));
#100096=CARTESIAN_POINT('Ctrl Pts',(16.6474610385354,18.8514691275068,-1.26926548143208));
#100097=CARTESIAN_POINT('Ctrl Pts',(16.6536719490448,18.8171191060285,-1.26707452535843));
#100098=CARTESIAN_POINT('Ctrl Pts',(16.6761041769704,18.708470376669,-1.26000955659443));
#100099=CARTESIAN_POINT('Ctrl Pts',(16.6954799621017,18.6348874107122,-1.25502391933505));
#100100=CARTESIAN_POINT('Ctrl Pts',(16.727155209449,18.5364540006172,-1.24820176212286));
#100101=CARTESIAN_POINT('Ctrl Pts',(16.736040526688,18.5105753721975,-1.24639313657688));
#100102=CARTESIAN_POINT('Ctrl Pts',(16.7454193884829,18.4848897112021,-1.2445862186816));
#100103=CARTESIAN_POINT('Origin',(18.734,19.211,0.));
#100104=CARTESIAN_POINT('',(16.7454194503191,18.4848895418526,-0.444429617362593));
#100105=CARTESIAN_POINT('',(16.7454194503191,18.4848895418526,-0.666446447912836));
#100106=CARTESIAN_POINT('',(16.7454194503191,18.4848895418526,0.));
#100107=CARTESIAN_POINT('',(20.3539256943887,20.5739122292573,0.));
#100108=CARTESIAN_POINT('Ctrl Pts',(16.7454194503191,18.4848895418526,-0.444429617362593));
#100109=CARTESIAN_POINT('Ctrl Pts',(16.770110946048,18.4172675601033,-0.440115253498862));
#100110=CARTESIAN_POINT('Ctrl Pts',(16.7982601300934,18.3508945674066,-0.435800889635131));
#100111=CARTESIAN_POINT('Ctrl Pts',(16.8297062688822,18.2861462896083,-0.4314865257714));
#100112=CARTESIAN_POINT('Ctrl Pts',(16.8611790966169,18.2213430586946,-0.427168500223636));
#100113=CARTESIAN_POINT('Ctrl Pts',(16.8959542522259,18.1581677454748,-0.422850474675871));
#100114=CARTESIAN_POINT('Ctrl Pts',(16.9338242035691,18.0969730245885,-0.418532449128106));
#100115=CARTESIAN_POINT('Ctrl Pts',(16.9717096236813,18.0357533074462,-0.414212659793034));
#100116=CARTESIAN_POINT('Ctrl Pts',(17.0126920735942,17.97651620248,-0.409892870457962));
#100117=CARTESIAN_POINT('Ctrl Pts',(17.0565212763453,17.9195844465527,-0.405573081122889));
#100118=CARTESIAN_POINT('Ctrl Pts',(17.100427251889,17.8625529669338,-0.401245725090954));
#100119=CARTESIAN_POINT('Ctrl Pts',(17.1471896162535,17.8078352797611,-0.396918369059018));
#100120=CARTESIAN_POINT('Ctrl Pts',(17.1965189481903,17.755719609379,-0.392591013027083));
#100121=CARTESIAN_POINT('Ctrl Pts',(17.2385584481092,17.71130553291,-0.38890314869949));
#100122=CARTESIAN_POINT('Ctrl Pts',(17.2824615181269,17.6687807432721,-0.385215284371896));
#100123=CARTESIAN_POINT('Ctrl Pts',(17.3280304443276,17.6283002152896,-0.381527420044303));
#100124=CARTESIAN_POINT('Ctrl Pts',(17.3823195172276,17.5800732650869,-0.37713383976892));
#100125=CARTESIAN_POINT('Ctrl Pts',(17.4391958858,17.5345513015008,-0.372740259493537));
#100126=CARTESIAN_POINT('Ctrl Pts',(17.4983592346194,17.4920232988986,-0.368346679218154));
#100127=CARTESIAN_POINT('Ctrl Pts',(17.5574362854365,17.4495573293242,-0.363959507592861));
#100128=CARTESIAN_POINT('Ctrl Pts',(17.6187933062776,17.4100769290324,-0.359572335967568));
#100129=CARTESIAN_POINT('Ctrl Pts',(17.6820956267706,17.3738320192261,-0.355185164342275));
#100130=CARTESIAN_POINT('Ctrl Pts',(17.7453254808102,17.3376286014228,-0.350803015009466));
#100131=CARTESIAN_POINT('Ctrl Pts',(17.810495795117,17.304653553715,-0.346420865676658));
#100132=CARTESIAN_POINT('Ctrl Pts',(17.8772429189521,17.2751135611627,-0.342038716343849));
#100133=CARTESIAN_POINT('Ctrl Pts',(17.9439489018955,17.245591776161,-0.337659268034262));
#100134=CARTESIAN_POINT('Ctrl Pts',(18.0122293270667,17.2195010391258,-0.333279819724674));
#100135=CARTESIAN_POINT('Ctrl Pts',(18.0816971982504,17.1970014759614,-0.328900371415087));
#100136=CARTESIAN_POINT('Ctrl Pts',(18.151144994395,17.1745084147899,-0.324522188691946));
#100137=CARTESIAN_POINT('Ctrl Pts',(18.2217790979678,17.155604615017,-0.320144005968804));
#100138=CARTESIAN_POINT('Ctrl Pts',(18.2931954157569,17.1404009759226,-0.315765823245663));
#100139=CARTESIAN_POINT('Ctrl Pts',(18.3646144753839,17.1251967531253,-0.311387472433939));
#100140=CARTESIAN_POINT('Ctrl Pts',(18.4368153380914,17.113693071257,-0.307009121622215));
#100141=CARTESIAN_POINT('Ctrl Pts',(18.5093833633923,17.1059497947652,-0.302630770810491));
#100142=CARTESIAN_POINT('Ctrl Pts',(18.5820273386455,17.0981984141328,-0.298247837601301));
#100143=CARTESIAN_POINT('Ctrl Pts',(18.6550387645182,17.09421534768,-0.293864904392111));
#100144=CARTESIAN_POINT('Ctrl Pts',(18.7279983301931,17.0940085073483,-0.289481971182921));
#100145=CARTESIAN_POINT('Ctrl Pts',(18.8009982495663,17.093801552614,-0.285096613787639));
#100146=CARTESIAN_POINT('Ctrl Pts',(18.8739457709894,17.0973749591399,-0.280711256392357));
#100147=CARTESIAN_POINT('Ctrl Pts',(18.9464247464519,17.1046845613501,-0.276325898997075));
#100148=CARTESIAN_POINT('Ctrl Pts',(19.0190318084556,17.1120070812603,-0.271932791695599));
#100149=CARTESIAN_POINT('Ctrl Pts',(19.0911681952094,17.1230789093043,-0.267539684394123));
#100150=CARTESIAN_POINT('Ctrl Pts',(19.1624265854903,17.1378044807966,-0.263146577092647));
#100151=CARTESIAN_POINT('Ctrl Pts',(19.209979484077,17.1476313040667,-0.260214922516055));
#100152=CARTESIAN_POINT('Ctrl Pts',(19.2571416240954,17.1590841897826,-0.257283267939462));
#100153=CARTESIAN_POINT('Ctrl Pts',(19.3037962299318,17.1721225499419,-0.254351613362869));
#100154=CARTESIAN_POINT('Ctrl Pts',(19.3728933426701,17.1914328200792,-0.250009729787665));
#100155=CARTESIAN_POINT('Ctrl Pts',(19.441158849408,17.2143020129624,-0.245667846212462));
#100156=CARTESIAN_POINT('Ctrl Pts',(19.5081940657064,17.2406415177372,-0.241325962637258));
#100157=CARTESIAN_POINT('Ctrl Pts',(19.575128336692,17.2669413590381,-0.236990617308954));
#100158=CARTESIAN_POINT('Ctrl Pts',(19.6408355376982,17.2967009666761,-0.232655271980649));
#100159=CARTESIAN_POINT('Ctrl Pts',(19.7049304637962,17.3297815027296,-0.228319926652345));
#100160=CARTESIAN_POINT('Ctrl Pts',(19.7689517228447,17.3628240179031,-0.223989564122503));
#100161=CARTESIAN_POINT('Ctrl Pts',(19.8313639491299,17.3991796603212,-0.219659201592662));
#100162=CARTESIAN_POINT('Ctrl Pts',(19.8918020078126,17.4386615699294,-0.21532883906282));
#100163=CARTESIAN_POINT('Ctrl Pts',(19.9522029223966,17.4781192146956,-0.211001137892668));
#100164=CARTESIAN_POINT('Ctrl Pts',(20.0106316627094,17.5206990484192,-0.206673436722516));
#100165=CARTESIAN_POINT('Ctrl Pts',(20.0667492121328,17.5661691462161,-0.202345735552364));
#100166=CARTESIAN_POINT('Ctrl Pts',(20.1228517146943,17.6116270520643,-0.198019194773624));
#100167=CARTESIAN_POINT('Ctrl Pts',(20.1766438725233,17.6599733741804,-0.193692653994883));
#100168=CARTESIAN_POINT('Ctrl Pts',(20.2278185824314,17.710934987148,-0.189366113216143));
#100169=CARTESIAN_POINT('Ctrl Pts',(20.2789973003963,17.7619005914824,-0.185039233578198));
#100170=CARTESIAN_POINT('Ctrl Pts',(20.3275578154845,17.8154815434691,-0.180712353940253));
#100171=CARTESIAN_POINT('Ctrl Pts',(20.3732301490776,17.8713681407361,-0.176385474302308));
#100172=CARTESIAN_POINT('Ctrl Pts',(20.4189572946786,17.9273218082918,-0.172053401915454));
#100173=CARTESIAN_POINT('Ctrl Pts',(20.4617890269818,17.9855862615223,-0.167721329528601));
#100174=CARTESIAN_POINT('Ctrl Pts',(20.5014965046459,18.0458197109183,-0.163389257141747));
#100175=CARTESIAN_POINT('Ctrl Pts',(20.5412284893311,18.1060903357408,-0.159054511047183));
#100176=CARTESIAN_POINT('Ctrl Pts',(20.5778321351825,18.1683319477764,-0.154719764952619));
#100177=CARTESIAN_POINT('Ctrl Pts',(20.6111242325247,18.2321774340216,-0.150385018858055));
#100178=CARTESIAN_POINT('Ctrl Pts',(20.6444833803135,18.2961515053878,-0.146041542563685));
#100179=CARTESIAN_POINT('Ctrl Pts',(20.6745174591996,18.3617354510943,-0.141698066269316));
#100180=CARTESIAN_POINT('Ctrl Pts',(20.7010913635959,18.4285419709235,-0.137354589974947));
#100181=CARTESIAN_POINT('Ctrl Pts',(20.7218496990689,18.480728210842,-0.133961662210443));
#100182=CARTESIAN_POINT('Ctrl Pts',(20.7404975995388,18.5336600360754,-0.130568734445939));
#100183=CARTESIAN_POINT('Ctrl Pts',(20.7569922795081,18.5871480648016,-0.127175806681435));
#100184=CARTESIAN_POINT('Ctrl Pts',(20.7789195363731,18.6582525510522,-0.12266540704014));
#100185=CARTESIAN_POINT('Ctrl Pts',(20.7971288498248,18.7306277670711,-0.118155007398845));
#100186=CARTESIAN_POINT('Ctrl Pts',(20.8114809457081,18.8038613010046,-0.113644607757551));
#100187=CARTESIAN_POINT('Ctrl Pts',(20.8265483310552,18.8807446973446,-0.108909415767653));
#100188=CARTESIAN_POINT('Ctrl Pts',(20.8373637791173,18.9585737514705,-0.104174223777755));
#100189=CARTESIAN_POINT('Ctrl Pts',(20.8438249692462,19.0368517897157,-0.0994390317878569));
#100190=CARTESIAN_POINT('Ctrl Pts',(20.8499589678183,19.1111658657987,-0.0949436276401115));
#100191=CARTESIAN_POINT('Ctrl Pts',(20.8521688918293,19.1858840436361,-0.0904482234923663));
#100192=CARTESIAN_POINT('Ctrl Pts',(20.8504195410052,19.2605714277716,-0.0859528193446209));
#100193=CARTESIAN_POINT('Ctrl Pts',(20.8486718350827,19.3351885839162,-0.0814616421919066));
#100194=CARTESIAN_POINT('Ctrl Pts',(20.8429722647592,19.4097745558195,-0.0769704650391922));
#100195=CARTESIAN_POINT('Ctrl Pts',(20.8333376405566,19.4838927828696,-0.0724792878864778));
#100196=CARTESIAN_POINT('Ctrl Pts',(20.8237095586262,19.5579606808563,-0.0679911604119481));
#100197=CARTESIAN_POINT('Ctrl Pts',(20.8101517936905,19.6315610202815,-0.0635030329374184));
#100198=CARTESIAN_POINT('Ctrl Pts',(20.7927330149949,19.7042619719479,-0.0590149054628886));
#100199=CARTESIAN_POINT('Ctrl Pts',(20.7753215178591,19.7769325324869,-0.0545286541571083));
#100200=CARTESIAN_POINT('Ctrl Pts',(20.7540523227982,19.8487040161605,-0.0500424028513279));
#100201=CARTESIAN_POINT('Ctrl Pts',(20.7290450048267,19.919155652887,-0.0455561515455476));
#100202=CARTESIAN_POINT('Ctrl Pts',(20.704034580516,19.9896160409194,-0.0410693429701386));
#100203=CARTESIAN_POINT('Ctrl Pts',(20.6752852491506,20.0587558278079,-0.0365825343947297));
#100204=CARTESIAN_POINT('Ctrl Pts',(20.642965902348,20.1261711226173,-0.0320957258193207));
#100205=CARTESIAN_POINT('Ctrl Pts',(20.6106450021441,20.1935896576844,-0.0276087015893536));
#100206=CARTESIAN_POINT('Ctrl Pts',(20.5747539463686,20.2592831330904,-0.0231216773593865));
#100207=CARTESIAN_POINT('Ctrl Pts',(20.5355083127276,20.3228708554384,-0.0186346531294194));
#100208=CARTESIAN_POINT('Ctrl Pts',(20.4962355967949,20.3865024578589,-0.0141445325320924));
#100209=CARTESIAN_POINT('Ctrl Pts',(20.4536039241545,20.448025026832,-0.00965441193476544));
#100210=CARTESIAN_POINT('Ctrl Pts',(20.4078726283013,20.5070861947508,-0.00516429133743847));
#100211=CARTESIAN_POINT('Ctrl Pts',(20.390340082504,20.5297291706837,-0.00344286089162564));
#100212=CARTESIAN_POINT('Ctrl Pts',(20.3723523809939,20.5520106992443,-0.00172143044581282));
#100213=CARTESIAN_POINT('Ctrl Pts',(20.3539256943887,20.5739122292573,0.));
#100214=CARTESIAN_POINT('',(17.1140596925741,20.5738948603531,-2.19263332840784E-7));
#100215=CARTESIAN_POINT('Origin',(18.734,19.211,0.));
#100216=CARTESIAN_POINT('Ctrl Pts',(17.1140596925741,20.5738948603531,-2.19263332840784E-7));
#100217=CARTESIAN_POINT('Ctrl Pts',(17.1607064305025,20.6293392920392,-0.00438522669745406));
#100218=CARTESIAN_POINT('Ctrl Pts',(17.2102945911145,20.6824950671961,-0.00877023413157529));
#100219=CARTESIAN_POINT('Ctrl Pts',(17.2625707969828,20.7330332126823,-0.0131552415656965));
#100220=CARTESIAN_POINT('Ctrl Pts',(17.3147693813981,20.7834963174456,-0.0175337379946171));
#100221=CARTESIAN_POINT('Ctrl Pts',(17.3696477435682,20.8313491749508,-0.0219122344235377));
#100222=CARTESIAN_POINT('Ctrl Pts',(17.4269127458042,20.8762963429729,-0.0262907308524583));
#100223=CARTESIAN_POINT('Ctrl Pts',(17.4841103523031,20.9211906122365,-0.0306640741864182));
#100224=CARTESIAN_POINT('Ctrl Pts',(17.5436886409257,20.9631856884276,-0.035037417520378));
#100225=CARTESIAN_POINT('Ctrl Pts',(17.6053194410708,21.0020246218004,-0.0394107608543379));
#100226=CARTESIAN_POINT('Ctrl Pts',(17.6669112432927,21.0408389791861,-0.0437813368818933));
#100227=CARTESIAN_POINT('Ctrl Pts',(17.7305525723989,21.0765008992431,-0.0481519129094486));
#100228=CARTESIAN_POINT('Ctrl Pts',(17.7958853222653,21.1087960510599,-0.052522488937004));
#100229=CARTESIAN_POINT('Ctrl Pts',(17.8611983685244,21.1410814630298,-0.0568917468490167));
#100230=CARTESIAN_POINT('Ctrl Pts',(17.9282013899052,21.1700019086928,-0.0612610047610293));
#100231=CARTESIAN_POINT('Ctrl Pts',(17.9965121600447,21.1953892475817,-0.065630262673042));
#100232=CARTESIAN_POINT('Ctrl Pts',(18.0648249509204,21.2207773374667,-0.069999649834335));
#100233=CARTESIAN_POINT('Ctrl Pts',(18.1344451137109,21.242631946831,-0.074369036995628));
#100234=CARTESIAN_POINT('Ctrl Pts',(18.2049725448516,21.260833883928,-0.078738424156921));
#100235=CARTESIAN_POINT('Ctrl Pts',(18.275571771191,21.2790543501514,-0.0831122592473974));
#100236=CARTESIAN_POINT('Ctrl Pts',(18.3470796408085,21.2936146004556,-0.0874860943378738));
#100237=CARTESIAN_POINT('Ctrl Pts',(18.4190839151667,21.3044461682865,-0.0918599294283503));
#100238=CARTESIAN_POINT('Ctrl Pts',(18.4911280120912,21.3152837266066,-0.0962361835049201));
#100239=CARTESIAN_POINT('Ctrl Pts',(18.5636685792402,21.322388450086,-0.10061243758149));
#100240=CARTESIAN_POINT('Ctrl Pts',(18.6362889712809,21.3257438508875,-0.10498869165806));
#100241=CARTESIAN_POINT('Ctrl Pts',(18.7090335036842,21.3291049875528,-0.109372426688018));
#100242=CARTESIAN_POINT('Ctrl Pts',(18.7818576501798,21.3287040083353,-0.113756161717976));
#100243=CARTESIAN_POINT('Ctrl Pts',(18.8543461708051,21.3245765420662,-0.118139896747934));
#100244=CARTESIAN_POINT('Ctrl Pts',(18.8963545400865,21.3221846029601,-0.120680348096389));
#100245=CARTESIAN_POINT('Ctrl Pts',(18.9382502971219,21.318542128427,-0.123220799444843));
#100246=CARTESIAN_POINT('Ctrl Pts',(18.9799541345816,21.3136639207639,-0.125761250793297));
#100247=CARTESIAN_POINT('Ctrl Pts',(19.0521147654861,21.3052231017867,-0.130157023059195));
#100248=CARTESIAN_POINT('Ctrl Pts',(19.1239757191856,21.2930474831033,-0.134552795325092));
#100249=CARTESIAN_POINT('Ctrl Pts',(19.1951211491521,21.2771694717047,-0.13894856759099));
#100250=CARTESIAN_POINT('Ctrl Pts',(19.2661637519632,21.2613144089446,-0.143337986606115));
#100251=CARTESIAN_POINT('Ctrl Pts',(19.336492418998,21.2417676813877,-0.14772740562124));
#100252=CARTESIAN_POINT('Ctrl Pts',(19.4056976665711,21.2186133205184,-0.152116824636366));
#100253=CARTESIAN_POINT('Ctrl Pts',(19.4748248958988,21.1954850626206,-0.156501295258381));
#100254=CARTESIAN_POINT('Ctrl Pts',(19.5428307683091,21.1687574028734,-0.160885765880396));
#100255=CARTESIAN_POINT('Ctrl Pts',(19.60931884804,21.1385647626645,-0.165270236502412));
#100256=CARTESIAN_POINT('Ctrl Pts',(19.6757666435217,21.1083904157775,-0.169652050631601));
#100257=CARTESIAN_POINT('Ctrl Pts',(19.7406980347465,21.0747554526423,-0.17403386476079));
#100258=CARTESIAN_POINT('Ctrl Pts',(19.8037358627713,21.0378426817602,-0.178415678889979));
#100259=CARTESIAN_POINT('Ctrl Pts',(19.8667560838771,21.0009402208808,-0.182796269146949));
#100260=CARTESIAN_POINT('Ctrl Pts',(19.9278833775877,20.9607620127547,-0.18717685940392));
#100261=CARTESIAN_POINT('Ctrl Pts',(19.9867660017252,20.9175363590974,-0.19155744966089));
#100262=CARTESIAN_POINT('Ctrl Pts',(20.0456514086938,20.8743086625677,-0.1959382469474));
#100263=CARTESIAN_POINT('Ctrl Pts',(20.1022915493499,20.828033520426,-0.20031904423391));
#100264=CARTESIAN_POINT('Ctrl Pts',(20.1563657971912,20.7789810391011,-0.20469984152042));
#100265=CARTESIAN_POINT('Ctrl Pts',(20.2104971638002,20.7298767435135,-0.209085266254415));
#100266=CARTESIAN_POINT('Ctrl Pts',(20.2620568697778,20.6779895750516,-0.213470690988409));
#100267=CARTESIAN_POINT('Ctrl Pts',(20.3107599897288,20.6236276702623,-0.217856115722404));
#100268=CARTESIAN_POINT('Ctrl Pts',(20.3594903544991,20.569235355095,-0.222243993689482));
#100269=CARTESIAN_POINT('Ctrl Pts',(20.4053606496669,20.5123659213336,-0.226631871656561));
#100270=CARTESIAN_POINT('Ctrl Pts',(20.4481269507232,20.4533597694728,-0.23101974962364));
#100271=CARTESIAN_POINT('Ctrl Pts',(20.4909689880789,20.3942491216075,-0.235415398233292));
#100272=CARTESIAN_POINT('Ctrl Pts',(20.5306957923997,20.3329946025317,-0.239811046842944));
#100273=CARTESIAN_POINT('Ctrl Pts',(20.5671076961722,20.2699641987499,-0.244206695452596));
#100274=CARTESIAN_POINT('Ctrl Pts',(20.5912140439174,20.2282351850303,-0.247116816126641));
#100275=CARTESIAN_POINT('Ctrl Pts',(20.613868403521,20.1857283140019,-0.250026936800686));
#100276=CARTESIAN_POINT('Ctrl Pts',(20.6350244604073,20.1425551518472,-0.252937057474731));
#100277=CARTESIAN_POINT('Ctrl Pts',(20.6668851126084,20.0775371236191,-0.257319648387443));
#100278=CARTESIAN_POINT('Ctrl Pts',(20.6954700480251,20.010752620059,-0.261702239300154));
#100279=CARTESIAN_POINT('Ctrl Pts',(20.720580205096,19.9425655054202,-0.266084830212866));
#100280=CARTESIAN_POINT('Ctrl Pts',(20.745652583015,19.8744809807951,-0.270460827356882));
#100281=CARTESIAN_POINT('Ctrl Pts',(20.7672603940222,19.8049984839898,-0.274836824500899));
#100282=CARTESIAN_POINT('Ctrl Pts',(20.7852512551748,19.7345048119585,-0.279212821644915));
#100283=CARTESIAN_POINT('Ctrl Pts',(20.8032205628375,19.6640955930635,-0.283583576237753));
#100284=CARTESIAN_POINT('Ctrl Pts',(20.8175814089924,19.5926780716228,-0.287954330830591));
#100285=CARTESIAN_POINT('Ctrl Pts',(20.8282307375361,19.520655644158,-0.292325085423429));
#100286=CARTESIAN_POINT('Ctrl Pts',(20.8388731698584,19.4486798564986,-0.296693009632021));
#100287=CARTESIAN_POINT('Ctrl Pts',(20.845808782324,19.3761004173276,-0.301060933840613));
#100288=CARTESIAN_POINT('Ctrl Pts',(20.8489855761766,19.3033309946066,-0.305428858049204));
#100289=CARTESIAN_POINT('Ctrl Pts',(20.8521613682029,19.2305845202815,-0.309795404799378));
#100290=CARTESIAN_POINT('Ctrl Pts',(20.8515806736046,19.157648664371,-0.314161951549551));
#100291=CARTESIAN_POINT('Ctrl Pts',(20.8472434850165,19.0849405971962,-0.318528498299725));
#100292=CARTESIAN_POINT('Ctrl Pts',(20.842906223341,19.0122313047932,-0.32289511863205));
#100293=CARTESIAN_POINT('Ctrl Pts',(20.8348123728149,18.939750291573,-0.327261738964374));
#100294=CARTESIAN_POINT('Ctrl Pts',(20.8230139324319,18.8679113961303,-0.331628359296699));
#100295=CARTESIAN_POINT('Ctrl Pts',(20.8112032798744,18.7959981426279,-0.335999499373007));
#100296=CARTESIAN_POINT('Ctrl Pts',(20.7956804601328,18.7247288123433,-0.340370639449314));
#100297=CARTESIAN_POINT('Ctrl Pts',(20.7765488036571,18.654507965305,-0.344741779525621));
#100298=CARTESIAN_POINT('Ctrl Pts',(20.7574067702789,18.5842490308754,-0.349115290483651));
#100299=CARTESIAN_POINT('Ctrl Pts',(20.7346521545122,18.5150401717766,-0.353488801441681));
#100300=CARTESIAN_POINT('Ctrl Pts',(20.7084376488589,18.4472690455607,-0.35786231239971));
#100301=CARTESIAN_POINT('Ctrl Pts',(20.6821764073163,18.3793770952527,-0.362243620564609));
#100302=CARTESIAN_POINT('Ctrl Pts',(20.6524431558452,18.31292843841,-0.366624928729508));
#100303=CARTESIAN_POINT('Ctrl Pts',(20.6194377827199,18.2482885336238,-0.371006236894407));
#100304=CARTESIAN_POINT('Ctrl Pts',(20.5965703635706,18.2035034681465,-0.374041779314993));
#100305=CARTESIAN_POINT('Ctrl Pts',(20.572133215651,18.1595861430692,-0.37707732173558));
#100306=CARTESIAN_POINT('Ctrl Pts',(20.54620485702,18.1166497104705,-0.380112864156166));
#100307=CARTESIAN_POINT('Ctrl Pts',(20.5087129403854,18.0545644402657,-0.384502201136292));
#100308=CARTESIAN_POINT('Ctrl Pts',(20.4679538797132,17.9942872987423,-0.388891538116418));
#100309=CARTESIAN_POINT('Ctrl Pts',(20.4241274618398,17.9361830865827,-0.393280875096543));
#100310=CARTESIAN_POINT('Ctrl Pts',(20.3803660305827,17.8781650324146,-0.397663703487278));
#100311=CARTESIAN_POINT('Ctrl Pts',(20.3335465592593,17.8223138929918,-0.402046531878012));
#100312=CARTESIAN_POINT('Ctrl Pts',(20.2839133009206,17.7689674900928,-0.406429360268747));
#100313=CARTESIAN_POINT('Ctrl Pts',(20.2343383423802,17.7156837484943,-0.410807040538664));
#100314=CARTESIAN_POINT('Ctrl Pts',(20.1819564893205,17.6648992500388,-0.415184720808581));
#100315=CARTESIAN_POINT('Ctrl Pts',(20.127052568789,17.616919217671,-0.419562401078499));
#100316=CARTESIAN_POINT('Ctrl Pts',(20.0721834605648,17.5689696074592,-0.423937305642242));
#100317=CARTESIAN_POINT('Ctrl Pts',(20.0147958199512,17.5238212515477,-0.428312210205985));
#100318=CARTESIAN_POINT('Ctrl Pts',(19.9552106611291,17.4817419159811,-0.432687114769728));
#100319=CARTESIAN_POINT('Ctrl Pts',(19.8956436547536,17.4396753997626,-0.437060686531434));
#100320=CARTESIAN_POINT('Ctrl Pts',(19.8338808528525,17.4006763255856,-0.44143425829314));
#100321=CARTESIAN_POINT('Ctrl Pts',(19.7702742782371,17.3649705797945,-0.445807830054846));
#100322=CARTESIAN_POINT('Ctrl Pts',(19.706666129022,17.3292639500971,-0.450181510085624));
#100323=CARTESIAN_POINT('Ctrl Pts',(19.6412145378353,17.2968510448943,-0.454555190116402));
#100324=CARTESIAN_POINT('Ctrl Pts',(19.5742968108292,17.2679121816783,-0.45892887014718));
#100325=CARTESIAN_POINT('Ctrl Pts',(19.5073098565464,17.2389433808242,-0.463307074808002));
#100326=CARTESIAN_POINT('Ctrl Pts',(19.4388541815959,17.2134559893026,-0.467685279468823));
#100327=CARTESIAN_POINT('Ctrl Pts',(19.3693270226857,17.191582119955,-0.472063484129645));
#100328=CARTESIAN_POINT('Ctrl Pts',(19.2997619936054,17.1696963363115,-0.476444073518358));
#100329=CARTESIAN_POINT('Ctrl Pts',(19.2291247856183,17.1514281144628,-0.480824662907072));
#100330=CARTESIAN_POINT('Ctrl Pts',(19.1578251136208,17.1368589071463,-0.485205252295786));
#100331=CARTESIAN_POINT('Ctrl Pts',(19.0863994489354,17.1222639547802,-0.489593582564878));
#100332=CARTESIAN_POINT('Ctrl Pts',(19.0143094596386,17.1113811421464,-0.49398191283397));
#100333=CARTESIAN_POINT('Ctrl Pts',(18.9419717193455,17.1042402215838,-0.498370243103063));
#100334=CARTESIAN_POINT('Ctrl Pts',(18.8929675902332,17.0994027108761,-0.501343052347909));
#100335=CARTESIAN_POINT('Ctrl Pts',(18.8438498553954,17.0962813345305,-0.504315861592754));
#100336=CARTESIAN_POINT('Ctrl Pts',(18.7947475345845,17.0948717578932,-0.5072886708376));
#100337=CARTESIAN_POINT('Ctrl Pts',(18.7222522737112,17.0927906418817,-0.511677762395248));
#100338=CARTESIAN_POINT('Ctrl Pts',(18.6495091103977,17.0944351532161,-0.516066853952897));
#100339=CARTESIAN_POINT('Ctrl Pts',(18.5769329023863,17.0998346993077,-0.520455945510545));
#100340=CARTESIAN_POINT('Ctrl Pts',(18.5044640605617,17.1052262575382,-0.524838544030911));
#100341=CARTESIAN_POINT('Ctrl Pts',(18.4321621606072,17.1143617873598,-0.529221142551278));
#100342=CARTESIAN_POINT('Ctrl Pts',(18.3604434342997,17.1272187033611,-0.533603741071644));
#100343=CARTESIAN_POINT('Ctrl Pts',(18.2888085527943,17.1400605886216,-0.537981215991463));
#100344=CARTESIAN_POINT('Ctrl Pts',(18.2177559628244,17.1566151328626,-0.542358690911283));
#100345=CARTESIAN_POINT('Ctrl Pts',(18.1476964397083,17.1768079895965,-0.546736165831102));
#100346=CARTESIAN_POINT('Ctrl Pts',(18.0776810968814,17.1969881124977,-0.551110880268134));
#100347=CARTESIAN_POINT('Ctrl Pts',(18.0086580405141,17.2208018623067,-0.555485594705165));
#100348=CARTESIAN_POINT('Ctrl Pts',(17.9410261268036,17.2481241923066,-0.559860309142197));
#100349=CARTESIAN_POINT('Ctrl Pts',(17.8734145775147,17.2754382953703,-0.564233706323445));
#100350=CARTESIAN_POINT('Ctrl Pts',(17.8071937860416,17.3062587006989,-0.568607103504694));
#100351=CARTESIAN_POINT('Ctrl Pts',(17.742744167297,17.340411623544,-0.572980500685942));
#100352=CARTESIAN_POINT('Ctrl Pts',(17.6782927189291,17.3745655159369,-0.577354022021053));
#100353=CARTESIAN_POINT('Ctrl Pts',(17.6156129682129,17.4120518861517,-0.581727543356163));
#100354=CARTESIAN_POINT('Ctrl Pts',(17.5550606878344,17.4526510305885,-0.586101064691274));
#100355=CARTESIAN_POINT('Ctrl Pts',(17.4944454063011,17.4932924160932,-0.590479136423054));
#100356=CARTESIAN_POINT('Ctrl Pts',(17.435962415829,17.5370527729163,-0.594857208154835));
#100357=CARTESIAN_POINT('Ctrl Pts',(17.3799377355334,17.5836695529341,-0.599235279886616));
#100358=CARTESIAN_POINT('Ctrl Pts',(17.3238823567118,17.6303118764521,-0.603615750567369));
#100359=CARTESIAN_POINT('Ctrl Pts',(17.2702883244171,17.6798134120468,-0.607996221248123));
#100360=CARTESIAN_POINT('Ctrl Pts',(17.2194458037231,17.7318737083872,-0.612376691928877));
#100361=CARTESIAN_POINT('Ctrl Pts',(17.1685131538602,17.7840262926627,-0.616764927924507));
#100362=CARTESIAN_POINT('Ctrl Pts',(17.1203420749117,17.8387463335722,-0.621153163920137));
#100363=CARTESIAN_POINT('Ctrl Pts',(17.0751829640465,17.895699638398,-0.625541399915768));
#100364=CARTESIAN_POINT('Ctrl Pts',(17.0445739865328,17.9343027550967,-0.628515759116857));
#100365=CARTESIAN_POINT('Ctrl Pts',(17.0153478916349,17.9739312043245,-0.631490118317945));
#100366=CARTESIAN_POINT('Ctrl Pts',(16.9875709408017,18.0144739696991,-0.634464477519034));
#100367=CARTESIAN_POINT('Ctrl Pts',(16.946006537119,18.0751406669388,-0.638915198812158));
#100368=CARTESIAN_POINT('Ctrl Pts',(16.9075293793436,18.1380885815645,-0.643365920105282));
#100369=CARTESIAN_POINT('Ctrl Pts',(16.8723941622653,18.202975841107,-0.647816641398406));
#100370=CARTESIAN_POINT('Ctrl Pts',(16.8373240418129,18.2677428810517,-0.652259116636339));
#100371=CARTESIAN_POINT('Ctrl Pts',(16.8055837739661,18.3344417187871,-0.656701591874273));
#100372=CARTESIAN_POINT('Ctrl Pts',(16.7773849587093,18.4027014288056,-0.661144067112207));
#100373=CARTESIAN_POINT('Ctrl Pts',(16.7661659236286,18.4298588846888,-0.662911527379083));
#100374=CARTESIAN_POINT('Ctrl Pts',(16.7555069732342,18.4572630951622,-0.66467898764596));
#100375=CARTESIAN_POINT('Ctrl Pts',(16.7454194503191,18.4848895418526,-0.666446447912836));
#100376=CARTESIAN_POINT('Origin',(-18.734,19.211,0.));
#100377=CARTESIAN_POINT('',(-20.7225806138391,18.4848897175613,-21.2464098975766));
#100378=CARTESIAN_POINT('',(-20.7225806137704,18.4848897173731,-21.4658225507677));
#100379=CARTESIAN_POINT('',(-20.7225806137986,18.4848897174502,0.));
#100380=CARTESIAN_POINT('',(-20.8509993841528,19.2093852254739,-21.5109437210328));
#100381=CARTESIAN_POINT('Ctrl Pts',(-20.7225806137704,18.4848897173731,
-21.4658225507677));
#100382=CARTESIAN_POINT('Ctrl Pts',(-20.7235160649965,18.4874516149495,
-21.4659708387453));
#100383=CARTESIAN_POINT('Ctrl Pts',(-20.7244465747682,18.4900153457236,
-21.4661191633266));
#100384=CARTESIAN_POINT('Ctrl Pts',(-20.7392648735409,18.5310899038959,
-21.4684945105102));
#100385=CARTESIAN_POINT('Ctrl Pts',(-20.752037343799,18.5699929221988,-21.4707297776479));
#100386=CARTESIAN_POINT('Ctrl Pts',(-20.769047825713,18.6273675720992,-21.4740351573867));
#100387=CARTESIAN_POINT('Ctrl Pts',(-20.7741789047585,18.6455652346253,
-21.4750848285083));
#100388=CARTESIAN_POINT('Ctrl Pts',(-20.7946969717739,18.7222520054448,
-21.47952257391));
#100389=CARTESIAN_POINT('Ctrl Pts',(-20.8078162681752,18.7813126039396,
-21.4829748366309));
#100390=CARTESIAN_POINT('Ctrl Pts',(-20.8199723987728,18.849765732952,-21.4870988243204));
#100391=CARTESIAN_POINT('Ctrl Pts',(-20.821498852619,18.8586939146429,-21.4876390876925));
#100392=CARTESIAN_POINT('Ctrl Pts',(-20.8236942930998,18.8720504219912,
-21.4884512443157));
#100393=CARTESIAN_POINT('Ctrl Pts',(-20.8244066210205,18.8764716559285,
-21.4887207236647));
#100394=CARTESIAN_POINT('Ctrl Pts',(-20.8256595713244,18.8844086792473,
-21.4892056988168));
#100395=CARTESIAN_POINT('Ctrl Pts',(-20.8262053651736,18.887923596436,-21.4894208972808));
#100396=CARTESIAN_POINT('Ctrl Pts',(-20.8272520064275,18.8947778637196,
-21.4898413773222));
#100397=CARTESIAN_POINT('Ctrl Pts',(-20.8277537217311,18.8981170278596,
-21.4900466025942));
#100398=CARTESIAN_POINT('Ctrl Pts',(-20.8288494645378,18.905530405555,-21.4905030547554));
#100399=CARTESIAN_POINT('Ctrl Pts',(-20.8294395976159,18.9096051687625,
-21.4907544964867));
#100400=CARTESIAN_POINT('Ctrl Pts',(-20.8308794579733,18.9197558115371,
-21.4913821951212));
#100401=CARTESIAN_POINT('Ctrl Pts',(-20.8317146611703,18.9258336681553,
-21.4917592268512));
#100402=CARTESIAN_POINT('Ctrl Pts',(-20.8356021208692,18.9550646364502,
-21.4935779570296));
#100403=CARTESIAN_POINT('Ctrl Pts',(-20.8382974076893,18.9782625879247,
-21.4950376552817));
#100404=CARTESIAN_POINT('Ctrl Pts',(-20.8474812625982,19.0706096824942,
-21.5009009210641));
#100405=CARTESIAN_POINT('Ctrl Pts',(-20.8509485247462,19.1400100451708,
-21.505422601223));
#100406=CARTESIAN_POINT('Ctrl Pts',(-20.8509994310935,19.209447985236,-21.5099894778226));
#100407=CARTESIAN_POINT('',(-17.1140743056112,17.8480877707428,-22.));
#100408=CARTESIAN_POINT('Ctrl Pts',(-20.8509993841528,19.2093852254739,
-21.5109437210328));
#100409=CARTESIAN_POINT('Ctrl Pts',(-20.8510560152528,19.2836296489979,
-21.5154240901546));
#100410=CARTESIAN_POINT('Ctrl Pts',(-20.8472020809542,19.3580185555351,
-21.5199044592764));
#100411=CARTESIAN_POINT('Ctrl Pts',(-20.8394225376055,19.4320993852161,
-21.5243848283982));
#100412=CARTESIAN_POINT('Ctrl Pts',(-20.8319236730415,19.5035074465459,
-21.5287035499137));
#100413=CARTESIAN_POINT('Ctrl Pts',(-20.8207776605642,19.5746287335346,
-21.5330222714292));
#100414=CARTESIAN_POINT('Ctrl Pts',(-20.8060239446483,19.6450573381528,
-21.5373409929446));
#100415=CARTESIAN_POINT('Ctrl Pts',(-20.7912800573181,19.7154390248567,
-21.5416568374273));
#100416=CARTESIAN_POINT('Ctrl Pts',(-20.7729333327059,19.7851284592732,
-21.54597268191));
#100417=CARTESIAN_POINT('Ctrl Pts',(-20.751074714518,19.85372746639,-21.5502885263927));
#100418=CARTESIAN_POINT('Ctrl Pts',(-20.7292229871427,19.9223048480364,
-21.5546030103284));
#100419=CARTESIAN_POINT('Ctrl Pts',(-20.7038617135749,19.989792011532,-21.5589174942642));
#100420=CARTESIAN_POINT('Ctrl Pts',(-20.6751318580095,20.0558053680112,
-21.5632319782));
#100421=CARTESIAN_POINT('Ctrl Pts',(-20.6464009777761,20.1218210788973,
-21.5675466160145));
#100422=CARTESIAN_POINT('Ctrl Pts',(-20.6143014783329,20.1863624243994,
-21.5718612538289));
#100423=CARTESIAN_POINT('Ctrl Pts',(-20.5790219329057,20.2490669858429,
-21.5761758916434));
#100424=CARTESIAN_POINT('Ctrl Pts',(-20.5437074985004,20.3118335576677,
-21.5804947963299));
#100425=CARTESIAN_POINT('Ctrl Pts',(-20.5052069895562,20.3727592890194,
-21.5848137010164));
#100426=CARTESIAN_POINT('Ctrl Pts',(-20.4637537248945,20.4315085215654,
-21.5891326057028));
#100427=CARTESIAN_POINT('Ctrl Pts',(-20.4222758047099,20.490292696909,-21.5934540791822));
#100428=CARTESIAN_POINT('Ctrl Pts',(-20.3778419441492,20.5468974099959,
-21.5977755526616));
#100429=CARTESIAN_POINT('Ctrl Pts',(-20.3307256309594,20.6010202370604,
-21.602097026141));
#100430=CARTESIAN_POINT('Ctrl Pts',(-20.2835347289174,20.6552287448428,
-21.6064253408548));
#100431=CARTESIAN_POINT('Ctrl Pts',(-20.2336532518318,20.7069471772808,
-21.6107536555687));
#100432=CARTESIAN_POINT('Ctrl Pts',(-20.1813905512658,20.7559108686608,
-21.6150819702825));
#100433=CARTESIAN_POINT('Ctrl Pts',(-20.1677437911292,20.7686961963311,
-21.6162121735069));
#100434=CARTESIAN_POINT('Ctrl Pts',(-20.1539348377413,20.7812939190609,
-21.6173423767313));
#100435=CARTESIAN_POINT('Ctrl Pts',(-20.1399695343548,20.7936998036476,
-21.6184725799557));
#100436=CARTESIAN_POINT('Ctrl Pts',(-20.0856806209083,20.8419266108937,
-21.6228661475946));
#100437=CARTESIAN_POINT('Ctrl Pts',(-20.0288044225739,20.8874484514207,
-21.6272597152335));
#100438=CARTESIAN_POINT('Ctrl Pts',(-19.969641252187,20.9299763511735,-21.6316532828724));
#100439=CARTESIAN_POINT('Ctrl Pts',(-19.9105643807625,20.9724422171713,
-21.6360404417891));
#100440=CARTESIAN_POINT('Ctrl Pts',(-19.8492075475795,21.0119225341567,
-21.6404276007057));
#100441=CARTESIAN_POINT('Ctrl Pts',(-19.7859054205823,21.0481673810923,
-21.6448147596223));
#100442=CARTESIAN_POINT('Ctrl Pts',(-19.7226757606735,21.0843707356065,
-21.6491968962016));
#100443=CARTESIAN_POINT('Ctrl Pts',(-19.6575056463758,21.1173457404982,
-21.6535790327809));
#100444=CARTESIAN_POINT('Ctrl Pts',(-19.5907587261481,21.1468857107715,
-21.6579611693603));
#100445=CARTESIAN_POINT('Ctrl Pts',(-19.5240529471153,21.1764074733181,
-21.6623406048961));
#100446=CARTESIAN_POINT('Ctrl Pts',(-19.4557727294709,21.2024982084515,
-21.6667200404319));
#100447=CARTESIAN_POINT('Ctrl Pts',(-19.3863050672729,21.2249977902694,
-21.6710994759677));
#100448=CARTESIAN_POINT('Ctrl Pts',(-19.3168574801292,21.2474908700645,
-21.675477645916));
#100449=CARTESIAN_POINT('Ctrl Pts',(-19.2462235870207,21.2663947090105,
-21.6798558158643));
#100450=CARTESIAN_POINT('Ctrl Pts',(-19.1748074790919,21.2815984077982,
-21.6842339858126));
#100451=CARTESIAN_POINT('Ctrl Pts',(-19.1033886290296,21.2968026903559,
-21.6886123238676));
#100452=CARTESIAN_POINT('Ctrl Pts',(-19.0311879752792,21.3083064524741,
-21.6929906619226));
#100453=CARTESIAN_POINT('Ctrl Pts',(-18.9586201563122,21.3160498296663,
-21.6973689999776));
#100454=CARTESIAN_POINT('Ctrl Pts',(-18.8859763854436,21.3238013113356,
-21.7017519205474));
#100455=CARTESIAN_POINT('Ctrl Pts',(-18.8129651613081,21.3277844990936,
-21.7061348411171));
#100456=CARTESIAN_POINT('Ctrl Pts',(-18.740005792739,21.3279914809591,-21.7105177616869));
#100457=CARTESIAN_POINT('Ctrl Pts',(-18.667006069685,21.3281985773082,-21.7149031064896));
#100458=CARTESIAN_POINT('Ctrl Pts',(-18.594058739949,21.324625332556,-21.7192884512922));
#100459=CARTESIAN_POINT('Ctrl Pts',(-18.5215799495222,21.3173159122399,
-21.7236737960949));
#100460=CARTESIAN_POINT('Ctrl Pts',(-18.4489730689546,21.3099935741492,
-21.7280668910191));
#100461=CARTESIAN_POINT('Ctrl Pts',(-18.3768368570158,21.2989219477122,
-21.7324599859433));
#100462=CARTESIAN_POINT('Ctrl Pts',(-18.3055786328722,21.284196597573,-21.7368530808674));
#100463=CARTESIAN_POINT('Ctrl Pts',(-18.2580238618235,21.2743695121678,
-21.7397848494573));
#100464=CARTESIAN_POINT('Ctrl Pts',(-18.2108598781006,21.2629162374028,
-21.7427166180472));
#100465=CARTESIAN_POINT('Ctrl Pts',(-18.1642034712006,21.2498773665349,
-21.7456483866371));
#100466=CARTESIAN_POINT('Ctrl Pts',(-18.0951059728948,21.230566977725,-21.7499902956831));
#100467=CARTESIAN_POINT('Ctrl Pts',(-18.0268401014068,21.2076976293853,
-21.754332204729));
#100468=CARTESIAN_POINT('Ctrl Pts',(-17.959804544219,21.1813579360736,-21.758674113775));
#100469=CARTESIAN_POINT('Ctrl Pts',(-17.8928699309423,21.1550579057671,
-21.7630094846598));
#100470=CARTESIAN_POINT('Ctrl Pts',(-17.8271624114981,21.1252980759476,
-21.7673448555445));
#100471=CARTESIAN_POINT('Ctrl Pts',(-17.7630671934661,21.0922172881398,
-21.7716802264293));
#100472=CARTESIAN_POINT('Ctrl Pts',(-17.6990456418676,21.0591745210102,
-21.7760106145506));
#100473=CARTESIAN_POINT('Ctrl Pts',(-17.6366331495171,21.0228185970339,
-21.7803410026719));
#100474=CARTESIAN_POINT('Ctrl Pts',(-17.5761948535926,20.9833363797407,
-21.7846713907932));
#100475=CARTESIAN_POINT('Ctrl Pts',(-17.5157937013986,20.9438784271429,
-21.7889991175759));
#100476=CARTESIAN_POINT('Ctrl Pts',(-17.4573647522916,20.9012982594394,
-21.7933268443586));
#100477=CARTESIAN_POINT('Ctrl Pts',(-17.4012470250051,20.8558278048605,
-21.7976545711413));
#100478=CARTESIAN_POINT('Ctrl Pts',(-17.3451443445715,20.81036954228,-21.8019811375301));
#100479=CARTESIAN_POINT('Ctrl Pts',(-17.2913520397843,20.7620228406339,
-21.8063077039189));
#100480=CARTESIAN_POINT('Ctrl Pts',(-17.2401772158046,20.7110608285729,
-21.8106342703077));
#100481=CARTESIAN_POINT('Ctrl Pts',(-17.1889983840908,20.6600948254439,
-21.8149611755297));
#100482=CARTESIAN_POINT('Ctrl Pts',(-17.1404377881069,20.6065134551268,
-21.8192880807517));
#100483=CARTESIAN_POINT('Ctrl Pts',(-17.0947654083712,20.5506264231522,
-21.8236149859736));
#100484=CARTESIAN_POINT('Ctrl Pts',(-17.0490382189606,20.4946723232895,
-21.827947083749));
#100485=CARTESIAN_POINT('Ctrl Pts',(-17.0062064773784,20.4364074215726,
-21.8322791815243));
#100486=CARTESIAN_POINT('Ctrl Pts',(-16.9664990268283,20.3761735106142,
-21.8366112792996));
#100487=CARTESIAN_POINT('Ctrl Pts',(-16.9267670699395,20.3159024249543,
-21.8409460507257));
#100488=CARTESIAN_POINT('Ctrl Pts',(-16.8901634882159,20.2536603390498,
-21.8452808221518));
#100489=CARTESIAN_POINT('Ctrl Pts',(-16.856871493227,20.1898143690508,-21.8496155935779));
#100490=CARTESIAN_POINT('Ctrl Pts',(-16.8235124512874,20.1258398192654,
-21.8539590948264));
#100491=CARTESIAN_POINT('Ctrl Pts',(-16.7934785159735,20.060255385527,-21.858302596075));
#100492=CARTESIAN_POINT('Ctrl Pts',(-16.7669047947946,19.9934483712413,
-21.8626460973235));
#100493=CARTESIAN_POINT('Ctrl Pts',(-16.7461481233425,19.9412655686561,
-21.8660387959885));
#100494=CARTESIAN_POINT('Ctrl Pts',(-16.7275016016086,19.8883372861217,
-21.8694314946536));
#100495=CARTESIAN_POINT('Ctrl Pts',(-16.7110080073322,19.8348528653473,
-21.8728241933186));
#100496=CARTESIAN_POINT('Ctrl Pts',(-16.6890808041098,19.7637486691424,
-21.8773345742491));
#100497=CARTESIAN_POINT('Ctrl Pts',(-16.6708715122103,19.691373744136,-21.8818449551797));
#100498=CARTESIAN_POINT('Ctrl Pts',(-16.6565194069635,19.6181404985465,
-21.8863553361102));
#100499=CARTESIAN_POINT('Ctrl Pts',(-16.6414519418388,19.5412570480063,
-21.891090530439));
#100500=CARTESIAN_POINT('Ctrl Pts',(-16.6306364194547,19.4634279279486,
-21.8958257247677));
#100501=CARTESIAN_POINT('Ctrl Pts',(-16.6241751632239,19.3851498151671,
-21.9005609190965));
#100502=CARTESIAN_POINT('Ctrl Pts',(-16.618041130639,19.3108360165285,-21.9050563044009));
#100503=CARTESIAN_POINT('Ctrl Pts',(-16.6158311432077,19.2361181121913,
-21.9095516897054));
#100504=CARTESIAN_POINT('Ctrl Pts',(-16.6175804022592,19.1614309945752,
-21.9140470750099));
#100505=CARTESIAN_POINT('Ctrl Pts',(-16.6193280165078,19.0868141041766,
-21.9185382333685));
#100506=CARTESIAN_POINT('Ctrl Pts',(-16.6250274669155,19.0122283910569,
-21.9230293917272));
#100507=CARTESIAN_POINT('Ctrl Pts',(-16.6346619440205,18.9381104129575,
-21.9275205500858));
#100508=CARTESIAN_POINT('Ctrl Pts',(-16.644289879149,18.8640427622465,-21.9320086588702));
#100509=CARTESIAN_POINT('Ctrl Pts',(-16.6578474702978,18.7904426603016,
-21.9364967676547));
#100510=CARTESIAN_POINT('Ctrl Pts',(-16.6752660492705,18.7177419335545,
-21.9409848764392));
#100511=CARTESIAN_POINT('Ctrl Pts',(-16.6926773473537,18.6450715953915,
-21.9454711092139));
#100512=CARTESIAN_POINT('Ctrl Pts',(-16.7139463177063,18.5733003216091,
-21.9499573419886));
#100513=CARTESIAN_POINT('Ctrl Pts',(-16.7389533863518,18.5028488795668,
-21.9544435747634));
#100514=CARTESIAN_POINT('Ctrl Pts',(-16.7639635634828,18.432388680109,-21.958930365196));
#100515=CARTESIAN_POINT('Ctrl Pts',(-16.7927126236932,18.363249066819,-21.9634171556287));
#100516=CARTESIAN_POINT('Ctrl Pts',(-16.8250316763889,18.2958339279402,
-21.9679039460613));
#100517=CARTESIAN_POINT('Ctrl Pts',(-16.8573522841798,18.2284155452484,
-21.9723909523848));
#100518=CARTESIAN_POINT('Ctrl Pts',(-16.8932430249613,18.1627222047342,
-21.9768779587083));
#100519=CARTESIAN_POINT('Ctrl Pts',(-16.9324883220855,18.0991345970228,
-21.9813649650317));
#100520=CARTESIAN_POINT('Ctrl Pts',(-16.9717607058636,18.0355031018739,
-21.9858550682355));
#100521=CARTESIAN_POINT('Ctrl Pts',(-17.0143920255779,17.9739806203857,
-21.9903451714393));
#100522=CARTESIAN_POINT('Ctrl Pts',(-17.0601229488358,17.9149195173194,
-21.994835274643));
#100523=CARTESIAN_POINT('Ctrl Pts',(-17.0776568931743,17.8922745755608,
-21.996556849762));
#100524=CARTESIAN_POINT('Ctrl Pts',(-17.0956460703827,17.8699911414134,
-21.998278424881));
#100525=CARTESIAN_POINT('Ctrl Pts',(-17.1140743056111,17.8480877707428,
-22.));
#100526=CARTESIAN_POINT('',(-20.3539402646795,17.8481050888384,-21.9999997807644));
#100527=CARTESIAN_POINT('Origin',(-18.734,19.211,-22.));
#100528=CARTESIAN_POINT('',(-20.8509997094733,19.2098909057104,-21.2890562790225));
#100529=CARTESIAN_POINT('Ctrl Pts',(-20.3539402646795,17.8481050888384,
-21.9999997807644));
#100530=CARTESIAN_POINT('Ctrl Pts',(-20.3072934957001,17.7926606237751,
-21.9956147707751));
#100531=CARTESIAN_POINT('Ctrl Pts',(-20.2577053013778,17.7395048193498,
-21.9912297607858));
#100532=CARTESIAN_POINT('Ctrl Pts',(-20.2054290597327,17.6889666487971,
-21.9868447507965));
#100533=CARTESIAN_POINT('Ctrl Pts',(-20.1532304392223,17.6385035186453,
-21.982466251785));
#100534=CARTESIAN_POINT('Ctrl Pts',(-20.0983520388586,17.5906506399773,
-21.9780877527736));
#100535=CARTESIAN_POINT('Ctrl Pts',(-20.0410869968869,17.545703455066,-21.9737092537621));
#100536=CARTESIAN_POINT('Ctrl Pts',(-19.9838893502852,17.5008091686081,
-21.969335907817));
#100537=CARTESIAN_POINT('Ctrl Pts',(-19.9243110199867,17.4588140795273,
-21.9649625618719));
#100538=CARTESIAN_POINT('Ctrl Pts',(-19.8626801771137,17.4199751375844,
-21.9605892159267));
#100539=CARTESIAN_POINT('Ctrl Pts',(-19.8010883319371,17.381160771474,-21.9562186372717));
#100540=CARTESIAN_POINT('Ctrl Pts',(-19.7374469588082,17.3454988470316,
-21.9518480586166));
#100541=CARTESIAN_POINT('Ctrl Pts',(-19.6721141643387,17.3132036951593,
-21.9474774799615));
#100542=CARTESIAN_POINT('Ctrl Pts',(-19.6068010732891,17.2809182830347,
-21.9431082194094));
#100543=CARTESIAN_POINT('Ctrl Pts',(-19.539798006527,17.2519978415642,-21.9387389588572));
#100544=CARTESIAN_POINT('Ctrl Pts',(-19.4714871908732,17.2266105111904,
-21.934369698305));
#100545=CARTESIAN_POINT('Ctrl Pts',(-19.4031743543433,17.2012224297694,
-21.9300003084946));
#100546=CARTESIAN_POINT('Ctrl Pts',(-19.33355414576,17.1793678332055,-21.9256309186843));
#100547=CARTESIAN_POINT('Ctrl Pts',(-19.2630266691229,17.1611659132123,
-21.9212615288739));
#100548=CARTESIAN_POINT('Ctrl Pts',(-19.1924273973489,17.142945464138,-21.9168876911383));
#100549=CARTESIAN_POINT('Ctrl Pts',(-19.1209194825959,17.1283852352836,
-21.9125138534028));
#100550=CARTESIAN_POINT('Ctrl Pts',(-19.0489151638194,17.1175536931661,
-21.9081400156672));
#100551=CARTESIAN_POINT('Ctrl Pts',(-18.9768710224476,17.1067161605729,
-21.9037637589438));
#100552=CARTESIAN_POINT('Ctrl Pts',(-18.9043304115686,17.0996114670891,
-21.8993875022204));
#100553=CARTESIAN_POINT('Ctrl Pts',(-18.8317099769259,17.096256100515,-21.895011245497));
#100554=CARTESIAN_POINT('Ctrl Pts',(-18.7589654023404,17.0928949981583,
-21.8906275078454));
#100555=CARTESIAN_POINT('Ctrl Pts',(-18.6861412147951,17.0932960158796,
-21.8862437701938));
#100556=CARTESIAN_POINT('Ctrl Pts',(-18.6136526546588,17.0974235248117,
-21.8818600325422));
#100557=CARTESIAN_POINT('Ctrl Pts',(-18.5716446773508,17.099815465019,-21.8793196047637));
#100558=CARTESIAN_POINT('Ctrl Pts',(-18.5297493105789,17.1034579173405,
-21.8767791769852));
#100559=CARTESIAN_POINT('Ctrl Pts',(-18.4880458594114,17.1083360799388,
-21.8742387492067));
#100560=CARTESIAN_POINT('Ctrl Pts',(-18.4158852200683,17.116776900112,-21.8698429764932));
#100561=CARTESIAN_POINT('Ctrl Pts',(-18.3440242584073,17.1289525208195,
-21.8654472037797));
#100562=CARTESIAN_POINT('Ctrl Pts',(-18.272878821027,17.1448305349506,-21.8610514310662));
#100563=CARTESIAN_POINT('Ctrl Pts',(-18.2018362105903,17.160685600489,-21.8566620115904));
#100564=CARTESIAN_POINT('Ctrl Pts',(-18.1315075364803,17.1802323315536,
-21.8522725921145));
#100565=CARTESIAN_POINT('Ctrl Pts',(-18.0623022824371,17.2033866965422,
-21.8478831726387));
#100566=CARTESIAN_POINT('Ctrl Pts',(-17.9931750463637,17.2265149586492,
-21.8434987015386));
#100567=CARTESIAN_POINT('Ctrl Pts',(-17.9251691678202,17.2532426232453,
-21.8391142304384));
#100568=CARTESIAN_POINT('Ctrl Pts',(-17.8586810826102,17.2834352688276,
-21.8347297593383));
#100569=CARTESIAN_POINT('Ctrl Pts',(-17.7922332814893,17.3136096211591,
-21.8303479447205));
#100570=CARTESIAN_POINT('Ctrl Pts',(-17.7273018852858,17.3472445902797,
-21.8259661301027));
#100571=CARTESIAN_POINT('Ctrl Pts',(-17.6642640529712,17.384157367578,-21.8215843154849));
#100572=CARTESIAN_POINT('Ctrl Pts',(-17.601243827434,17.4210598349556,-21.8172037247295));
#100573=CARTESIAN_POINT('Ctrl Pts',(-17.5401165299889,17.4612380500253,
-21.8128231339742));
#100574=CARTESIAN_POINT('Ctrl Pts',(-17.4812339028314,17.5044637109674,
-21.8084425432188));
#100575=CARTESIAN_POINT('Ctrl Pts',(-17.4223484927206,17.547691414872,-21.8040617454248));
#100576=CARTESIAN_POINT('Ctrl Pts',(-17.365708349646,17.5939665647424,-21.7996809476307));
#100577=CARTESIAN_POINT('Ctrl Pts',(-17.3116341001189,17.6430190540522,
-21.7953001498367));
#100578=CARTESIAN_POINT('Ctrl Pts',(-17.2575027316979,17.692123357746,-21.7909147245846));
#100579=CARTESIAN_POINT('Ctrl Pts',(-17.2059430246541,17.7440105345835,
-21.7865292993325));
#100580=CARTESIAN_POINT('Ctrl Pts',(-17.1572399043858,17.798372447926,-21.7821438740803));
#100581=CARTESIAN_POINT('Ctrl Pts',(-17.1085095392263,17.852764771731,-21.7777559955884));
#100582=CARTESIAN_POINT('Ctrl Pts',(-17.0626392444271,17.9096342143152,
-21.7733681170964));
#100583=CARTESIAN_POINT('Ctrl Pts',(-17.0198729444951,17.9686403750982,
-21.7689802386045));
#100584=CARTESIAN_POINT('Ctrl Pts',(-16.9770309082245,18.0277510319582,
-21.7645845894648));
#100585=CARTESIAN_POINT('Ctrl Pts',(-16.9373041057529,18.0890055601327,
-21.7601889403251));
#100586=CARTESIAN_POINT('Ctrl Pts',(-16.9008922045882,18.1520359730375,
-21.7557932911855));
#100587=CARTESIAN_POINT('Ctrl Pts',(-16.8767858983712,18.1937649238989,
-21.7528831749654));
#100588=CARTESIAN_POINT('Ctrl Pts',(-16.8541315758308,18.2362717295104,
-21.7499730587453));
#100589=CARTESIAN_POINT('Ctrl Pts',(-16.8329755513189,18.2794448242231,
-21.7470629425252));
#100590=CARTESIAN_POINT('Ctrl Pts',(-16.8011149074337,18.3444628334097,
-21.7426803527574));
#100591=CARTESIAN_POINT('Ctrl Pts',(-16.772529978103,18.4112473176336,-21.7382977629896));
#100592=CARTESIAN_POINT('Ctrl Pts',(-16.7474198249775,18.4794344129146,
-21.7339151732219));
#100593=CARTESIAN_POINT('Ctrl Pts',(-16.7223474511024,18.5475189179272,
-21.7295391772393));
#100594=CARTESIAN_POINT('Ctrl Pts',(-16.7007396419766,18.6170013950868,
-21.7251631812567));
#100595=CARTESIAN_POINT('Ctrl Pts',(-16.6827487806458,18.6874950476855,
-21.7207871852741));
#100596=CARTESIAN_POINT('Ctrl Pts',(-16.6647794728902,18.7579042468375,
-21.7164164318621));
#100597=CARTESIAN_POINT('Ctrl Pts',(-16.650418624554,18.8293217487381,-21.71204567845));
#100598=CARTESIAN_POINT('Ctrl Pts',(-16.6397692918518,18.9013441570891,
-21.7076749250379));
#100599=CARTESIAN_POINT('Ctrl Pts',(-16.6291268554032,18.973319925447,-21.7033070020215));
#100600=CARTESIAN_POINT('Ctrl Pts',(-16.6221912368165,19.0458993457387,
-21.698939079005));
#100601=CARTESIAN_POINT('Ctrl Pts',(-16.6190144349639,19.1186687502037,
-21.6945711559885));
#100602=CARTESIAN_POINT('Ctrl Pts',(-16.6158386349475,19.19141520611,-21.6902046104402));
#100603=CARTESIAN_POINT('Ctrl Pts',(-16.6164193196609,19.2643510442235,
-21.6858380648919));
#100604=CARTESIAN_POINT('Ctrl Pts',(-16.6207564965869,19.3370590944058,
-21.6814715193436));
#100605=CARTESIAN_POINT('Ctrl Pts',(-16.6250937465921,19.4097683696811,
-21.6771049002213));
#100606=CARTESIAN_POINT('Ctrl Pts',(-16.6331875836567,19.4822493665785,
-21.6727382810989));
#100607=CARTESIAN_POINT('Ctrl Pts',(-16.6449860089037,19.5540882466713,
-21.6683716619766));
#100608=CARTESIAN_POINT('Ctrl Pts',(-16.6567966463011,19.6260014847561,
-21.6640005231147));
#100609=CARTESIAN_POINT('Ctrl Pts',(-16.6723194491993,19.6972708005986,
-21.6596293842528));
#100610=CARTESIAN_POINT('Ctrl Pts',(-16.6914510872628,19.7674916343271,
-21.6552582453909));
#100611=CARTESIAN_POINT('Ctrl Pts',(-16.7105931022024,19.8377505553794,
-21.6508847356516));
#100612=CARTESIAN_POINT('Ctrl Pts',(-16.7333476979536,19.9069594022358,
-21.6465112259124));
#100613=CARTESIAN_POINT('Ctrl Pts',(-16.7595621821267,19.9747305174941,
-21.6421377161732));
#100614=CARTESIAN_POINT('Ctrl Pts',(-16.7858234022015,20.0426224569562,
-21.6377564092208));
#100615=CARTESIAN_POINT('Ctrl Pts',(-16.8155566307479,20.1090711042367,
-21.6333751022684));
#100616=CARTESIAN_POINT('Ctrl Pts',(-16.8485619796008,20.1737110008893,
-21.6289937953161));
#100617=CARTESIAN_POINT('Ctrl Pts',(-16.8714294691446,20.2184962315317,
-21.6259582421587));
#100618=CARTESIAN_POINT('Ctrl Pts',(-16.8958666987907,20.2624137158362,
-21.6229226890013));
#100619=CARTESIAN_POINT('Ctrl Pts',(-16.9217951496002,20.3053503004923,
-21.6198871358439));
#100620=CARTESIAN_POINT('Ctrl Pts',(-16.9592870711159,20.3674355779312,
-21.6154977983717));
#100621=CARTESIAN_POINT('Ctrl Pts',(-17.0000461372983,20.4277127259959,
-21.6111084608995));
#100622=CARTESIAN_POINT('Ctrl Pts',(-17.0438725612033,20.4858169439674,
-21.6067191234274));
#100623=CARTESIAN_POINT('Ctrl Pts',(-17.0876339985392,20.5438350040133,
-21.6023362945397));
#100624=CARTESIAN_POINT('Ctrl Pts',(-17.1344534764691,20.5996861485813,
-21.597953465652));
#100625=CARTESIAN_POINT('Ctrl Pts',(-17.1840867418393,20.6530325558661,
-21.5935706367643));
#100626=CARTESIAN_POINT('Ctrl Pts',(-17.2336617074652,20.7063163019118,
-21.5891929559925));
#100627=CARTESIAN_POINT('Ctrl Pts',(-17.2860435680415,20.7571008040507,
-21.5848152752207));
#100628=CARTESIAN_POINT('Ctrl Pts',(-17.3409474964239,20.8050808393179,
-21.580437594449));
#100629=CARTESIAN_POINT('Ctrl Pts',(-17.3958166125325,20.853030452461,-21.5760626893806));
#100630=CARTESIAN_POINT('Ctrl Pts',(-17.4532042613681,20.8981788105171,
-21.5716877843123));
#100631=CARTESIAN_POINT('Ctrl Pts',(-17.512789428658,20.9402581474269,-21.5673128792439));
#100632=CARTESIAN_POINT('Ctrl Pts',(-17.5723564435283,20.9823246650092,
-21.5629393069756));
#100633=CARTESIAN_POINT('Ctrl Pts',(-17.6341192541722,21.0213237397462,
-21.5585657347073));
#100634=CARTESIAN_POINT('Ctrl Pts',(-17.6977258376919,21.0570294852826,
-21.5541921624389));
#100635=CARTESIAN_POINT('Ctrl Pts',(-17.7613339958298,21.0927361147356,
-21.5498184819002));
#100636=CARTESIAN_POINT('Ctrl Pts',(-17.826785596102,21.1251490188774,-21.5454448013616));
#100637=CARTESIAN_POINT('Ctrl Pts',(-17.8937033322731,21.1540878802069,
-21.5410711208229));
#100638=CARTESIAN_POINT('Ctrl Pts',(-17.9606902956987,21.1830566791589,
-21.5366929156557));
#100639=CARTESIAN_POINT('Ctrl Pts',(-18.0291459798704,21.2085440679544,
-21.5323147104885));
#100640=CARTESIAN_POINT('Ctrl Pts',(-18.0986731480005,21.2304179337444,
-21.5279365053214));
#100641=CARTESIAN_POINT('Ctrl Pts',(-18.1682381862999,21.2523037138266,
-21.5235559154264));
#100642=CARTESIAN_POINT('Ctrl Pts',(-18.2388754035045,21.2705719312819,
-21.5191753255314));
#100643=CARTESIAN_POINT('Ctrl Pts',(-18.3101750846391,21.2851411333656,
-21.5147947356365));
#100644=CARTESIAN_POINT('Ctrl Pts',(-18.3816007583693,21.2997360804675,
-21.5104064048669));
#100645=CARTESIAN_POINT('Ctrl Pts',(-18.4536907566283,21.3106188870059,
-21.5060180740973));
#100646=CARTESIAN_POINT('Ctrl Pts',(-18.5260285057222,21.3177598006341,
-21.5016297433277));
#100647=CARTESIAN_POINT('Ctrl Pts',(-18.5750325606489,21.3225972987322,
-21.4986569386059));
#100648=CARTESIAN_POINT('Ctrl Pts',(-18.6241502208557,21.3257186676998,
-21.4956841338842));
#100649=CARTESIAN_POINT('Ctrl Pts',(-18.6732524671973,21.3271282421579,
-21.4927113291624));
#100650=CARTESIAN_POINT('Ctrl Pts',(-18.7457477304191,21.3292093581758,
-21.4883222374839));
#100651=CARTESIAN_POINT('Ctrl Pts',(-18.8184908959863,21.3275648466035,
-21.4839331458055));
#100652=CARTESIAN_POINT('Ctrl Pts',(-18.8910671061329,21.3221653000585,
-21.479544054127));
#100653=CARTESIAN_POINT('Ctrl Pts',(-18.963535950148,21.316773741371,-21.4751614554825));
#100654=CARTESIAN_POINT('Ctrl Pts',(-19.0358378521743,21.3076382108716,
-21.4707788568379));
#100655=CARTESIAN_POINT('Ctrl Pts',(-19.1075565804155,21.2947812940009,
-21.4663962581934));
#100656=CARTESIAN_POINT('Ctrl Pts',(-19.1791914639276,21.2819394078585,
-21.462018783145));
#100657=CARTESIAN_POINT('Ctrl Pts',(-19.2502440557651,21.2653848625367,
-21.4576413080965));
#100658=CARTESIAN_POINT('Ctrl Pts',(-19.3203035805937,21.2451920045519,
-21.4532638330481));
#100659=CARTESIAN_POINT('Ctrl Pts',(-19.3903189251763,21.2250118803879,
-21.4488891184798));
#100660=CARTESIAN_POINT('Ctrl Pts',(-19.4593419831432,21.2011981291416,
-21.4445144039115));
#100661=CARTESIAN_POINT('Ctrl Pts',(-19.526973898285,21.1738757975579,-21.4401396893431));
#100662=CARTESIAN_POINT('Ctrl Pts',(-19.5945854490438,21.1465616928953,
-21.4357662920281));
#100663=CARTESIAN_POINT('Ctrl Pts',(-19.6608062418169,21.1157412858173,
-21.4313928947131));
#100664=CARTESIAN_POINT('Ctrl Pts',(-19.7252558616823,21.0815883610994,
-21.427019497398));
#100665=CARTESIAN_POINT('Ctrl Pts',(-19.789707311205,21.0474344668157,-21.4226459759268));
#100666=CARTESIAN_POINT('Ctrl Pts',(-19.8523870628951,21.0099480945831,
-21.4182724544556));
#100667=CARTESIAN_POINT('Ctrl Pts',(-19.9129393440595,20.9693489480272,
-21.4138989329844));
#100668=CARTESIAN_POINT('Ctrl Pts',(-19.9735546264145,20.9287075603779,
-21.4095208611139));
#100669=CARTESIAN_POINT('Ctrl Pts',(-20.0320376175175,20.8849472013051,
-21.4051427892433));
#100670=CARTESIAN_POINT('Ctrl Pts',(-20.0880622982484,20.8383304189569,
-21.4007647173728));
#100671=CARTESIAN_POINT('Ctrl Pts',(-20.1441176775264,20.7916880930898,
-21.3963842465516));
#100672=CARTESIAN_POINT('Ctrl Pts',(-20.1977117100798,20.7421865550631,
-21.3920037757304));
#100673=CARTESIAN_POINT('Ctrl Pts',(-20.2485542308314,20.6901262562305,
-21.3876233049092));
#100674=CARTESIAN_POINT('Ctrl Pts',(-20.2994868807634,20.637973669447,-21.3832350687719));
#100675=CARTESIAN_POINT('Ctrl Pts',(-20.3476579595778,20.5832536259681,
-21.3788468326346));
#100676=CARTESIAN_POINT('Ctrl Pts',(-20.3928170701037,20.5263003185328,
-21.3744585964973));
#100677=CARTESIAN_POINT('Ctrl Pts',(-20.4234260340952,20.4876972168292,
-21.3714842384918));
#100678=CARTESIAN_POINT('Ctrl Pts',(-20.4526521165782,20.448068783469,-21.3685098804864));
#100679=CARTESIAN_POINT('Ctrl Pts',(-20.4804290561878,20.407526034695,-21.3655355224809));
#100680=CARTESIAN_POINT('Ctrl Pts',(-20.5219871935396,20.3468684840126,
-21.361085472178));
#100681=CARTESIAN_POINT('Ctrl Pts',(-20.5604590169179,20.2839304044478,
-21.356635421875));
#100682=CARTESIAN_POINT('Ctrl Pts',(-20.5955899436348,20.2190535113564,
-21.3521853715721));
#100683=CARTESIAN_POINT('Ctrl Pts',(-20.6306645775744,20.1542805751153,
-21.3477424519006));
#100684=CARTESIAN_POINT('Ctrl Pts',(-20.6624087272335,20.0875754000713,
-21.3432995322291));
#100685=CARTESIAN_POINT('Ctrl Pts',(-20.6906107246637,20.0193090201965,
-21.3388566125576));
#100686=CARTESIAN_POINT('Ctrl Pts',(-20.7187694166618,19.9511474664102,
-21.3344205151885));
#100687=CARTESIAN_POINT('Ctrl Pts',(-20.7433965961624,19.8814299018275,
-21.3299844178194));
#100688=CARTESIAN_POINT('Ctrl Pts',(-20.7643270348899,19.8105507746598,
-21.3255483204504));
#100689=CARTESIAN_POINT('Ctrl Pts',(-20.7852384845802,19.7397359522305,
-21.3211162477088));
#100690=CARTESIAN_POINT('Ctrl Pts',(-20.8024597234804,19.667762104018,-21.3166841749672));
#100691=CARTESIAN_POINT('Ctrl Pts',(-20.8158744345335,19.5950414545796,
-21.3122521022256));
#100692=CARTESIAN_POINT('Ctrl Pts',(-20.8292816033587,19.5223616912788,
-21.307822521353));
#100693=CARTESIAN_POINT('Ctrl Pts',(-20.8388864096936,19.4489364165862,
-21.3033929404804));
#100694=CARTESIAN_POINT('Ctrl Pts',(-20.8446233306527,19.3751893909619,
-21.2989633596079));
#100695=CARTESIAN_POINT('Ctrl Pts',(-20.8489003446554,19.3202091910428,
-21.2956609994128));
#100696=CARTESIAN_POINT('Ctrl Pts',(-20.8510286075112,19.2650504520942,
-21.2923586392176));
#100697=CARTESIAN_POINT('Ctrl Pts',(-20.8509997094733,19.2098909057104,
-21.2890562790225));
#100698=CARTESIAN_POINT('Ctrl Pts',(-20.8509997571968,19.2099860824115,
-21.2873808744862));
#100699=CARTESIAN_POINT('Ctrl Pts',(-20.8509646300435,19.1366426709241,
-21.2832143337499));
#100700=CARTESIAN_POINT('Ctrl Pts',(-20.8471180797899,19.0633455484618,
-21.279152411229));
#100701=CARTESIAN_POINT('Ctrl Pts',(-20.8225239542534,18.828621677677,-21.2662357234474));
#100702=CARTESIAN_POINT('Ctrl Pts',(-20.7869893936289,18.6693653068234,
-21.2576412236419));
#100703=CARTESIAN_POINT('Ctrl Pts',(-20.729996333494,18.5054455806247,-21.2476752856251));
#100704=CARTESIAN_POINT('Ctrl Pts',(-20.7263281350187,18.4951529628947,
-21.2470444477784));
#100705=CARTESIAN_POINT('Ctrl Pts',(-20.7225806138391,18.4848897175613,
-21.2464098975766));
#100706=CARTESIAN_POINT('Origin',(-18.734,19.211,0.));
#100707=CARTESIAN_POINT('',(-20.7225807433525,18.4848900722565,-20.4442393203449));
#100708=CARTESIAN_POINT('',(-20.7225806137969,18.4848897174457,-20.6683679590049));
#100709=CARTESIAN_POINT('',(-20.7225806137986,18.4848897174502,0.));
#100710=CARTESIAN_POINT('Ctrl Pts',(-20.7225806137969,18.4848897174457,
-20.6683679590049));
#100711=CARTESIAN_POINT('Ctrl Pts',(-20.7238652346132,18.4884078773075,
-20.6685903986784));
#100712=CARTESIAN_POINT('Ctrl Pts',(-20.7251405258313,18.4919294648717,
-20.6688125292484));
#100713=CARTESIAN_POINT('Ctrl Pts',(-20.7310458686688,18.5083726433526,
-20.6698472828421));
#100714=CARTESIAN_POINT('Ctrl Pts',(-20.7355595959726,18.5213358782087,
-20.6706560544971));
#100715=CARTESIAN_POINT('Ctrl Pts',(-20.7688588121525,18.6200511751937,
-20.6767638173075));
#100716=CARTESIAN_POINT('Ctrl Pts',(-20.7922497953967,18.7075304791077,
-20.6818795084204));
#100717=CARTESIAN_POINT('Ctrl Pts',(-20.8373639114506,18.9333413712789,
-20.6946257510643));
#100718=CARTESIAN_POINT('Ctrl Pts',(-20.8511051845657,19.0728052824219,
-20.7020608117507));
#100719=CARTESIAN_POINT('Ctrl Pts',(-20.8509840406739,19.2328904078365,
-20.7109057277407));
#100720=CARTESIAN_POINT('Ctrl Pts',(-20.8506770362226,19.253177132247,-20.7120328020567));
#100721=CARTESIAN_POINT('Ctrl Pts',(-20.8483264321579,19.332818346702,-20.7164920697114));
#100722=CARTESIAN_POINT('Ctrl Pts',(-20.8440773388105,19.3920752179361,
-20.7198853164855));
#100723=CARTESIAN_POINT('Ctrl Pts',(-20.8363297205134,19.459955297946,-20.7239378705037));
#100724=CARTESIAN_POINT('Ctrl Pts',(-20.8352591881887,19.4688348537521,
-20.7244712782586));
#100725=CARTESIAN_POINT('Ctrl Pts',(-20.8335616373004,19.4822018792377,
-20.7252795633576));
#100726=CARTESIAN_POINT('Ctrl Pts',(-20.8329764095954,19.4866946847716,
-20.725552141968));
#100727=CARTESIAN_POINT('Ctrl Pts',(-20.8319046586591,19.4947212851328,
-20.7260407894413));
#100728=CARTESIAN_POINT('Ctrl Pts',(-20.8314236226012,19.4982557598237,
-20.7262565460338));
#100729=CARTESIAN_POINT('Ctrl Pts',(-20.8303644473523,19.5058936686,-20.7267240650099));
#100730=CARTESIAN_POINT('Ctrl Pts',(-20.8297832003999,19.5099965687839,
-20.7269759956357));
#100731=CARTESIAN_POINT('Ctrl Pts',(-20.8281309514489,19.5214178873796,
-20.7276794520146));
#100732=CARTESIAN_POINT('Ctrl Pts',(-20.8270336482833,19.5287323560194,
-20.7281324246829));
#100733=CARTESIAN_POINT('Ctrl Pts',(-20.8205389580125,19.5705308933003,
-20.7307344515959));
#100734=CARTESIAN_POINT('Ctrl Pts',(-20.81432804568,19.6048809225384,-20.732925408145));
#100735=CARTESIAN_POINT('Ctrl Pts',(-20.7918958094138,19.713529682705,-20.739990378814));
#100736=CARTESIAN_POINT('Ctrl Pts',(-20.7725200156514,19.7871126711618,
-20.744976017493));
#100737=CARTESIAN_POINT('Ctrl Pts',(-20.6904215892157,20.0422401707648,
-20.7626582236558));
#100738=CARTESIAN_POINT('Ctrl Pts',(-20.6070117016007,20.2161882405814,
-20.7753361389334));
#100739=CARTESIAN_POINT('Ctrl Pts',(-20.4894886988923,20.3943877308854,
-20.7884543995998));
#100740=CARTESIAN_POINT('Ctrl Pts',(-20.477434543749,20.4120758252533,-20.7897596208203));
#100741=CARTESIAN_POINT('Ctrl Pts',(-20.4603099695348,20.4364030108672,
-20.7915596757558));
#100742=CARTESIAN_POINT('Ctrl Pts',(-20.4554657132109,20.4431990307239,
-20.792063084789));
#100743=CARTESIAN_POINT('Ctrl Pts',(-20.4470415409645,20.454870677359,-20.7929286584956));
#100744=CARTESIAN_POINT('Ctrl Pts',(-20.4434807113584,20.4597598975535,
-20.7932915529839));
#100745=CARTESIAN_POINT('Ctrl Pts',(-20.4360700412671,20.4698440656833,
-20.794040704147));
#100746=CARTESIAN_POINT('Ctrl Pts',(-20.4322172523278,20.4750367765269,
-20.7944268409867));
#100747=CARTESIAN_POINT('Ctrl Pts',(-20.4231497182478,20.4871415269331,
-20.7953278842125));
#100748=CARTESIAN_POINT('Ctrl Pts',(-20.417916214374,20.494039420199,-20.7958420496878));
#100749=CARTESIAN_POINT('Ctrl Pts',(-20.4008334149364,20.5162704190809,
-20.7975016064568));
#100750=CARTESIAN_POINT('Ctrl Pts',(-20.3888156628372,20.5314732708375,
-20.7986403352536));
#100751=CARTESIAN_POINT('Ctrl Pts',(-20.3265598481577,20.6080439164203,
-20.8043989788289));
#100752=CARTESIAN_POINT('Ctrl Pts',(-20.2731078844067,20.6667223149236,
-20.8088862894284));
#100753=CARTESIAN_POINT('Ctrl Pts',(-20.1000689128619,20.8364655915517,
-20.8223348306495));
#100754=CARTESIAN_POINT('Ctrl Pts',(-19.9708585941075,20.9368208953897,
-20.8309358542029));
#100755=CARTESIAN_POINT('Ctrl Pts',(-19.7791774678144,21.0530166252851,
-20.8434651113487));
#100756=CARTESIAN_POINT('Ctrl Pts',(-19.7255937341235,21.0824063123928,
-20.8469515638519));
#100757=CARTESIAN_POINT('Ctrl Pts',(-19.6626471178312,21.1134685529451,
-20.8511147275503));
#100758=CARTESIAN_POINT('Ctrl Pts',(-19.6544483063012,21.1174487858551,
-20.8516582659053));
#100759=CARTESIAN_POINT('Ctrl Pts',(-19.6421586496759,21.123317223867,-20.8524752965509));
#100760=CARTESIAN_POINT('Ctrl Pts',(-19.6380869386098,21.1252455705193,
-20.8527463620862));
#100761=CARTESIAN_POINT('Ctrl Pts',(-19.6307807916038,21.1286772234577,
-20.8532334758977));
#100762=CARTESIAN_POINT('Ctrl Pts',(-19.6275486861925,21.1301853653746,
-20.853449221096));
#100763=CARTESIAN_POINT('Ctrl Pts',(-19.6205325546384,21.133437616634,-20.8539181167342));
#100764=CARTESIAN_POINT('Ctrl Pts',(-19.6167472360457,21.1351787019003,
-20.8541714431054));
#100765=CARTESIAN_POINT('Ctrl Pts',(-19.6061409439359,21.1400192603131,
-20.8548821771415));
#100766=CARTESIAN_POINT('Ctrl Pts',(-19.5993086988774,21.1430936790285,
-20.8553410773669));
#100767=CARTESIAN_POINT('Ctrl Pts',(-19.5591797901109,21.1608956088416,
-20.8580420257431));
#100768=CARTESIAN_POINT('Ctrl Pts',(-19.525526096485,21.1747975052504,-20.8603296642863));
#100769=CARTESIAN_POINT('Ctrl Pts',(-19.4153876736243,21.2170033453429,
-20.8678506049317));
#100770=CARTESIAN_POINT('Ctrl Pts',(-19.3376246634642,21.2417570242178,
-20.8732107339635));
#100771=CARTESIAN_POINT('Ctrl Pts',(-19.0810913452032,21.3073779395742,
-20.8906948008783));
#100772=CARTESIAN_POINT('Ctrl Pts',(-18.8983629616855,21.3295571239798,
-20.9027594276025));
#100773=CARTESIAN_POINT('Ctrl Pts',(-18.692724428247,21.3277152135146,-20.9154088546417));
#100774=CARTESIAN_POINT('Ctrl Pts',(-18.6704140468334,21.3271625302196,
-20.9167705223312));
#100775=CARTESIAN_POINT('Ctrl Pts',(-18.6396296753637,21.325912616701,-20.9186352215502));
#100776=CARTESIAN_POINT('Ctrl Pts',(-18.6311455225524,21.3255169883947,
-20.9191476478689));
#100777=CARTESIAN_POINT('Ctrl Pts',(-18.6165837343287,21.3247501014288,
-20.9200246650255));
#100778=CARTESIAN_POINT('Ctrl Pts',(-18.6105049471499,21.3244036632551,
-20.920390029593));
#100779=CARTESIAN_POINT('Ctrl Pts',(-18.5979923812975,21.3236363853174,
-20.9211405933597));
#100780=CARTESIAN_POINT('Ctrl Pts',(-18.5915588554447,21.3232123687426,
-20.9215256888571));
#100781=CARTESIAN_POINT('Ctrl Pts',(-18.5766193347189,21.3221591772321,
-20.922418077333));
#100782=CARTESIAN_POINT('Ctrl Pts',(-18.5681149671147,21.3215079731021,
-20.9229246736432));
#100783=CARTESIAN_POINT('Ctrl Pts',(-18.5410182405817,21.3192683013282,
-20.9245344989172));
#100784=CARTESIAN_POINT('Ctrl Pts',(-18.5224425239929,21.3174853802474,
-20.9256316224427));
#100785=CARTESIAN_POINT('Ctrl Pts',(-18.3441712716333,21.2979926669864,
-20.9361045577907));
#100786=CARTESIAN_POINT('Ctrl Pts',(-18.186954372689,21.2624029531223,-20.9448518902129));
#100787=CARTESIAN_POINT('Ctrl Pts',(-17.908489805109,21.1650362875258,-20.9608716365759));
#100788=CARTESIAN_POINT('Ctrl Pts',(-17.7862406205074,21.1087531818223,
-20.9681341966779));
#100789=CARTESIAN_POINT('Ctrl Pts',(-17.6566075194641,21.0334050827816,
-20.9769255641358));
#100790=CARTESIAN_POINT('Ctrl Pts',(-17.6431400772507,21.0253757712625,
-20.9778530778051));
#100791=CARTESIAN_POINT('Ctrl Pts',(-17.6248244002669,21.0141783055513,
-20.9791357969203));
#100792=CARTESIAN_POINT('Ctrl Pts',(-17.6198977606776,21.0111385255583,
-20.9794829645817));
#100793=CARTESIAN_POINT('Ctrl Pts',(-17.6120881042092,21.0062755592598,
-20.9800367960227));
#100794=CARTESIAN_POINT('Ctrl Pts',(-17.6091968773176,21.0044655197175,
-20.9802425986771));
#100795=CARTESIAN_POINT('Ctrl Pts',(-17.6032369892519,21.0007142784723,
-20.9806684486323));
#100796=CARTESIAN_POINT('Ctrl Pts',(-17.600168955563,20.9987721742235,-20.9808885589073));
#100797=CARTESIAN_POINT('Ctrl Pts',(-17.5928703093444,20.9941256941398,
-20.9814142901131));
#100798=CARTESIAN_POINT('Ctrl Pts',(-17.5886443072106,20.9914141506399,
-20.9817203841157));
#100799=CARTESIAN_POINT('Ctrl Pts',(-17.57442015286,20.9822158591705,-20.9827562590519));
#100800=CARTESIAN_POINT('Ctrl Pts',(-17.5644673557949,20.9756598598023,
-20.983490451711));
#100801=CARTESIAN_POINT('Ctrl Pts',(-17.540688908616,20.9597072588907,-20.9852661645549));
#100802=CARTESIAN_POINT('Ctrl Pts',(-17.526918352114,20.950230374788,-20.9863123308712));
#100803=CARTESIAN_POINT('Ctrl Pts',(-17.4756938282233,20.9140763361337,
-20.9902669930896));
#100804=CARTESIAN_POINT('Ctrl Pts',(-17.439001926931,20.8863455983022,-20.993227799718));
#100805=CARTESIAN_POINT('Ctrl Pts',(-17.3454296110854,20.8107148103743,
-21.0010640329972));
#100806=CARTESIAN_POINT('Ctrl Pts',(-17.2901177494593,20.7609737723358,
-21.0059872623381));
#100807=CARTESIAN_POINT('Ctrl Pts',(-17.1277324302756,20.5986932500524,
-21.0211541477343));
#100808=CARTESIAN_POINT('Ctrl Pts',(-17.0303110719726,20.4771945623109,
-21.0312703118379));
#100809=CARTESIAN_POINT('Ctrl Pts',(-16.9342094177865,20.3259062394142,
-21.0423125676483));
#100810=CARTESIAN_POINT('Ctrl Pts',(-16.9217170001419,20.3054827384802,
-21.0437748245359));
#100811=CARTESIAN_POINT('Ctrl Pts',(-16.9046536700756,20.2764928750974,
-21.0458116546682));
#100812=CARTESIAN_POINT('Ctrl Pts',(-16.899791504457,20.2681008757307,-21.0463968010334));
#100813=CARTESIAN_POINT('Ctrl Pts',(-16.8920195799322,20.2544716192993,
-21.0473399979026));
#100814=CARTESIAN_POINT('Ctrl Pts',(-16.8890741224234,20.2492549761941,
-21.0476993358021));
#100815=CARTESIAN_POINT('Ctrl Pts',(-16.8829818648259,20.2383573078666,
-21.0484465497037));
#100816=CARTESIAN_POINT('Ctrl Pts',(-16.8798389788568,20.2326741573979,
-21.0488342821771));
#100817=CARTESIAN_POINT('Ctrl Pts',(-16.8724721085011,20.2192069924331,
-21.0497485508298));
#100818=CARTESIAN_POINT('Ctrl Pts',(-16.8682706978415,20.2114107182159,
-21.0502742766826));
#100819=CARTESIAN_POINT('Ctrl Pts',(-16.8544955238803,20.1854604344387,
-21.0520126238802));
#100820=CARTESIAN_POINT('Ctrl Pts',(-16.8451366468869,20.1671932289247,
-21.0532176403368));
#100821=CARTESIAN_POINT('Ctrl Pts',(-16.7969196933668,20.06960912344,-21.0595612073592));
#100822=CARTESIAN_POINT('Ctrl Pts',(-16.762785859985,19.9880502692792,-21.0645332885322));
#100823=CARTESIAN_POINT('Ctrl Pts',(-16.6909611660007,19.7809240624421,
-21.076633940842));
#100824=CARTESIAN_POINT('Ctrl Pts',(-16.6596407171892,19.6535530519481,
-21.0836113184103));
#100825=CARTESIAN_POINT('Ctrl Pts',(-16.6347043027225,19.4868063465345,
-21.0929114939677));
#100826=CARTESIAN_POINT('Ctrl Pts',(-16.6301239880343,19.4493632957288,
-21.0950118496028));
#100827=CARTESIAN_POINT('Ctrl Pts',(-16.6221952111272,19.3661565949755,
-21.0997432653302));
#100828=CARTESIAN_POINT('Ctrl Pts',(-16.6193295724543,19.3203679203164,
-21.102389568849));
#100829=CARTESIAN_POINT('Ctrl Pts',(-16.6177244757135,19.2669024109276,
-21.1055661136472));
#100830=CARTESIAN_POINT('Ctrl Pts',(-16.6175368076586,19.2592775904332,
-21.1060211791667));
#100831=CARTESIAN_POINT('Ctrl Pts',(-16.6173018816819,19.2470458197098,
-21.1067547253886));
#100832=CARTESIAN_POINT('Ctrl Pts',(-16.6172284509348,19.2424393600136,
-21.1070317798662));
#100833=CARTESIAN_POINT('Ctrl Pts',(-16.6171246650432,19.234251712285,-21.1075257080918));
#100834=CARTESIAN_POINT('Ctrl Pts',(-16.6170883600617,19.2306706475776,
-21.1077422458778));
#100835=CARTESIAN_POINT('Ctrl Pts',(-16.6170304170128,19.2230469031411,
-21.1082043308926));
#100836=CARTESIAN_POINT('Ctrl Pts',(-16.6170112722208,19.2190043107715,
-21.1084500090353));
#100837=CARTESIAN_POINT('Ctrl Pts',(-16.6169907239663,19.2080241066514,
-21.1091190261681));
#100838=CARTESIAN_POINT('Ctrl Pts',(-16.6170118442319,19.2010865741262,
-21.1095435945458));
#100839=CARTESIAN_POINT('Ctrl Pts',(-16.6172932400599,19.1657349853193,
-21.1117161605605));
#100840=CARTESIAN_POINT('Ctrl Pts',(-16.618091467561,19.1373296005919,-21.1134917535019));
#100841=CARTESIAN_POINT('Ctrl Pts',(-16.6221164440865,19.0539291421224,
-21.1187764209565));
#100842=CARTESIAN_POINT('Ctrl Pts',(-16.6269181780206,18.9990359186557,
-21.1223457032781));
#100843=CARTESIAN_POINT('Ctrl Pts',(-16.6514754102595,18.8055884773547,
-21.1351165688919));
#100844=CARTESIAN_POINT('Ctrl Pts',(-16.6828169386274,18.6688559358138,
-21.1444680068812));
#100845=CARTESIAN_POINT('Ctrl Pts',(-16.7562388452252,18.4505243812992,
-21.1593417237258));
#100846=CARTESIAN_POINT('Ctrl Pts',(-16.7905178048905,18.3667588904991,
-21.1650403449655));
#100847=CARTESIAN_POINT('Ctrl Pts',(-16.8360573533758,18.273081400192,-21.1713958568454));
#100848=CARTESIAN_POINT('Ctrl Pts',(-16.8421815755244,18.2607891536605,
-21.1722296015031));
#100849=CARTESIAN_POINT('Ctrl Pts',(-16.8521958699974,18.2411695968639,
-21.1735601876361));
#100850=CARTESIAN_POINT('Ctrl Pts',(-16.8560100733402,18.2338041992708,
-21.1740596714804));
#100851=CARTESIAN_POINT('Ctrl Pts',(-16.8628598094688,18.2207652873705,
-21.1749439080675));
#100852=CARTESIAN_POINT('Ctrl Pts',(-16.8658780886411,18.2150828727072,
-21.1753292636354));
#100853=CARTESIAN_POINT('Ctrl Pts',(-16.8722213227627,18.2032709785249,
-21.1761303343288));
#100854=CARTESIAN_POINT('Ctrl Pts',(-16.8755507543537,18.1971439811875,
-21.1765458845793));
#100855=CARTESIAN_POINT('Ctrl Pts',(-16.8842770147452,18.1812728771118,
-21.1776224368516));
#100856=CARTESIAN_POINT('Ctrl Pts',(-16.8897206261015,18.1715546344465,
-21.1782817610144));
#100857=CARTESIAN_POINT('Ctrl Pts',(-16.9137061157043,18.1295160435795,
-21.1811349016419));
#100858=CARTESIAN_POINT('Ctrl Pts',(-16.9330234362541,18.0976442438993,
-21.1833006497502));
#100859=CARTESIAN_POINT('Ctrl Pts',(-16.9865976085496,18.0142982800807,
-21.1889869011616));
#100860=CARTESIAN_POINT('Ctrl Pts',(-17.0222853097246,17.9637855831186,
-21.1924562585561));
#100861=CARTESIAN_POINT('Ctrl Pts',(-17.1467844133524,17.8029990871616,
-21.2037070626936));
#100862=CARTESIAN_POINT('Ctrl Pts',(-17.244432781696,17.7000707935218,-21.2112299041505));
#100863=CARTESIAN_POINT('Ctrl Pts',(-17.4090248353282,17.5581614134058,
-21.2232601561996));
#100864=CARTESIAN_POINT('Ctrl Pts',(-17.4690435227198,17.5117892711482,
-21.2275427149157));
#100865=CARTESIAN_POINT('Ctrl Pts',(-17.539237091923,17.4633384159903,-21.2325974879184));
#100866=CARTESIAN_POINT('Ctrl Pts',(-17.5470988982186,17.4579896789482,
-21.2331642649796));
#100867=CARTESIAN_POINT('Ctrl Pts',(-17.5588060741698,17.4501396202669,
-21.234009622133));
#100868=CARTESIAN_POINT('Ctrl Pts',(-17.5626240952516,17.4475974568778,
-21.2342855277687));
#100869=CARTESIAN_POINT('Ctrl Pts',(-17.5694372858565,17.4430929020754,
-21.2347783105935));
#100870=CARTESIAN_POINT('Ctrl Pts',(-17.5724291996125,17.4411256831499,
-21.2349948599685));
#100871=CARTESIAN_POINT('Ctrl Pts',(-17.5788817139648,17.43690648726,-21.2354622172894));
#100872=CARTESIAN_POINT('Ctrl Pts',(-17.582343871688,17.4346570691078,-21.2357131842254));
#100873=CARTESIAN_POINT('Ctrl Pts',(-17.5919271525371,17.4284704543625,
-21.236408370159));
#100874=CARTESIAN_POINT('Ctrl Pts',(-17.5980619658802,17.4245547170155,
-21.236853968528));
#100875=CARTESIAN_POINT('Ctrl Pts',(-17.6319353181023,17.4031790140468,
-21.2393169275164));
#100876=CARTESIAN_POINT('Ctrl Pts',(-17.6600546605555,17.3863344374671,
-21.2413709740104));
#100877=CARTESIAN_POINT('Ctrl Pts',(-17.8308695867514,17.2893258792621,
-21.2538531240551));
#100878=CARTESIAN_POINT('Ctrl Pts',(-17.9820760932208,17.2252792955987,
-21.2648705847584));
#100879=CARTESIAN_POINT('Ctrl Pts',(-18.2489491721557,17.1471434353869,
-21.2830112442204));
#100880=CARTESIAN_POINT('Ctrl Pts',(-18.361186433397,17.1239457147987,-21.2902910156378));
#100881=CARTESIAN_POINT('Ctrl Pts',(-18.488924710063,17.1081850669349,-21.2981493541542));
#100882=CARTESIAN_POINT('Ctrl Pts',(-18.5031016629,17.1065811933026,-21.2990159238424));
#100883=CARTESIAN_POINT('Ctrl Pts',(-18.5257080644195,17.1042548765083,
-21.3003890824671));
#100884=CARTESIAN_POINT('Ctrl Pts',(-18.5341273126123,17.1034394533356,
-21.3008985760084));
#100885=CARTESIAN_POINT('Ctrl Pts',(-18.5489948411865,17.1020893919952,
-21.3017949870334));
#100886=CARTESIAN_POINT('Ctrl Pts',(-18.5554410671652,17.1015338186437,
-21.3021825566988));
#100887=CARTESIAN_POINT('Ctrl Pts',(-18.5687893026233,17.1004450148337,
-21.3029828742049));
#100888=CARTESIAN_POINT('Ctrl Pts',(-18.575691591258,17.0999160676548,-21.3033954832756));
#100889=CARTESIAN_POINT('Ctrl Pts',(-18.5934369133651,17.0986436997339,
-21.3044531783063));
#100890=CARTESIAN_POINT('Ctrl Pts',(-18.6042833867069,17.0979498994373,
-21.3050967049058));
#100891=CARTESIAN_POINT('Ctrl Pts',(-18.6497613108504,17.0953923745097,
-21.3077829610856));
#100892=CARTESIAN_POINT('Ctrl Pts',(-18.6844317031404,17.0942962020218,
-21.3098016555644));
#100893=CARTESIAN_POINT('Ctrl Pts',(-18.7749971765672,17.0936594007023,
-21.3150108109381));
#100894=CARTESIAN_POINT('Ctrl Pts',(-18.830875632806,17.0954793165037,-21.3181606736556));
#100895=CARTESIAN_POINT('Ctrl Pts',(-19.0845512127364,17.1138151352687,
-21.3322947409199));
#100896=CARTESIAN_POINT('Ctrl Pts',(-19.2794566076175,17.1558775631409,
-21.3426052583601));
#100897=CARTESIAN_POINT('Ctrl Pts',(-19.4955730150691,17.2354712891762,
-21.3558294172691));
#100898=CARTESIAN_POINT('Ctrl Pts',(-19.5252603478741,17.2471736430862,
-21.3576899717256));
#100899=CARTESIAN_POINT('Ctrl Pts',(-19.5609553935453,17.2621849063027,
-21.3599938957978));
#100900=CARTESIAN_POINT('Ctrl Pts',(-19.5672278349472,17.264858467493,-21.3604012884993));
#100901=CARTESIAN_POINT('Ctrl Pts',(-19.5775390666039,17.2693125059558,
-21.3610753655013));
#100902=CARTESIAN_POINT('Ctrl Pts',(-19.5815854528846,17.2710754188214,
-21.3613410032996));
#100903=CARTESIAN_POINT('Ctrl Pts',(-19.588876396886,17.2742790730214,-21.3618217028382));
#100904=CARTESIAN_POINT('Ctrl Pts',(-19.5921228733818,17.275715334382,-21.3620364884069));
#100905=CARTESIAN_POINT('Ctrl Pts',(-19.5984344687416,17.2785266277539,
-21.3624555260017));
#100906=CARTESIAN_POINT('Ctrl Pts',(-19.6014998841126,17.2799007700566,
-21.3626597155257));
#100907=CARTESIAN_POINT('Ctrl Pts',(-19.6105435276379,17.283980668308,-21.363264075301));
#100908=CARTESIAN_POINT('Ctrl Pts',(-19.616512394334,17.2867069007629,-21.3636654869535));
#100909=CARTESIAN_POINT('Ctrl Pts',(-19.6448684015059,17.2998179610146,
-21.3655841816581));
#100910=CARTESIAN_POINT('Ctrl Pts',(-19.667084469502,17.3105655023873,-21.3671223254333));
#100911=CARTESIAN_POINT('Ctrl Pts',(-19.7292832157982,17.3420090902268,
-21.3715175443288));
#100912=CARTESIAN_POINT('Ctrl Pts',(-19.7687994160794,17.3635949699764,
-21.3744153798857));
#100913=CARTESIAN_POINT('Ctrl Pts',(-19.8895235802651,17.4346299534854,
-21.3835371507064));
#100914=CARTESIAN_POINT('Ctrl Pts',(-19.9681106256475,17.4882998853338,
-21.3898622740666));
#100915=CARTESIAN_POINT('Ctrl Pts',(-20.1606339789982,17.6397358276908,
-21.4060184879364));
#100916=CARTESIAN_POINT('Ctrl Pts',(-20.2682893331312,17.7446685562577,
-21.4156928918988));
#100917=CARTESIAN_POINT('Ctrl Pts',(-20.3729857877411,17.8709946863554,
-21.425708948531));
#100918=CARTESIAN_POINT('Ctrl Pts',(-20.3818932538555,17.8819640741452,
-21.4265670672809));
#100919=CARTESIAN_POINT('Ctrl Pts',(-20.3959064983343,17.8995786384601,
-21.4279268969339));
#100920=CARTESIAN_POINT('Ctrl Pts',(-20.4010836841691,17.9061662213677,
-21.4284314840876));
#100921=CARTESIAN_POINT('Ctrl Pts',(-20.4101516090927,17.9178465471727,
-21.4293192505649));
#100922=CARTESIAN_POINT('Ctrl Pts',(-20.4140585606511,17.9229265147453,
-21.4297030757404));
#100923=CARTESIAN_POINT('Ctrl Pts',(-20.4220973657185,17.9334776761386,
-21.4304956227197));
#100924=CARTESIAN_POINT('Ctrl Pts',(-20.4262258339122,17.9389513637989,
-21.4309042074721));
#100925=CARTESIAN_POINT('Ctrl Pts',(-20.4367661202862,17.9530682243811,
-21.4319514493149));
#100926=CARTESIAN_POINT('Ctrl Pts',(-20.4431388058203,17.9617404747377,
-21.4325885652028));
#100927=CARTESIAN_POINT('Ctrl Pts',(-20.4695468605432,17.9982581275464,
-21.435245908051));
#100928=CARTESIAN_POINT('Ctrl Pts',(-20.488970717365,18.0265407422626,-21.4372424412269));
#100929=CARTESIAN_POINT('Ctrl Pts',(-20.5378440241057,18.1015475541661,
-21.4423912149845));
#100930=CARTESIAN_POINT('Ctrl Pts',(-20.5661683690365,18.1489747118992,
-21.445503583397));
#100931=CARTESIAN_POINT('Ctrl Pts',(-20.6274493266389,18.2613501573442,
-21.4526165474944));
#100932=CARTESIAN_POINT('Ctrl Pts',(-20.658974556634,18.3269984218444,-21.4565793224947));
#100933=CARTESIAN_POINT('Ctrl Pts',(-20.6995931154224,18.4241148417424,
-21.4622948401121));
#100934=CARTESIAN_POINT('Ctrl Pts',(-20.711437453539,18.4543722148084,-21.4640561340388));
#100935=CARTESIAN_POINT('Ctrl Pts',(-20.7225806137704,18.4848897173731,
-21.4658225507677));
#100936=CARTESIAN_POINT('Ctrl Pts',(-20.7225806138391,18.4848897175613,
-21.2464098975766));
#100937=CARTESIAN_POINT('Ctrl Pts',(-20.7152359994648,18.4647752003672,
-21.2451662684389));
#100938=CARTESIAN_POINT('Ctrl Pts',(-20.707586702596,18.4447735039477,-21.2439083812047));
#100939=CARTESIAN_POINT('Ctrl Pts',(-20.6969531989406,18.4181848178665,
-21.2422033325788));
#100940=CARTESIAN_POINT('Ctrl Pts',(-20.6942367444667,18.4114919784822,
-21.2417713244391));
#100941=CARTESIAN_POINT('Ctrl Pts',(-20.6899234875745,18.4010190441321,
-21.2410906959478));
#100942=CARTESIAN_POINT('Ctrl Pts',(-20.6883498252307,18.3972293946838,
-21.2408434557225));
#100943=CARTESIAN_POINT('Ctrl Pts',(-20.6853860462295,18.3901502868224,
-21.2403797795697));
#100944=CARTESIAN_POINT('Ctrl Pts',(-20.6839986202765,18.3868597611576,
-21.2401635072466));
#100945=CARTESIAN_POINT('Ctrl Pts',(-20.6808109679336,18.3793527945521,
-21.2396684128177));
#100946=CARTESIAN_POINT('Ctrl Pts',(-20.6790053702831,18.3751386910184,
-21.239389266955));
#100947=CARTESIAN_POINT('Ctrl Pts',(-20.6734104194994,18.3621968676265,
-21.2385283072623));
#100948=CARTESIAN_POINT('Ctrl Pts',(-20.6695759641248,18.3534889434377,
-21.2379438451609));
#100949=CARTESIAN_POINT('Ctrl Pts',(-20.6165875202679,18.2353202223973,
-21.2299450063012));
#100950=CARTESIAN_POINT('Ctrl Pts',(-20.5582778615877,18.1302176834212,
-21.2220507285775));
#100951=CARTESIAN_POINT('Ctrl Pts',(-20.4306977127279,17.9402699446208,
-21.2069341869007));
#100952=CARTESIAN_POINT('Ctrl Pts',(-20.3631210364827,17.8547160587159,
-21.1997397457768));
#100953=CARTESIAN_POINT('Ctrl Pts',(-20.252301798355,17.7347154429134,-21.1892458908812));
#100954=CARTESIAN_POINT('Ctrl Pts',(-20.2138109877699,17.6961347651446,
-21.1857978963002));
#100955=CARTESIAN_POINT('Ctrl Pts',(-20.1573001305014,17.6437039968266,
-21.1810074796356));
#100956=CARTESIAN_POINT('Ctrl Pts',(-20.1404826770932,17.6285946904318,
-21.1796136224393));
#100957=CARTESIAN_POINT('Ctrl Pts',(-20.1143229067879,17.6058385619071,
-21.1774930207077));
#100958=CARTESIAN_POINT('Ctrl Pts',(-20.1051522240041,17.5979977813365,
-21.1767583171528));
#100959=CARTESIAN_POINT('Ctrl Pts',(-20.0880167126455,17.5835989526179,
-21.1754013999514));
#100960=CARTESIAN_POINT('Ctrl Pts',(-20.0800700521631,17.5770199365629,
-21.1747783384348));
#100961=CARTESIAN_POINT('Ctrl Pts',(-20.06690184825,17.5662792829195,-21.1737559504324));
#100962=CARTESIAN_POINT('Ctrl Pts',(-20.0617082118684,17.56208384689,-21.1733552581288));
#100963=CARTESIAN_POINT('Ctrl Pts',(-20.0514511068144,17.5538780066179,
-21.1725688653188));
#100964=CARTESIAN_POINT('Ctrl Pts',(-20.0463889625842,17.5498660703872,
-21.1721831057767));
#100965=CARTESIAN_POINT('Ctrl Pts',(-20.0346569859217,17.5406551497722,
-21.1712944239702));
#100966=CARTESIAN_POINT('Ctrl Pts',(-20.0279741760687,17.5354728147413,
-21.1707921675384));
#100967=CARTESIAN_POINT('Ctrl Pts',(-20.0099151881518,17.5216410519944,
-21.169445380337));
#100968=CARTESIAN_POINT('Ctrl Pts',(-19.9984820620083,17.5130664464331,
-21.168603789409));
#100969=CARTESIAN_POINT('Ctrl Pts',(-19.8931905239911,17.4357533870795,
-21.1609510811334));
#100970=CARTESIAN_POINT('Ctrl Pts',(-19.7938966826245,17.3747409118555,
-21.1544535643496));
#100971=CARTESIAN_POINT('Ctrl Pts',(-19.5451166395735,17.2488130918211,
-21.1391851304526));
#100972=CARTESIAN_POINT('Ctrl Pts',(-19.3922058557569,17.1923764489089,
-21.1305981481223));
#100973=CARTESIAN_POINT('Ctrl Pts',(-19.2022751842734,17.1461759830774,
-21.1193807164723));
#100974=CARTESIAN_POINT('Ctrl Pts',(-19.170006384746,17.1391221009559,-21.1174551044213));
#100975=CARTESIAN_POINT('Ctrl Pts',(-19.1304434962872,17.1314388632321,
-21.1150556719566));
#100976=CARTESIAN_POINT('Ctrl Pts',(-19.1232921207835,17.1300882746966,
-21.1146204235108));
#100977=CARTESIAN_POINT('Ctrl Pts',(-19.1120820261218,17.1280309763835,
-21.1139355616461));
#100978=CARTESIAN_POINT('Ctrl Pts',(-19.1080278880933,17.1272991793239,
-21.113687351279));
#100979=CARTESIAN_POINT('Ctrl Pts',(-19.1004544984534,17.1259549499233,
-21.1132226466908));
#100980=CARTESIAN_POINT('Ctrl Pts',(-19.0969358244336,17.1253395897244,
-21.1130063210192));
#100981=CARTESIAN_POINT('Ctrl Pts',(-19.0889105109887,17.1239570134916,
-21.1125119826549));
#100982=CARTESIAN_POINT('Ctrl Pts',(-19.0844029522625,17.1231954908363,
-21.1122336521205));
#100983=CARTESIAN_POINT('Ctrl Pts',(-19.0726563214473,17.1212500862499,
-21.111506628694));
#100984=CARTESIAN_POINT('Ctrl Pts',(-19.0654135712445,17.120089230196,-21.1110566820063));
#100985=CARTESIAN_POINT('Ctrl Pts',(-19.0185462950184,17.1128270472442,
-21.108134916606));
#100986=CARTESIAN_POINT('Ctrl Pts',(-18.9787639863779,17.1078151658732,
-21.1056078731911));
#100987=CARTESIAN_POINT('Ctrl Pts',(-18.9293667005263,17.1030123453667,
-21.10243141649));
#100988=CARTESIAN_POINT('Ctrl Pts',(-18.9198608688469,17.1021529614027,
-21.101818379856));
#100989=CARTESIAN_POINT('Ctrl Pts',(-18.9031213067476,17.1007536641103,
-21.1007360681414));
#100990=CARTESIAN_POINT('Ctrl Pts',(-18.8958899391321,17.100186588023,-21.1002676096077));
#100991=CARTESIAN_POINT('Ctrl Pts',(-18.7362362311158,17.0884919561016,
-21.0899068464011));
#100992=CARTESIAN_POINT('Ctrl Pts',(-18.5830546826722,17.0938640484914,
-21.0796431322706));
#100993=CARTESIAN_POINT('Ctrl Pts',(-18.3399085143707,17.1289344740535,
-21.0636989433115));
#100994=CARTESIAN_POINT('Ctrl Pts',(-18.248999002911,17.1482147657485,-21.0578086437992));
#100995=CARTESIAN_POINT('Ctrl Pts',(-18.1393450836464,17.1791242524669,
-21.0508127870644));
#100996=CARTESIAN_POINT('Ctrl Pts',(-18.1191382116848,17.1851474499124,
-21.0495279174345));
#100997=CARTESIAN_POINT('Ctrl Pts',(-18.0904788198603,17.1941584763851,
-21.0477111912655));
#100998=CARTESIAN_POINT('Ctrl Pts',(-18.0819505774123,17.1968995072183,
-21.0471712941368));
#100999=CARTESIAN_POINT('Ctrl Pts',(-18.0672481701988,17.2017281244331,
-21.0462416846104));
#101000=CARTESIAN_POINT('Ctrl Pts',(-18.0610658247117,17.2037902277812,
-21.0458511393867));
#101001=CARTESIAN_POINT('Ctrl Pts',(-18.0492329237,17.2077978726255,-21.0451042869256));
#101002=CARTESIAN_POINT('Ctrl Pts',(-18.0435808997982,17.2097388528464,
-21.0447478333971));
#101003=CARTESIAN_POINT('Ctrl Pts',(-18.0288749934262,17.2148587721622,
-21.0438210793781));
#101004=CARTESIAN_POINT('Ctrl Pts',(-18.0198343062371,17.2180754046305,
-21.0432520333695));
#101005=CARTESIAN_POINT('Ctrl Pts',(-17.9889266955431,17.229309510024,-21.0413087397583));
#101006=CARTESIAN_POINT('Ctrl Pts',(-17.9671698833289,17.2376264766844,
-21.0399444668155));
#101007=CARTESIAN_POINT('Ctrl Pts',(-17.7867453367255,17.3100319687421,
-21.0286508791931));
#101008=CARTESIAN_POINT('Ctrl Pts',(-17.6362495753156,17.392780616265,-21.0194297122358));
#101009=CARTESIAN_POINT('Ctrl Pts',(-17.4241895045278,17.5454041718357,
-21.0052229945768));
#101010=CARTESIAN_POINT('Ctrl Pts',(-17.3544763511468,17.6026701463593,
-21.0002984137781));
#101011=CARTESIAN_POINT('Ctrl Pts',(-17.2604233414268,17.6905556007389,
-20.9929548669999));
#101012=CARTESIAN_POINT('Ctrl Pts',(-17.2329445862863,17.7176776763696,
-20.990713732154));
#101013=CARTESIAN_POINT('Ctrl Pts',(-17.2009529130676,17.7510295810089,
-20.9879643250547));
#101014=CARTESIAN_POINT('Ctrl Pts',(-17.1957109990217,17.7565537340423,
-20.9875091393365));
#101015=CARTESIAN_POINT('Ctrl Pts',(-17.1876303376171,17.7651620296073,
-20.9867999110871));
#101016=CARTESIAN_POINT('Ctrl Pts',(-17.1847706914004,17.7682265881143,
-20.9865474425624));
#101017=CARTESIAN_POINT('Ctrl Pts',(-17.1794973579274,17.7739115447412,
-20.9860790832809));
#101018=CARTESIAN_POINT('Ctrl Pts',(-17.1770811768264,17.776529550696,-20.985863387877));
#101019=CARTESIAN_POINT('Ctrl Pts',(-17.171650206002,17.7824440588812,-20.9853760793965));
#101020=CARTESIAN_POINT('Ctrl Pts',(-17.168639253863,17.7857439916569,-20.9851041836218));
#101021=CARTESIAN_POINT('Ctrl Pts',(-17.1598305600817,17.7954596965133,
-20.9843037090298));
#101022=CARTESIAN_POINT('Ctrl Pts',(-17.1540617387684,17.8019014011743,
-20.9837730352611));
#101023=CARTESIAN_POINT('Ctrl Pts',(-17.1140886154277,17.847091111986,-20.9800517939001));
#101024=CARTESIAN_POINT('Ctrl Pts',(-17.0812767165212,17.8870418646467,
-20.9767700694316));
#101025=CARTESIAN_POINT('Ctrl Pts',(-17.0366049255505,17.9456838931232,
-20.9720108784507));
#101026=CARTESIAN_POINT('Ctrl Pts',(-17.0235224619813,17.9634257801954,
-20.9705781363113));
#101027=CARTESIAN_POINT('Ctrl Pts',(-16.9840416998996,18.0187565066996,
-20.9661386995925));
#101028=CARTESIAN_POINT('Ctrl Pts',(-16.9585880704776,18.0570022160794,
-20.9631104032372));
#101029=CARTESIAN_POINT('Ctrl Pts',(-16.8768044981679,18.1890055004216,
-20.952852536024));
#101030=CARTESIAN_POINT('Ctrl Pts',(-16.8264950267668,18.286296732229,-20.9456215479727));
#101031=CARTESIAN_POINT('Ctrl Pts',(-16.7624918150616,18.4377746827603,
-20.935051674093));
#101032=CARTESIAN_POINT('Ctrl Pts',(-16.743043719579,18.4893242944996,-20.9315643799399));
#101033=CARTESIAN_POINT('Ctrl Pts',(-16.7147841334681,18.5741075002619,
-20.9260094669004));
#101034=CARTESIAN_POINT('Ctrl Pts',(-16.7047328255545,18.6068975892386,
-20.9239034475204));
#101035=CARTESIAN_POINT('Ctrl Pts',(-16.692567015497,18.6503243895863,-20.9211678961681));
#101036=CARTESIAN_POINT('Ctrl Pts',(-16.6897316565199,18.6607521313475,
-20.9205150390416));
#101037=CARTESIAN_POINT('Ctrl Pts',(-16.6852176288022,18.677870219475,-20.9194497533633));
#101038=CARTESIAN_POINT('Ctrl Pts',(-16.6834916184812,18.6845477737855,
-20.9190357959774));
#101039=CARTESIAN_POINT('Ctrl Pts',(-16.6802131744755,18.697492107773,-20.9182363927813));
#101040=CARTESIAN_POINT('Ctrl Pts',(-16.6786567166939,18.7037577804726,
-20.9178508207361));
#101041=CARTESIAN_POINT('Ctrl Pts',(-16.6751283426088,18.7182445126901,
-20.916962478573));
#101042=CARTESIAN_POINT('Ctrl Pts',(-16.6731769522369,18.7264704953727,
-20.916460374614));
#101043=CARTESIAN_POINT('Ctrl Pts',(-16.6680598872477,18.7486314794224,
-20.9151138004726));
#101044=CARTESIAN_POINT('Ctrl Pts',(-16.6649859067855,18.7625873604674,
-20.9142722722917));
#101045=CARTESIAN_POINT('Ctrl Pts',(-16.6380608291297,18.8910033987868,
-20.9065856922688));
#101046=CARTESIAN_POINT('Ctrl Pts',(-16.6235871694191,19.0072310393739,
-20.9000578439795));
#101047=CARTESIAN_POINT('Ctrl Pts',(-16.6120973750738,19.2868148923392,
-20.8847399161451));
#101048=CARTESIAN_POINT('Ctrl Pts',(-16.6242137074027,19.4497645786932,
-20.8761331037338));
#101049=CARTESIAN_POINT('Ctrl Pts',(-16.6609680124453,19.6414320748346,
-20.8649250547471));
#101050=CARTESIAN_POINT('Ctrl Pts',(-16.6677798589054,19.6730253932406,
-20.8630398995738));
#101051=CARTESIAN_POINT('Ctrl Pts',(-16.676995934903,19.7114752634247,-20.8606856482955));
#101052=CARTESIAN_POINT('Ctrl Pts',(-16.6787161391372,19.7184933112644,
-20.8602534748482));
#101053=CARTESIAN_POINT('Ctrl Pts',(-16.6814701905088,19.729485528465,-20.8595725042855));
#101054=CARTESIAN_POINT('Ctrl Pts',(-16.6824797484422,19.7334658064096,
-20.8593250865489));
#101055=CARTESIAN_POINT('Ctrl Pts',(-16.6843891937364,19.7409031078772,
-20.8588611648892));
#101056=CARTESIAN_POINT('Ctrl Pts',(-16.6852862528948,19.7443607996941,
-20.8586448251508));
#101057=CARTESIAN_POINT('Ctrl Pts',(-16.6873549100026,19.7522521645731,
-20.8581495888958));
#101058=CARTESIAN_POINT('Ctrl Pts',(-16.6885321618239,19.7566842971341,
-20.857870368922));
#101059=CARTESIAN_POINT('Ctrl Pts',(-16.6921981460778,19.7703074816635,
-20.8570088909108));
#101060=CARTESIAN_POINT('Ctrl Pts',(-16.6947344562219,19.7794854473959,
-20.8564239797095));
#101061=CARTESIAN_POINT('Ctrl Pts',(-16.7185343451424,19.8633992576212,
-20.8510365618186));
#101062=CARTESIAN_POINT('Ctrl Pts',(-16.7438334688544,19.936920850802,-20.8460297370155));
#101063=CARTESIAN_POINT('Ctrl Pts',(-16.7885257179879,20.0467579655339,
-20.8382685750025));
#101064=CARTESIAN_POINT('Ctrl Pts',(-16.8050335551802,20.0841837645915,
-20.835571509564));
#101065=CARTESIAN_POINT('Ctrl Pts',(-16.8696061976661,20.2197976882591,
-20.8256494079995));
#101066=CARTESIAN_POINT('Ctrl Pts',(-16.9241744076404,20.3147082127857,
-20.8184221012403));
#101067=CARTESIAN_POINT('Ctrl Pts',(-17.0168586001139,20.4504114142015,
-20.8078599064588));
#101068=CARTESIAN_POINT('Ctrl Pts',(-17.0496456073477,20.4946145597812,
-20.804376610865));
#101069=CARTESIAN_POINT('Ctrl Pts',(-17.1055890392046,20.5641964861083,
-20.7988272183826));
#101070=CARTESIAN_POINT('Ctrl Pts',(-17.1277042687642,20.5903756655214,
-20.7967228268436));
#101071=CARTESIAN_POINT('Ctrl Pts',(-17.1576168855612,20.6240895262534,
-20.7939889661635));
#101072=CARTESIAN_POINT('Ctrl Pts',(-17.1648493283023,20.632116430481,-20.793336214705));
#101073=CARTESIAN_POINT('Ctrl Pts',(-17.1767991111987,20.6451764067874,
-20.7922710048987));
#101074=CARTESIAN_POINT('Ctrl Pts',(-17.1814800943103,20.6502423416708,
-20.7918570189909));
#101075=CARTESIAN_POINT('Ctrl Pts',(-17.1905913556545,20.6600067138341,
-20.7910574934934));
#101076=CARTESIAN_POINT('Ctrl Pts',(-17.1950185320719,20.6647079290479,
-20.7906718279997));
#101077=CARTESIAN_POINT('Ctrl Pts',(-17.2052936953164,20.6755195689603,
-20.7897831737492));
#101078=CARTESIAN_POINT('Ctrl Pts',(-17.211156953004,20.6816153784147,-20.789280851952));
#101079=CARTESIAN_POINT('Ctrl Pts',(-17.2270311388425,20.6979224365489,
-20.7879334761326));
#101080=CARTESIAN_POINT('Ctrl Pts',(-17.2371093648017,20.708067774687,-20.7870913683861));
#101081=CARTESIAN_POINT('Ctrl Pts',(-17.3310032720836,20.8006907364185,
-20.7793648727674));
#101082=CARTESIAN_POINT('Ctrl Pts',(-17.4214563952892,20.876157973595,-20.7728015699113));
#101083=CARTESIAN_POINT('Ctrl Pts',(-17.6516586437018,21.037747046402,-20.7574080994725));
#101084=CARTESIAN_POINT('Ctrl Pts',(-17.7960287030646,21.115905529318,-20.7487612801579));
#101085=CARTESIAN_POINT('Ctrl Pts',(-17.9767197820359,21.1881637888426,
-20.7375685778981));
#101086=CARTESIAN_POINT('Ctrl Pts',(-18.0057508617983,21.1990399746008,
-20.7357583833923));
#101087=CARTESIAN_POINT('Ctrl Pts',(-18.0417424942445,21.2116297611677,
-20.7334875428134));
#101088=CARTESIAN_POINT('Ctrl Pts',(-18.048488264599,21.2139512108072,-20.7330607897004));
#101089=CARTESIAN_POINT('Ctrl Pts',(-18.0591164770944,21.2175487613245,
-20.7323864470807));
#101090=CARTESIAN_POINT('Ctrl Pts',(-18.0629911723919,21.2188478163658,
-20.7321401922051));
#101091=CARTESIAN_POINT('Ctrl Pts',(-18.0702630954118,21.2212624473527,
-20.7316772137967));
#101092=CARTESIAN_POINT('Ctrl Pts',(-18.0736593962089,21.2223806382822,
-20.7314606469632));
#101093=CARTESIAN_POINT('Ctrl Pts',(-18.0814483292277,21.2249231964012,
-20.7309632227257));
#101094=CARTESIAN_POINT('Ctrl Pts',(-18.0858427868814,21.2263417948775,
-20.7306820311186));
#101095=CARTESIAN_POINT('Ctrl Pts',(-18.0994689231671,21.2306913445902,
-20.7298085049893));
#101096=CARTESIAN_POINT('Ctrl Pts',(-18.1087159491924,21.2335732774126,
-20.7292134107893));
#101097=CARTESIAN_POINT('Ctrl Pts',(-18.2199126560322,21.2673934772227,
-20.7220325508895));
#101098=CARTESIAN_POINT('Ctrl Pts',(-18.3240264479709,21.2906529106698,
-20.7150668263269));
#101099=CARTESIAN_POINT('Ctrl Pts',(-18.5377423054188,21.321722761019,-20.7008203925458));
#101100=CARTESIAN_POINT('Ctrl Pts',(-18.6471161595362,21.3290466606485,
-20.6935600582885));
#101101=CARTESIAN_POINT('Ctrl Pts',(-18.8191820635797,21.3272121252008,
-20.6824360458578));
#101102=CARTESIAN_POINT('Ctrl Pts',(-18.8817380677183,21.3237669956584,
-20.6784511134523));
#101103=CARTESIAN_POINT('Ctrl Pts',(-18.9688268937871,21.3150829634757,
-20.6729960955378));
#101104=CARTESIAN_POINT('Ctrl Pts',(-18.9935548418232,21.3121758977807,
-20.6714575322988));
#101105=CARTESIAN_POINT('Ctrl Pts',(-19.0367601328771,21.3063221945307,
-20.6687868757669));
#101106=CARTESIAN_POINT('Ctrl Pts',(-19.0552600187143,21.3035656100988,
-20.667649001354));
#101107=CARTESIAN_POINT('Ctrl Pts',(-19.082145839258,21.299194512327,-20.6660031598973));
#101108=CARTESIAN_POINT('Ctrl Pts',(-19.0905619898507,21.2977739210157,
-20.6654890767733));
#101109=CARTESIAN_POINT('Ctrl Pts',(-19.1053191349361,21.2951911270328,
-20.664589567943));
#101110=CARTESIAN_POINT('Ctrl Pts',(-19.1116637979455,21.2940507941765,
-20.6642034528007));
#101111=CARTESIAN_POINT('Ctrl Pts',(-19.1239855933328,21.2917780380252,
-20.6634547557497));
#101112=CARTESIAN_POINT('Ctrl Pts',(-19.1299632416492,21.2906487970295,
-20.6630920767236));
#101113=CARTESIAN_POINT('Ctrl Pts',(-19.1442608459029,21.2878839479357,
-20.662225845325));
#101114=CARTESIAN_POINT('Ctrl Pts',(-19.1525760472977,21.2862240820405,
-20.6617230701115));
#101115=CARTESIAN_POINT('Ctrl Pts',(-19.1826608302047,21.2800304297158,
-20.6599074744352));
#101116=CARTESIAN_POINT('Ctrl Pts',(-19.204369094039,21.27520358256,-20.6586040075469));
#101117=CARTESIAN_POINT('Ctrl Pts',(-19.4052504162273,21.2272038315851,
-20.646593406177));
#101118=CARTESIAN_POINT('Ctrl Pts',(-19.5781382614978,21.161151721059,-20.6367288607255));
#101119=CARTESIAN_POINT('Ctrl Pts',(-19.8115607126271,21.035037415791,-20.6222695482745));
#101120=CARTESIAN_POINT('Ctrl Pts',(-19.8805486379102,20.9924807747384,
-20.6178178032159));
#101121=CARTESIAN_POINT('Ctrl Pts',(-19.9766416479195,20.9253061314895,
-20.6111129213783));
#101122=CARTESIAN_POINT('Ctrl Pts',(-20.0058193888798,20.9037725378276,
-20.6090041897175));
#101123=CARTESIAN_POINT('Ctrl Pts',(-20.0403302052841,20.8769070639192,
-20.6064015535575));
#101124=CARTESIAN_POINT('Ctrl Pts',(-20.0462081228253,20.872281068771,-20.6059543652548));
#101125=CARTESIAN_POINT('Ctrl Pts',(-20.0553184316746,20.8650326256605,
-20.6052549397604));
#101126=CARTESIAN_POINT('Ctrl Pts',(-20.0585678799266,20.8624315775757,
-20.6050042074991));
#101127=CARTESIAN_POINT('Ctrl Pts',(-20.0645866185924,20.857584635999,-20.6045373987949));
#101128=CARTESIAN_POINT('Ctrl Pts',(-20.0673579134824,20.8553413231554,
-20.604321507035));
#101129=CARTESIAN_POINT('Ctrl Pts',(-20.0736189686333,20.8502468777262,
-20.6038315983027));
#101130=CARTESIAN_POINT('Ctrl Pts',(-20.0771052823971,20.8473916116828,
-20.6035572852201));
#101131=CARTESIAN_POINT('Ctrl Pts',(-20.0873944146572,20.8389098545557,
-20.6027432679808));
#101132=CARTESIAN_POINT('Ctrl Pts',(-20.0941710862548,20.8332519983257,
-20.6022013638953));
#101133=CARTESIAN_POINT('Ctrl Pts',(-20.143789056171,20.7912964047527,-20.5981921760178));
#101134=CARTESIAN_POINT('Ctrl Pts',(-20.1852027882272,20.7533524859523,
-20.5946174055716));
#101135=CARTESIAN_POINT('Ctrl Pts',(-20.2694056946639,20.6698082744742,
-20.5869377264677));
#101136=CARTESIAN_POINT('Ctrl Pts',(-20.3117845642145,20.6238649911955,
-20.5828224214743));
#101137=CARTESIAN_POINT('Ctrl Pts',(-20.4227518412588,20.4923359103383,
-20.5714554666818));
#101138=CARTESIAN_POINT('Ctrl Pts',(-20.4868272471835,20.4031847999859,
-20.5642058558508));
#101139=CARTESIAN_POINT('Ctrl Pts',(-20.5724488758391,20.2621240945041,
-20.5535968573673));
#101140=CARTESIAN_POINT('Ctrl Pts',(-20.5993182072117,20.2136689133617,
-20.5500892113808));
#101141=CARTESIAN_POINT('Ctrl Pts',(-20.6397608240933,20.1334695794462,
-20.5445056329858));
#101142=CARTESIAN_POINT('Ctrl Pts',(-20.6545119640231,20.1023520395552,
-20.542390810797));
#101143=CARTESIAN_POINT('Ctrl Pts',(-20.6728942756066,20.0609971313829,
-20.5396456255145));
#101144=CARTESIAN_POINT('Ctrl Pts',(-20.6772145010782,20.0510735354429,
-20.5389917354065));
#101145=CARTESIAN_POINT('Ctrl Pts',(-20.6841645607711,20.0347686637089,
-20.5379251655332));
#101146=CARTESIAN_POINT('Ctrl Pts',(-20.6868395890268,20.0284069773867,
-20.5375109503167));
#101147=CARTESIAN_POINT('Ctrl Pts',(-20.6919565565327,20.0160694343696,
-20.5367113258279));
#101148=CARTESIAN_POINT('Ctrl Pts',(-20.69440236109,20.010095273095,-20.5363257888581));
#101149=CARTESIAN_POINT('Ctrl Pts',(-20.6999852443612,19.9962785263683,
-20.535437921984));
#101150=CARTESIAN_POINT('Ctrl Pts',(-20.7031028023643,19.9884281329464,
-20.534936255541));
#101151=CARTESIAN_POINT('Ctrl Pts',(-20.7113578704912,19.9672726128737,
-20.533591727848));
#101152=CARTESIAN_POINT('Ctrl Pts',(-20.7164081045861,19.953933735049,-20.5327517937283));
#101153=CARTESIAN_POINT('Ctrl Pts',(-20.7714922868465,19.8038811168905,
-20.5233872789514));
#101154=CARTESIAN_POINT('Ctrl Pts',(-20.807433641414,19.6624018986933,-20.5153747723651));
#101155=CARTESIAN_POINT('Ctrl Pts',(-20.8435716232148,19.416112685353,-20.5018390757858));
#101156=CARTESIAN_POINT('Ctrl Pts',(-20.8510665768693,19.3129337983554,
-20.4962758775061));
#101157=CARTESIAN_POINT('Ctrl Pts',(-20.8509605930263,19.1495719709784,
-20.4871374802086));
#101158=CARTESIAN_POINT('Ctrl Pts',(-20.8483662200053,19.089551891809,-20.4837077513012));
#101159=CARTESIAN_POINT('Ctrl Pts',(-20.8424571664132,19.0207954149847,
-20.4796145097686));
#101160=CARTESIAN_POINT('Ctrl Pts',(-20.841632618508,19.0118665127582,-20.4790797464361));
#101161=CARTESIAN_POINT('Ctrl Pts',(-20.8403055954211,18.9984292733184,
-20.4782697850337));
#101162=CARTESIAN_POINT('Ctrl Pts',(-20.8398453013716,18.9939167418798,
-20.4779968993075));
#101163=CARTESIAN_POINT('Ctrl Pts',(-20.8389970519398,18.985857509629,-20.4775079023638));
#101164=CARTESIAN_POINT('Ctrl Pts',(-20.8386146300039,18.982310278849,-20.4772921050407));
#101165=CARTESIAN_POINT('Ctrl Pts',(-20.8377689780624,18.9746480716415,
-20.4768247302818));
#101166=CARTESIAN_POINT('Ctrl Pts',(-20.8373026477863,18.9705335403155,
-20.4765729858425));
#101167=CARTESIAN_POINT('Ctrl Pts',(-20.8359714187925,18.959088018593,-20.4758706109915));
#101168=CARTESIAN_POINT('Ctrl Pts',(-20.8350802526843,18.9517602270393,
-20.4754185410009));
#101169=CARTESIAN_POINT('Ctrl Pts',(-20.8297855227008,18.9100449594236,
-20.4728319942608));
#101170=CARTESIAN_POINT('Ctrl Pts',(-20.8245763661117,18.8757672010279,
-20.4706561904851));
#101171=CARTESIAN_POINT('Ctrl Pts',(-20.805407187068,18.7675849999349,-20.4636610960151));
#101172=CARTESIAN_POINT('Ctrl Pts',(-20.7883503387104,18.6942914438053,
-20.4587324781192));
#101173=CARTESIAN_POINT('Ctrl Pts',(-20.7540340414928,18.5758063603463,
-20.4505956795289));
#101174=CARTESIAN_POINT('Ctrl Pts',(-20.7390724281762,18.5300554743709,
-20.4474104160584));
#101175=CARTESIAN_POINT('Ctrl Pts',(-20.7225807433525,18.4848900722567,
-20.4442393203449));
#101176=CARTESIAN_POINT('Origin',(-18.734,19.211,0.));
#101177=CARTESIAN_POINT('',(-20.7225806138715,18.48488971765,-19.6425236773711));
#101178=CARTESIAN_POINT('',(-20.7227695130846,18.4848207703082,-19.8664843328284));
#101179=CARTESIAN_POINT('',(-20.7225806137986,18.4848897174502,0.));
#101180=CARTESIAN_POINT('',(-20.8479202214574,19.2118282579775,-19.9109991817851));
#101181=CARTESIAN_POINT('Ctrl Pts',(-20.7227695130846,18.4848207703082,
-19.8664843328284));
#101182=CARTESIAN_POINT('Ctrl Pts',(-20.804884879996,18.7170154428126,-19.8813041288781));
#101183=CARTESIAN_POINT('Ctrl Pts',(-20.8469525585721,18.9645595409249,
-19.8961239249278));
#101184=CARTESIAN_POINT('Ctrl Pts',(-20.8478239854299,19.2118314138294,
-19.9109437209775));
#101185=CARTESIAN_POINT('Ctrl Pts',(-20.8509998750784,19.2117272674116,
-19.9127739856851));
#101186=CARTESIAN_POINT('Ctrl Pts',(-20.8509329967896,19.4064030179171,
-19.9239833448391));
#101187=CARTESIAN_POINT('Ctrl Pts',(-20.8240164289188,19.6001371512442,
-19.9342646615468));
#101188=CARTESIAN_POINT('Ctrl Pts',(-20.7539266223477,19.8478012358022,
-19.9484105777364));
#101189=CARTESIAN_POINT('Ctrl Pts',(-20.7341848393677,19.9073324161759,
-19.9519023179064));
#101190=CARTESIAN_POINT('Ctrl Pts',(-20.7008063068113,19.9947844856038,
-19.9572865274355));
#101191=CARTESIAN_POINT('Ctrl Pts',(-20.6891489403589,20.0234269582284,
-19.9590922948951));
#101192=CARTESIAN_POINT('Ctrl Pts',(-20.6740381883075,20.0583438718382,
-19.9613581802236));
#101193=CARTESIAN_POINT('Ctrl Pts',(-20.6711741838903,20.064871177176,-19.9617845754105));
#101194=CARTESIAN_POINT('Ctrl Pts',(-20.6666170558022,20.0751163138349,
-19.9624584640114));
#101195=CARTESIAN_POINT('Ctrl Pts',(-20.6649460109109,20.0788439897307,
-19.9627046254899));
#101196=CARTESIAN_POINT('Ctrl Pts',(-20.6617920753916,20.0858254111333,
-19.9631675124283));
#101197=CARTESIAN_POINT('Ctrl Pts',(-20.6603117270743,20.0890802442623,
-19.9633840817028));
#101198=CARTESIAN_POINT('Ctrl Pts',(-20.6568999796044,20.0965314836647,
-19.9638816154836));
#101199=CARTESIAN_POINT('Ctrl Pts',(-20.6549630916597,20.1007253169778,
-19.9641629148743));
#101200=CARTESIAN_POINT('Ctrl Pts',(-20.6489187115762,20.113701126155,-19.9650371214703));
#101201=CARTESIAN_POINT('Ctrl Pts',(-20.6447646744777,20.1224611048584,
-19.9656327945442));
#101202=CARTESIAN_POINT('Ctrl Pts',(-20.5974958425972,20.2203976442717,
-19.9723516834412));
#101203=CARTESIAN_POINT('Ctrl Pts',(-20.5482381121763,20.3064614442048,
-19.978804301781));
#101204=CARTESIAN_POINT('Ctrl Pts',(-20.3994520607462,20.5286955145451,
-19.9964221181772));
#101205=CARTESIAN_POINT('Ctrl Pts',(-20.2893760933458,20.656985506077,-20.0076101401363));
#101206=CARTESIAN_POINT('Ctrl Pts',(-20.142381265471,20.7918586839756,-20.0201370322126));
#101207=CARTESIAN_POINT('Ctrl Pts',(-20.1190566221779,20.8123339058851,
-20.0220657955069));
#101208=CARTESIAN_POINT('Ctrl Pts',(-20.083694192387,20.8420253874502,-20.0249044937089));
#101209=CARTESIAN_POINT('Ctrl Pts',(-20.0719947948906,20.8516365151964,
-20.0258302504258));
#101210=CARTESIAN_POINT('Ctrl Pts',(-20.0530931164119,20.8668276842146,
-20.0273048426957));
#101211=CARTESIAN_POINT('Ctrl Pts',(-20.0459563402534,20.8724880483815,
-20.0278568908671));
#101212=CARTESIAN_POINT('Ctrl Pts',(-20.032275018599,20.8831959448073,-20.0289062961756));
#101213=CARTESIAN_POINT('Ctrl Pts',(-20.0257370300029,20.888251546457,-20.0294039696052));
#101214=CARTESIAN_POINT('Ctrl Pts',(-20.0142093374607,20.8970581291556,
-20.0302748583175));
#101215=CARTESIAN_POINT('Ctrl Pts',(-20.0092323688278,20.9008255440729,
-20.0306487201506));
#101216=CARTESIAN_POINT('Ctrl Pts',(-19.9993768526463,20.9082175337247,
-20.0313848825214));
#101217=CARTESIAN_POINT('Ctrl Pts',(-19.9944992178411,20.9118432199949,
-20.031747224437));
#101218=CARTESIAN_POINT('Ctrl Pts',(-19.9827969500719,20.9204638635275,
-20.0326118280847));
#101219=CARTESIAN_POINT('Ctrl Pts',(-19.9759578325285,20.9254390536238,
-20.0331133193308));
#101220=CARTESIAN_POINT('Ctrl Pts',(-19.9511436683167,20.9432639806312,
-20.0349193587283));
#101221=CARTESIAN_POINT('Ctrl Pts',(-19.9329971415061,20.9558733813039,
-20.0362146834485));
#101222=CARTESIAN_POINT('Ctrl Pts',(-19.7605626419638,21.0717316823665,
-20.0482971339985));
#101223=CARTESIAN_POINT('Ctrl Pts',(-19.5935258037612,21.1545469264989,
-20.058226996901));
#101224=CARTESIAN_POINT('Ctrl Pts',(-19.3420019683425,21.2403940052829,
-20.0727154285207));
#101225=CARTESIAN_POINT('Ctrl Pts',(-19.2647854177626,21.2619439918426,
-20.0771209800648));
#101226=CARTESIAN_POINT('Ctrl Pts',(-19.1513519633396,21.2867658503118,
-20.0837630738697));
#101227=CARTESIAN_POINT('Ctrl Pts',(-19.1159749302518,21.2935660447937,
-20.0858583070635));
#101228=CARTESIAN_POINT('Ctrl Pts',(-19.073079047516,21.30068182661,-20.0884459728523));
#101229=CARTESIAN_POINT('Ctrl Pts',(-19.0657076913315,21.3018645916638,
-20.0888923157214));
#101230=CARTESIAN_POINT('Ctrl Pts',(-19.0542202447418,21.3036455251472,
-20.0895907064303));
#101231=CARTESIAN_POINT('Ctrl Pts',(-19.0501083029054,21.3042706082139,
-20.0898412565919));
#101232=CARTESIAN_POINT('Ctrl Pts',(-19.0424675729422,21.3054090986372,
-20.0903079091407));
#101233=CARTESIAN_POINT('Ctrl Pts',(-19.0389393200879,21.3059257090573,
-20.0905238279943));
#101234=CARTESIAN_POINT('Ctrl Pts',(-19.030944958559,21.3070756280897,-20.0910140347372));
#101235=CARTESIAN_POINT('Ctrl Pts',(-19.0264781434004,21.3077035751025,
-20.0912886202271));
#101236=CARTESIAN_POINT('Ctrl Pts',(-19.0149391402234,21.3092881429337,
-20.0919996560863));
#101237=CARTESIAN_POINT('Ctrl Pts',(-19.0078641268994,21.3102232773034,
-20.0924372735682));
#101238=CARTESIAN_POINT('Ctrl Pts',(-18.9643736385953,21.3157479995676,
-20.0951369196823));
#101239=CARTESIAN_POINT('Ctrl Pts',(-18.927850962396,21.3194253804304,-20.0974452298616));
#101240=CARTESIAN_POINT('Ctrl Pts',(-18.7213619389661,21.334806177892,-20.110659789649));
#101241=CARTESIAN_POINT('Ctrl Pts',(-18.5505653489567,21.3269081264315,
-20.1221547076964));
#101242=CARTESIAN_POINT('Ctrl Pts',(-18.2884045167855,21.2827745397975,
-20.1394321265249));
#101243=CARTESIAN_POINT('Ctrl Pts',(-18.1954218306955,21.2605713935224,
-20.1454985875449));
#101244=CARTESIAN_POINT('Ctrl Pts',(-18.0838108543755,21.2257955611563,
-20.1526795157099));
#101245=CARTESIAN_POINT('Ctrl Pts',(-18.0634741698727,21.2191190806999,
-20.1539841059781));
#101246=CARTESIAN_POINT('Ctrl Pts',(-18.0347231103209,21.2091946959523,
-20.1558235730162));
#101247=CARTESIAN_POINT('Ctrl Pts',(-18.0262233551174,21.2061998487007,
-20.1563667679624));
#101248=CARTESIAN_POINT('Ctrl Pts',(-18.0116010459551,21.2009425493188,
-20.1573002560387));
#101249=CARTESIAN_POINT('Ctrl Pts',(-18.0054694057941,21.1987059071154,
-20.1576914007262));
#101250=CARTESIAN_POINT('Ctrl Pts',(-17.9937544296498,21.194371137569,-20.1584381760808));
#101251=CARTESIAN_POINT('Ctrl Pts',(-17.9881694343077,21.1922777044536,
-20.1587939589084));
#101252=CARTESIAN_POINT('Ctrl Pts',(-17.9736814654561,21.1867772128867,
-20.1597163216899));
#101253=CARTESIAN_POINT('Ctrl Pts',(-17.9647924607477,21.1833335506472,
-20.1602816708529));
#101254=CARTESIAN_POINT('Ctrl Pts',(-17.9346222919521,21.1714104300775,
-20.1621988566334));
#101255=CARTESIAN_POINT('Ctrl Pts',(-17.9134551616601,21.1626454603826,
-20.1635410827725));
#101256=CARTESIAN_POINT('Ctrl Pts',(-17.7304080204605,21.0833439233905,
-20.1751339207498));
#101257=CARTESIAN_POINT('Ctrl Pts',(-17.5778023356978,20.9931566251877,
-20.1846226481057));
#101258=CARTESIAN_POINT('Ctrl Pts',(-17.3699603892135,20.8322717347333,
-20.1989262911642));
#101259=CARTESIAN_POINT('Ctrl Pts',(-17.3050599679199,20.7753702029045,
-20.2036497927853));
#101260=CARTESIAN_POINT('Ctrl Pts',(-17.2170884180828,20.6881879279199,
-20.2107225725073));
#101261=CARTESIAN_POINT('Ctrl Pts',(-17.1910740434533,20.6609944899403,
-20.2129086417915));
#101262=CARTESIAN_POINT('Ctrl Pts',(-17.1607209933252,20.6275236777881,
-20.2155970395049));
#101263=CARTESIAN_POINT('Ctrl Pts',(-17.1556721850282,20.621895980275,-20.2160489851472));
#101264=CARTESIAN_POINT('Ctrl Pts',(-17.1478791669026,20.6131152499366,
-20.2167542503612));
#101265=CARTESIAN_POINT('Ctrl Pts',(-17.1451139090301,20.6099808649583,
-20.2170060241879));
#101266=CARTESIAN_POINT('Ctrl Pts',(-17.1400080879926,20.604158815895,-20.2174737723779));
#101267=CARTESIAN_POINT('Ctrl Pts',(-17.1376650223745,20.6014734231465,
-20.2176895557201));
#101268=CARTESIAN_POINT('Ctrl Pts',(-17.1323898274841,20.5953966029653,
-20.2181779338014));
#101269=CARTESIAN_POINT('Ctrl Pts',(-17.1294617005161,20.5920017898766,
-20.2184508166558));
#101270=CARTESIAN_POINT('Ctrl Pts',(-17.1208698812539,20.5819763902115,
-20.2192567625331));
#101271=CARTESIAN_POINT('Ctrl Pts',(-17.1152364292426,20.5753201744836,
-20.2197919623718));
#101272=CARTESIAN_POINT('Ctrl Pts',(-17.0754280443729,20.5276908507112,
-20.2236211945399));
#101273=CARTESIAN_POINT('Ctrl Pts',(-17.0427745988218,20.4854768864669,
-20.2270123268198));
#101274=CARTESIAN_POINT('Ctrl Pts',(-17.0014698657048,20.4276926691785,
-20.2316028871494));
#101275=CARTESIAN_POINT('Ctrl Pts',(-16.9913672212685,20.4131783109953,
-20.2327518680578));
#101276=CARTESIAN_POINT('Ctrl Pts',(-16.9542828102629,20.358449712802,-20.2370647154527));
#101277=CARTESIAN_POINT('Ctrl Pts',(-16.928502063074,20.3174407268073,-20.2402571474152));
#101278=CARTESIAN_POINT('Ctrl Pts',(-16.8491453205084,20.1810393442284,
-20.2506814069089));
#101279=CARTESIAN_POINT('Ctrl Pts',(-16.8015457833797,20.0823653990544,
-20.2579141799284));
#101280=CARTESIAN_POINT('Ctrl Pts',(-16.7417565160167,19.9291163151288,
-20.2684877832564));
#101281=CARTESIAN_POINT('Ctrl Pts',(-16.7237398566363,19.8770181068162,
-20.2719769928328));
#101282=CARTESIAN_POINT('Ctrl Pts',(-16.6978380967518,19.791439864176,-20.2775346565794));
#101283=CARTESIAN_POINT('Ctrl Pts',(-16.6886997911586,19.7583691662929,
-20.2796415520352));
#101284=CARTESIAN_POINT('Ctrl Pts',(-16.6777441127393,19.714604554195,-20.2823781060041));
#101285=CARTESIAN_POINT('Ctrl Pts',(-16.6751997194972,19.7040996174073,
-20.2830311069466));
#101286=CARTESIAN_POINT('Ctrl Pts',(-16.6711634531294,19.6868591832121,
-20.2840965978255));
#101287=CARTESIAN_POINT('Ctrl Pts',(-16.6696238752665,19.6801351604117,
-20.284510617228));
#101288=CARTESIAN_POINT('Ctrl Pts',(-16.6667068937383,19.6671029497557,
-20.285310120112));
#101289=CARTESIAN_POINT('Ctrl Pts',(-16.6653254325331,19.6607957573325,
-20.2856957299459));
#101290=CARTESIAN_POINT('Ctrl Pts',(-16.6622017498403,19.6462154501031,
-20.2865841308635));
#101291=CARTESIAN_POINT('Ctrl Pts',(-16.6604801817904,19.6379379861622,
-20.2870862559163));
#101292=CARTESIAN_POINT('Ctrl Pts',(-16.6559824261701,19.6156432341906,
-20.2884328251107));
#101293=CARTESIAN_POINT('Ctrl Pts',(-16.6532984651169,19.6016076314751,
-20.2892743280243));
#101294=CARTESIAN_POINT('Ctrl Pts',(-16.6299799881091,19.4725978897857,
-20.2969546135082));
#101295=CARTESIAN_POINT('Ctrl Pts',(-16.6187508688479,19.35612077854,-20.3034768593072));
#101296=CARTESIAN_POINT('Ctrl Pts',(-16.6150144513764,19.0766239483158,
-20.3187792468033));
#101297=CARTESIAN_POINT('Ctrl Pts',(-16.6315987518409,18.9142613277445,
-20.32737647937));
#101298=CARTESIAN_POINT('Ctrl Pts',(-16.6736109104469,18.7236124388203,
-20.3385851003764));
#101299=CARTESIAN_POINT('Ctrl Pts',(-16.6813527832375,18.6919730488902,
-20.340484669114));
#101300=CARTESIAN_POINT('Ctrl Pts',(-16.6917044350884,18.6535322451149,
-20.3428549836005));
#101301=CARTESIAN_POINT('Ctrl Pts',(-16.6936238539226,18.6465474765195,
-20.3432882160116));
#101302=CARTESIAN_POINT('Ctrl Pts',(-16.6966885873772,18.6356148205229,
-20.3439705047836));
#101303=CARTESIAN_POINT('Ctrl Pts',(-16.6978096390778,18.6316601082338,
-20.3442181733064));
#101304=CARTESIAN_POINT('Ctrl Pts',(-16.6999263046096,18.6242752271231,
-20.3446823147868));
#101305=CARTESIAN_POINT('Ctrl Pts',(-16.7009190838304,18.620844304409,-20.3448986220296));
#101306=CARTESIAN_POINT('Ctrl Pts',(-16.7032047245649,18.6130196275873,
-20.3453934677246));
#101307=CARTESIAN_POINT('Ctrl Pts',(-16.7045031605318,18.6086275618869,
-20.3456723275607));
#101308=CARTESIAN_POINT('Ctrl Pts',(-16.7085366015657,18.5951451990489,
-20.3465316486347));
#101309=CARTESIAN_POINT('Ctrl Pts',(-16.7113184618293,18.5860692024863,
-20.3471147443886));
#101310=CARTESIAN_POINT('Ctrl Pts',(-16.7367817781939,18.504944909698,-20.3523662003622));
#101311=CARTESIAN_POINT('Ctrl Pts',(-16.7632408399181,18.4341472256021,
-20.3572277648161));
#101312=CARTESIAN_POINT('Ctrl Pts',(-16.8475388062047,18.2407998437208,
-20.3710207776939));
#101313=CARTESIAN_POINT('Ctrl Pts',(-16.9134444274173,18.1221449755099,
-20.380071654904));
#101314=CARTESIAN_POINT('Ctrl Pts',(-17.0412232627869,17.9365264809378,
-20.3946755832312));
#101315=CARTESIAN_POINT('Ctrl Pts',(-17.0968871011714,17.8657711017126,
-20.400374317523));
#101316=CARTESIAN_POINT('Ctrl Pts',(-17.1707190562842,17.7833195617048,
-20.4071681362679));
#101317=CARTESIAN_POINT('Ctrl Pts',(-17.1847745268805,17.7680796195588,
-20.4084311588121));
#101318=CARTESIAN_POINT('Ctrl Pts',(-17.2051791613217,17.7465973921756,
-20.4102226229612));
#101319=CARTESIAN_POINT('Ctrl Pts',(-17.2113470127651,17.7401852465992,
-20.4107588038578));
#101320=CARTESIAN_POINT('Ctrl Pts',(-17.2220949648835,17.7291516629236,
-20.4116840330176));
#101321=CARTESIAN_POINT('Ctrl Pts',(-17.2266562504447,17.7245121421788,
-20.4120738932576));
#101322=CARTESIAN_POINT('Ctrl Pts',(-17.2354572831088,17.7156423188519,
-20.4128208258324));
#101323=CARTESIAN_POINT('Ctrl Pts',(-17.2396937293779,17.7114088425072,
-20.4131780377929));
#101324=CARTESIAN_POINT('Ctrl Pts',(-17.2508157881043,17.7003885130447,
-20.4141098133903));
#101325=CARTESIAN_POINT('Ctrl Pts',(-17.2577300776067,17.6936307002295,
-20.4146830950959));
#101326=CARTESIAN_POINT('Ctrl Pts',(-17.2817710489933,17.6704536774689,
-20.4166561462286));
#101327=CARTESIAN_POINT('Ctrl Pts',(-17.2991276785304,17.6542747879271,
-20.4180455186176));
#101328=CARTESIAN_POINT('Ctrl Pts',(-17.4372220490245,17.5298231529634,
-20.4288399098562));
#101329=CARTESIAN_POINT('Ctrl Pts',(-17.5697669392347,17.435455854964,-20.4376192523952));
#101330=CARTESIAN_POINT('Ctrl Pts',(-17.826002806886,17.2941698767093,-20.4535153747511));
#101331=CARTESIAN_POINT('Ctrl Pts',(-17.9457644034907,17.241895789985,-20.4606076528614));
#101332=CARTESIAN_POINT('Ctrl Pts',(-18.0808431626167,17.1972431688575,
-20.4690033218645));
#101333=CARTESIAN_POINT('Ctrl Pts',(-18.092165579344,17.1936058909993,-20.4697100607116));
#101334=CARTESIAN_POINT('Ctrl Pts',(-18.1083099118619,17.188569256165,-20.470722839672));
#101335=CARTESIAN_POINT('Ctrl Pts',(-18.1131073251388,17.1870912853774,
-20.4710244270176));
#101336=CARTESIAN_POINT('Ctrl Pts',(-18.1213857891815,17.1845730882951,
-20.4715460102468));
#101337=CARTESIAN_POINT('Ctrl Pts',(-18.1248643808242,17.1835247234353,
-20.4717655314615));
#101338=CARTESIAN_POINT('Ctrl Pts',(-18.1316159712677,17.1815088986904,
-20.4721923107604));
#101339=CARTESIAN_POINT('Ctrl Pts',(-18.134888617637,17.1805403969773,-20.4723995005998));
#101340=CARTESIAN_POINT('Ctrl Pts',(-18.143727874773,17.1779477519314,-20.4729599469651));
#101341=CARTESIAN_POINT('Ctrl Pts',(-18.1492987920689,17.1763385734176,
-20.4733140610665));
#101342=CARTESIAN_POINT('Ctrl Pts',(-18.1700194199307,17.17044547435,-20.4746342979861));
#101343=CARTESIAN_POINT('Ctrl Pts',(-18.1852097317425,17.166307828859,-20.4756083763569));
#101344=CARTESIAN_POINT('Ctrl Pts',(-18.3278725961528,17.1291525194958,
-20.4848055002339));
#101345=CARTESIAN_POINT('Ctrl Pts',(-18.4581078740452,17.1079294301442,
-20.4935470591748));
#101346=CARTESIAN_POINT('Ctrl Pts',(-18.7483666258248,17.0880649382775,
-20.512765243392));
#101347=CARTESIAN_POINT('Ctrl Pts',(-18.9080248088637,17.0951566177402,
-20.523134715843));
#101348=CARTESIAN_POINT('Ctrl Pts',(-19.0864174187945,17.1234311203351,
-20.5342281069483));
#101349=CARTESIAN_POINT('Ctrl Pts',(-19.1073848159156,17.1270792492146,
-20.5355251447755));
#101350=CARTESIAN_POINT('Ctrl Pts',(-19.1371282788457,17.132717671934,-20.5373559214712));
#101351=CARTESIAN_POINT('Ctrl Pts',(-19.1459516440063,17.1344486061607,
-20.5378978712834));
#101352=CARTESIAN_POINT('Ctrl Pts',(-19.161156975732,17.1375322593507,-20.5388299066604));
#101353=CARTESIAN_POINT('Ctrl Pts',(-19.1675441579279,17.1388583499106,
-20.5392208366072));
#101354=CARTESIAN_POINT('Ctrl Pts',(-19.1797638916366,17.1414543536714,
-20.5399676695837));
#101355=CARTESIAN_POINT('Ctrl Pts',(-19.1855973918155,17.1427194517779,
-20.5403237225325));
#101356=CARTESIAN_POINT('Ctrl Pts',(-19.200756728963,17.1460742163823,-20.5412477970872));
#101357=CARTESIAN_POINT('Ctrl Pts',(-19.210073971578,17.1482024059497,-20.5418145788388));
#101358=CARTESIAN_POINT('Ctrl Pts',(-19.2418174041233,17.155679583403,-20.5437418189165));
#101359=CARTESIAN_POINT('Ctrl Pts',(-19.2641709741738,17.1613318975078,
-20.5450925279138));
#101360=CARTESIAN_POINT('Ctrl Pts',(-19.4549969360399,17.2129148995966,
-20.5565784041027));
#101361=CARTESIAN_POINT('Ctrl Pts',(-19.6172789241533,17.2791600141646,
-20.5659713132975));
#101362=CARTESIAN_POINT('Ctrl Pts',(-19.8460072152757,17.4074466969931,
-20.5802385721217));
#101363=CARTESIAN_POINT('Ctrl Pts',(-19.9196794697496,17.455002753997,-20.5850329924141));
#101364=CARTESIAN_POINT('Ctrl Pts',(-20.0207558647494,17.5295153697323,
-20.5922013954482));
#101365=CARTESIAN_POINT('Ctrl Pts',(-20.0507099894184,17.5528668276205,
-20.594407091961));
#101366=CARTESIAN_POINT('Ctrl Pts',(-20.0858687975861,17.5818292848284,
-20.597117248846));
#101367=CARTESIAN_POINT('Ctrl Pts',(-20.0916937737515,17.5866804261975,
-20.5975703739912));
#101368=CARTESIAN_POINT('Ctrl Pts',(-20.1006932904131,17.5942576092888,
-20.5982770887487));
#101369=CARTESIAN_POINT('Ctrl Pts',(-20.1038860824254,17.5969620114556,
-20.5985291224611));
#101370=CARTESIAN_POINT('Ctrl Pts',(-20.1097830253455,17.6019870215249,
-20.5989970938741));
#101371=CARTESIAN_POINT('Ctrl Pts',(-20.1124893426084,17.6043049979944,
-20.5992128389032));
#101372=CARTESIAN_POINT('Ctrl Pts',(-20.1185827491747,17.6095507641986,
-20.5997008031928));
#101373=CARTESIAN_POINT('Ctrl Pts',(-20.1219663903594,17.6124824547283,
-20.5999733084864));
#101374=CARTESIAN_POINT('Ctrl Pts',(-20.1318927161188,17.6211382053024,
-20.600777214251));
#101375=CARTESIAN_POINT('Ctrl Pts',(-20.1384093794245,17.6268917773528,
-20.601310736214));
#101376=CARTESIAN_POINT('Ctrl Pts',(-20.1842711531029,17.667888625123,-20.6051052317313));
#101377=CARTESIAN_POINT('Ctrl Pts',(-20.2223172484895,17.7045505680284,
-20.6084614050717));
#101378=CARTESIAN_POINT('Ctrl Pts',(-20.2724917961696,17.7566571257431,
-20.6131348661714));
#101379=CARTESIAN_POINT('Ctrl Pts',(-20.2858389487213,17.7709076254727,
-20.6144037567851));
#101380=CARTESIAN_POINT('Ctrl Pts',(-20.3975967056274,17.8935872679086,
-20.6252363275479));
#101381=CARTESIAN_POINT('Ctrl Pts',(-20.4847193340846,18.0117847032248,
-20.635041563272));
#101382=CARTESIAN_POINT('Ctrl Pts',(-20.5902290418307,18.1912387775492,
-20.6484906099546));
#101383=CARTESIAN_POINT('Ctrl Pts',(-20.6191743051358,18.2457963052028,
-20.652416720791));
#101384=CARTESIAN_POINT('Ctrl Pts',(-20.6616864794049,18.3351579187673,
-20.6585827206034));
#101385=CARTESIAN_POINT('Ctrl Pts',(-20.6767885690955,18.3691880460116,
-20.6608723820402));
#101386=CARTESIAN_POINT('Ctrl Pts',(-20.6952311498234,18.4138894314091,
-20.6638069544908));
#101387=CARTESIAN_POINT('Ctrl Pts',(-20.6993949387512,18.4242118304521,
-20.6644796438639));
#101388=CARTESIAN_POINT('Ctrl Pts',(-20.7060329030986,18.4410494907003,
-20.6655690059949));
#101389=CARTESIAN_POINT('Ctrl Pts',(-20.7085566166865,18.4475448755945,
-20.6659873429946));
#101390=CARTESIAN_POINT('Ctrl Pts',(-20.7133473834865,18.4600577369324,
-20.6667896316462));
#101391=CARTESIAN_POINT('Ctrl Pts',(-20.7156191778918,18.4660733041461,
-20.6671737389019));
#101392=CARTESIAN_POINT('Ctrl Pts',(-20.7194496212452,18.476357603124,-20.6678277322614));
#101393=CARTESIAN_POINT('Ctrl Pts',(-20.7210219845465,18.4806211373333,
-20.6680980731543));
#101394=CARTESIAN_POINT('Ctrl Pts',(-20.7225806137969,18.4848897174457,
-20.6683679590049));
#101395=CARTESIAN_POINT('',(-20.8509992561167,19.2127747116643,-19.6896815252242));
#101396=CARTESIAN_POINT('Ctrl Pts',(-20.7225807433526,18.4848900722567,
-20.4442393203449));
#101397=CARTESIAN_POINT('Ctrl Pts',(-20.6728906059831,18.3488048232718,
-20.4346846760922));
#101398=CARTESIAN_POINT('Ctrl Pts',(-20.6093080638511,18.2180329568345,
-20.4252946696087));
#101399=CARTESIAN_POINT('Ctrl Pts',(-20.5215596808033,18.076641000874,-20.4150700053436));
#101400=CARTESIAN_POINT('Ctrl Pts',(-20.5100907656587,18.0587666924442,
-20.4137751521916));
#101401=CARTESIAN_POINT('Ctrl Pts',(-20.4937578192524,18.0341352659228,
-20.4119870263363));
#101402=CARTESIAN_POINT('Ctrl Pts',(-20.489120264994,18.0272301561407,-20.4114853253551));
#101403=CARTESIAN_POINT('Ctrl Pts',(-20.4810444660834,18.0153574414848,
-20.410621905054));
#101404=CARTESIAN_POINT('Ctrl Pts',(-20.4776254578743,18.010376929243,-20.4102594642419));
#101405=CARTESIAN_POINT('Ctrl Pts',(-20.4705005833394,18.0000926601601,
-20.4095105249595));
#101406=CARTESIAN_POINT('Ctrl Pts',(-20.4667916236948,17.9947911150203,
-20.4091241495084));
#101407=CARTESIAN_POINT('Ctrl Pts',(-20.4580472077302,17.9824131472918,
-20.4082213013032));
#101408=CARTESIAN_POINT('Ctrl Pts',(-20.4529923702198,17.9753505093745,
-20.4077055785196));
#101409=CARTESIAN_POINT('Ctrl Pts',(-20.4364321499066,17.9525108047212,
-20.4060357450383));
#101410=CARTESIAN_POINT('Ctrl Pts',(-20.4247517091076,17.9368614770944,
-20.4048884148582));
#101411=CARTESIAN_POINT('Ctrl Pts',(-20.3638544321887,17.8575843122734,
-20.3990559677338));
#101412=CARTESIAN_POINT('Ctrl Pts',(-20.3112538502044,17.796633773947,-20.3945074746445));
#101413=CARTESIAN_POINT('Ctrl Pts',(-20.138483026706,17.6180975957617,-20.3807326283317));
#101414=CARTESIAN_POINT('Ctrl Pts',(-20.0077165243318,17.5117208941659,
-20.3718907614783));
#101415=CARTESIAN_POINT('Ctrl Pts',(-19.8645530330822,17.4211561819165,
-20.3623782531059));
#101416=CARTESIAN_POINT('Ctrl Pts',(-19.8633411537126,17.420391273265,-20.3622977373751));
#101417=CARTESIAN_POINT('Ctrl Pts',(-19.81655501399,17.3909273954177,-20.3591895853458));
#101418=CARTESIAN_POINT('Ctrl Pts',(-19.7699069101227,17.3639792984401,
-20.3561002921224));
#101419=CARTESIAN_POINT('Ctrl Pts',(-19.7145584441951,17.3347616067901,
-20.3523863368298));
#101420=CARTESIAN_POINT('Ctrl Pts',(-19.7068050888467,17.33072990669,-20.3518649966277));
#101421=CARTESIAN_POINT('Ctrl Pts',(-19.6950331765953,17.3247008801767,
-20.3510714814948));
#101422=CARTESIAN_POINT('Ctrl Pts',(-19.6910327562121,17.3226680803822,
-20.3508014819472));
#101423=CARTESIAN_POINT('Ctrl Pts',(-19.6838432653658,17.3190434795445,
-20.3503155779541));
#101424=CARTESIAN_POINT('Ctrl Pts',(-19.6806566133226,17.3174470009492,
-20.3500999709661));
#101425=CARTESIAN_POINT('Ctrl Pts',(-19.6737268225542,17.313997115266,-20.3496305813145));
#101426=CARTESIAN_POINT('Ctrl Pts',(-19.6699822753743,17.3121467604877,
-20.3493766185275));
#101427=CARTESIAN_POINT('Ctrl Pts',(-19.6594568561791,17.3069843599479,
-20.3486619023854));
#101428=CARTESIAN_POINT('Ctrl Pts',(-19.6526637936787,17.303697512072,-20.3481996277763));
#101429=CARTESIAN_POINT('Ctrl Pts',(-19.6121138579633,17.2843441626581,
-20.3454348739854));
#101430=CARTESIAN_POINT('Ctrl Pts',(-19.5779559774992,17.2691388890306,
-20.3430842637068));
#101431=CARTESIAN_POINT('Ctrl Pts',(-19.4646091700166,17.2222383027167,
-20.3352555019467));
#101432=CARTESIAN_POINT('Ctrl Pts',(-19.3839086960102,17.1944237767704,
-20.3296395655382));
#101433=CARTESIAN_POINT('Ctrl Pts',(-19.1303563755561,17.1238379271948,
-20.3122523962994));
#101434=CARTESIAN_POINT('Ctrl Pts',(-18.9535875700027,17.0979099373504,
-20.3005610254208));
#101435=CARTESIAN_POINT('Ctrl Pts',(-18.752839403414,17.0939610479623,-20.2882045288104));
#101436=CARTESIAN_POINT('Ctrl Pts',(-18.7300372273483,17.0938809178972,
-20.2868128276617));
#101437=CARTESIAN_POINT('Ctrl Pts',(-18.6977234993785,17.0942894515593,
-20.2848566749309));
#101438=CARTESIAN_POINT('Ctrl Pts',(-18.6882103146583,17.0944738745489,
-20.2842827535119));
#101439=CARTESIAN_POINT('Ctrl Pts',(-18.6727394882684,17.0948781498583,
-20.283352537761));
#101440=CARTESIAN_POINT('Ctrl Pts',(-18.6667810406777,17.0950590396748,
-20.2829950275873));
#101441=CARTESIAN_POINT('Ctrl Pts',(-18.6542977717837,17.0954907966553,
-20.2822475745448));
#101442=CARTESIAN_POINT('Ctrl Pts',(-18.6477731783199,17.0957466886174,
-20.2818577931372));
#101443=CARTESIAN_POINT('Ctrl Pts',(-18.632231273506,17.0964282663284,-20.2809313804777));
#101444=CARTESIAN_POINT('Ctrl Pts',(-18.6232152485678,17.0968814524183,
-20.2803956165752));
#101445=CARTESIAN_POINT('Ctrl Pts',(-18.5927418222677,17.0986086635144,
-20.2785901794381));
#101446=CARTESIAN_POINT('Ctrl Pts',(-18.5713005723079,17.1001518345607,
-20.2773289409156));
#101447=CARTESIAN_POINT('Ctrl Pts',(-18.3710912248426,17.1176301312793,
-20.2656276868687));
#101448=CARTESIAN_POINT('Ctrl Pts',(-18.1950096865446,17.155909585088,-20.2559846656249));
#101449=CARTESIAN_POINT('Ctrl Pts',(-17.9123224784601,17.2562496983917,
-20.239659495714));
#101450=CARTESIAN_POINT('Ctrl Pts',(-17.8024525421218,17.3061604911142,
-20.2330499538334));
#101451=CARTESIAN_POINT('Ctrl Pts',(-17.6891592405312,17.3697811165665,
-20.2253492287921));
#101452=CARTESIAN_POINT('Ctrl Pts',(-17.6809102776687,17.3744866680367,
-20.2247831552277));
#101453=CARTESIAN_POINT('Ctrl Pts',(-17.668729829774,17.3815439474008,-20.223938864268));
#101454=CARTESIAN_POINT('Ctrl Pts',(-17.6647737376536,17.3838532672582,
-20.2236633191161));
#101455=CARTESIAN_POINT('Ctrl Pts',(-17.6577463291092,17.3879860686191,
-20.223171430173));
#101456=CARTESIAN_POINT('Ctrl Pts',(-17.6546721017577,17.389804500895,-20.2229554153578));
#101457=CARTESIAN_POINT('Ctrl Pts',(-17.6480701593711,17.393732195175,-20.2224897131493));
#101458=CARTESIAN_POINT('Ctrl Pts',(-17.6445440323422,17.3958439221123,
-20.2222398701498));
#101459=CARTESIAN_POINT('Ctrl Pts',(-17.6348222554596,17.4017046324115,
-20.2215480153092));
#101460=CARTESIAN_POINT('Ctrl Pts',(-17.6286397260923,17.4054751171345,
-20.2211046318912));
#101461=CARTESIAN_POINT('Ctrl Pts',(-17.5947844377301,17.4263612041883,
-20.2186584702281));
#101462=CARTESIAN_POINT('Ctrl Pts',(-17.5674913724603,17.4440803409526,
-20.2166193474724));
#101463=CARTESIAN_POINT('Ctrl Pts',(-17.4062323924254,17.5541372896315,
-20.2042133326344));
#101464=CARTESIAN_POINT('Ctrl Pts',(-17.2828701653958,17.6610377443148,
-20.1932565596486));
#101465=CARTESIAN_POINT('Ctrl Pts',(-17.0940658716516,17.8671437397052,
-20.1749990462804));
#101466=CARTESIAN_POINT('Ctrl Pts',(-17.0224173953814,17.9596701525316,
-20.1675583081085));
#101467=CARTESIAN_POINT('Ctrl Pts',(-16.9509757827139,18.0696333521042,
-20.1595513474906));
#101468=CARTESIAN_POINT('Ctrl Pts',(-16.9433122896736,18.081694583312,-20.1586833737028));
#101469=CARTESIAN_POINT('Ctrl Pts',(-16.9313098110433,18.1010141617528,
-20.1573090685292));
#101470=CARTESIAN_POINT('Ctrl Pts',(-16.9268912795455,18.1082223459977,
-20.156799809085));
#101471=CARTESIAN_POINT('Ctrl Pts',(-16.9191746656097,18.1209817915745,
-20.155904432912));
#101472=CARTESIAN_POINT('Ctrl Pts',(-16.9158585990382,18.126521998109,-20.1555176600582));
#101473=CARTESIAN_POINT('Ctrl Pts',(-16.9090523342738,18.1380123018482,
-20.1547195928986));
#101474=CARTESIAN_POINT('Ctrl Pts',(-16.9055657637645,18.143964467078,-20.1543084339737));
#101475=CARTESIAN_POINT('Ctrl Pts',(-16.896690896535,18.1592865956576,-20.1532557261412));
#101476=CARTESIAN_POINT('Ctrl Pts',(-16.8913451116359,18.1686810490569,
-20.1526157185331));
#101477=CARTESIAN_POINT('Ctrl Pts',(-16.8693339928606,18.208061058517,-20.1499550578646));
#101478=CARTESIAN_POINT('Ctrl Pts',(-16.853326246324,18.2384095068536,-20.1479579335101));
#101479=CARTESIAN_POINT('Ctrl Pts',(-16.813545968641,18.3184856500672,-20.1428138659717));
#101480=CARTESIAN_POINT('Ctrl Pts',(-16.7909645796331,18.3687770176533,
-20.1397063117002));
#101481=CARTESIAN_POINT('Ctrl Pts',(-16.729508374182,18.5213196846395,-20.1305619110663));
#101482=CARTESIAN_POINT('Ctrl Pts',(-16.6965650566323,18.625760433208,-20.1246737943342));
#101483=CARTESIAN_POINT('Ctrl Pts',(-16.6614983193697,18.7768154286109,
-20.116231033899));
#101484=CARTESIAN_POINT('Ctrl Pts',(-16.6526050361312,18.8216746533904,
-20.1137310759661));
#101485=CARTESIAN_POINT('Ctrl Pts',(-16.6414626797021,18.8892907854021,
-20.109931173351));
#101486=CARTESIAN_POINT('Ctrl Pts',(-16.6381180741534,18.9118542887672,
-20.1086578632305));
#101487=CARTESIAN_POINT('Ctrl Pts',(-16.6349974222111,18.9355397495938,
-20.1073117924615));
#101488=CARTESIAN_POINT('Ctrl Pts',(-16.6348568850456,18.9366127662384,
-20.1072507914662));
#101489=CARTESIAN_POINT('Ctrl Pts',(-16.6322374465911,18.9567322622386,
-20.1061066103224));
#101490=CARTESIAN_POINT('Ctrl Pts',(-16.6300171109765,18.9758109798522,
-20.1050151058199));
#101491=CARTESIAN_POINT('Ctrl Pts',(-16.6247209031575,19.0274277145969,
-20.1020383098619));
#101492=CARTESIAN_POINT('Ctrl Pts',(-16.6221385626885,19.0600096082949,
-20.1001338376914));
#101493=CARTESIAN_POINT('Ctrl Pts',(-16.6199272709424,19.0994978606305,
-20.0977810017928));
#101494=CARTESIAN_POINT('Ctrl Pts',(-16.6195764447247,19.1063613035157,
-20.0973704250738));
#101495=CARTESIAN_POINT('Ctrl Pts',(-16.6190544600331,19.1176512677001,
-20.0966921914135));
#101496=CARTESIAN_POINT('Ctrl Pts',(-16.6188637624841,19.122076894036,-20.096425604087));
#101497=CARTESIAN_POINT('Ctrl Pts',(-16.6185448279198,19.1300611628517,
-20.0959432995976));
#101498=CARTESIAN_POINT('Ctrl Pts',(-16.6184116783697,19.1336195536188,
-20.0957278604086));
#101499=CARTESIAN_POINT('Ctrl Pts',(-16.6181402572395,19.141398419221,-20.0952558208679));
#101500=CARTESIAN_POINT('Ctrl Pts',(-16.618005636687,19.1456189263562,-20.0949990237828));
#101501=CARTESIAN_POINT('Ctrl Pts',(-16.6176594987087,19.1575951432613,
-20.0942684353934));
#101502=CARTESIAN_POINT('Ctrl Pts',(-16.6174779917045,19.1653515579983,
-20.0937930147968));
#101503=CARTESIAN_POINT('Ctrl Pts',(-16.6166002516263,19.2143832865097,
-20.090774172285));
#101504=CARTESIAN_POINT('Ctrl Pts',(-16.6170688673251,19.2556676444565,
-20.0881719902205));
#101505=CARTESIAN_POINT('Ctrl Pts',(-16.6263056167701,19.4830965564417,
-20.0735979883229));
#101506=CARTESIAN_POINT('Ctrl Pts',(-16.6584150814937,19.667474680233,-20.0609880542896));
#101507=CARTESIAN_POINT('Ctrl Pts',(-16.7265097397931,19.8843092161046,
-20.0463553693014));
#101508=CARTESIAN_POINT('Ctrl Pts',(-16.7398954494216,19.9229759886991,
-20.0437495378147));
#101509=CARTESIAN_POINT('Ctrl Pts',(-16.7714206331086,20.0061601274996,
-20.038155973527));
#101510=CARTESIAN_POINT('Ctrl Pts',(-16.7899728257612,20.0504976674327,
-20.0351826552735));
#101511=CARTESIAN_POINT('Ctrl Pts',(-16.8152563240624,20.1055777254093,
-20.0314966012245));
#101512=CARTESIAN_POINT('Ctrl Pts',(-16.8205950248732,20.1169404023194,
-20.0307365803096));
#101513=CARTESIAN_POINT('Ctrl Pts',(-16.829222354364,20.1348859510944,-20.0295367007417));
#101514=CARTESIAN_POINT('Ctrl Pts',(-16.8324447082229,20.1415001904288,
-20.0290945558979));
#101515=CARTESIAN_POINT('Ctrl Pts',(-16.8385177147121,20.1538024090151,
-20.0282723197112));
#101516=CARTESIAN_POINT('Ctrl Pts',(-16.8413596455273,20.159494578937,-20.0278919298622));
#101517=CARTESIAN_POINT('Ctrl Pts',(-16.8477345680061,20.1721203225221,
-20.0270482709653));
#101518=CARTESIAN_POINT('Ctrl Pts',(-16.8512802274971,20.1790474239422,
-20.0265854523787));
#101519=CARTESIAN_POINT('Ctrl Pts',(-16.8617121017617,20.1991539030193,
-20.0252421315433));
#101520=CARTESIAN_POINT('Ctrl Pts',(-16.868699165901,20.2122806425408,-20.0243651931879));
#101521=CARTESIAN_POINT('Ctrl Pts',(-16.9263126056649,20.3178238053714,
-20.0173123880134));
#101522=CARTESIAN_POINT('Ctrl Pts',(-16.9836392822435,20.4064221959172,
-20.0113903529587));
#101523=CARTESIAN_POINT('Ctrl Pts',(-17.1506102904383,20.6265458347475,
-19.9961927724823));
#101524=CARTESIAN_POINT('Ctrl Pts',(-17.2699801424405,20.7496769061546,
-19.9872040129537));
#101525=CARTESIAN_POINT('Ctrl Pts',(-17.4310700848671,20.8799462121164,
-19.9753651326896));
#101526=CARTESIAN_POINT('Ctrl Pts',(-17.4598889608157,20.9020495346235,
-19.9732549007287));
#101527=CARTESIAN_POINT('Ctrl Pts',(-17.4950130511549,20.9275811739013,
-19.9706731292046));
#101528=CARTESIAN_POINT('Ctrl Pts',(-17.5007870632448,20.9317339815871,
-19.9702484037449));
#101529=CARTESIAN_POINT('Ctrl Pts',(-17.5102509758777,20.9384685543212,
-19.9695515550325));
#101530=CARTESIAN_POINT('Ctrl Pts',(-17.5139284352826,20.9410678184152,
-19.969280604102));
#101531=CARTESIAN_POINT('Ctrl Pts',(-17.5205321909445,20.9457038906499,
-19.9687936860607));
#101532=CARTESIAN_POINT('Ctrl Pts',(-17.5234553626189,20.9477450568451,
-19.968578021834));
#101533=CARTESIAN_POINT('Ctrl Pts',(-17.5298043194842,20.952154532896,-19.9681093209745));
#101534=CARTESIAN_POINT('Ctrl Pts',(-17.5332318947952,20.9545200891387,
-19.9678561086374));
#101535=CARTESIAN_POINT('Ctrl Pts',(-17.542843949844,20.9611121036239,-19.9671455732856));
#101536=CARTESIAN_POINT('Ctrl Pts',(-17.5490438430358,20.9653158248424,
-19.9666867569045));
#101537=CARTESIAN_POINT('Ctrl Pts',(-17.5855322703882,20.9897744472999,
-19.9639840988715));
#101538=CARTESIAN_POINT('Ctrl Pts',(-17.6163154316405,21.0092762570028,
-19.9616945576796));
#101539=CARTESIAN_POINT('Ctrl Pts',(-17.7176718529215,21.0698799307747,
-19.9541639183685));
#101540=CARTESIAN_POINT('Ctrl Pts',(-17.790121126065,21.1076940730335,-19.9487955231222));
#101541=CARTESIAN_POINT('Ctrl Pts',(-18.0316576092181,21.2164893821606,
-19.9313020627634));
#101542=CARTESIAN_POINT('Ctrl Pts',(-18.2078510505483,21.2697536045674,
-19.9192368835383));
#101543=CARTESIAN_POINT('Ctrl Pts',(-18.4107597067682,21.3032962078264,
-19.9065862044123));
#101544=CARTESIAN_POINT('Ctrl Pts',(-18.4328493528678,21.3065896678846,
-19.9052235065917));
#101545=CARTESIAN_POINT('Ctrl Pts',(-18.4634073217987,21.310652529906,-19.903357762854));
#101546=CARTESIAN_POINT('Ctrl Pts',(-18.4718337372479,21.3117213041717,
-19.9028453020299));
#101547=CARTESIAN_POINT('Ctrl Pts',(-18.4863097608782,21.313468929447,-19.9019683343136));
#101548=CARTESIAN_POINT('Ctrl Pts',(-18.4923562347127,21.3141724479337,
-19.9016030528011));
#101549=CARTESIAN_POINT('Ctrl Pts',(-18.5048099557765,21.3155670462917,
-19.9008527586787));
#101550=CARTESIAN_POINT('Ctrl Pts',(-18.5112174982534,21.3162549696037,
-19.9004678492857));
#101551=CARTESIAN_POINT('Ctrl Pts',(-18.5261056533957,21.3177846514556,
-19.8995760599226));
#101552=CARTESIAN_POINT('Ctrl Pts',(-18.5345884445009,21.3186044841792,
-19.8990698751179));
#101553=CARTESIAN_POINT('Ctrl Pts',(-18.561633245491,21.3210535290192,-19.897462037221));
#101554=CARTESIAN_POINT('Ctrl Pts',(-18.5802122374725,21.3224889415647,
-19.8963664720597));
#101555=CARTESIAN_POINT('Ctrl Pts',(-18.7564804645901,21.3337684677006,
-19.8860513128699));
#101556=CARTESIAN_POINT('Ctrl Pts',(-18.9147901479484,21.3261771440115,
-19.8774371923853));
#101557=CARTESIAN_POINT('Ctrl Pts',(-19.133304647157,21.2909647471643,-19.8654175769343));
#101558=CARTESIAN_POINT('Ctrl Pts',(-19.1953264881964,21.2780933740107,
-19.8619838223684));
#101559=CARTESIAN_POINT('Ctrl Pts',(-19.2922208170295,21.2534064072117,
-19.8564699346951));
#101560=CARTESIAN_POINT('Ctrl Pts',(-19.3275224580092,21.2434284233966,
-19.8544287090835));
#101561=CARTESIAN_POINT('Ctrl Pts',(-19.4078776284072,21.2184440457469,
-19.8496720799651));
#101562=CARTESIAN_POINT('Ctrl Pts',(-19.4527190446368,21.2028295227764,
-19.8469364951043));
#101563=CARTESIAN_POINT('Ctrl Pts',(-19.5041874679935,21.1829431372245,
-19.8436603913552));
#101564=CARTESIAN_POINT('Ctrl Pts',(-19.5113656418058,21.1801244569969,
-19.8432003460221));
#101565=CARTESIAN_POINT('Ctrl Pts',(-19.5228321684879,21.1755493844044,
-19.8424601887408));
#101566=CARTESIAN_POINT('Ctrl Pts',(-19.5271305091645,21.1738179916393,
-19.8421815413537));
#101567=CARTESIAN_POINT('Ctrl Pts',(-19.5347454477853,21.1707215595706,
-19.8416857135591));
#101568=CARTESIAN_POINT('Ctrl Pts',(-19.5380643013971,21.1693621887294,
-19.8414688771737));
#101569=CARTESIAN_POINT('Ctrl Pts',(-19.545105165204,21.1664574022672,-19.8410072758713));
#101570=CARTESIAN_POINT('Ctrl Pts',(-19.5488261634816,21.1649098146488,
-19.8407623856657));
#101571=CARTESIAN_POINT('Ctrl Pts',(-19.5587594185208,21.1607451994584,
-19.8401061763205));
#101572=CARTESIAN_POINT('Ctrl Pts',(-19.5649635720808,21.158109134152,-19.8396937277843));
#101573=CARTESIAN_POINT('Ctrl Pts',(-19.5953243714915,21.1450376858571,
-19.8376630109399));
#101574=CARTESIAN_POINT('Ctrl Pts',(-19.6192964325269,21.1341826544191,
-19.8360211750285));
#101575=CARTESIAN_POINT('Ctrl Pts',(-19.6875994671247,21.1017060739613,
-19.831244645076));
#101576=CARTESIAN_POINT('Ctrl Pts',(-19.7313838060925,21.0789792025445,
-19.8280615524495));
#101577=CARTESIAN_POINT('Ctrl Pts',(-19.8622003523279,21.005166116682,-19.818257712721));
#101578=CARTESIAN_POINT('Ctrl Pts',(-19.9464116339282,20.9493688012213,
-19.8115418948507));
#101579=CARTESIAN_POINT('Ctrl Pts',(-20.0549024968569,20.8657530180286,
-19.8025410873885));
#101580=CARTESIAN_POINT('Ctrl Pts',(-20.0829148471729,20.8429987237112,
-19.8001815409466));
#101581=CARTESIAN_POINT('Ctrl Pts',(-20.1868001578078,20.754110140009,-19.791310017457));
#101582=CARTESIAN_POINT('Ctrl Pts',(-20.2585130730344,20.6833050595772,
-19.7849405203657));
#101583=CARTESIAN_POINT('Ctrl Pts',(-20.3341511245986,20.5971460824146,
-19.7779428091084));
#101584=CARTESIAN_POINT('Ctrl Pts',(-20.3432733702532,20.5865449167058,
-19.7770935587611));
#101585=CARTESIAN_POINT('Ctrl Pts',(-20.3576837179667,20.5694587493837,
-19.7757432252811));
#101586=CARTESIAN_POINT('Ctrl Pts',(-20.3630394689401,20.5630315830412,
-19.7752393709102));
#101587=CARTESIAN_POINT('Ctrl Pts',(-20.3724519313685,20.5515990357681,
-19.7743502625094));
#101588=CARTESIAN_POINT('Ctrl Pts',(-20.3765241311846,20.5466065985188,
-19.7739643812795));
#101589=CARTESIAN_POINT('Ctrl Pts',(-20.3849325598667,20.5362014116365,
-19.7731650172965));
#101590=CARTESIAN_POINT('Ctrl Pts',(-20.3892651129541,20.530785780431,-19.7727516854409));
#101591=CARTESIAN_POINT('Ctrl Pts',(-20.4003867771015,20.5167429403856,
-19.7716868303743));
#101592=CARTESIAN_POINT('Ctrl Pts',(-20.4071355896917,20.5080839690015,
-19.7710369188416));
#101593=CARTESIAN_POINT('Ctrl Pts',(-20.4356099872692,20.470958244399,-19.7682782440148));
#101594=CARTESIAN_POINT('Ctrl Pts',(-20.456679536607,20.4419942173802,-19.7661952793857));
#101595=CARTESIAN_POINT('Ctrl Pts',(-20.5337126838843,20.3302437027319,
-19.7583966171025));
#101596=CARTESIAN_POINT('Ctrl Pts',(-20.5845280728317,20.2440638564465,
-19.7528697247338));
#101597=CARTESIAN_POINT('Ctrl Pts',(-20.6638151472762,20.0848300110632,
-19.7431609957673));
#101598=CARTESIAN_POINT('Ctrl Pts',(-20.6946793403609,20.0131856015894,
-19.7389559408234));
#101599=CARTESIAN_POINT('Ctrl Pts',(-20.7569619472626,19.8433810274421,
-19.7290683047582));
#101600=CARTESIAN_POINT('Ctrl Pts',(-20.7853043460614,19.7443156568392,
-19.723357616558));
#101601=CARTESIAN_POINT('Ctrl Pts',(-20.8083091498158,19.6341127964012,
-19.7166879443766));
#101602=CARTESIAN_POINT('Ctrl Pts',(-20.8102239738572,19.6246144216661,
-19.7161105312899));
#101603=CARTESIAN_POINT('Ctrl Pts',(-20.8129550808653,19.610569896252,-19.7152525410502));
#101604=CARTESIAN_POINT('Ctrl Pts',(-20.8138218293213,19.6060335271828,
-19.7149747635366));
#101605=CARTESIAN_POINT('Ctrl Pts',(-20.8153332624705,19.5979801487786,
-19.7144804213719));
#101606=CARTESIAN_POINT('Ctrl Pts',(-20.8159838885478,19.5944643042486,
-19.7142641983415));
#101607=CARTESIAN_POINT('Ctrl Pts',(-20.8173589116012,19.5869273059115,
-19.7137997822212));
#101608=CARTESIAN_POINT('Ctrl Pts',(-20.8180805645791,19.5829057589892,
-19.7135514426252));
#101609=CARTESIAN_POINT('Ctrl Pts',(-20.819537629611,19.5746485627133,-19.7130404718471));
#101610=CARTESIAN_POINT('Ctrl Pts',(-20.8202717900265,19.5704127141436,
-19.7127777724921));
#101611=CARTESIAN_POINT('Ctrl Pts',(-20.822097106375,19.5596872247049,-19.7121111890396));
#101612=CARTESIAN_POINT('Ctrl Pts',(-20.8231709050189,19.5531947302344,
-19.7117063802511));
#101613=CARTESIAN_POINT('Ctrl Pts',(-20.8419517274706,19.4362562556051,
-19.7043930786085));
#101614=CARTESIAN_POINT('Ctrl Pts',(-20.8509055124935,19.3245986120908,
-19.6970632785419));
#101615=CARTESIAN_POINT('Ctrl Pts',(-20.8509992561167,19.2127747116643,
-19.6896815252242));
#101616=CARTESIAN_POINT('Ctrl Pts',(-20.8509992546756,19.2127764298092,
-19.6896816386429));
#101617=CARTESIAN_POINT('Ctrl Pts',(-20.8510842733145,19.1114583848993,
-19.6829934015258));
#101618=CARTESIAN_POINT('Ctrl Pts',(-20.8438956128816,19.0102558470168,
-19.6762800379215));
#101619=CARTESIAN_POINT('Ctrl Pts',(-20.8169455020383,18.8226665579838,
-19.6640097393302));
#101620=CARTESIAN_POINT('Ctrl Pts',(-20.7989633497378,18.7362425929389,
-19.6584263192726));
#101621=CARTESIAN_POINT('Ctrl Pts',(-20.7702151437283,18.63139866288,-19.6517544981652));
#101622=CARTESIAN_POINT('Ctrl Pts',(-20.7645030418353,18.6116943474891,
-19.6505048401514));
#101623=CARTESIAN_POINT('Ctrl Pts',(-20.755915138356,18.5836032652825,-19.6487288464412));
#101624=CARTESIAN_POINT('Ctrl Pts',(-20.7532718150684,18.5751471632154,
-19.648194953417));
#101625=CARTESIAN_POINT('Ctrl Pts',(-20.748597373308,18.5605165894664,-19.6472724085706));
#101626=CARTESIAN_POINT('Ctrl Pts',(-20.746590773711,18.5543344664484,-19.6468829576124));
#101627=CARTESIAN_POINT('Ctrl Pts',(-20.7426778410948,18.5424655563447,
-19.6461359337708));
#101628=CARTESIAN_POINT('Ctrl Pts',(-20.7407757522879,18.5367774456252,
-19.6457782254421));
#101629=CARTESIAN_POINT('Ctrl Pts',(-20.7357295714009,18.5218976172911,
-19.644843218429));
#101630=CARTESIAN_POINT('Ctrl Pts',(-20.7325463159622,18.5127192551639,
-19.644267219346));
#101631=CARTESIAN_POINT('Ctrl Pts',(-20.72708934705,18.4973280754487,-19.6433024502794));
#101632=CARTESIAN_POINT('Ctrl Pts',(-20.7248495421185,18.4911035763927,
-19.6429125887592));
#101633=CARTESIAN_POINT('Ctrl Pts',(-20.7225806138715,18.48488971765,-19.6425236773711));
#101634=CARTESIAN_POINT('Origin',(-18.734,19.211,0.));
#101635=CARTESIAN_POINT('',(-20.7225806605155,18.4848898453927,-18.8452754875981));
#101636=CARTESIAN_POINT('',(-20.7225806137985,18.4848897174502,-19.0663245303817));
#101637=CARTESIAN_POINT('',(-20.7225806137986,18.4848897174502,0.));
#101638=CARTESIAN_POINT('',(-20.8499620916056,19.2091158126,-19.1109437209775));
#101639=CARTESIAN_POINT('Ctrl Pts',(-20.7225806137985,18.4848897174502,
-19.0663245303817));
#101640=CARTESIAN_POINT('Ctrl Pts',(-20.7389261121638,18.5296547372455,
-19.0692018356968));
#101641=CARTESIAN_POINT('Ctrl Pts',(-20.7537412852729,18.5749225972442,
-19.0720791410119));
#101642=CARTESIAN_POINT('Ctrl Pts',(-20.7670007520343,18.6205790127139,
-19.074956446327));
#101643=CARTESIAN_POINT('Ctrl Pts',(-20.7921933233439,18.7073247712844,
-19.0804232362541));
#101644=CARTESIAN_POINT('Ctrl Pts',(-20.8118478930289,18.7957464915235,
-19.0858900261812));
#101645=CARTESIAN_POINT('Ctrl Pts',(-20.8257819138173,18.8852126076307,
-19.0913568161083));
#101646=CARTESIAN_POINT('Ctrl Pts',(-20.8394880731084,18.9732156942584,
-19.0967342082257));
#101647=CARTESIAN_POINT('Ctrl Pts',(-20.847659220755,19.0622293912709,-19.1021116003431));
#101648=CARTESIAN_POINT('Ctrl Pts',(-20.8501673751634,19.1516313189109,
-19.1074889924605));
#101649=CARTESIAN_POINT('Ctrl Pts',(-20.8507044999982,19.170776868907,-19.1086405686328));
#101650=CARTESIAN_POINT('Ctrl Pts',(-20.8509820862726,19.1899401417876,
-19.1097921448052));
#101651=CARTESIAN_POINT('Ctrl Pts',(-20.8509991606888,19.2091148891276,
-19.1109437209775));
#101652=CARTESIAN_POINT('Ctrl Pts',(-20.8499620916056,19.2091158126,-19.1109437209775));
#101653=CARTESIAN_POINT('Ctrl Pts',(-20.8456332387307,19.7149949859819,
-19.1413398983212));
#101654=CARTESIAN_POINT('Ctrl Pts',(-20.4101935795872,20.9330881089954,
-19.2141280112252));
#101655=CARTESIAN_POINT('Ctrl Pts',(-18.3741968251019,21.6882711019051,
-19.3293080596899));
#101656=CARTESIAN_POINT('Ctrl Pts',(-16.4562524007973,20.2493623486038,
-19.4564838663713));
#101657=CARTESIAN_POINT('Ctrl Pts',(-16.6280000239014,17.8578205442182,
-19.5836596730528));
#101658=CARTESIAN_POINT('Ctrl Pts',(-18.7318719156386,16.7077369880416,
-19.7108354797341));
#101659=CARTESIAN_POINT('Ctrl Pts',(-20.2929105236617,17.5576360808446,
-19.805110366326));
#101660=CARTESIAN_POINT('Ctrl Pts',(-20.670180515561,18.3361167516014,-19.8569933173575));
#101661=CARTESIAN_POINT('Ctrl Pts',(-20.7227695130846,18.4848207703082,
-19.8664843328284));
#101662=CARTESIAN_POINT('Ctrl Pts',(-20.7225806138715,18.48488971765,-19.6425236773711));
#101663=CARTESIAN_POINT('Ctrl Pts',(-20.7166172131094,18.4685578966628,
-19.6415015055718));
#101664=CARTESIAN_POINT('Ctrl Pts',(-20.7104526312527,18.4522995775035,
-19.6404859043171));
#101665=CARTESIAN_POINT('Ctrl Pts',(-20.6487986673468,18.2955482034438,
-19.6307079256196));
#101666=CARTESIAN_POINT('Ctrl Pts',(-20.5786228568079,18.1612956446388,
-19.6224835837011));
#101667=CARTESIAN_POINT('Ctrl Pts',(-20.4575557776264,17.9799307339345,
-19.6106418681866));
#101668=CARTESIAN_POINT('Ctrl Pts',(-20.4177432745747,17.9260159116697,
-19.6070082161425));
#101669=CARTESIAN_POINT('Ctrl Pts',(-20.3413736183221,17.8322507236163,
-19.6003215113211));
#101670=CARTESIAN_POINT('Ctrl Pts',(-20.3057195639882,17.7917409230834,
-19.5972951937388));
#101671=CARTESIAN_POINT('Ctrl Pts',(-20.2493176315369,17.7323919628987,
-19.5925699520392));
#101672=CARTESIAN_POINT('Ctrl Pts',(-20.2296773196887,17.712527965864,-19.5909350015854));
#101673=CARTESIAN_POINT('Ctrl Pts',(-20.2047675548798,17.688312184712,-19.588865181943));
#101674=CARTESIAN_POINT('Ctrl Pts',(-20.1998614349834,17.683588583954,-19.5884576962871));
#101675=CARTESIAN_POINT('Ctrl Pts',(-20.1919761559026,17.6760696375325,
-19.5878028856512));
#101676=CARTESIAN_POINT('Ctrl Pts',(-20.1890115022321,17.673259054155,-19.5875567198869));
#101677=CARTESIAN_POINT('Ctrl Pts',(-20.1834366917092,17.6680045163247,
-19.5870938286371));
#101678=CARTESIAN_POINT('Ctrl Pts',(-20.1808284717707,17.6655585878109,
-19.5868772593599));
#101679=CARTESIAN_POINT('Ctrl Pts',(-20.1748364833881,17.6599679024864,
-19.5863797305478));
#101680=CARTESIAN_POINT('Ctrl Pts',(-20.1714486197794,17.6568276144712,
-19.5860984361602));
#101681=CARTESIAN_POINT('Ctrl Pts',(-20.1609189938946,17.647131344696,-19.5852242629529));
#101682=CARTESIAN_POINT('Ctrl Pts',(-20.1537425733231,17.6406134222842,
-19.584628618581));
#101683=CARTESIAN_POINT('Ctrl Pts',(-20.0721348493485,17.5675105048281,
-19.5778593740185));
#101684=CARTESIAN_POINT('Ctrl Pts',(-19.9931343333311,17.5062306342215,
-19.571351026869));
#101685=CARTESIAN_POINT('Ctrl Pts',(-19.7683195062158,17.3560189856748,
-19.5535366215855));
#101686=CARTESIAN_POINT('Ctrl Pts',(-19.6155670518583,17.2787399673944,
-19.5422128321443));
#101687=CARTESIAN_POINT('Ctrl Pts',(-19.427543704499,17.2106124556297,-19.5296790850231));
#101688=CARTESIAN_POINT('Ctrl Pts',(-19.3996982400038,17.2011743396427,
-19.5278545919433));
#101689=CARTESIAN_POINT('Ctrl Pts',(-19.3513391404719,17.1858985926629,
-19.524739673399));
#101690=CARTESIAN_POINT('Ctrl Pts',(-19.3309178131635,17.1797854616425,
-19.5234405163735));
#101691=CARTESIAN_POINT('Ctrl Pts',(-19.3017501179458,17.1715319942469,
-19.5216073163191));
#101692=CARTESIAN_POINT('Ctrl Pts',(-19.293077565758,17.16913756039,-19.5210650318227));
#101693=CARTESIAN_POINT('Ctrl Pts',(-19.278090262191,17.1651023121824,-19.520132620291));
#101694=CARTESIAN_POINT('Ctrl Pts',(-19.2717827567293,17.1634352829587,
-19.519741646839));
#101695=CARTESIAN_POINT('Ctrl Pts',(-19.259691302829,17.1602993236621,-19.5189948665447));
#101696=CARTESIAN_POINT('Ctrl Pts',(-19.2539086617314,17.1588256423046,
-19.5186389091404));
#101697=CARTESIAN_POINT('Ctrl Pts',(-19.2388562878887,17.1550573160074,
-19.5177153766906));
#101698=CARTESIAN_POINT('Ctrl Pts',(-19.2295770566492,17.1528008899165,
-19.5171490387924));
#101699=CARTESIAN_POINT('Ctrl Pts',(-19.1978869943889,17.1453215725636,
-19.5152248176217));
#101700=CARTESIAN_POINT('Ctrl Pts',(-19.1754059279767,17.1404012032832,
-19.5138766425967));
#101701=CARTESIAN_POINT('Ctrl Pts',(-18.981100328157,17.1011825799175,-19.5023583755693));
#101702=CARTESIAN_POINT('Ctrl Pts',(-18.8057153303756,17.0879710926004,
-19.4929364677679));
#101703=CARTESIAN_POINT('Ctrl Pts',(-18.543606155358,17.100776917375,-19.4786584615024));
#101704=CARTESIAN_POINT('Ctrl Pts',(-18.4568716572268,17.1104075240527,
-19.4738857159276));
#101705=CARTESIAN_POINT('Ctrl Pts',(-18.3336761093493,17.1318501841942,
-19.4667465262771));
#101706=CARTESIAN_POINT('Ctrl Pts',(-18.2965500849234,17.1393435745284,
-19.4645468137002));
#101707=CARTESIAN_POINT('Ctrl Pts',(-18.2522658486713,17.1495251446863,
-19.4618432947216));
#101708=CARTESIAN_POINT('Ctrl Pts',(-18.2448933202246,17.1512619041448,
-19.4613905333992));
#101709=CARTESIAN_POINT('Ctrl Pts',(-18.2334641924935,17.154019105174,-19.4606842684048));
#101710=CARTESIAN_POINT('Ctrl Pts',(-18.2294009441658,17.1550120894247,
-19.4604323175444));
#101711=CARTESIAN_POINT('Ctrl Pts',(-18.2218813668174,17.1568733715334,
-19.4599644071962));
#101712=CARTESIAN_POINT('Ctrl Pts',(-18.218424277394,17.1577383571726,-19.4597486397965));
#101713=CARTESIAN_POINT('Ctrl Pts',(-18.2106267385444,17.1597102852452,
-19.4592605129146));
#101714=CARTESIAN_POINT('Ctrl Pts',(-18.2062876338038,17.1608222705395,
-19.4589878666401));
#101715=CARTESIAN_POINT('Ctrl Pts',(-18.1935291856974,17.1641350732742,
-19.4581832634119));
#101716=CARTESIAN_POINT('Ctrl Pts',(-18.185119964687,17.1663740121364,-19.457649180118));
#101717=CARTESIAN_POINT('Ctrl Pts',(-18.1255636510094,17.1826246479992,
-19.45384111562));
#101718=CARTESIAN_POINT('Ctrl Pts',(-18.0749494120633,17.1985008914827,
-19.450471193311));
#101719=CARTESIAN_POINT('Ctrl Pts',(-18.0111255607433,17.2211864322055,
-19.4460944167734));
#101720=CARTESIAN_POINT('Ctrl Pts',(-17.9973136798349,17.2262585204482,
-19.4451394507847));
#101721=CARTESIAN_POINT('Ctrl Pts',(-17.8512337501419,17.2816378419006,
-19.4349634651908));
#101722=CARTESIAN_POINT('Ctrl Pts',(-17.7242725277974,17.34494304558,-19.4254871326029));
#101723=CARTESIAN_POINT('Ctrl Pts',(-17.5184301558905,17.4747823698172,
-19.4096959386094));
#101724=CARTESIAN_POINT('Ctrl Pts',(-17.4363125358383,17.5352690422902,
-19.4032524952369));
#101725=CARTESIAN_POINT('Ctrl Pts',(-17.3476244041252,17.6110406117418,
-19.3961392173745));
#101726=CARTESIAN_POINT('Ctrl Pts',(-17.3364906027865,17.6207563586093,
-19.3952430114356));
#101727=CARTESIAN_POINT('Ctrl Pts',(-17.3196645239569,17.6357525871239,
-19.393883415819));
#101728=CARTESIAN_POINT('Ctrl Pts',(-17.3138982253714,17.6409489808396,
-19.3934165329491));
#101729=CARTESIAN_POINT('Ctrl Pts',(-17.3034586776592,17.6504613147828,
-19.392569479121));
#101730=CARTESIAN_POINT('Ctrl Pts',(-17.2987760730753,17.6547668092685,
-19.3921888736617));
#101731=CARTESIAN_POINT('Ctrl Pts',(-17.2887080652307,17.6641080894601,
-19.3913690599734));
#101732=CARTESIAN_POINT('Ctrl Pts',(-17.2833294074414,17.6691510470874,
-19.390930164901));
#101733=CARTESIAN_POINT('Ctrl Pts',(-17.2688148935935,17.6829028475961,
-19.3897431864966));
#101734=CARTESIAN_POINT('Ctrl Pts',(-17.2597303057014,17.6916655463418,
-19.3889974350811));
#101735=CARTESIAN_POINT('Ctrl Pts',(-17.2159014219187,17.7347047404359,
-19.3853847861468));
#101736=CARTESIAN_POINT('Ctrl Pts',(-17.1822695630136,17.770096055695,-19.3825674146219));
#101737=CARTESIAN_POINT('Ctrl Pts',(-17.1228467552732,17.8371237459432,
-19.3774772542927));
#101738=CARTESIAN_POINT('Ctrl Pts',(-17.0966901564294,17.8684027185722,
-19.3751922462857));
#101739=CARTESIAN_POINT('Ctrl Pts',(-16.9982921795763,17.9932262243659,
-19.3663721453531));
#101740=CARTESIAN_POINT('Ctrl Pts',(-16.9330325132811,18.0919954830018,
-19.3600340072474));
#101741=CARTESIAN_POINT('Ctrl Pts',(-16.8405341843086,18.261234394413,-19.3494988692561));
#101742=CARTESIAN_POINT('Ctrl Pts',(-16.8082096184992,18.3286184553558,
-19.345375939591));
#101743=CARTESIAN_POINT('Ctrl Pts',(-16.7662504132167,18.4294359442087,
-19.3391195568939));
#101744=CARTESIAN_POINT('Ctrl Pts',(-16.7537679116808,18.4616260101356,
-19.3371091840047));
#101745=CARTESIAN_POINT('Ctrl Pts',(-16.7395821609449,18.5010416645928,
-19.3346157121536));
#101746=CARTESIAN_POINT('Ctrl Pts',(-16.7371218303058,18.5079915174602,
-19.3341748709852));
#101747=CARTESIAN_POINT('Ctrl Pts',(-16.7333370813812,18.518862718646,-19.3334832342328));
#101748=CARTESIAN_POINT('Ctrl Pts',(-16.731987748799,18.5227754178003,-19.3332338897752));
#101749=CARTESIAN_POINT('Ctrl Pts',(-16.7294965297472,18.5300686015429,
-19.3327683021498));
#101750=CARTESIAN_POINT('Ctrl Pts',(-16.7283517127724,18.5334480248905,
-19.332552235105));
#101751=CARTESIAN_POINT('Ctrl Pts',(-16.7257700044639,18.5411329334869,
-19.332060152502));
#101752=CARTESIAN_POINT('Ctrl Pts',(-16.7243384192817,18.5454401365259,
-19.3317838296685));
#101753=CARTESIAN_POINT('Ctrl Pts',(-16.7201156087495,18.5582831319594,
-19.3309584204669));
#101754=CARTESIAN_POINT('Ctrl Pts',(-16.7173648764901,18.5668319914621,
-19.3304070436378));
#101755=CARTESIAN_POINT('Ctrl Pts',(-16.6965145515918,18.633074244889,-19.3261209845785));
#101756=CARTESIAN_POINT('Ctrl Pts',(-16.6808415129951,18.6914964684959,
-19.3222617998779));
#101757=CARTESIAN_POINT('Ctrl Pts',(-16.6546073646064,18.8092124193351,
-19.314433419105));
#101758=CARTESIAN_POINT('Ctrl Pts',(-16.644031920348,18.8684508559508,-19.3104683957893));
#101759=CARTESIAN_POINT('Ctrl Pts',(-16.6214469210267,19.0359172690096,
-19.2993046531377));
#101760=CARTESIAN_POINT('Ctrl Pts',(-16.6152389138853,19.1447473494696,
-19.2921113262475));
#101761=CARTESIAN_POINT('Ctrl Pts',(-16.6189332628197,19.3283941239019,
-19.2803108674788));
#101762=CARTESIAN_POINT('Ctrl Pts',(-16.6244041523391,19.4030837634912,
-19.275603303176));
#101763=CARTESIAN_POINT('Ctrl Pts',(-16.6361829230597,19.4959652699098,
-19.2698679418007));
#101764=CARTESIAN_POINT('Ctrl Pts',(-16.638793470919,19.5145643746092,-19.268725302349));
#101765=CARTESIAN_POINT('Ctrl Pts',(-16.6429521100254,19.5415764842162,
-19.2670738846304));
#101766=CARTESIAN_POINT('Ctrl Pts',(-16.6443041714466,19.5500183439875,
-19.2665589317755));
#101767=CARTESIAN_POINT('Ctrl Pts',(-16.6467656960257,19.5648128637118,
-19.2656584203537));
#101768=CARTESIAN_POINT('Ctrl Pts',(-16.6478531088453,19.5711690327715,
-19.2652721675857));
#101769=CARTESIAN_POINT('Ctrl Pts',(-16.6500220358079,19.5835074492661,
-19.2645235809914));
#101770=CARTESIAN_POINT('Ctrl Pts',(-16.6511003077451,19.589490195629,-19.2641611482747));
#101771=CARTESIAN_POINT('Ctrl Pts',(-16.6537413168854,19.6037905732882,
-19.2632961065535));
#101772=CARTESIAN_POINT('Ctrl Pts',(-16.6553281975708,19.6121036824611,
-19.2627942698272));
#101773=CARTESIAN_POINT('Ctrl Pts',(-16.6612452408737,19.6421224712256,
-19.2609856718521));
#101774=CARTESIAN_POINT('Ctrl Pts',(-16.6658659759476,19.6637699081349,
-19.2596881687402));
#101775=CARTESIAN_POINT('Ctrl Pts',(-16.7123527334063,19.8659666151263,
-19.2476219094418));
#101776=CARTESIAN_POINT('Ctrl Pts',(-16.7774160942318,20.0403517913336,
-19.237707022582));
#101777=CARTESIAN_POINT('Ctrl Pts',(-16.9020317915031,20.2749691408593,
-19.2232256316142));
#101778=CARTESIAN_POINT('Ctrl Pts',(-16.9437034448167,20.3436844567665,
-19.2188098913474));
#101779=CARTESIAN_POINT('Ctrl Pts',(-17.0096018150903,20.4395931918922,
-19.2121539441067));
#101780=CARTESIAN_POINT('Ctrl Pts',(-17.0307858376637,20.4687962866522,
-19.2100557258158));
#101781=CARTESIAN_POINT('Ctrl Pts',(-17.0572426813734,20.5033736607171,
-19.2074647488007));
#101782=CARTESIAN_POINT('Ctrl Pts',(-17.0618126072333,20.5092812115193,
-19.2070182178698));
#101783=CARTESIAN_POINT('Ctrl Pts',(-17.068976302196,20.5184411614074,-19.2063195966805));
#101784=CARTESIAN_POINT('Ctrl Pts',(-17.071548611285,20.5217103739068,-19.2060690057086));
#101785=CARTESIAN_POINT('Ctrl Pts',(-17.0763437521366,20.5277678152197,
-19.2056023188159));
#101786=CARTESIAN_POINT('Ctrl Pts',(-17.0785639988411,20.5305580171941,
-19.2053864066902));
#101787=CARTESIAN_POINT('Ctrl Pts',(-17.0836082195718,20.5368643629984,
-19.2048962686192));
#101788=CARTESIAN_POINT('Ctrl Pts',(-17.0864363717232,20.540377082653,-19.2046217454134));
#101789=CARTESIAN_POINT('Ctrl Pts',(-17.0937669457726,20.5494227333948,
-19.2039109697467));
#101790=CARTESIAN_POINT('Ctrl Pts',(-17.0982861059209,20.5549419402853,
-19.2034735515306));
#101791=CARTESIAN_POINT('Ctrl Pts',(-17.1261965426133,20.5886793773029,
-19.20077725352));
#101792=CARTESIAN_POINT('Ctrl Pts',(-17.1502880085899,20.6163072188492,
-19.1984722199439));
#101793=CARTESIAN_POINT('Ctrl Pts',(-17.2905010253499,20.7689159230848,
-19.1852467127015));
#101794=CARTESIAN_POINT('Ctrl Pts',(-17.4206787319678,20.8801260208167,
-19.1737355294254));
#101795=CARTESIAN_POINT('Ctrl Pts',(-17.642208916033,21.0272514777714,-19.1564537798313));
#101796=CARTESIAN_POINT('Ctrl Pts',(-17.7251024988708,21.0745737921114,
-19.1503970165453));
#101797=CARTESIAN_POINT('Ctrl Pts',(-17.830159968478,21.1254763065328,-19.1432262657578));
#101798=CARTESIAN_POINT('Ctrl Pts',(-17.84954595053,21.1345091416212,-19.1419227555922));
#101799=CARTESIAN_POINT('Ctrl Pts',(-17.8772885830223,21.1469276084966,
-19.1400845366582));
#101800=CARTESIAN_POINT('Ctrl Pts',(-17.885534623554,21.1505557909514,-19.1395415249103));
#101801=CARTESIAN_POINT('Ctrl Pts',(-17.8997938349771,21.1567213739146,
-19.1386082557128));
#101802=CARTESIAN_POINT('Ctrl Pts',(-17.905795992482,21.1592837868447,-19.1382171477241));
#101803=CARTESIAN_POINT('Ctrl Pts',(-17.917306638786,21.1641350526862,-19.137470377294));
#101804=CARTESIAN_POINT('Ctrl Pts',(-17.9228131309953,21.166428455597,-19.1371145630072));
#101805=CARTESIAN_POINT('Ctrl Pts',(-17.937147490831,21.172327613964,-19.1361919781533));
#101806=CARTESIAN_POINT('Ctrl Pts',(-17.9459902214585,21.1758970772313,
-19.1356264396111));
#101807=CARTESIAN_POINT('Ctrl Pts',(-17.9761755332288,21.1878451557532,
-19.1337078903903));
#101808=CARTESIAN_POINT('Ctrl Pts',(-17.9976304466896,21.195936934427,-19.1323645092174));
#101809=CARTESIAN_POINT('Ctrl Pts',(-18.1851818948047,21.2632128522568,
-19.1207855173296));
#101810=CARTESIAN_POINT('Ctrl Pts',(-18.3579352619381,21.301779968253,-19.1113092300231));
#101811=CARTESIAN_POINT('Ctrl Pts',(-18.6195106265435,21.3266674229788,
-19.0970104506064));
#101812=CARTESIAN_POINT('Ctrl Pts',(-18.7059505313282,21.3295767221752,
-19.0922778542927));
#101813=CARTESIAN_POINT('Ctrl Pts',(-18.8299777535521,21.3261587560286,
-19.0851928046099));
#101814=CARTESIAN_POINT('Ctrl Pts',(-18.8675999548003,21.3241159337922,
-19.0830042089902));
#101815=CARTESIAN_POINT('Ctrl Pts',(-18.912683301989,21.3204592858548,-19.0803130120171));
#101816=CARTESIAN_POINT('Ctrl Pts',(-18.9202182271931,21.3198074755743,
-19.079860915993));
#101817=CARTESIAN_POINT('Ctrl Pts',(-18.9319122328687,21.3187327211717,
-19.0791554669945));
#101818=CARTESIAN_POINT('Ctrl Pts',(-18.9360739134314,21.3183378012635,
-19.0789036610764));
#101819=CARTESIAN_POINT('Ctrl Pts',(-18.943781348226,21.317583368309,-19.0784358822704));
#101820=CARTESIAN_POINT('Ctrl Pts',(-18.9473273745515,21.3172272271488,
-19.0782201005901));
#101821=CARTESIAN_POINT('Ctrl Pts',(-18.9553314382059,21.3164029276073,
-19.077731764547));
#101822=CARTESIAN_POINT('Ctrl Pts',(-18.9597888723646,21.3159295658945,
-19.0774589222978));
#101823=CARTESIAN_POINT('Ctrl Pts',(-18.9729100098262,21.3144939964824,
-19.0766532163828));
#101824=CARTESIAN_POINT('Ctrl Pts',(-18.981569189485,21.3134924438504,-19.076118217829));
#101825=CARTESIAN_POINT('Ctrl Pts',(-19.0431301354751,21.3059865082933,
-19.0722925744649));
#101826=CARTESIAN_POINT('Ctrl Pts',(-19.0957714001299,21.2975402777894,
-19.0689050266426));
#101827=CARTESIAN_POINT('Ctrl Pts',(-19.1656342010236,21.2836077891774,
-19.0643010877012));
#101828=CARTESIAN_POINT('Ctrl Pts',(-19.1831899234458,21.2798739735191,
-19.0631348875672));
#101829=CARTESIAN_POINT('Ctrl Pts',(-19.2477379940259,21.2652853487951,
-19.0588173024872));
#101830=CARTESIAN_POINT('Ctrl Pts',(-19.294402090412,21.2530490407273,-19.0556378676121));
#101831=CARTESIAN_POINT('Ctrl Pts',(-19.4453994711384,21.2078885063341,
-19.0452268413031));
#101832=CARTESIAN_POINT('Ctrl Pts',(-19.5476142114292,21.168469870797,-19.0379942682635));
#101833=CARTESIAN_POINT('Ctrl Pts',(-19.7146192688719,21.088711887975,-19.026098281523));
#101834=CARTESIAN_POINT('Ctrl Pts',(-19.7811164761318,21.0524574037317,
-19.0213354801221));
#101835=CARTESIAN_POINT('Ctrl Pts',(-19.8616162830218,21.0027944978295,
-19.0155405260873));
#101836=CARTESIAN_POINT('Ctrl Pts',(-19.8775637273199,20.9926587894657,
-19.0143908295255));
#101837=CARTESIAN_POINT('Ctrl Pts',(-19.9005445890706,20.9776171548102,
-19.0127311581586));
#101838=CARTESIAN_POINT('Ctrl Pts',(-19.9076869362773,20.9728800835885,
-19.0122149216488));
#101839=CARTESIAN_POINT('Ctrl Pts',(-19.9201552672233,20.9645011566095,
-19.0113129290612));
#101840=CARTESIAN_POINT('Ctrl Pts',(-19.9254936984965,20.9608781077735,
-19.0109264717404));
#101841=CARTESIAN_POINT('Ctrl Pts',(-19.9358248169164,20.9537974608059,
-19.0101780419633));
#101842=CARTESIAN_POINT('Ctrl Pts',(-19.9408193472458,20.9503426759105,
-19.0098159680157));
#101843=CARTESIAN_POINT('Ctrl Pts',(-19.9527191909723,20.9420354592015,
-19.0089526617102));
#101844=CARTESIAN_POINT('Ctrl Pts',(-19.9596105233162,20.9371631080892,
-19.0084521945275));
#101845=CARTESIAN_POINT('Ctrl Pts',(-19.9843471523556,20.9194508498627,
-19.0066536997101));
#101846=CARTESIAN_POINT('Ctrl Pts',(-20.0020217117558,20.9063740884316,
-19.0053647936434));
#101847=CARTESIAN_POINT('Ctrl Pts',(-20.167906501024,20.7795963401822,-18.9932204252046));
#101848=CARTESIAN_POINT('Ctrl Pts',(-20.3006547512269,20.6470296389423,
-18.9832348745875));
#101849=CARTESIAN_POINT('Ctrl Pts',(-20.4625580244662,20.4357743235519,
-18.9687215007074));
#101850=CARTESIAN_POINT('Ctrl Pts',(-20.5072417379585,20.3701362141873,
-18.9643555763264));
#101851=CARTESIAN_POINT('Ctrl Pts',(-20.5665927326588,20.2714600875568,
-18.9577673965023));
#101852=CARTESIAN_POINT('Ctrl Pts',(-20.5842696339808,20.2403073689867,
-18.9556838237881));
#101853=CARTESIAN_POINT('Ctrl Pts',(-20.6046593330345,20.202149943009,-18.9531090958991));
#101854=CARTESIAN_POINT('Ctrl Pts',(-20.6081371499621,20.1955580171731,
-18.9526634938179));
#101855=CARTESIAN_POINT('Ctrl Pts',(-20.6135001090306,20.1852615749484,
-18.951966012591));
#101856=CARTESIAN_POINT('Ctrl Pts',(-20.6154093115193,20.1815695637682,
-18.9517156248228));
#101857=CARTESIAN_POINT('Ctrl Pts',(-20.6189363572698,20.1746994587619,
-18.9512491186223));
#101858=CARTESIAN_POINT('Ctrl Pts',(-20.6205570474101,20.1715228909476,
-18.9510331827391));
#101859=CARTESIAN_POINT('Ctrl Pts',(-20.6242112024594,20.1643157872284,
-18.9505427344713));
#101860=CARTESIAN_POINT('Ctrl Pts',(-20.6262397957424,20.1602828527987,
-18.9502679232218));
#101861=CARTESIAN_POINT('Ctrl Pts',(-20.6322139864624,20.148310653789,-18.9494510988611));
#101862=CARTESIAN_POINT('Ctrl Pts',(-20.6361225704899,20.1403531732521,
-18.9489068637317));
#101863=CARTESIAN_POINT('Ctrl Pts',(-20.664856928934,20.0809122872286,-18.9448330223966));
#101864=CARTESIAN_POINT('Ctrl Pts',(-20.6876363959591,20.0284713799653,
-18.9411920729833));
#101865=CARTESIAN_POINT('Ctrl Pts',(-20.7683687191834,19.8198984997821,
-18.9267030292914));
#101866=CARTESIAN_POINT('Ctrl Pts',(-20.8099462681566,19.6580661827971,
-18.9155001930197));
#101867=CARTESIAN_POINT('Ctrl Pts',(-20.8399080762695,19.4351614982078,
-18.901006237287));
#101868=CARTESIAN_POINT('Ctrl Pts',(-20.8452891073375,19.3770014254749,
-18.8973012028165));
#101869=CARTESIAN_POINT('Ctrl Pts',(-20.8500786761297,19.2829677171489,
-18.8914415141523));
#101870=CARTESIAN_POINT('Ctrl Pts',(-20.8509926290775,19.2472045485215,
-18.8892430074392));
#101871=CARTESIAN_POINT('Ctrl Pts',(-20.8510022031418,19.2004601928484,
-18.8864069215302));
#101872=CARTESIAN_POINT('Ctrl Pts',(-20.8509191302474,19.1894867776335,
-18.8857438248984));
#101873=CARTESIAN_POINT('Ctrl Pts',(-20.8506443290511,19.1715808574569,
-18.8846660756149));
#101874=CARTESIAN_POINT('Ctrl Pts',(-20.8505038546913,19.1646478764242,
-18.8842498251253));
#101875=CARTESIAN_POINT('Ctrl Pts',(-20.8501671509485,19.1512747950672,
-18.8834488851803));
#101876=CARTESIAN_POINT('Ctrl Pts',(-20.8499755812812,19.1448346639406,
-18.8830640542783));
#101877=CARTESIAN_POINT('Ctrl Pts',(-20.84946265105,19.129887466604,-18.8821728824703));
#101878=CARTESIAN_POINT('Ctrl Pts',(-20.8491193700894,19.1213812264981,
-18.8816672336651));
#101879=CARTESIAN_POINT('Ctrl Pts',(-20.847863432152,19.0943134819767,-18.8800628357042));
#101880=CARTESIAN_POINT('Ctrl Pts',(-20.8467576609092,19.0757614989822,
-18.8789701371894));
#101881=CARTESIAN_POINT('Ctrl Pts',(-20.8436139219907,19.0325961004741,
-18.876442454687));
#101882=CARTESIAN_POINT('Ctrl Pts',(-20.8413892428455,19.0079987641029,
-18.8750132736541));
#101883=CARTESIAN_POINT('Ctrl Pts',(-20.8320826211675,18.9219185224895,
-18.8700446756409));
#101884=CARTESIAN_POINT('Ctrl Pts',(-20.8227356710758,18.8607101995958,
-18.8665718396773));
#101885=CARTESIAN_POINT('Ctrl Pts',(-20.7895029368918,18.6927921155633,
-18.8571028374997));
#101886=CARTESIAN_POINT('Ctrl Pts',(-20.7600278787111,18.5874456537938,
-18.8512348473893));
#101887=CARTESIAN_POINT('Ctrl Pts',(-20.7225806605155,18.4848898453927,
-18.8452754875981));
#101888=CARTESIAN_POINT('Origin',(-18.734,19.211,0.));
#101889=CARTESIAN_POINT('',(-20.7225806765445,18.484889889291,-18.0457834329553));
#101890=CARTESIAN_POINT('',(-20.7225806130935,18.4848897155193,-18.2676549617288));
#101891=CARTESIAN_POINT('',(-20.7225806137986,18.4848897174502,0.));
#101892=CARTESIAN_POINT('',(-20.8509999976816,19.2110990761722,-18.3109437209775));
#101893=CARTESIAN_POINT('Ctrl Pts',(-20.7225806130935,18.4848897155193,
-18.2676549617288));
#101894=CARTESIAN_POINT('Ctrl Pts',(-20.7253379764187,18.4924412395355,
-18.268103955216));
#101895=CARTESIAN_POINT('Ctrl Pts',(-20.7280524567443,18.5000088307141,
-18.2685519707272));
#101896=CARTESIAN_POINT('Ctrl Pts',(-20.7645972677333,18.6037465066057,
-18.2746683362838));
#101897=CARTESIAN_POINT('Ctrl Pts',(-20.7914816982396,18.70222490975,-18.2801721418135));
#101898=CARTESIAN_POINT('Ctrl Pts',(-20.8346080680977,18.9213865413653,
-18.2923170310514));
#101899=CARTESIAN_POINT('Ctrl Pts',(-20.8477551444556,19.0422954410914,
-18.2989530517298));
#101900=CARTESIAN_POINT('Ctrl Pts',(-20.85072784998,19.1751560966423,-18.3067847632183));
#101901=CARTESIAN_POINT('Ctrl Pts',(-20.8508914867126,19.1866690186424,
-18.3074678984705));
#101902=CARTESIAN_POINT('Ctrl Pts',(-20.8509827720571,19.2017457699954,
-18.3083690347001));
#101903=CARTESIAN_POINT('Ctrl Pts',(-20.8509953499484,19.205309144036,-18.308582495384));
#101904=CARTESIAN_POINT('Ctrl Pts',(-20.8509997172436,19.2096548902916,
-18.3088434247664));
#101905=CARTESIAN_POINT('Ctrl Pts',(-20.8510000697841,19.2104372756591,
-18.3088904248973));
#101906=CARTESIAN_POINT('Ctrl Pts',(-20.8509999886041,19.2112196594398,
-18.3089374488649));
#101907=CARTESIAN_POINT('Ctrl Pts',(-20.8509999976816,19.2110990761722,
-18.3109437209775));
#101908=CARTESIAN_POINT('Ctrl Pts',(-20.8509997507685,19.2163749670545,
-18.3112630160645));
#101909=CARTESIAN_POINT('Ctrl Pts',(-20.8509797813958,19.2216508039048,
-18.3115823111514));
#101910=CARTESIAN_POINT('Ctrl Pts',(-20.8509400905189,19.2269264921969,
-18.3119016062384));
#101911=CARTESIAN_POINT('Ctrl Pts',(-20.8503946018242,19.2994325325996,
-18.3162898151688));
#101912=CARTESIAN_POINT('Ctrl Pts',(-20.8461186979221,19.3720520465351,
-18.3206780240992));
#101913=CARTESIAN_POINT('Ctrl Pts',(-20.8380978239802,19.4443695505457,
-18.3250662330295));
#101914=CARTESIAN_POINT('Ctrl Pts',(-20.8300888543451,19.51657972339,-18.3294479291303));
#101915=CARTESIAN_POINT('Ctrl Pts',(-20.8183460011053,19.5884883006379,
-18.333829625231));
#101916=CARTESIAN_POINT('Ctrl Pts',(-20.8029067175876,19.6596802802896,
-18.3382113213318));
#101917=CARTESIAN_POINT('Ctrl Pts',(-20.7874855764568,19.7307886036995,
-18.3425878685909));
#101918=CARTESIAN_POINT('Ctrl Pts',(-20.7683767353654,19.8011815331898,
-18.3469644158501));
#101919=CARTESIAN_POINT('Ctrl Pts',(-20.7456691798644,19.870451371053,-18.3513409631092));
#101920=CARTESIAN_POINT('Ctrl Pts',(-20.722976025165,19.9396772789918,-18.3557147348257));
#101921=CARTESIAN_POINT('Ctrl Pts',(-20.696688834233,20.0077810512473,-18.3600885065421));
#101922=CARTESIAN_POINT('Ctrl Pts',(-20.6669468334595,20.0743687155665,
-18.3644622782586));
#101923=CARTESIAN_POINT('Ctrl Pts',(-20.6372138832767,20.140936117036,-18.3688347190216));
#101924=CARTESIAN_POINT('Ctrl Pts',(-20.6040284070354,20.2059878863297,
-18.3732071597847));
#101925=CARTESIAN_POINT('Ctrl Pts',(-20.5675776766823,20.2691502273176,
-18.3775796005477));
#101926=CARTESIAN_POINT('Ctrl Pts',(-20.5311260142799,20.3323141833736,
-18.3819521531146));
#101927=CARTESIAN_POINT('Ctrl Pts',(-20.4914091748394,20.3935881984054,
-18.3863247056814));
#101928=CARTESIAN_POINT('Ctrl Pts',(-20.4486594348613,20.4526247510585,
-18.3906972582483));
#101929=CARTESIAN_POINT('Ctrl Pts',(-20.4058653275905,20.5117225740729,
-18.3950743488151));
#101930=CARTESIAN_POINT('Ctrl Pts',(-20.3600323187904,20.5685779068974,
-18.3994514393819));
#101931=CARTESIAN_POINT('Ctrl Pts',(-20.3114344316434,20.6228745035823,
-18.4038285299488));
#101932=CARTESIAN_POINT('Ctrl Pts',(-20.2628100033865,20.677200753654,-18.4082080110072));
#101933=CARTESIAN_POINT('Ctrl Pts',(-20.2114180304767,20.7289651427762,
-18.4125874920657));
#101934=CARTESIAN_POINT('Ctrl Pts',(-20.1575691237185,20.7778886208009,
-18.4169669731242));
#101935=CARTESIAN_POINT('Ctrl Pts',(-20.1036247701345,20.8268988153621,
-18.4213542167834));
#101936=CARTESIAN_POINT('Ctrl Pts',(-20.0472151597967,20.8730577373941,
-18.4257414604427));
#101937=CARTESIAN_POINT('Ctrl Pts',(-19.9886831896891,20.9161272953981,
-18.4301287041019));
#101938=CARTESIAN_POINT('Ctrl Pts',(-19.9488870900788,20.9454104447154,
-18.4331116070412));
#101939=CARTESIAN_POINT('Ctrl Pts',(-19.9081105258029,20.973266366868,-18.4360945099806));
#101940=CARTESIAN_POINT('Ctrl Pts',(-19.8664678605233,20.9996323112596,
-18.4390774129199));
#101941=CARTESIAN_POINT('Ctrl Pts',(-19.8052064921927,21.0384197860745,
-18.4434656218502));
#101942=CARTESIAN_POINT('Ctrl Pts',(-19.7418305075797,21.0741319931224,
-18.4478538307805));
#101943=CARTESIAN_POINT('Ctrl Pts',(-19.6766813842659,21.1065318007774,
-18.4522420397107));
#101944=CARTESIAN_POINT('Ctrl Pts',(-19.6116289530531,21.1388835217459,
-18.4566237358114));
#101945=CARTESIAN_POINT('Ctrl Pts',(-19.5448090356318,21.1679323895269,
-18.461005431912));
#101946=CARTESIAN_POINT('Ctrl Pts',(-19.4765908557838,21.1934852637299,
-18.4653871280127));
#101947=CARTESIAN_POINT('Ctrl Pts',(-19.4084528377262,21.2190081112721,
-18.4697636752717));
#101948=CARTESIAN_POINT('Ctrl Pts',(-19.3389202706957,21.2410429575789,
-18.4741402225307));
#101949=CARTESIAN_POINT('Ctrl Pts',(-19.2683841301352,21.2594439463797,
-18.4785167697897));
#101950=CARTESIAN_POINT('Ctrl Pts',(-19.1978927225701,21.2778332655408,
-18.482890541506));
#101951=CARTESIAN_POINT('Ctrl Pts',(-19.1263994698862,21.2925931782368,
-18.4872643132223));
#101952=CARTESIAN_POINT('Ctrl Pts',(-19.0543110010058,21.3036275021214,
-18.4916380849387));
#101953=CARTESIAN_POINT('Ctrl Pts',(-18.9822444688885,21.3146584682241,
-18.4960105257016));
#101954=CARTESIAN_POINT('Ctrl Pts',(-18.9095835567039,21.3219660233356,
-18.5003829664645));
#101955=CARTESIAN_POINT('Ctrl Pts',(-18.8367439345953,21.3255053047708,
-18.5047554072274));
#101956=CARTESIAN_POINT('Ctrl Pts',(-18.7639024499697,21.3290446767058,
-18.5091279597941));
#101957=CARTESIAN_POINT('Ctrl Pts',(-18.6908827282539,21.3288155622467,
-18.5135005123608));
#101958=CARTESIAN_POINT('Ctrl Pts',(-18.6181027067747,21.3248251624538,
-18.5178730649275));
#101959=CARTESIAN_POINT('Ctrl Pts',(-18.545247151444,21.3208306212736,-18.5222501554941));
#101960=CARTESIAN_POINT('Ctrl Pts',(-18.4726322757206,21.3130670274164,
-18.5266272460608));
#101961=CARTESIAN_POINT('Ctrl Pts',(-18.4006723159525,21.3015936130792,
-18.5310043366275));
#101962=CARTESIAN_POINT('Ctrl Pts',(-18.3286730561795,21.2901139326845,
-18.5353838176858));
#101963=CARTESIAN_POINT('Ctrl Pts',(-18.2573298966116,21.274920498468,-18.5397632987441));
#101964=CARTESIAN_POINT('Ctrl Pts',(-18.1870456019999,21.2561234404085,
-18.5441427798024));
#101965=CARTESIAN_POINT('Ctrl Pts',(-18.1166367289477,21.2372930646898,
-18.5485300234614));
#101966=CARTESIAN_POINT('Ctrl Pts',(-18.0472909281451,21.2148464584352,
-18.5529172671205));
#101967=CARTESIAN_POINT('Ctrl Pts',(-17.9793940004978,21.1889430693312,
-18.5573045107796));
#101968=CARTESIAN_POINT('Ctrl Pts',(-17.9332306321345,21.1713312607487,
-18.5602874137201));
#101969=CARTESIAN_POINT('Ctrl Pts',(-17.8877366290261,21.1521225055481,
-18.5632703166607));
#101970=CARTESIAN_POINT('Ctrl Pts',(-17.8430266573749,21.1313789997632,
-18.5662532196012));
#101971=CARTESIAN_POINT('Ctrl Pts',(-17.7772529124848,21.1008628082464,
-18.5706414285354));
#101972=CARTESIAN_POINT('Ctrl Pts',(-17.7129203794324,21.0669039749608,
-18.5750296374695));
#101973=CARTESIAN_POINT('Ctrl Pts',(-17.6504132837269,21.0296612736616,
-18.5794178464036));
#101974=CARTESIAN_POINT('Ctrl Pts',(-17.587998958915,20.992473846706,-18.5837995425081));
#101975=CARTESIAN_POINT('Ctrl Pts',(-17.5274051041887,20.9520124717683,
-18.5881812386125));
#101976=CARTESIAN_POINT('Ctrl Pts',(-17.4689939738821,20.9084830643884,
-18.592562934717));
#101977=CARTESIAN_POINT('Ctrl Pts',(-17.4106514813021,20.8650048075263,
-18.5969394819799));
#101978=CARTESIAN_POINT('Ctrl Pts',(-17.3544870028684,20.8184659667525,
-18.6013160292428));
#101979=CARTESIAN_POINT('Ctrl Pts',(-17.3008348082146,20.7691163413092,
-18.6056925765056));
#101980=CARTESIAN_POINT('Ctrl Pts',(-17.2472166390029,20.7197980126811,
-18.6100663482258));
#101981=CARTESIAN_POINT('Ctrl Pts',(-17.1961079465062,20.6676727619676,
-18.614440119946));
#101982=CARTESIAN_POINT('Ctrl Pts',(-17.1478097053802,20.6130304380626,
-18.6188138916662));
#101983=CARTESIAN_POINT('Ctrl Pts',(-17.0995261615713,20.5584047420004,
-18.6231863324329));
#101984=CARTESIAN_POINT('Ctrl Pts',(-17.0540516905116,20.5012638546118,
-18.6275587731997));
#101985=CARTESIAN_POINT('Ctrl Pts',(-17.0116490089849,20.4419330053863,
-18.6319312139665));
#101986=CARTESIAN_POINT('Ctrl Pts',(-16.9692452432171,20.3826006390646,
-18.636303766537));
#101987=CARTESIAN_POINT('Ctrl Pts',(-16.9299137017802,20.3210785933442,
-18.6406763191075));
#101988=CARTESIAN_POINT('Ctrl Pts',(-16.8938745512703,20.257722185175,-18.6450488716781));
#101989=CARTESIAN_POINT('Ctrl Pts',(-16.8577979979711,20.1943000233362,
-18.6494259622486));
#101990=CARTESIAN_POINT('Ctrl Pts',(-16.8250208968201,20.1290401182288,
-18.653803052819));
#101991=CARTESIAN_POINT('Ctrl Pts',(-16.7957176611923,20.0623228383323,
-18.6581801433895));
#101992=CARTESIAN_POINT('Ctrl Pts',(-16.76639842198,19.9955691216533,-18.6625596244516));
#101993=CARTESIAN_POINT('Ctrl Pts',(-16.7405569966209,19.9273568969086,
-18.6669391055137));
#101994=CARTESIAN_POINT('Ctrl Pts',(-16.718318792152,19.8580844367843,-18.6713185865757));
#101995=CARTESIAN_POINT('Ctrl Pts',(-16.6960411706153,19.7886891916906,
-18.6757058302385));
#101996=CARTESIAN_POINT('Ctrl Pts',(-16.6773796475306,19.7182304251215,
-18.6800930739013));
#101997=CARTESIAN_POINT('Ctrl Pts',(-16.66240897934,19.6471188405936,-18.6844803175641));
#101998=CARTESIAN_POINT('Ctrl Pts',(-16.6522303676452,19.5987698159082,
-18.6874632204703));
#101999=CARTESIAN_POINT('Ctrl Pts',(-16.6437568500118,19.5501192245646,
-18.6904461233765));
#102000=CARTESIAN_POINT('Ctrl Pts',(-16.6369981960583,19.5012971482211,
-18.6934290262827));
#102001=CARTESIAN_POINT('Ctrl Pts',(-16.6270554032346,19.4294740021261,
-18.6978172352092));
#102002=CARTESIAN_POINT('Ctrl Pts',(-16.6207874279489,19.3569992504147,
-18.7022054441356));
#102003=CARTESIAN_POINT('Ctrl Pts',(-16.6182687405808,19.2842819071561,
-18.7065936530621));
#102004=CARTESIAN_POINT('Ctrl Pts',(-16.6157537913624,19.2116724884915,
-18.7109753491589));
#102005=CARTESIAN_POINT('Ctrl Pts',(-16.6169771002007,19.1388216711239,
-18.7153570452558));
#102006=CARTESIAN_POINT('Ctrl Pts',(-16.6219616061144,19.0661455117954,
-18.7197387413526));
#102007=CARTESIAN_POINT('Ctrl Pts',(-16.6269402548369,18.9935547527373,
-18.7241152886079));
#102008=CARTESIAN_POINT('Ctrl Pts',(-16.635671288018,18.9211387228721,-18.7284918358631));
#102009=CARTESIAN_POINT('Ctrl Pts',(-16.6481255978396,18.8493137016531,
-18.7328683831184));
#102010=CARTESIAN_POINT('Ctrl Pts',(-16.6605720093189,18.7775342308183,
-18.737242154831));
#102011=CARTESIAN_POINT('Ctrl Pts',(-16.6767369302059,18.706345499076,-18.7416159265436));
#102012=CARTESIAN_POINT('Ctrl Pts',(-16.6965395553235,18.6361574681891,
-18.7459896982562));
#102013=CARTESIAN_POINT('Ctrl Pts',(-16.7163361544359,18.5659907957552,
-18.7503621390155));
#102014=CARTESIAN_POINT('Ctrl Pts',(-16.7397681292067,18.4968246835922,
-18.7547345797747));
#102015=CARTESIAN_POINT('Ctrl Pts',(-16.7667042167163,18.4290560754925,
-18.7591070205339));
#102016=CARTESIAN_POINT('Ctrl Pts',(-16.793640992985,18.3612857345413,-18.763479573097));
#102017=CARTESIAN_POINT('Ctrl Pts',(-16.8240818798548,18.2949134161282,
-18.7678521256601));
#102018=CARTESIAN_POINT('Ctrl Pts',(-16.8578472840042,18.2303165718431,
-18.7722246782231));
#102019=CARTESIAN_POINT('Ctrl Pts',(-16.8916477311643,18.1656526865152,
-18.7766017687863));
#102020=CARTESIAN_POINT('Ctrl Pts',(-16.9287793604438,18.1027683827113,
-18.7809788593494));
#102021=CARTESIAN_POINT('Ctrl Pts',(-16.9690167487982,18.0420162007209,
-18.7853559499125));
#102022=CARTESIAN_POINT('Ctrl Pts',(-17.0092761122842,17.9812308397084,
-18.7897354309673));
#102023=CARTESIAN_POINT('Ctrl Pts',(-17.0526443249076,17.922580307009,-18.7941149120221));
#102024=CARTESIAN_POINT('Ctrl Pts',(-17.0988543828187,17.866385627545,-18.7984943930769));
#102025=CARTESIAN_POINT('Ctrl Pts',(-17.1451463477484,17.8100913433872,
-18.8028816367326));
#102026=CARTESIAN_POINT('Ctrl Pts',(-17.1942898914324,17.756261961755,-18.8072688803883));
#102027=CARTESIAN_POINT('Ctrl Pts',(-17.2459801414532,17.7051826470085,
-18.811656124044));
#102028=CARTESIAN_POINT('Ctrl Pts',(-17.2811245310937,17.6704536344907,
-18.8146390270174));
#102029=CARTESIAN_POINT('Ctrl Pts',(-17.3174454256991,17.6369951039856,
-18.8176219299908));
#102030=CARTESIAN_POINT('Ctrl Pts',(-17.3548387352822,17.6048856809362,
-18.8206048329642));
#102031=CARTESIAN_POINT('Ctrl Pts',(-17.4098487897262,17.5576488589001,
-18.8249930418924));
#102032=CARTESIAN_POINT('Ctrl Pts',(-17.4673958504111,17.5131492751001,
-18.8293812508206));
#102033=CARTESIAN_POINT('Ctrl Pts',(-17.5271763106366,17.4716709388988,
-18.8337694597489));
#102034=CARTESIAN_POINT('Ctrl Pts',(-17.5868680467466,17.4302541634261,
-18.8381511558474));
#102035=CARTESIAN_POINT('Ctrl Pts',(-17.6487862091493,17.3918500068484,
-18.8425328519459));
#102036=CARTESIAN_POINT('Ctrl Pts',(-17.7125933764228,17.3567029608737,
-18.8469145480444));
#102037=CARTESIAN_POINT('Ctrl Pts',(-17.7763255651959,17.3215972154757,
-18.8512910953013));
#102038=CARTESIAN_POINT('Ctrl Pts',(-17.8419419289082,17.2897412091786,
-18.8556676425581));
#102039=CARTESIAN_POINT('Ctrl Pts',(-17.9090766869075,17.261335791087,-18.8600441898149));
#102040=CARTESIAN_POINT('Ctrl Pts',(-17.9761688690183,17.232948387299,-18.8644179615291));
#102041=CARTESIAN_POINT('Ctrl Pts',(-18.0447770916552,17.2080074173236,
-18.8687917332432));
#102042=CARTESIAN_POINT('Ctrl Pts',(-18.1145129035437,17.1866668413218,
-18.8731655049573));
#102043=CARTESIAN_POINT('Ctrl Pts',(-18.1842274945899,17.165332759329,-18.877537945718));
#102044=CARTESIAN_POINT('Ctrl Pts',(-18.255068532685,17.1475970372532,-18.8819103864787));
#102045=CARTESIAN_POINT('Ctrl Pts',(-18.3266312007886,17.1335641618984,
-18.8862828272393));
#102046=CARTESIAN_POINT('Ctrl Pts',(-18.3981956987569,17.1195309277215,
-18.8906553798038));
#102047=CARTESIAN_POINT('Ctrl Pts',(-18.4704813896214,17.1092008191085,
-18.8950279323682));
#102048=CARTESIAN_POINT('Ctrl Pts',(-18.5430736858689,17.1026271338844,
-18.8994004849326));
#102049=CARTESIAN_POINT('Ctrl Pts',(-18.6157413211391,17.0960466262419,
-18.903777575497));
#102050=CARTESIAN_POINT('Ctrl Pts',(-18.6887157156737,17.0932303693191,
-18.9081546660613));
#102051=CARTESIAN_POINT('Ctrl Pts',(-18.7615784216612,17.0941796413822,
-18.9125317566257));
#102052=CARTESIAN_POINT('Ctrl Pts',(-18.8344809206765,17.0951294318781,
-18.9169112376817));
#102053=CARTESIAN_POINT('Ctrl Pts',(-18.9072711279992,17.0998488145901,
-18.9212907187377));
#102054=CARTESIAN_POINT('Ctrl Pts',(-18.9795345883529,17.1082870462371,
-18.9256701997936));
#102055=CARTESIAN_POINT('Ctrl Pts',(-19.0519261352051,17.116740234593,-18.9300574434504));
#102056=CARTESIAN_POINT('Ctrl Pts',(-19.1237885946081,17.1289253543979,
-18.9344446871071));
#102057=CARTESIAN_POINT('Ctrl Pts',(-19.194717166806,17.1447404102557,-18.9388319307639));
#102058=CARTESIAN_POINT('Ctrl Pts',(-19.2429417616886,17.155493124404,-18.9418148337244));
#102059=CARTESIAN_POINT('Ctrl Pts',(-19.2907349020838,17.1679227808446,
-18.944797736685));
#102060=CARTESIAN_POINT('Ctrl Pts',(-19.3379741345028,17.1819844148328,
-18.9477806396456));
#102061=CARTESIAN_POINT('Ctrl Pts',(-19.407471955745,17.2026717307615,-18.9521690525414));
#102062=CARTESIAN_POINT('Ctrl Pts',(-19.4760413397733,17.2269742190327,
-18.9565574654372));
#102063=CARTESIAN_POINT('Ctrl Pts',(-19.5432790871371,17.2547903079878,
-18.960945878333));
#102064=CARTESIAN_POINT('Ctrl Pts',(-19.6105530590736,17.2826213829585,
-18.9653366555017));
#102065=CARTESIAN_POINT('Ctrl Pts',(-19.6764934827205,17.3139697486589,
-18.9697274326704));
#102066=CARTESIAN_POINT('Ctrl Pts',(-19.7407097395332,17.3486830290391,
-18.9741182098391));
#102067=CARTESIAN_POINT('Ctrl Pts',(-19.8047168505583,17.3832832518117,
-18.9784946866952));
#102068=CARTESIAN_POINT('Ctrl Pts',(-19.8670105658331,17.4212263095738,
-18.9828711635512));
#102069=CARTESIAN_POINT('Ctrl Pts',(-19.9272240799091,17.4623132655833,
-18.9872476404073));
#102070=CARTESIAN_POINT('Ctrl Pts',(-19.9873983214049,17.5033734237751,
-18.9916212628287));
#102071=CARTESIAN_POINT('Ctrl Pts',(-20.0454946569097,17.5475731395301,
-18.9959948852502));
#102072=CARTESIAN_POINT('Ctrl Pts',(-20.1011734655357,17.5946690576694,
-19.0003685076716));
#102073=CARTESIAN_POINT('Ctrl Pts',(-20.1568343267224,17.641749794968,-19.0047407203049));
#102074=CARTESIAN_POINT('Ctrl Pts',(-20.2100788408593,17.69172456909,-19.0091129329383));
#102075=CARTESIAN_POINT('Ctrl Pts',(-20.260600151433,17.7443095153903,-19.0134851455716));
#102076=CARTESIAN_POINT('Ctrl Pts',(-20.3114804721155,17.7972681362267,
-19.0178884276391));
#102077=CARTESIAN_POINT('Ctrl Pts',(-20.3595983637694,17.8528738414539,
-19.0222917097066));
#102078=CARTESIAN_POINT('Ctrl Pts',(-20.4046791157894,17.9107999030667,
-19.0266949917741));
#102079=CARTESIAN_POINT('Ctrl Pts',(-20.4494793907307,17.9683655684614,
-19.031070878121));
#102080=CARTESIAN_POINT('Ctrl Pts',(-20.4912799667756,18.0282223741802,
-19.0354467644678));
#102081=CARTESIAN_POINT('Ctrl Pts',(-20.529853854989,18.0900192100124,-19.0398226508146));
#102082=CARTESIAN_POINT('Ctrl Pts',(-20.5687899873458,18.152396374738,-19.0442396307425));
#102083=CARTESIAN_POINT('Ctrl Pts',(-20.6044382512207,18.2167497689265,
-19.0486566106703));
#102084=CARTESIAN_POINT('Ctrl Pts',(-20.636612911253,18.2826934181353,-19.0530735905982));
#102085=CARTESIAN_POINT('Ctrl Pts',(-20.6687875712854,18.3486370673441,
-19.057490570526));
#102086=CARTESIAN_POINT('Ctrl Pts',(-20.6974884771346,18.4161704915587,
-19.0619075504539));
#102087=CARTESIAN_POINT('Ctrl Pts',(-20.7225806137985,18.4848897174502,
-19.0663245303817));
#102088=CARTESIAN_POINT('',(-20.8509990913971,19.2090541452052,-18.0890148351743));
#102089=CARTESIAN_POINT('Ctrl Pts',(-20.7225806605155,18.4848898453927,
-18.8452754875981));
#102090=CARTESIAN_POINT('Ctrl Pts',(-20.7113123812129,18.4540296760972,
-18.843482250775));
#102091=CARTESIAN_POINT('Ctrl Pts',(-20.6993222446765,18.4234222395519,
-18.8416799355164));
#102092=CARTESIAN_POINT('Ctrl Pts',(-20.6575319528,18.3236548005616,-18.8356910254822));
#102093=CARTESIAN_POINT('Ctrl Pts',(-20.6247656769741,18.2558249992468,
-18.8314363670982));
#102094=CARTESIAN_POINT('Ctrl Pts',(-20.5838856248111,18.1815816305726,
-18.8264132177367));
#102095=CARTESIAN_POINT('Ctrl Pts',(-20.5792539498844,18.1733021359491,
-18.8258477181026));
#102096=CARTESIAN_POINT('Ctrl Pts',(-20.5723045746278,18.1610732133138,
-18.8250041205476));
#102097=CARTESIAN_POINT('Ctrl Pts',(-20.5700293834158,18.1570995925474,
-18.8247286884852));
#102098=CARTESIAN_POINT('Ctrl Pts',(-20.5659565723776,18.1500396455026,
-18.8242369226343));
#102099=CARTESIAN_POINT('Ctrl Pts',(-20.5641640160301,18.1469504564686,
-18.8240209171774));
#102100=CARTESIAN_POINT('Ctrl Pts',(-20.5602911440827,18.1403149105042,
-18.8235551451304));
#102101=CARTESIAN_POINT('Ctrl Pts',(-20.5582083430706,18.1367701250521,
-18.8233052224583));
#102102=CARTESIAN_POINT('Ctrl Pts',(-20.5524255485203,18.1269935192338,
-18.8226129291748));
#102103=CARTESIAN_POINT('Ctrl Pts',(-20.5487038996259,18.1207746659344,
-18.8221691841879));
#102104=CARTESIAN_POINT('Ctrl Pts',(-20.5280542387278,18.0866678935757,
-18.8197173785031));
#102105=CARTESIAN_POINT('Ctrl Pts',(-20.5105162385413,18.0591566599313,
-18.8176727794783));
#102106=CARTESIAN_POINT('Ctrl Pts',(-20.4017836244343,17.8969850172192,
-18.8052648880665));
#102107=CARTESIAN_POINT('Ctrl Pts',(-20.295956086838,17.7727960098617,-18.7943130933028));
#102108=CARTESIAN_POINT('Ctrl Pts',(-20.0915016564241,17.5823449808717,
-18.7760620014946));
#102109=CARTESIAN_POINT('Ctrl Pts',(-19.9995963204598,17.5099410141166,
-18.7686228828945));
#102110=CARTESIAN_POINT('Ctrl Pts',(-19.8902556624036,17.4375947956546,
-18.7606174281779));
#102111=CARTESIAN_POINT('Ctrl Pts',(-19.8782592760728,17.4298307490648,
-18.7597494731479));
#102112=CARTESIAN_POINT('Ctrl Pts',(-19.859041198722,17.4176671312054,-18.7583751914239));
#102113=CARTESIAN_POINT('Ctrl Pts',(-19.8518703321578,17.4131884412315,
-18.7578659368403));
#102114=CARTESIAN_POINT('Ctrl Pts',(-19.8391760175082,17.4053653029108,
-18.756970565691));
#102115=CARTESIAN_POINT('Ctrl Pts',(-19.833663773927,17.4020029644157,-18.7565837930307));
#102116=CARTESIAN_POINT('Ctrl Pts',(-19.8222308203897,17.3951007006677,
-18.755785722893));
#102117=CARTESIAN_POINT('Ctrl Pts',(-19.8163080118224,17.3915643861245,
-18.7553745608133));
#102118=CARTESIAN_POINT('Ctrl Pts',(-19.8010605116558,17.382561405085,-18.7543218379008));
#102119=CARTESIAN_POINT('Ctrl Pts',(-19.7917109736051,17.3771370460735,
-18.753681818445));
#102120=CARTESIAN_POINT('Ctrl Pts',(-19.7525150425459,17.3547960620988,
-18.7510210498005));
#102121=CARTESIAN_POINT('Ctrl Pts',(-19.7223002266858,17.3385340298066,
-18.7490238316801));
#102122=CARTESIAN_POINT('Ctrl Pts',(-19.6425552085979,17.2980824952101,
-18.7438794698669));
#102123=CARTESIAN_POINT('Ctrl Pts',(-19.5924512962847,17.2750795562293,
-18.7407717208731));
#102124=CARTESIAN_POINT('Ctrl Pts',(-19.4404219898909,17.2123468928775,
-18.7316269788336));
#102125=CARTESIAN_POINT('Ctrl Pts',(-19.3362575503628,17.1785303208363,
-18.7257387140683));
#102126=CARTESIAN_POINT('Ctrl Pts',(-19.185213426797,17.142132491777,-18.7172798297436));
#102127=CARTESIAN_POINT('Ctrl Pts',(-19.1401412152453,17.1328143986246,
-18.7147637885898));
#102128=CARTESIAN_POINT('Ctrl Pts',(-19.0730014604782,17.1212017992091,
-18.7109849046902));
#102129=CARTESIAN_POINT('Ctrl Pts',(-19.0511430224418,17.117773121191,-18.7097497768155));
#102130=CARTESIAN_POINT('Ctrl Pts',(-18.9782541198754,17.1075077681755,
-18.7056036522646));
#102131=CARTESIAN_POINT('Ctrl Pts',(-18.9270322243903,17.1021905540812,
-18.7026454778712));
#102132=CARTESIAN_POINT('Ctrl Pts',(-18.867052076745,17.0981675916767,-18.6990775024238));
#102133=CARTESIAN_POINT('Ctrl Pts',(-18.8584286626431,17.0976422113308,
-18.6985620256782));
#102134=CARTESIAN_POINT('Ctrl Pts',(-18.8453433190052,17.0969253540233,
-18.6977757076402));
#102135=CARTESIAN_POINT('Ctrl Pts',(-18.8408834816923,17.0966951818743,
-18.6975069832111));
#102136=CARTESIAN_POINT('Ctrl Pts',(-18.8328642849029,17.0963067486482,
-18.6970224336897));
#102137=CARTESIAN_POINT('Ctrl Pts',(-18.8293052282903,17.0961433601086,
-18.6968068987933));
#102138=CARTESIAN_POINT('Ctrl Pts',(-18.821556239394,17.0958072215883,-18.696336559941));
#102139=CARTESIAN_POINT('Ctrl Pts',(-18.8173662547135,17.0956379383725,
-18.6960815698099));
#102140=CARTESIAN_POINT('Ctrl Pts',(-18.8055579713674,17.0951959991779,
-18.6953611135334));
#102141=CARTESIAN_POINT('Ctrl Pts',(-18.7979387537046,17.0949520457045,
-18.6948940874485));
#102142=CARTESIAN_POINT('Ctrl Pts',(-18.7515938608364,17.093718696713,-18.6920409088379));
#102143=CARTESIAN_POINT('Ctrl Pts',(-18.712850946846,17.0937513276122,-18.6896030499337));
#102144=CARTESIAN_POINT('Ctrl Pts',(-18.5834929022021,17.0974108849747,
-18.6813344256672));
#102145=CARTESIAN_POINT('Ctrl Pts',(-18.4931159169131,17.105795927002,-18.6753498012045));
#102146=CARTESIAN_POINT('Ctrl Pts',(-18.3372635874928,17.1304245151083,
-18.6649228875809));
#102147=CARTESIAN_POINT('Ctrl Pts',(-18.2714997253667,17.1440485806457,
-18.6604883537513));
#102148=CARTESIAN_POINT('Ctrl Pts',(-18.0953557075175,17.1893690885935,
-18.6486171010104));
#102149=CARTESIAN_POINT('Ctrl Pts',(-17.9867142930103,17.2269562587735,
-18.641313125844));
#102150=CARTESIAN_POINT('Ctrl Pts',(-17.868588098506,17.2789144507888,-18.6334337531152));
#102151=CARTESIAN_POINT('Ctrl Pts',(-17.8555937025524,17.2847874673492,
-18.6325676243562));
#102152=CARTESIAN_POINT('Ctrl Pts',(-17.8349986740339,17.2943474629822,
-18.6311956787686));
#102153=CARTESIAN_POINT('Ctrl Pts',(-17.8273592287719,17.297949334983,-18.6306869495171));
#102154=CARTESIAN_POINT('Ctrl Pts',(-17.8139191786754,17.3043846866594,
-18.6297921892407));
#102155=CARTESIAN_POINT('Ctrl Pts',(-17.8081096339815,17.3071991431927,
-18.6294055049388));
#102156=CARTESIAN_POINT('Ctrl Pts',(-17.7961157072515,17.3130775343609,
-18.6286073172593));
#102157=CARTESIAN_POINT('Ctrl Pts',(-17.7899332461023,17.3161452303458,
-18.6281959507582));
#102158=CARTESIAN_POINT('Ctrl Pts',(-17.7740927630202,17.3241019442315,
-18.6271420829112));
#102159=CARTESIAN_POINT('Ctrl Pts',(-17.7644569619894,17.3290349417425,
-18.6265011295292));
#102160=CARTESIAN_POINT('Ctrl Pts',(-17.724319012616,17.34997344661,-18.6238312679306));
#102161=CARTESIAN_POINT('Ctrl Pts',(-17.6941709566264,17.366648816462,-18.6218260965537));
#102162=CARTESIAN_POINT('Ctrl Pts',(-17.6166178156028,17.4120511171355,
-18.6166565980664));
#102163=CARTESIAN_POINT('Ctrl Pts',(-17.5699093038678,17.441917318193,-18.6135321724689));
#102164=CARTESIAN_POINT('Ctrl Pts',(-17.4344715393567,17.536208068346,-18.6043583487418));
#102165=CARTESIAN_POINT('Ctrl Pts',(-17.3495159790017,17.6057252311954,
-18.5984575786685));
#102166=CARTESIAN_POINT('Ctrl Pts',(-17.2253112073214,17.7245851535917,
-18.5890964014264));
#102167=CARTESIAN_POINT('Ctrl Pts',(-17.1822224217581,17.76962684187,-18.5856839902293));
#102168=CARTESIAN_POINT('Ctrl Pts',(-17.1041153451539,17.8588417505782,
-18.5790314238806));
#102169=CARTESIAN_POINT('Ctrl Pts',(-17.0687523206251,17.9026403749648,
-18.5758089764813));
#102170=CARTESIAN_POINT('Ctrl Pts',(-17.029908573929,17.9548792126231,-18.5719467462809));
#102171=CARTESIAN_POINT('Ctrl Pts',(-17.0246824943781,17.9620001282147,
-18.5714198751705));
#102172=CARTESIAN_POINT('Ctrl Pts',(-17.0168571441804,17.9728038404035,
-18.5706195801113));
#102173=CARTESIAN_POINT('Ctrl Pts',(-17.0142247480488,17.9764626782294,
-18.5703483875093));
#102174=CARTESIAN_POINT('Ctrl Pts',(-17.0095309312963,17.9830308859647,
-18.5698612109275));
#102175=CARTESIAN_POINT('Ctrl Pts',(-17.0074651589293,17.9859370807053,
-18.5696455312086));
#102176=CARTESIAN_POINT('Ctrl Pts',(-17.0030041910248,17.992246608846,-18.5691770011826));
#102177=CARTESIAN_POINT('Ctrl Pts',(-17.0006117183176,17.9956517439941,
-18.5689239762789));
#102178=CARTESIAN_POINT('Ctrl Pts',(-16.9939490143187,18.0051942652536,
-18.5682144840628));
#102179=CARTESIAN_POINT('Ctrl Pts',(-16.9897012831795,18.0113471813133,
-18.5677565303065));
#102180=CARTESIAN_POINT('Ctrl Pts',(-16.9650753799944,18.0474255522536,
-18.5650690811547));
#102181=CARTESIAN_POINT('Ctrl Pts',(-16.9454362925661,18.0778454173411,
-18.5627944718622));
#102182=CARTESIAN_POINT('Ctrl Pts',(-16.8845227381142,18.1777284189964,
-18.5553355677207));
#102183=CARTESIAN_POINT('Ctrl Pts',(-16.8464430677305,18.2490522921136,
-18.5500264486163));
#102184=CARTESIAN_POINT('Ctrl Pts',(-16.7350623018389,18.4898890543805,
-18.5325062086297));
#102185=CARTESIAN_POINT('Ctrl Pts',(-16.6798120052927,18.6668568314805,
-18.5203494408362));
#102186=CARTESIAN_POINT('Ctrl Pts',(-16.6444200791822,18.8706503759169,
-18.5076276806556));
#102187=CARTESIAN_POINT('Ctrl Pts',(-16.6409648788929,18.892588076754,-18.506272762166));
#102188=CARTESIAN_POINT('Ctrl Pts',(-16.6366687924886,18.9229676729009,
-18.5044158648713));
#102189=CARTESIAN_POINT('Ctrl Pts',(-16.6355325843793,18.9313657311761,
-18.5039045871614));
#102190=CARTESIAN_POINT('Ctrl Pts',(-16.633667589146,18.9458024219286,-18.5030291118981));
#102191=CARTESIAN_POINT('Ctrl Pts',(-16.6329143483417,18.9518377398332,
-18.5026641456139));
#102192=CARTESIAN_POINT('Ctrl Pts',(-16.6314162863302,18.9642768976401,
-18.5019140171535));
#102193=CARTESIAN_POINT('Ctrl Pts',(-16.6306746865337,18.9706810673731,
-18.5015289603209));
#102194=CARTESIAN_POINT('Ctrl Pts',(-16.6290188354424,18.9855754793064,
-18.5006360198249));
#102195=CARTESIAN_POINT('Ctrl Pts',(-16.6281266721895,18.9940681025113,
-18.5001288370362));
#102196=CARTESIAN_POINT('Ctrl Pts',(-16.6254422588638,19.021200389181,-18.4985145827147));
#102197=CARTESIAN_POINT('Ctrl Pts',(-16.6238458866772,19.0398588554769,
-18.4974136689816));
#102198=CARTESIAN_POINT('Ctrl Pts',(-16.6207015717367,19.0834052108706,
-18.4948641876817));
#102199=CARTESIAN_POINT('Ctrl Pts',(-16.6193453325324,19.1083043921394,
-18.4934215645896));
#102200=CARTESIAN_POINT('Ctrl Pts',(-16.6161236358701,19.1959354658402,
-18.4883909198547));
#102201=CARTESIAN_POINT('Ctrl Pts',(-16.6166075820429,19.2587228882699,
-18.4848714188122));
#102202=CARTESIAN_POINT('Ctrl Pts',(-16.6250763360982,19.4208964994915,
-18.4758936563694));
#102203=CARTESIAN_POINT('Ctrl Pts',(-16.6372896489054,19.5199041061963,
-18.4705265895589));
#102204=CARTESIAN_POINT('Ctrl Pts',(-16.6703757761435,19.688927065847,-18.4611455235353));
#102205=CARTESIAN_POINT('Ctrl Pts',(-16.6879763700105,19.7594024107075,
-18.4571637022484));
#102206=CARTESIAN_POINT('Ctrl Pts',(-16.7224337106618,19.8723309385836,
-18.4504775309333));
#102207=CARTESIAN_POINT('Ctrl Pts',(-16.7371044392647,19.9153898114008,
-18.4478528432147));
#102208=CARTESIAN_POINT('Ctrl Pts',(-16.7558349744706,19.9650623877469,
-18.4447001323656));
#102209=CARTESIAN_POINT('Ctrl Pts',(-16.7585593050228,19.9721708149481,
-18.4442459260524));
#102210=CARTESIAN_POINT('Ctrl Pts',(-16.7629929661602,19.9835551610362,
-18.4435133850684));
#102211=CARTESIAN_POINT('Ctrl Pts',(-16.7646780406065,19.9878405393788,
-18.4432364675873));
#102212=CARTESIAN_POINT('Ctrl Pts',(-16.7676990371587,19.9954503554379,
-18.4427425887856));
#102213=CARTESIAN_POINT('Ctrl Pts',(-16.7690294317274,19.9987769368674,
-18.4425259618986));
#102214=CARTESIAN_POINT('Ctrl Pts',(-16.7718806419747,20.0058540770918,
-18.4420635208414));
#102215=CARTESIAN_POINT('Ctrl Pts',(-16.7734037461362,20.0096035986067,
-18.4418175748332));
#102216=CARTESIAN_POINT('Ctrl Pts',(-16.7775739730624,20.0197858733875,
-18.4411471627926));
#102217=CARTESIAN_POINT('Ctrl Pts',(-16.7802420377899,20.0262099176705,
-18.440721459362));
#102218=CARTESIAN_POINT('Ctrl Pts',(-16.7940581786047,20.0590183658349,
-18.4385337340417));
#102219=CARTESIAN_POINT('Ctrl Pts',(-16.8057086627393,20.0851863359754,
-18.4367436744521));
#102220=CARTESIAN_POINT('Ctrl Pts',(-16.8415930256975,20.1615755179546,
-18.4314010059629));
#102221=CARTESIAN_POINT('Ctrl Pts',(-16.8672833686317,20.2110830646669,
-18.4277867724062));
#102222=CARTESIAN_POINT('Ctrl Pts',(-16.9641148025644,20.380926188453,-18.4149792257097));
#102223=CARTESIAN_POINT('Ctrl Pts',(-17.0451937295155,20.4951959966145,
-18.4056419046629));
#102224=CARTESIAN_POINT('Ctrl Pts',(-17.1956136785661,20.6680671950216,
-18.3908536158708));
#102225=CARTESIAN_POINT('Ctrl Pts',(-17.2584993159252,20.7317164875509,
-18.3852223007828));
#102226=CARTESIAN_POINT('Ctrl Pts',(-17.335455302848,20.8003235761346,-18.3789320111313));
#102227=CARTESIAN_POINT('Ctrl Pts',(-17.3457701912751,20.8093412375359,
-18.3781002816309));
#102228=CARTESIAN_POINT('Ctrl Pts',(-17.3624602970714,20.8236488902854,
-18.3767724235661));
#102229=CARTESIAN_POINT('Ctrl Pts',(-17.3687801563195,20.8290025900825,
-18.3762736669715));
#102230=CARTESIAN_POINT('Ctrl Pts',(-17.3800617019963,20.8384462900963,
-18.375390433832));
#102231=CARTESIAN_POINT('Ctrl Pts',(-17.3850108793157,20.8425510092054,
-18.3750053572364));
#102232=CARTESIAN_POINT('Ctrl Pts',(-17.3953661692853,20.8510600871905,
-18.3742045864678));
#102233=CARTESIAN_POINT('Ctrl Pts',(-17.4007755032213,20.855460417677,-18.3737890584724));
#102234=CARTESIAN_POINT('Ctrl Pts',(-17.4148896843368,20.8668264604222,
-18.3727119634686));
#102235=CARTESIAN_POINT('Ctrl Pts',(-17.4236280616696,20.873750336746,-18.3720520801946));
#102236=CARTESIAN_POINT('Ctrl Pts',(-17.4619075006349,20.9035919582972,
-18.3691910091844));
#102237=CARTESIAN_POINT('Ctrl Pts',(-17.4919991324997,20.9257947287182,
-18.3670181151365));
#102238=CARTESIAN_POINT('Ctrl Pts',(-17.57360358355,20.9827299583572,-18.3613084696117));
#102239=CARTESIAN_POINT('Ctrl Pts',(-17.6260844569564,21.0160127168111,
-18.3578234738029));
#102240=CARTESIAN_POINT('Ctrl Pts',(-17.7615180464885,21.0937673349624,
-18.3491860913571));
#102241=CARTESIAN_POINT('Ctrl Pts',(-17.8461113089125,21.1351071274312,
-18.3441102629351));
#102242=CARTESIAN_POINT('Ctrl Pts',(-18.0471320316314,21.2172543976426,
-18.3322971687134));
#102243=CARTESIAN_POINT('Ctrl Pts',(-18.1649197548056,21.2537880565793,
-18.3255544315244));
#102244=CARTESIAN_POINT('Ctrl Pts',(-18.294420180211,21.2818809072839,-18.3177000941544));
#102245=CARTESIAN_POINT('Ctrl Pts',(-18.3036605879557,21.2838208154799,
-18.3171372495877));
#102246=CARTESIAN_POINT('Ctrl Pts',(-18.3173921952109,21.2866078199623,
-18.3162968628275));
#102247=CARTESIAN_POINT('Ctrl Pts',(-18.321873805411,21.2875023198,-18.3160219571014));
#102248=CARTESIAN_POINT('Ctrl Pts',(-18.329862256082,21.2890698821095,-18.3155307659069));
#102249=CARTESIAN_POINT('Ctrl Pts',(-18.3333679369158,21.2897485900853,
-18.3153148057859));
#102250=CARTESIAN_POINT('Ctrl Pts',(-18.3409196493654,21.2911908063273,
-18.3148487135619));
#102251=CARTESIAN_POINT('Ctrl Pts',(-18.3449661373781,21.2919513703712,
-18.3145984231655));
#102252=CARTESIAN_POINT('Ctrl Pts',(-18.3561680328796,21.2940230252584,
-18.3139040976406));
#102253=CARTESIAN_POINT('Ctrl Pts',(-18.3633279397275,21.2953090316292,
-18.3134586750977));
#102254=CARTESIAN_POINT('Ctrl Pts',(-18.401803121093,21.3020151268502,-18.3110568826375));
#102255=CARTESIAN_POINT('Ctrl Pts',(-18.4332290461028,21.3067661149977,
-18.309065955719));
#102256=CARTESIAN_POINT('Ctrl Pts',(-18.6266527132522,21.3315682526454,
-18.2966817144529));
#102257=CARTESIAN_POINT('Ctrl Pts',(-18.7904105055977,21.3335340649681,
-18.2856881651653));
#102258=CARTESIAN_POINT('Ctrl Pts',(-19.0691176224929,21.3045780093424,
-18.2673840949449));
#102259=CARTESIAN_POINT('Ctrl Pts',(-19.184281020735,21.2828657153222,-18.2599322079371));
#102260=CARTESIAN_POINT('Ctrl Pts',(-19.3108537418502,21.2479420728577,
-18.2519148693099));
#102261=CARTESIAN_POINT('Ctrl Pts',(-19.3245918804956,21.2440013512247,
-18.2510467591403));
#102262=CARTESIAN_POINT('Ctrl Pts',(-19.3463926963135,21.2375082469543,
-18.249672278985));
#102263=CARTESIAN_POINT('Ctrl Pts',(-19.3544816211667,21.2350462076016,
-18.249162979794));
#102264=CARTESIAN_POINT('Ctrl Pts',(-19.3687213290974,21.2306186582975,
-18.2482675567575));
#102265=CARTESIAN_POINT('Ctrl Pts',(-19.3748782359761,21.2286733577662,
-18.2478807765782));
#102266=CARTESIAN_POINT('Ctrl Pts',(-19.3875939364863,21.2245917028674,
-18.2470827163397));
#102267=CARTESIAN_POINT('Ctrl Pts',(-19.3941513888815,21.2224513976623,
-18.2466715715529));
#102268=CARTESIAN_POINT('Ctrl Pts',(-19.4109558812591,21.2168755037443,
-18.2456189455179));
#102269=CARTESIAN_POINT('Ctrl Pts',(-19.4211873656841,21.2133934010812,
-18.2449790050895));
#102270=CARTESIAN_POINT('Ctrl Pts',(-19.4631591849632,21.1987494536888,
-18.2423573175786));
#102271=CARTESIAN_POINT('Ctrl Pts',(-19.4946589458198,21.1869097048001,
-18.2403980965002));
#102272=CARTESIAN_POINT('Ctrl Pts',(-19.5758782853012,21.1541516269173,
-18.2353573405987));
#102273=CARTESIAN_POINT('Ctrl Pts',(-19.6251053130139,21.1320750178919,
-18.232313460381));
#102274=CARTESIAN_POINT('Ctrl Pts',(-19.7875131334145,21.0516528946919,
-18.2222267901521));
#102275=CARTESIAN_POINT('Ctrl Pts',(-19.8962588136807,20.9849920601618,
-18.2154131056184));
#102276=CARTESIAN_POINT('Ctrl Pts',(-20.0802520402526,20.8479849206862,
-18.2028688011266));
#102277=CARTESIAN_POINT('Ctrl Pts',(-20.1576161874521,20.781167365725,-18.1972001957628));
#102278=CARTESIAN_POINT('Ctrl Pts',(-20.2367056090523,20.7021937393487,
-18.1905785829377));
#102279=CARTESIAN_POINT('Ctrl Pts',(-20.2435159618116,20.6952993191145,
-18.1900010840718));
#102280=CARTESIAN_POINT('Ctrl Pts',(-20.253501809508,20.6850504006879,-18.1891429902576));
#102281=CARTESIAN_POINT('Ctrl Pts',(-20.2567141574148,20.6817317657371,
-18.1888651959223));
#102282=CARTESIAN_POINT('Ctrl Pts',(-20.2623940489886,20.6758253876297,
-18.1883708351796));
#102283=CARTESIAN_POINT('Ctrl Pts',(-20.2648659238849,20.6732418774289,
-18.1881546104882));
#102284=CARTESIAN_POINT('Ctrl Pts',(-20.2701482855966,20.6676928767169,
-18.1876902036748));
#102285=CARTESIAN_POINT('Ctrl Pts',(-20.272956694062,20.6647255537303,-18.1874418751137));
#102286=CARTESIAN_POINT('Ctrl Pts',(-20.2787023602443,20.6586194588903,
-18.1869309311276));
#102287=CARTESIAN_POINT('Ctrl Pts',(-20.281638680851,20.6554798345072,-18.1866682475573));
#102288=CARTESIAN_POINT('Ctrl Pts',(-20.2950923992441,20.6410065001642,
-18.1854575478593));
#102289=CARTESIAN_POINT('Ctrl Pts',(-20.3054946772955,20.6295670646149,
-18.1845013204067));
#102290=CARTESIAN_POINT('Ctrl Pts',(-20.373802653567,20.5527750441598,-18.1780928773938));
#102291=CARTESIAN_POINT('Ctrl Pts',(-20.4277374315298,20.4840135069281,
-18.1724082714805));
#102292=CARTESIAN_POINT('Ctrl Pts',(-20.5185485974922,20.3522138435245,
-18.1618726270031));
#102293=CARTESIAN_POINT('Ctrl Pts',(-20.5567134720684,20.290211972345,-18.1570467852984));
#102294=CARTESIAN_POINT('Ctrl Pts',(-20.5938938829306,20.2221905888911,
-18.1519487435824));
#102295=CARTESIAN_POINT('Ctrl Pts',(-20.5961630741471,20.2180056347125,
-18.1516358473825));
#102296=CARTESIAN_POINT('Ctrl Pts',(-20.6621519663309,20.0953198686994,
-18.1424854513605));
#102297=CARTESIAN_POINT('Ctrl Pts',(-20.7144538820208,19.9710037717547,
-18.1338552316719));
#102298=CARTESIAN_POINT('Ctrl Pts',(-20.7593062374906,19.8274998292925,
-18.1246739477026));
#102299=CARTESIAN_POINT('Ctrl Pts',(-20.7638398849016,19.8124045708868,
-18.123717027009));
#102300=CARTESIAN_POINT('Ctrl Pts',(-20.7704399625781,19.7895036156674,
-18.1222783558662));
#102301=CARTESIAN_POINT('Ctrl Pts',(-20.7726309376648,19.7817346645665,
-18.1217925574626));
#102302=CARTESIAN_POINT('Ctrl Pts',(-20.7764755274864,19.7677975362387,
-18.1209250381826));
#102303=CARTESIAN_POINT('Ctrl Pts',(-20.7781457594234,19.7616340820893,
-18.1205427810745));
#102304=CARTESIAN_POINT('Ctrl Pts',(-20.78162868502,19.7485471941944,-18.119734034827));
#102305=CARTESIAN_POINT('Ctrl Pts',(-20.7834342132145,19.7416219231616,
-18.1193077820769));
#102306=CARTESIAN_POINT('Ctrl Pts',(-20.7870375877092,19.7275080528404,
-18.1184424999487));
#102307=CARTESIAN_POINT('Ctrl Pts',(-20.7888328801429,19.7203189000964,
-18.1180035578064));
#102308=CARTESIAN_POINT('Ctrl Pts',(-20.7932123060319,19.7023815980453,
-18.1169127792003));
#102309=CARTESIAN_POINT('Ctrl Pts',(-20.7957500888887,19.6916222779489,
-18.1162624274975));
#102310=CARTESIAN_POINT('Ctrl Pts',(-20.8334344277754,19.5260604299048,
-18.1063132200247));
#102311=CARTESIAN_POINT('Ctrl Pts',(-20.8511450351187,19.3678091395082,
-18.0976370754808));
#102312=CARTESIAN_POINT('Ctrl Pts',(-20.8509991056215,19.209054030408,-18.0890148055994));
#102313=CARTESIAN_POINT('Ctrl Pts',(-20.8509991057282,19.2090541464559,
-18.0890148119022));
#102314=CARTESIAN_POINT('Ctrl Pts',(-20.8508677556262,19.0661512803534,
-18.0812535052745));
#102315=CARTESIAN_POINT('Ctrl Pts',(-20.8362673125345,18.9236435276234,
-18.0735576995762));
#102316=CARTESIAN_POINT('Ctrl Pts',(-20.8054605704913,18.7741529475324,
-18.0645866360258));
#102317=CARTESIAN_POINT('Ctrl Pts',(-20.8034247687687,18.7646085115214,
-18.0640097962226));
#102318=CARTESIAN_POINT('Ctrl Pts',(-20.8001177070468,18.7496130180313,
-18.0630966111073));
#102319=CARTESIAN_POINT('Ctrl Pts',(-20.7988906685246,18.7441522175532,
-18.0627626188202));
#102320=CARTESIAN_POINT('Ctrl Pts',(-20.7965252968809,18.7338171694132,
-18.0621276602403));
#102321=CARTESIAN_POINT('Ctrl Pts',(-20.7953913008448,18.7289419560779,
-18.0618269359283));
#102322=CARTESIAN_POINT('Ctrl Pts',(-20.7934049810816,18.7205376622443,
-18.0613063720389));
#102323=CARTESIAN_POINT('Ctrl Pts',(-20.792560840268,18.717006631999,-18.0610870021718));
#102324=CARTESIAN_POINT('Ctrl Pts',(-20.7909046571635,18.7101568059559,
-18.060660145096));
#102325=CARTESIAN_POINT('Ctrl Pts',(-20.7900936622065,18.7068377983904,
-18.0604527244233));
#102326=CARTESIAN_POINT('Ctrl Pts',(-20.7878798168748,18.6978717951775,
-18.0598908229163));
#102327=CARTESIAN_POINT('Ctrl Pts',(-20.7864617259332,18.6922286452664,
-18.059535476532));
#102328=CARTESIAN_POINT('Ctrl Pts',(-20.7810875036896,18.6712094602303,
-18.0582057915177));
#102329=CARTESIAN_POINT('Ctrl Pts',(-20.7769818152394,18.6558726787763,
-18.0572233519935));
#102330=CARTESIAN_POINT('Ctrl Pts',(-20.7580005331028,18.5880323254332,
-18.0528276743546));
#102331=CARTESIAN_POINT('Ctrl Pts',(-20.7412781925629,18.5360963365021,
-18.0493294498771));
#102332=CARTESIAN_POINT('Ctrl Pts',(-20.7225806765445,18.484889889291,-18.0457834329553));
#102333=CARTESIAN_POINT('Origin',(-18.734,19.211,0.));
#102334=CARTESIAN_POINT('',(-20.7225806138883,18.484889717696,-17.2426990599955));
#102335=CARTESIAN_POINT('',(-20.7225806135343,18.4848897167264,-17.4677765237272));
#102336=CARTESIAN_POINT('',(-20.7225806137986,18.4848897174502,0.));
#102337=CARTESIAN_POINT('Ctrl Pts',(-20.7225806135343,18.4848897167264,
-17.4677765237272));
#102338=CARTESIAN_POINT('Ctrl Pts',(-20.7401855017382,18.5331037968631,
-17.4710694629831));
#102339=CARTESIAN_POINT('Ctrl Pts',(-20.7560325936953,18.5819462166473,
-17.4743159902952));
#102340=CARTESIAN_POINT('Ctrl Pts',(-20.7795153171967,18.6644279559498,
-17.479647141129));
#102341=CARTESIAN_POINT('Ctrl Pts',(-20.7881324561808,18.6977612804346,
-17.4817614807328));
#102342=CARTESIAN_POINT('Ctrl Pts',(-20.798385541561,18.7418321682609,-17.4845061478134));
#102343=CARTESIAN_POINT('Ctrl Pts',(-20.8007569905954,18.7523915971316,
-17.4851599905889));
#102344=CARTESIAN_POINT('Ctrl Pts',(-20.8045078945201,18.7697136045771,
-17.4862265075556));
#102345=CARTESIAN_POINT('Ctrl Pts',(-20.8059354157485,18.7764654688328,
-17.4866407168297));
#102346=CARTESIAN_POINT('Ctrl Pts',(-20.8086343584051,18.78954661849,-17.4874403466462));
#102347=CARTESIAN_POINT('Ctrl Pts',(-20.8099098928635,18.7958749682356,
-17.4878258947998));
#102348=CARTESIAN_POINT('Ctrl Pts',(-20.8127876279131,18.8104973732348,
-17.488713811454));
#102349=CARTESIAN_POINT('Ctrl Pts',(-20.814369179777,18.8187954169063,-17.4892155163142));
#102350=CARTESIAN_POINT('Ctrl Pts',(-20.8184877298123,18.8411305981548,
-17.4905602003735));
#102351=CARTESIAN_POINT('Ctrl Pts',(-20.8209326213357,18.8551844312056,
-17.4914002514707));
#102352=CARTESIAN_POINT('Ctrl Pts',(-20.8418093122528,18.9828153677844,
-17.498976914763));
#102353=CARTESIAN_POINT('Ctrl Pts',(-20.8510962906784,19.0977007821835,
-17.5054071166955));
#102354=CARTESIAN_POINT('Ctrl Pts',(-20.8508421937833,19.3990360594247,
-17.5219135397002));
#102355=CARTESIAN_POINT('Ctrl Pts',(-20.8261075478748,19.5844189879619,
-17.5316811244396));
#102356=CARTESIAN_POINT('Ctrl Pts',(-20.7737437540893,19.7778655756826,
-17.5434580816054));
#102357=CARTESIAN_POINT('Ctrl Pts',(-20.7698906310782,19.7915518728401,
-17.5443004711881));
#102358=CARTESIAN_POINT('Ctrl Pts',(-20.7643392702007,19.8105351281857,
-17.5454830104063));
#102359=CARTESIAN_POINT('Ctrl Pts',(-20.7627574776275,19.8158661152896,
-17.5458166554832));
#102360=CARTESIAN_POINT('Ctrl Pts',(-20.7601843571699,19.8244144477096,
-17.546354256482));
#102361=CARTESIAN_POINT('Ctrl Pts',(-20.7592063131648,19.8276358103852,
-17.5465574398533));
#102362=CARTESIAN_POINT('Ctrl Pts',(-20.7571469224101,19.8343610324556,
-17.5469828914886));
#102363=CARTESIAN_POINT('Ctrl Pts',(-20.7560641553507,19.8378644170424,
-17.5472052452409));
#102364=CARTESIAN_POINT('Ctrl Pts',(-20.753422272186,19.8463343881325,-17.5477445402991));
#102365=CARTESIAN_POINT('Ctrl Pts',(-20.7518539338272,19.8512980544694,
-17.5480620177548));
#102366=CARTESIAN_POINT('Ctrl Pts',(-20.746300568609,19.8686509684515,-17.5491768136078));
#102367=CARTESIAN_POINT('Ctrl Pts',(-20.7422197101637,19.8810089186436,
-17.5499794781113));
#102368=CARTESIAN_POINT('Ctrl Pts',(-20.7174287549397,19.9538209592796,
-17.554757362591));
#102369=CARTESIAN_POINT('Ctrl Pts',(-20.6941056009685,20.0133447400581,
-17.5588615753347));
#102370=CARTESIAN_POINT('Ctrl Pts',(-20.5919077580978,20.2429950445904,
-17.5752528778096));
#102371=CARTESIAN_POINT('Ctrl Pts',(-20.4932538776527,20.403426203793,-17.5878515549434));
#102372=CARTESIAN_POINT('Ctrl Pts',(-20.339345532912,20.5921931517566,-17.6032548905438));
#102373=CARTESIAN_POINT('Ctrl Pts',(-20.3022242623432,20.6342014585516,
-17.6067354325915));
#102374=CARTESIAN_POINT('Ctrl Pts',(-20.2551575013988,20.6833836584273,
-17.6108793456923));
#102375=CARTESIAN_POINT('Ctrl Pts',(-20.2467641375125,20.6920058930676,
-17.6116085810263));
#102376=CARTESIAN_POINT('Ctrl Pts',(-20.2327633285163,20.7061452605599,
-17.6128091802791));
#102377=CARTESIAN_POINT('Ctrl Pts',(-20.2271979156031,20.7117034525592,
-17.6132823734987));
#102378=CARTESIAN_POINT('Ctrl Pts',(-20.2170712362349,20.7217048858146,
-17.6141361456632));
#102379=CARTESIAN_POINT('Ctrl Pts',(-20.2125206755465,20.7261587894095,
-17.6145171931039));
#102380=CARTESIAN_POINT('Ctrl Pts',(-20.2027146364378,20.7356702968274,
-17.6153327865034));
#102381=CARTESIAN_POINT('Ctrl Pts',(-20.1974529644605,20.7407214191377,
-17.6157670469204));
#102382=CARTESIAN_POINT('Ctrl Pts',(-20.1830322554327,20.7544225698834,
-17.6169481756598));
#102383=CARTESIAN_POINT('Ctrl Pts',(-20.1738218512727,20.7630182838601,
-17.6176926990876));
#102384=CARTESIAN_POINT('Ctrl Pts',(-20.1246865380443,20.8080604985663,
-17.6216137907165));
#102385=CARTESIAN_POINT('Ctrl Pts',(-20.0834512976085,20.8430518380806,
-17.6247285140547));
#102386=CARTESIAN_POINT('Ctrl Pts',(-19.8904550279948,20.994502633775,-17.6386249558782));
#102387=CARTESIAN_POINT('Ctrl Pts',(-19.7246997223292,21.0916324078305,
-17.648649131046));
#102388=CARTESIAN_POINT('Ctrl Pts',(-19.532889788244,21.1715452891823,-17.6602001879931));
#102389=CARTESIAN_POINT('Ctrl Pts',(-19.5175438116647,21.1777287052002,
-17.6611246906026));
#102390=CARTESIAN_POINT('Ctrl Pts',(-19.4525633609,21.2030303001758,-17.6650468672106));
#102391=CARTESIAN_POINT('Ctrl Pts',(-19.4022941167739,21.2204526575283,
-17.6680992391007));
#102392=CARTESIAN_POINT('Ctrl Pts',(-19.3430951510089,21.2385028907138,
-17.6717720244273));
#102393=CARTESIAN_POINT('Ctrl Pts',(-19.3347477946261,21.2409918611138,
-17.6722916909952));
#102394=CARTESIAN_POINT('Ctrl Pts',(-19.3220833337508,21.2446831300285,
-17.6730831509535));
#102395=CARTESIAN_POINT('Ctrl Pts',(-19.3177772636195,21.245923385887,-17.6733527857104));
#102396=CARTESIAN_POINT('Ctrl Pts',(-19.3100395985306,21.2481254457913,
-17.6738383000373));
#102397=CARTESIAN_POINT('Ctrl Pts',(-19.3066094866584,21.2490922639705,
-17.6740538842183));
#102398=CARTESIAN_POINT('Ctrl Pts',(-19.2991494074299,21.251174657215,-17.6745235372396));
#102399=CARTESIAN_POINT('Ctrl Pts',(-19.2951186240095,21.2522869405726,
-17.6747777879111));
#102400=CARTESIAN_POINT('Ctrl Pts',(-19.2837833323716,21.2553787717146,
-17.6754941120813));
#102401=CARTESIAN_POINT('Ctrl Pts',(-19.2764715518758,21.2573310793282,
-17.6759577176318));
#102402=CARTESIAN_POINT('Ctrl Pts',(-19.2326173819694,21.2687889621607,
-17.678746880659));
#102403=CARTESIAN_POINT('Ctrl Pts',(-19.1958388841269,21.2773540702253,
-17.6811215430674));
#102404=CARTESIAN_POINT('Ctrl Pts',(-19.0738711903075,21.3023396898997,
-17.6890698828279));
#102405=CARTESIAN_POINT('Ctrl Pts',(-18.9879041063387,21.314507765477,-17.6947856458968));
#102406=CARTESIAN_POINT('Ctrl Pts',(-18.7261753247924,21.3352736700453,
-17.7121323654626));
#102407=CARTESIAN_POINT('Ctrl Pts',(-18.5498247968382,21.3272946240507,
-17.7236767744086));
#102408=CARTESIAN_POINT('Ctrl Pts',(-18.3538349909117,21.293712395024,-17.7359157952053));
#102409=CARTESIAN_POINT('Ctrl Pts',(-18.3312645955787,21.289465927971,-17.7373176563944));
#102410=CARTESIAN_POINT('Ctrl Pts',(-18.2994198014168,21.2829363154545,
-17.7392854628916));
#102411=CARTESIAN_POINT('Ctrl Pts',(-18.2900855071934,21.2809565145285,
-17.7398610319646));
#102412=CARTESIAN_POINT('Ctrl Pts',(-18.2749371285508,21.2776363669525,
-17.7407931868183));
#102413=CARTESIAN_POINT('Ctrl Pts',(-18.2691148405509,21.276334448173,-17.741150998533));
#102414=CARTESIAN_POINT('Ctrl Pts',(-18.2569362181612,21.2735570843908,
-17.7418985026749));
#102415=CARTESIAN_POINT('Ctrl Pts',(-18.2505810368542,21.2720768267715,
-17.7422880361825));
#102416=CARTESIAN_POINT('Ctrl Pts',(-18.2354734744866,21.2684842324869,
-17.7432128060565));
#102417=CARTESIAN_POINT('Ctrl Pts',(-18.2267274796152,21.2663453864129,
-17.7437471833));
#102418=CARTESIAN_POINT('Ctrl Pts',(-18.1972848267411,21.2589457606144,
-17.7455429939267));
#102419=CARTESIAN_POINT('Ctrl Pts',(-18.1766537735633,21.2534275381563,
-17.746796116402));
#102420=CARTESIAN_POINT('Ctrl Pts',(-18.0646429720959,21.221644134476,-17.7535762391585));
#102421=CARTESIAN_POINT('Ctrl Pts',(-17.9750234795633,21.1895566352275,
-17.7589089307374));
#102422=CARTESIAN_POINT('Ctrl Pts',(-17.7316856130007,21.0834532436264,
-17.7735136302517));
#102423=CARTESIAN_POINT('Ctrl Pts',(-17.5843250381929,20.9967633772086,
-17.7824762307702));
#102424=CARTESIAN_POINT('Ctrl Pts',(-17.4194444096351,20.8708228937859,
-17.7943223132381));
#102425=CARTESIAN_POINT('Ctrl Pts',(-17.3905292247996,20.8475067486092,
-17.7964791248145));
#102426=CARTESIAN_POINT('Ctrl Pts',(-17.3567880977732,20.8188021307609,
-17.7991126703789));
#102427=CARTESIAN_POINT('Ctrl Pts',(-17.3513556187075,20.8141328163614,
-17.7995404077042));
#102428=CARTESIAN_POINT('Ctrl Pts',(-17.342535023044,20.8064731707622,-17.8002412142003));
#102429=CARTESIAN_POINT('Ctrl Pts',(-17.3391325480752,20.8034993599396,
-17.800513088652));
#102430=CARTESIAN_POINT('Ctrl Pts',(-17.3330617886125,20.7981590493674,
-17.8010009970408));
#102431=CARTESIAN_POINT('Ctrl Pts',(-17.3303899401623,20.795796680892,-17.8012167228393));
#102432=CARTESIAN_POINT('Ctrl Pts',(-17.3246195900884,20.7906686706827,
-17.8016847806611));
#102433=CARTESIAN_POINT('Ctrl Pts',(-17.3215232961562,20.7879006973786,
-17.801937284191));
#102434=CARTESIAN_POINT('Ctrl Pts',(-17.3129044808975,20.7801500410381,
-17.8026438769515));
#102435=CARTESIAN_POINT('Ctrl Pts',(-17.3074001082275,20.7751473941808,
-17.8030994334585));
#102436=CARTESIAN_POINT('Ctrl Pts',(-17.2757262840235,20.746054383076,-17.8057451865685));
#102437=CARTESIAN_POINT('Ctrl Pts',(-17.2501425757728,20.7213380379271,
-17.8079789114837));
#102438=CARTESIAN_POINT('Ctrl Pts',(-17.1701688941047,20.6400818718344,
-17.8152436471109));
#102439=CARTESIAN_POINT('Ctrl Pts',(-17.1182960689422,20.5811612570308,
-17.8203928897734));
#102440=CARTESIAN_POINT('Ctrl Pts',(-16.9535227908271,20.3715988317451,
-17.8379884213599));
#102441=CARTESIAN_POINT('Ctrl Pts',(-16.8574389357575,20.2088156622849,
-17.8503967891509));
#102442=CARTESIAN_POINT('Ctrl Pts',(-16.7756319364519,20.0153384689312,
-17.8633116409322));
#102443=CARTESIAN_POINT('Ctrl Pts',(-16.767439216009,19.9950947543902,-17.8646436958221));
#102444=CARTESIAN_POINT('Ctrl Pts',(-16.7565247311852,19.9668778953813,
-17.866474504849));
#102445=CARTESIAN_POINT('Ctrl Pts',(-16.7535353304409,19.959010379158,-17.8669822213399));
#102446=CARTESIAN_POINT('Ctrl Pts',(-16.7484719090493,19.945441287623,-17.8678532078645));
#102447=CARTESIAN_POINT('Ctrl Pts',(-16.7463753511042,19.9397482838492,
-17.8682172289767));
#102448=CARTESIAN_POINT('Ctrl Pts',(-16.7420986081804,19.9279794367077,
-17.8689668815873));
#102449=CARTESIAN_POINT('Ctrl Pts',(-16.7399216800821,19.9219024707035,
-17.8693524012691));
#102450=CARTESIAN_POINT('Ctrl Pts',(-16.7349121175787,19.9077140414799,
-17.8702488977921));
#102451=CARTESIAN_POINT('Ctrl Pts',(-16.7321009872935,19.899595064957,-17.8707591561239));
#102452=CARTESIAN_POINT('Ctrl Pts',(-16.7232285355061,19.8734564550765,
-17.872393289621));
#102453=CARTESIAN_POINT('Ctrl Pts',(-16.717360383947,19.8553718888468,-17.8735107878467));
#102454=CARTESIAN_POINT('Ctrl Pts',(-16.6890932315124,19.7640868483366,
-17.8790893020267));
#102455=CARTESIAN_POINT('Ctrl Pts',(-16.6704313017467,19.6897846862073,
-17.8834272040591));
#102456=CARTESIAN_POINT('Ctrl Pts',(-16.6348812019892,19.5067474962954,
-17.8937893867801));
#102457=CARTESIAN_POINT('Ctrl Pts',(-16.6223602186109,19.3973989326201,
-17.8997042896731));
#102458=CARTESIAN_POINT('Ctrl Pts',(-16.6158407657569,19.21726838309,-17.9095210497298));
#102459=CARTESIAN_POINT('Ctrl Pts',(-16.6168022693298,19.1468873021952,
-17.9133779394741));
#102460=CARTESIAN_POINT('Ctrl Pts',(-16.6243087937617,19.0288080833941,
-17.9200628991658));
#102461=CARTESIAN_POINT('Ctrl Pts',(-16.6289792851901,18.9810480340628,
-17.9228265846165));
#102462=CARTESIAN_POINT('Ctrl Pts',(-16.6362812414009,18.9258249278941,
-17.9261338217255));
#102463=CARTESIAN_POINT('Ctrl Pts',(-16.6373370215447,18.9181635907677,
-17.9265951617907));
#102464=CARTESIAN_POINT('Ctrl Pts',(-16.6390934126413,18.9059148907293,
-17.9273370070947));
#102465=CARTESIAN_POINT('Ctrl Pts',(-16.6397671807793,18.9013236663577,
-17.9276160371743));
#102466=CARTESIAN_POINT('Ctrl Pts',(-16.6409885716106,18.8931871149466,
-17.9281122978151));
#102467=CARTESIAN_POINT('Ctrl Pts',(-16.6415301168857,18.8896409214478,
-17.9283291822336));
#102468=CARTESIAN_POINT('Ctrl Pts',(-16.6426986196792,18.8821174250364,
-17.9287906053366));
#102469=CARTESIAN_POINT('Ctrl Pts',(-16.6433279011421,18.8781405914226,
-17.9290352678897));
#102470=CARTESIAN_POINT('Ctrl Pts',(-16.6450604254318,18.8673904112795,
-17.9296986501418));
#102471=CARTESIAN_POINT('Ctrl Pts',(-16.6461852541719,18.8606206630246,
-17.9301185645419));
#102472=CARTESIAN_POINT('Ctrl Pts',(-16.6519790006109,18.8267699403666,
-17.9322286700516));
#102473=CARTESIAN_POINT('Ctrl Pts',(-16.6571417652368,18.799777570755,-17.9339446224644));
#102474=CARTESIAN_POINT('Ctrl Pts',(-16.6736716341648,18.7216314860609,
-17.9389949988822));
#102475=CARTESIAN_POINT('Ctrl Pts',(-16.6864139312297,18.6707916448975,
-17.9423839237506));
#102476=CARTESIAN_POINT('Ctrl Pts',(-16.7400427017259,18.4861647181204,
-17.9549557968131));
#102477=CARTESIAN_POINT('Ctrl Pts',(-16.7922768025696,18.3560336899456,
-17.9643088319393));
#102478=CARTESIAN_POINT('Ctrl Pts',(-16.9003234586108,18.1488746997371,
-17.9794199513256));
#102479=CARTESIAN_POINT('Ctrl Pts',(-16.9491609184168,18.0687069461899,
-17.985337714743));
#102480=CARTESIAN_POINT('Ctrl Pts',(-17.0111142392699,17.980738045826,-17.9919033924047));
#102481=CARTESIAN_POINT('Ctrl Pts',(-17.0191787029997,17.9695219478511,
-17.9927421000779));
#102482=CARTESIAN_POINT('Ctrl Pts',(-17.0322729491753,17.9516814550668,
-17.9940789146032));
#102483=CARTESIAN_POINT('Ctrl Pts',(-17.0372328847845,17.9450065114993,
-17.9945797061127));
#102484=CARTESIAN_POINT('Ctrl Pts',(-17.046100363026,17.9332186329614,-17.9954652800468));
#102485=CARTESIAN_POINT('Ctrl Pts',(-17.0499921053631,17.9280939946098,
-17.9958506733455));
#102486=CARTESIAN_POINT('Ctrl Pts',(-17.0581403101354,17.9174654204216,
-17.9966508600066));
#102487=CARTESIAN_POINT('Ctrl Pts',(-17.0624006673761,17.9119645572096,
-17.9970654933702));
#102488=CARTESIAN_POINT('Ctrl Pts',(-17.07351521257,17.8977589637143,-17.9981376061424));
#102489=CARTESIAN_POINT('Ctrl Pts',(-17.080410808674,17.8890867872441,-17.998793431286));
#102490=CARTESIAN_POINT('Ctrl Pts',(-17.1104638535129,17.8518940291715,
-18.0016123670032));
#102491=CARTESIAN_POINT('Ctrl Pts',(-17.1342942784982,17.8239237572226,
-18.0037482259425));
#102492=CARTESIAN_POINT('Ctrl Pts',(-17.1993307128797,17.7514960808774,
-18.0093369078352));
#102493=CARTESIAN_POINT('Ctrl Pts',(-17.2417390417962,17.7081628290951,
-18.0127407925299));
#102494=CARTESIAN_POINT('Ctrl Pts',(-17.4051227625998,17.5549616247987,
-18.0251420618489));
#102495=CARTESIAN_POINT('Ctrl Pts',(-17.5368178052085,17.4573962770316,
-18.0337549347408));
#102496=CARTESIAN_POINT('Ctrl Pts',(-17.7277458751237,17.3475673864056,
-18.0461063587303));
#102497=CARTESIAN_POINT('Ctrl Pts',(-17.7782018912341,17.3211912185194,
-18.0493640336671));
#102498=CARTESIAN_POINT('Ctrl Pts',(-17.8376620574325,17.2930986114799,
-18.0532655104877));
#102499=CARTESIAN_POINT('Ctrl Pts',(-17.8456935988078,17.2893654939656,
-18.0537937880132));
#102500=CARTESIAN_POINT('Ctrl Pts',(-17.8578521232322,17.2838066363091,
-18.0545958068095));
#102501=CARTESIAN_POINT('Ctrl Pts',(-17.8619620223047,17.2819434617903,
-18.054867302408));
#102502=CARTESIAN_POINT('Ctrl Pts',(-17.8693303735596,17.2786314653362,
-18.0553548038713));
#102503=CARTESIAN_POINT('Ctrl Pts',(-17.8725865564176,17.2771777238878,
-18.0555705037516));
#102504=CARTESIAN_POINT('Ctrl Pts',(-17.8796473691379,17.2740467558734,
-18.0560388225161));
#102505=CARTESIAN_POINT('Ctrl Pts',(-17.8834532197337,17.2723725314838,
-18.056291614618));
#102506=CARTESIAN_POINT('Ctrl Pts',(-17.8941008105343,17.2677259595913,
-18.0569998117208));
#102507=CARTESIAN_POINT('Ctrl Pts',(-17.9009532867877,17.264778580328,-18.05745669459));
#102508=CARTESIAN_POINT('Ctrl Pts',(-17.9408923290698,17.2478496155883,
-18.06012541439));
#102509=CARTESIAN_POINT('Ctrl Pts',(-17.9743127827382,17.2346765987319,
-18.0623816493635));
#102510=CARTESIAN_POINT('Ctrl Pts',(-18.0829466238835,17.1950199450604,
-18.0697528868596));
#102511=CARTESIAN_POINT('Ctrl Pts',(-18.1593235042396,17.1719337179707,
-18.0749897188038));
#102512=CARTESIAN_POINT('Ctrl Pts',(-18.4177801794577,17.1094875973268,
-18.0925434068086));
#102513=CARTESIAN_POINT('Ctrl Pts',(-18.6037654070718,17.0898172640501,
-18.1048130633488));
#102514=CARTESIAN_POINT('Ctrl Pts',(-18.8119854703271,17.0953220357282,
-18.1176218690414));
#102515=CARTESIAN_POINT('Ctrl Pts',(-18.8340129485203,17.0962488444504,
-18.1189668128272));
#102516=CARTESIAN_POINT('Ctrl Pts',(-18.8644577863475,17.0980065888805,
-18.12081234421));
#102517=CARTESIAN_POINT('Ctrl Pts',(-18.8728900698285,17.098544097219,-18.1213220830863));
#102518=CARTESIAN_POINT('Ctrl Pts',(-18.8873796929115,17.0995548597065,
-18.1221956180186));
#102519=CARTESIAN_POINT('Ctrl Pts',(-18.8934385800864,17.1000037302157,
-18.1225601751643));
#102520=CARTESIAN_POINT('Ctrl Pts',(-18.9059260984624,17.1009829328824,
-18.123310093654));
#102521=CARTESIAN_POINT('Ctrl Pts',(-18.9123544122758,17.1015165770021,
-18.1236953468707));
#102522=CARTESIAN_POINT('Ctrl Pts',(-18.9273092110382,17.1028268926181,
-18.1245898067636));
#102523=CARTESIAN_POINT('Ctrl Pts',(-18.9358336618118,17.1036259283162,
-18.1250983050296));
#102524=CARTESIAN_POINT('Ctrl Pts',(-18.9631072862941,17.1063494168758,
-18.1267210427773));
#102525=CARTESIAN_POINT('Ctrl Pts',(-18.98183602836,17.1084725774156,-18.1278290314348));
#102526=CARTESIAN_POINT('Ctrl Pts',(-19.075264635266,17.1203297704018,-18.1333277643457));
#102527=CARTESIAN_POINT('Ctrl Pts',(-19.1494399374305,17.1337963651649,
-18.1375994757886));
#102528=CARTESIAN_POINT('Ctrl Pts',(-19.388582866453,17.1905395078047,-18.1512689195985));
#102529=CARTESIAN_POINT('Ctrl Pts',(-19.5490461983368,17.2497676839973,
-18.1602348803489));
#102530=CARTESIAN_POINT('Ctrl Pts',(-19.7075115497828,17.3311001337633,
-18.170209306771));
#102531=CARTESIAN_POINT('Ctrl Pts',(-19.714340044477,17.33465204729,-18.1706415377684));
#102532=CARTESIAN_POINT('Ctrl Pts',(-19.7666465489977,17.3622233010299,
-18.1739721943461));
#102533=CARTESIAN_POINT('Ctrl Pts',(-19.8112511998049,17.3878535145652,
-18.1769274241472));
#102534=CARTESIAN_POINT('Ctrl Pts',(-19.8621406753092,17.419614786967,-18.1804878549526));
#102535=CARTESIAN_POINT('Ctrl Pts',(-19.8693791899731,17.4241937838352,
-18.1809988849493));
#102536=CARTESIAN_POINT('Ctrl Pts',(-19.8802944931801,17.4311917790733,
-18.1817767893069));
#102537=CARTESIAN_POINT('Ctrl Pts',(-19.8839919529383,17.4335785880251,
-18.182041575074));
#102538=CARTESIAN_POINT('Ctrl Pts',(-19.8905259528545,17.4378253819979,
-18.1825118108566));
#102539=CARTESIAN_POINT('Ctrl Pts',(-19.8933654925071,17.4396806724508,
-18.1827169462355));
#102540=CARTESIAN_POINT('Ctrl Pts',(-19.8962227854308,17.4415573765363,
-18.1829241589128));
#102541=CARTESIAN_POINT('Ctrl Pts',(-19.8962449713584,17.4415719491156,
-18.1829257678984));
#102542=CARTESIAN_POINT('Ctrl Pts',(-19.8962888781377,17.4416007899762,
-18.1829289522362));
#102543=CARTESIAN_POINT('Ctrl Pts',(-19.8963105991032,17.4416150583076,
-18.1829305275947));
#102544=CARTESIAN_POINT('Ctrl Pts',(-19.8963536046105,17.4416433094208,
-18.1829336467506));
#102545=CARTESIAN_POINT('Ctrl Pts',(-19.8963748891621,17.4416572921861,
-18.1829351905469));
#102546=CARTESIAN_POINT('Ctrl Pts',(-19.8964170484326,17.4416849895688,
-18.1829382485014));
#102547=CARTESIAN_POINT('Ctrl Pts',(-19.8964379230461,17.4416987040959,
-18.1829397626504));
#102548=CARTESIAN_POINT('Ctrl Pts',(-19.8964792864155,17.4417258806912,
-18.1829427630446));
#102549=CARTESIAN_POINT('Ctrl Pts',(-19.896499775309,17.4417393428306,-18.1829442492981));
#102550=CARTESIAN_POINT('Ctrl Pts',(-19.8965403902076,17.4417660296852,
-18.1829471955629));
#102551=CARTESIAN_POINT('Ctrl Pts',(-19.8965605160865,17.4417792542996,
-18.1829486555635));
#102552=CARTESIAN_POINT('Ctrl Pts',(-19.8966004260652,17.4418054799222,
-18.1829515508495));
#102553=CARTESIAN_POINT('Ctrl Pts',(-19.8966202100444,17.4418184808345,
-18.1829529861248));
#102554=CARTESIAN_POINT('Ctrl Pts',(-19.8966594552758,17.4418442715238,
-18.1829558333384));
#102555=CARTESIAN_POINT('Ctrl Pts',(-19.8966789167048,17.4418570614016,
-18.1829572452882));
#102556=CARTESIAN_POINT('Ctrl Pts',(-19.8967175357825,17.441882442428,-18.1829600472218));
#102557=CARTESIAN_POINT('Ctrl Pts',(-19.8967366932362,17.4418950334342,
-18.1829614371902));
#102558=CARTESIAN_POINT('Ctrl Pts',(-19.8967747204561,17.441920027252,-18.1829641963253));
#102559=CARTESIAN_POINT('Ctrl Pts',(-19.8967935905899,17.4419324302919,
-18.1829655655174));
#102560=CARTESIAN_POINT('Ctrl Pts',(-19.8968310602207,17.441957059345,-18.1829682843338));
#102561=CARTESIAN_POINT('Ctrl Pts',(-19.8968496593935,17.4419692851327,
-18.1829696339336));
#102562=CARTESIAN_POINT('Ctrl Pts',(-19.8968866015324,17.4419935691303,
-18.1829723146094));
#102563=CARTESIAN_POINT('Ctrl Pts',(-19.8969049445855,17.4420056273859,
-18.1829736456908));
#102564=CARTESIAN_POINT('Ctrl Pts',(-19.8969413887515,17.4420295856634,
-18.1829762903623));
#102565=CARTESIAN_POINT('Ctrl Pts',(-19.8969594898772,17.4420414856832,
-18.1829776039525));
#102566=CARTESIAN_POINT('Ctrl Pts',(-19.8969954631084,17.4420651359514,
-18.1829802145768));
#102567=CARTESIAN_POINT('Ctrl Pts',(-19.897013335426,17.4420768863292,-18.1829815116254));
#102568=CARTESIAN_POINT('Ctrl Pts',(-19.8970488639132,17.4421002457469,
-18.1829840900982));
#102569=CARTESIAN_POINT('Ctrl Pts',(-19.8970665200289,17.4421118547419,
-18.1829853715177));
#102570=CARTESIAN_POINT('Ctrl Pts',(-19.8971016279526,17.4421349391516,
-18.1829879195895));
#102571=CARTESIAN_POINT('Ctrl Pts',(-19.897119079708,17.4421464145228,-18.1829891862372));
#102572=CARTESIAN_POINT('Ctrl Pts',(-19.8971537899676,17.4421692389291,
-18.1829917055657));
#102573=CARTESIAN_POINT('Ctrl Pts',(-19.8971710484817,17.4421805879625,
-18.1829929582466));
#102574=CARTESIAN_POINT('Ctrl Pts',(-19.8972053830992,17.4422031667976,
-18.1829954504262));
#102575=CARTESIAN_POINT('Ctrl Pts',(-19.8972224590889,17.442214396517,-18.1829966899162));
#102576=CARTESIAN_POINT('Ctrl Pts',(-19.8972564383126,17.4422367430508,
-18.1829991564131));
#102577=CARTESIAN_POINT('Ctrl Pts',(-19.8972733416852,17.4422478599493,
-18.1830003834295));
#102578=CARTESIAN_POINT('Ctrl Pts',(-19.8973069854023,17.442269987218,-18.1830028256838));
#102579=CARTESIAN_POINT('Ctrl Pts',(-19.8973237257178,17.4422809975625,
-18.183004040919));
#102580=CARTESIAN_POINT('Ctrl Pts',(-19.8973570527172,17.4423029178835,
-18.1830064602913));
#102581=CARTESIAN_POINT('Ctrl Pts',(-19.8973736392493,17.442313827754,-18.1830076644169));
#102582=CARTESIAN_POINT('Ctrl Pts',(-19.8974066666262,17.4423355523342,
-18.1830100621453));
#102583=CARTESIAN_POINT('Ctrl Pts',(-19.897423107775,17.4423463672379,-18.1830112557697));
#102584=CARTESIAN_POINT('Ctrl Pts',(-19.8974558529991,17.4423679075333,
-18.1830136331196));
#102585=CARTESIAN_POINT('Ctrl Pts',(-19.8974721570837,17.4423786329256,
-18.1830148168454));
#102586=CARTESIAN_POINT('Ctrl Pts',(-19.8975046361975,17.4423999994567,
-18.1830171749789));
#102587=CARTESIAN_POINT('Ctrl Pts',(-19.8975208111424,17.4424106405348,
-18.1830183493801));
#102588=CARTESIAN_POINT('Ctrl Pts',(-19.9010488516823,17.4447317165572,
-18.1832745125599));
#102589=CARTESIAN_POINT('Ctrl Pts',(-19.9045537927668,17.447052583312,-18.183530204642));
#102590=CARTESIAN_POINT('Ctrl Pts',(-19.9146662813489,17.453792181521,-18.1842713686692));
#102591=CARTESIAN_POINT('Ctrl Pts',(-19.9212557994442,17.4582376523508,
-18.1847585891006));
#102592=CARTESIAN_POINT('Ctrl Pts',(-19.9651742349692,17.4882275328669,
-18.1880336327274));
#102593=CARTESIAN_POINT('Ctrl Pts',(-20.0016984188908,17.5149236401384,
-18.1908920390145));
#102594=CARTESIAN_POINT('Ctrl Pts',(-20.1326696719915,17.6172472167952,
-18.201566640356));
#102595=CARTESIAN_POINT('Ctrl Pts',(-20.2214394250199,17.6997597580939,
-18.2096352593239));
#102596=CARTESIAN_POINT('Ctrl Pts',(-20.3997272059662,17.8964923539837,
-18.2271158178451));
#102597=CARTESIAN_POINT('Ctrl Pts',(-20.4855739095568,18.0132601995372,
-18.2364224381902));
#102598=CARTESIAN_POINT('Ctrl Pts',(-20.566111389986,18.1502165884514,-18.246123913703));
#102599=CARTESIAN_POINT('Ctrl Pts',(-20.573236888791,18.1626196900897,-18.2469927641882));
#102600=CARTESIAN_POINT('Ctrl Pts',(-20.5843753119834,18.1824710732244,
-18.2483681911947));
#102601=CARTESIAN_POINT('Ctrl Pts',(-20.5884701466914,18.1898726687203,
-18.2488777032028));
#102602=CARTESIAN_POINT('Ctrl Pts',(-20.5956126063765,18.2029676583951,
-18.249773373814));
#102603=CARTESIAN_POINT('Ctrl Pts',(-20.5986787282876,18.2086507895718,
-18.2501601898928));
#102604=CARTESIAN_POINT('Ctrl Pts',(-20.6049655425978,18.2204322342301,
-18.2509582030556));
#102605=CARTESIAN_POINT('Ctrl Pts',(-20.6081825385662,18.2265324413498,
-18.2513692654643));
#102606=CARTESIAN_POINT('Ctrl Pts',(-20.6163612988826,18.2422267535564,
-18.2524214299886));
#102607=CARTESIAN_POINT('Ctrl Pts',(-20.6212795907519,18.251843383262,-18.2530609939365));
#102608=CARTESIAN_POINT('Ctrl Pts',(-20.6414807697391,18.2920993416723,
-18.2557173388225));
#102609=CARTESIAN_POINT('Ctrl Pts',(-20.6560933274745,18.3230705305152,
-18.2577106884445));
#102610=CARTESIAN_POINT('Ctrl Pts',(-20.6889342113013,18.3972907919699,
-18.262380301961));
#102611=CARTESIAN_POINT('Ctrl Pts',(-20.706487756653,18.4408166001664,-18.2650344917798));
#102612=CARTESIAN_POINT('Ctrl Pts',(-20.7225806130935,18.4848897155193,
-18.2676549617288));
#102613=CARTESIAN_POINT('Ctrl Pts',(-20.7225806765445,18.484889889291,-18.0457834329553));
#102614=CARTESIAN_POINT('Ctrl Pts',(-20.6985951200092,18.4192012099311,
-18.0412345298138));
#102615=CARTESIAN_POINT('Ctrl Pts',(-20.6713591064839,18.3547130434287,
-18.036607855267));
#102616=CARTESIAN_POINT('Ctrl Pts',(-20.6100060409437,18.227448935695,-18.0272719316093));
#102617=CARTESIAN_POINT('Ctrl Pts',(-20.5758218726607,18.1648334862876,
-18.0225709514097));
#102618=CARTESIAN_POINT('Ctrl Pts',(-20.4890913966248,18.0234447836004,
-18.011794881422));
#102619=CARTESIAN_POINT('Ctrl Pts',(-20.4342892301375,17.9462257578456,
-18.005787549224));
#102620=CARTESIAN_POINT('Ctrl Pts',(-20.361084885175,17.8564764069634,-17.9986728828564));
#102621=CARTESIAN_POINT('Ctrl Pts',(-20.3474241242239,17.8402330487983,
-17.9973791311543));
#102622=CARTESIAN_POINT('Ctrl Pts',(-20.328911847463,17.8188812174145,-17.9956697355559));
#102623=CARTESIAN_POINT('Ctrl Pts',(-20.324276160027,17.8135880196861,-17.9952452354522));
#102624=CARTESIAN_POINT('Ctrl Pts',(-20.3150435150256,17.8031512905271,
-17.9944067364924));
#102625=CARTESIAN_POINT('Ctrl Pts',(-20.3104476374453,17.7980069238265,
-17.9939927000969));
#102626=CARTESIAN_POINT('Ctrl Pts',(-20.301501530191,17.7880911338653,-17.993193177619));
#102627=CARTESIAN_POINT('Ctrl Pts',(-20.2971544606214,17.7833169742058,
-17.9928075651126));
#102628=CARTESIAN_POINT('Ctrl Pts',(-20.2870651929699,17.7723377813853,
-17.9919191768738));
#102629=CARTESIAN_POINT('Ctrl Pts',(-20.2813075066278,17.7661470815407,
-17.9914170670517));
#102630=CARTESIAN_POINT('Ctrl Pts',(-20.2657196142296,17.7495869254381,
-17.9900705803206));
#102631=CARTESIAN_POINT('Ctrl Pts',(-20.2558211518402,17.7392821099702,
-17.9892291439662));
#102632=CARTESIAN_POINT('Ctrl Pts',(-20.1641189056051,17.6457298162365,
-17.9815546374228));
#102633=CARTESIAN_POINT('Ctrl Pts',(-20.0756615354366,17.5692751728815,
-17.9750375279399));
#102634=CARTESIAN_POINT('Ctrl Pts',(-19.8501150346933,17.404801296368,-17.959755147767));
#102635=CARTESIAN_POINT('Ctrl Pts',(-19.7083291484311,17.3245383569685,
-17.9511720259872));
#102636=CARTESIAN_POINT('Ctrl Pts',(-19.5285298595371,17.2484785602851,
-17.9399673976099));
#102637=CARTESIAN_POINT('Ctrl Pts',(-19.4979839399778,17.2363870329634,
-17.9380520963707));
#102638=CARTESIAN_POINT('Ctrl Pts',(-19.4603865151649,17.2225071199732,
-17.9356661433535));
#102639=CARTESIAN_POINT('Ctrl Pts',(-19.4535892950707,17.2200372815341,
-17.9352336646788));
#102640=CARTESIAN_POINT('Ctrl Pts',(-19.4428808250131,17.2162082513649,
-17.9345503685363));
#102641=CARTESIAN_POINT('Ctrl Pts',(-19.4389779416827,17.2148255974089,
-17.9343009216384));
#102642=CARTESIAN_POINT('Ctrl Pts',(-19.4317044484996,17.2122728468447,
-17.933835244512));
#102643=CARTESIAN_POINT('Ctrl Pts',(-19.4283349281391,17.2110998182016,
-17.9336191910398));
#102644=CARTESIAN_POINT('Ctrl Pts',(-19.4206744250733,17.2084546662967,
-17.9331272720577));
#102645=CARTESIAN_POINT('Ctrl Pts',(-19.4163816851902,17.206987820791,-17.9328511001117));
#102646=CARTESIAN_POINT('Ctrl Pts',(-19.403587754782,17.2026619599005,-17.9320265497939));
#102647=CARTESIAN_POINT('Ctrl Pts',(-19.395073199251,17.1998432026886,-17.9314758878544));
#102648=CARTESIAN_POINT('Ctrl Pts',(-19.3293524721863,17.1785486865685,
-17.9272122412649));
#102649=CARTESIAN_POINT('Ctrl Pts',(-19.2714057866816,17.1624647890181,
-17.9233761802053));
#102650=CARTESIAN_POINT('Ctrl Pts',(-19.0646095532864,17.1144434065282,
-17.9095986480423));
#102651=CARTESIAN_POINT('Ctrl Pts',(-18.9130774368891,17.0961033169612,
-17.8993834197686));
#102652=CARTESIAN_POINT('Ctrl Pts',(-18.6951686767517,17.0933362306514,
-17.8852648883115));
#102653=CARTESIAN_POINT('Ctrl Pts',(-18.6294493227224,17.0955619352564,
-17.8810743215709));
#102654=CARTESIAN_POINT('Ctrl Pts',(-18.5382841715414,17.1029092676702,
-17.8753676862236));
#102655=CARTESIAN_POINT('Ctrl Pts',(-18.5126726798799,17.1054441282285,
-17.8737760310758));
#102656=CARTESIAN_POINT('Ctrl Pts',(-18.4682385804139,17.1106616895351,
-17.8710341334243));
#102657=CARTESIAN_POINT('Ctrl Pts',(-18.449394529272,17.1131320552646,-17.8698774440636));
#102658=CARTESIAN_POINT('Ctrl Pts',(-18.4219756719704,17.1171027943525,
-17.8682029035969));
#102659=CARTESIAN_POINT('Ctrl Pts',(-18.4133732116025,17.118402772822,-17.8676787497316));
#102660=CARTESIAN_POINT('Ctrl Pts',(-18.3983851880166,17.1207623123725,
-17.8667675802522));
#102661=CARTESIAN_POINT('Ctrl Pts',(-18.3919960637012,17.1217981902648,
-17.8663798197476));
#102662=CARTESIAN_POINT('Ctrl Pts',(-18.3796570304333,17.123856855543,-17.8656321849995));
#102663=CARTESIAN_POINT('Ctrl Pts',(-18.3737065559855,17.1248758232317,
-17.8652721936421));
#102664=CARTESIAN_POINT('Ctrl Pts',(-18.3595833261947,17.1273565364797,
-17.8644190447225));
#102665=CARTESIAN_POINT('Ctrl Pts',(-18.3514146116188,17.1288409397269,
-17.8639266110314));
#102666=CARTESIAN_POINT('Ctrl Pts',(-18.3224743261575,17.1342759749742,
-17.8621854505945));
#102667=CARTESIAN_POINT('Ctrl Pts',(-18.3017530076761,17.1384897728596,
-17.8609450944425));
#102668=CARTESIAN_POINT('Ctrl Pts',(-18.0916287167026,17.1845083349567,
-17.8484221103672));
#102669=CARTESIAN_POINT('Ctrl Pts',(-17.9087686838356,17.2518400501761,
-17.838091247687));
#102670=CARTESIAN_POINT('Ctrl Pts',(-17.6716117867266,17.378346812602,-17.8234097502943));
#102671=CARTESIAN_POINT('Ctrl Pts',(-17.6075183318053,17.41703128546,-17.8192802040188));
#102672=CARTESIAN_POINT('Ctrl Pts',(-17.5170123390496,17.4784226366979,
-17.8130147588829));
#102673=CARTESIAN_POINT('Ctrl Pts',(-17.4888937658892,17.4985183381089,
-17.8110023534249));
#102674=CARTESIAN_POINT('Ctrl Pts',(-17.455388180843,17.5237255100739,-17.8085066242993));
#102675=CARTESIAN_POINT('Ctrl Pts',(-17.4495181962696,17.5281898857285,
-17.8080656481993));
#102676=CARTESIAN_POINT('Ctrl Pts',(-17.4403901534224,17.5352077398579,
-17.8073738457691));
#102677=CARTESIAN_POINT('Ctrl Pts',(-17.4371159894631,17.5377403080053,
-17.8071244716997));
#102678=CARTESIAN_POINT('Ctrl Pts',(-17.4310334042903,17.5424737695482,
-17.8066588582191));
#102679=CARTESIAN_POINT('Ctrl Pts',(-17.4282231122649,17.5446721660874,
-17.8064427951141));
#102680=CARTESIAN_POINT('Ctrl Pts',(-17.4218510184215,17.5496828582446,
-17.8059507598805));
#102681=CARTESIAN_POINT('Ctrl Pts',(-17.4182927095791,17.5524994964141,
-17.8056744807194));
#102682=CARTESIAN_POINT('Ctrl Pts',(-17.4077225426793,17.5609219116814,
-17.8048493201447));
#102683=CARTESIAN_POINT('Ctrl Pts',(-17.4007373596164,17.5665607896425,
-17.8042981502665));
#102684=CARTESIAN_POINT('Ctrl Pts',(-17.3470609360387,17.6104585739092,
-17.800018609476));
#102685=CARTESIAN_POINT('Ctrl Pts',(-17.3019937264599,17.6506508648063,
-17.7961661517238));
#102686=CARTESIAN_POINT('Ctrl Pts',(-17.1528658178934,17.7955552030458,
-17.7826699821423));
#102687=CARTESIAN_POINT('Ctrl Pts',(-17.0580649604111,17.9091879598663,
-17.7727712742713));
#102688=CARTESIAN_POINT('Ctrl Pts',(-16.9186473011171,18.1170487009912,
-17.7565251032165));
#102689=CARTESIAN_POINT('Ctrl Pts',(-16.8677190120586,18.206392833318,-17.7500258788693));
#102690=CARTESIAN_POINT('Ctrl Pts',(-16.8170973498081,18.3124499183923,
-17.7428593430256));
#102691=CARTESIAN_POINT('Ctrl Pts',(-16.8108625941288,18.325872576935,-17.7419617195481));
#102692=CARTESIAN_POINT('Ctrl Pts',(-16.8015710638977,18.3464378377419,
-17.740600425083));
#102693=CARTESIAN_POINT('Ctrl Pts',(-16.7984120934352,18.3535335085488,
-17.7401332474842));
#102694=CARTESIAN_POINT('Ctrl Pts',(-16.7927370135165,18.3664720351234,
-17.7392858826598));
#102695=CARTESIAN_POINT('Ctrl Pts',(-16.7902080645199,18.3723091278191,
-17.7389052593423));
#102696=CARTESIAN_POINT('Ctrl Pts',(-16.7848064214292,18.3849323904007,
-17.7380856562206));
#102697=CARTESIAN_POINT('Ctrl Pts',(-16.7819427658821,18.3917223552396,
-17.7376469882315));
#102698=CARTESIAN_POINT('Ctrl Pts',(-16.7742770997471,18.4101666636094,
-17.7364612273543));
#102699=CARTESIAN_POINT('Ctrl Pts',(-16.7695435781595,18.4218492821528,
-17.7357164582436));
#102700=CARTESIAN_POINT('Ctrl Pts',(-16.747061600226,18.4787922142323,-17.7321159094484));
#102701=CARTESIAN_POINT('Ctrl Pts',(-16.7307706102398,18.5246145458371,
-17.7293092478705));
#102702=CARTESIAN_POINT('Ctrl Pts',(-16.7037373127509,18.6098455860685,
-17.7242274497607));
#102703=CARTESIAN_POINT('Ctrl Pts',(-16.6925298605576,18.6490808565139,
-17.7219404679047));
#102704=CARTESIAN_POINT('Ctrl Pts',(-16.64929393253,18.8188798706058,-17.7122163846758));
#102705=CARTESIAN_POINT('Ctrl Pts',(-16.6286077305665,18.9520014028685,
-17.7050482410997));
#102706=CARTESIAN_POINT('Ctrl Pts',(-16.6169859545199,19.148775679534,-17.6942149502253));
#102707=CARTESIAN_POINT('Ctrl Pts',(-16.6160720171754,19.2114959085012,
-17.6907228035505));
#102708=CARTESIAN_POINT('Ctrl Pts',(-16.6188649731704,19.3050698584071,
-17.6853380267219));
#102709=CARTESIAN_POINT('Ctrl Pts',(-16.6204647157198,19.3359547721859,
-17.6835321195927));
#102710=CARTESIAN_POINT('Ctrl Pts',(-16.6232647715201,19.3739006052262,
-17.6812660780505));
#102711=CARTESIAN_POINT('Ctrl Pts',(-16.6238252382374,19.3810067159219,
-17.6808396716993));
#102712=CARTESIAN_POINT('Ctrl Pts',(-16.6247633415222,19.3921805926096,
-17.6801657690125));
#102713=CARTESIAN_POINT('Ctrl Pts',(-16.6251168889131,19.3962504027756,
-17.6799196046971));
#102714=CARTESIAN_POINT('Ctrl Pts',(-16.6258019820485,19.4038805408688,
-17.6794567146712));
#102715=CARTESIAN_POINT('Ctrl Pts',(-16.6261307690229,19.4074410607812,
-17.6792401451599));
#102716=CARTESIAN_POINT('Ctrl Pts',(-16.626904994002,19.4155995489266,-17.6787426138371));
#102717=CARTESIAN_POINT('Ctrl Pts',(-16.6273564611378,19.4201968904136,
-17.6784613171599));
#102718=CARTESIAN_POINT('Ctrl Pts',(-16.6288020339352,19.4344379411968,
-17.677587129888));
#102719=CARTESIAN_POINT('Ctrl Pts',(-16.6298473244732,19.4440761672906,
-17.6769914736153));
#102720=CARTESIAN_POINT('Ctrl Pts',(-16.6423861071656,19.552724100822,-17.6702341536958));
#102721=CARTESIAN_POINT('Ctrl Pts',(-16.6607910025215,19.650799697077,-17.6637390136366));
#102722=CARTESIAN_POINT('Ctrl Pts',(-16.715531310881,19.8598750215869,-17.6495000049824));
#102723=CARTESIAN_POINT('Ctrl Pts',(-16.7542821631584,19.9699302654033,
-17.641760308951));
#102724=CARTESIAN_POINT('Ctrl Pts',(-16.8274376647242,20.1332884303513,
-17.6301901867847));
#102725=CARTESIAN_POINT('Ctrl Pts',(-16.8554998142507,20.1891789740647,
-17.626212585505));
#102726=CARTESIAN_POINT('Ctrl Pts',(-16.904317991302,20.2765342442579,-17.6199755853184));
#102727=CARTESIAN_POINT('Ctrl Pts',(-16.9235093489325,20.3088266549785,
-17.6176649915191));
#102728=CARTESIAN_POINT('Ctrl Pts',(-16.9495089489827,20.3500370396981,
-17.6147077975544));
#102729=CARTESIAN_POINT('Ctrl Pts',(-16.9555418644964,20.3594338712831,
-17.6140328915913));
#102730=CARTESIAN_POINT('Ctrl Pts',(-16.9654645930722,20.3746237328452,
-17.6129408024179));
#102731=CARTESIAN_POINT('Ctrl Pts',(-16.9693091337935,20.3804459481904,
-17.6125219399504));
#102732=CARTESIAN_POINT('Ctrl Pts',(-16.9767512074393,20.3915960388531,
-17.6117192175117));
#102733=CARTESIAN_POINT('Ctrl Pts',(-16.9803443580061,20.3969267332437,
-17.6113351988377));
#102734=CARTESIAN_POINT('Ctrl Pts',(-16.9886176291906,20.409080899034,-17.6104590075412));
#102735=CARTESIAN_POINT('Ctrl Pts',(-16.9933136022126,20.4158934925906,
-17.6099674420141));
#102736=CARTESIAN_POINT('Ctrl Pts',(-17.0058745942221,20.4338894063995,
-17.6086676261772));
#102737=CARTESIAN_POINT('Ctrl Pts',(-17.0138082928204,20.4450244819346,
-17.6078620024366));
#102738=CARTESIAN_POINT('Ctrl Pts',(-17.0737687035965,20.5274778792088,
-17.6018845299312));
#102739=CARTESIAN_POINT('Ctrl Pts',(-17.1301061482496,20.5955610073797,
-17.5968867281685));
#102740=CARTESIAN_POINT('Ctrl Pts',(-17.2865870583059,20.7622508795801,
-17.5842174296299));
#102741=CARTESIAN_POINT('Ctrl Pts',(-17.3925690089595,20.8547593171523,
-17.576753249044));
#102742=CARTESIAN_POINT('Ctrl Pts',(-17.5527036666521,20.9686644804882,
-17.5659056486565));
#102743=CARTESIAN_POINT('Ctrl Pts',(-17.5997605933034,20.9993918859522,
-17.5627599921487));
#102744=CARTESIAN_POINT('Ctrl Pts',(-17.6726904283673,21.0429769854792,
-17.5578610120988));
#102745=CARTESIAN_POINT('Ctrl Pts',(-17.69769800557,21.0572382492745,-17.5561770558546));
#102746=CARTESIAN_POINT('Ctrl Pts',(-17.7291086790429,21.0743118306277,
-17.5540470883347));
#102747=CARTESIAN_POINT('Ctrl Pts',(-17.7352465173272,21.0776089635654,
-17.5536301869386));
#102748=CARTESIAN_POINT('Ctrl Pts',(-17.744977300651,21.0827744253641,-17.552967971154));
#102749=CARTESIAN_POINT('Ctrl Pts',(-17.7485595854915,21.0846628800549,
-17.5527239127521));
#102750=CARTESIAN_POINT('Ctrl Pts',(-17.7553209733597,21.0882024919853,
-17.5522627134764));
#102751=CARTESIAN_POINT('Ctrl Pts',(-17.7584988567404,21.0898558624569,
-17.5520457152807));
#102752=CARTESIAN_POINT('Ctrl Pts',(-17.7657675796006,21.0936141787162,
-17.5515488612772));
#102753=CARTESIAN_POINT('Ctrl Pts',(-17.7698610888007,21.0957138575405,
-17.5512686790194));
#102754=CARTESIAN_POINT('Ctrl Pts',(-17.7807336208873,21.1012460019208,
-17.5505235888855));
#102755=CARTESIAN_POINT('Ctrl Pts',(-17.7875242640531,21.1046553051206,
-17.5500572899114));
#102756=CARTESIAN_POINT('Ctrl Pts',(-17.8348275142629,21.1280863273992,
-17.54680333902));
#102757=CARTESIAN_POINT('Ctrl Pts',(-17.8759507443142,21.1468414080146,
-17.5439455470446));
#102758=CARTESIAN_POINT('Ctrl Pts',(-17.9231850083496,21.1665828239092,
-17.5406558110589));
#102759=CARTESIAN_POINT('Ctrl Pts',(-17.9287408809804,21.1688771365707,
-17.5402687445102));
#102760=CARTESIAN_POINT('Ctrl Pts',(-18.080145808931,21.2306467415208,-17.5297188583977));
#102761=CARTESIAN_POINT('Ctrl Pts',(-18.2321701161883,21.2736848361996,
-17.5191274540402));
#102762=CARTESIAN_POINT('Ctrl Pts',(-18.4891774617685,21.3163169586241,
-17.502214753407));
#102763=CARTESIAN_POINT('Ctrl Pts',(-18.5918926189619,21.3257360424972,
-17.4956954335792));
#102764=CARTESIAN_POINT('Ctrl Pts',(-18.7097044899123,21.327912372036,-17.4885097256611));
#102765=CARTESIAN_POINT('Ctrl Pts',(-18.7245122324675,21.3280305294063,
-17.4876115975902));
#102766=CARTESIAN_POINT('Ctrl Pts',(-18.747088938308,21.327973791018,-17.4862496984533));
#102767=CARTESIAN_POINT('Ctrl Pts',(-18.7548574922321,21.3279115049266,
-17.4857824159939));
#102768=CARTESIAN_POINT('Ctrl Pts',(-18.7689864179481,21.3277204392288,
-17.4849349404553));
#102769=CARTESIAN_POINT('Ctrl Pts',(-18.7753468598717,21.3276057511583,
-17.4845543107185));
#102770=CARTESIAN_POINT('Ctrl Pts',(-18.7890725087859,21.3272963641361,
-17.483734782192));
#102771=CARTESIAN_POINT('Ctrl Pts',(-18.796437428351,21.327091881683,-17.4832961947411));
#102772=CARTESIAN_POINT('Ctrl Pts',(-18.8163930810902,21.3264335508718,
-17.4821108656093));
#102773=CARTESIAN_POINT('Ctrl Pts',(-18.8289811992942,21.3259057449613,
-17.4813664448226));
#102774=CARTESIAN_POINT('Ctrl Pts',(-18.8900493571073,21.3227988792562,
-17.4777701752275));
#102775=CARTESIAN_POINT('Ctrl Pts',(-18.9384378558316,21.3186649645855,
-17.4749673007283));
#102776=CARTESIAN_POINT('Ctrl Pts',(-19.0271581928347,21.3080008014141,
-17.4698884559444));
#102777=CARTESIAN_POINT('Ctrl Pts',(-19.067524120617,21.3019605433582,-17.4676007725183));
#102778=CARTESIAN_POINT('Ctrl Pts',(-19.2400316756001,21.2710237990694,
-17.4578740025092));
#102779=CARTESIAN_POINT('Ctrl Pts',(-19.3698054401631,21.2347383362235,
-17.4507041686132));
#102780=CARTESIAN_POINT('Ctrl Pts',(-19.5537914738126,21.1638352688755,
-17.4398678578979));
#102781=CARTESIAN_POINT('Ctrl Pts',(-19.6112868413681,21.1386904046713,
-17.4363743124226));
#102782=CARTESIAN_POINT('Ctrl Pts',(-19.6953392007928,21.0973914704745,
-17.4309875850741));
#102783=CARTESIAN_POINT('Ctrl Pts',(-19.7227978203557,21.0831443539837,
-17.4291812000981));
#102784=CARTESIAN_POINT('Ctrl Pts',(-19.7561871347506,21.0648806008284,
-17.4269146260797));
#102785=CARTESIAN_POINT('Ctrl Pts',(-19.7624240518356,21.0614280010019,
-17.4264881838816));
#102786=CARTESIAN_POINT('Ctrl Pts',(-19.7722074697831,21.055947408298,-17.4258142371316));
#102787=CARTESIAN_POINT('Ctrl Pts',(-19.7757658076228,21.0539405012419,
-17.4255680648901));
#102788=CARTESIAN_POINT('Ctrl Pts',(-19.7824276929388,21.050157730718,-17.4251051683479));
#102789=CARTESIAN_POINT('Ctrl Pts',(-19.785532557818,21.0483842997452,-17.4248886002967));
#102790=CARTESIAN_POINT('Ctrl Pts',(-19.7926381769983,21.0443018158387,
-17.4243910835013));
#102791=CARTESIAN_POINT('Ctrl Pts',(-19.7966358651826,21.0419875354163,
-17.4241097999639));
#102792=CARTESIAN_POINT('Ctrl Pts',(-19.808999337092,21.0347761359002,-17.42323569332));
#102793=CARTESIAN_POINT('Ctrl Pts',(-19.8173389445984,21.0298347070425,
-17.4226401052558));
#102794=CARTESIAN_POINT('Ctrl Pts',(-19.9078136176254,20.9753831851072,
-17.4161158807588));
#102795=CARTESIAN_POINT('Ctrl Pts',(-19.9865184503359,20.9204091419468,
-17.4098781014981));
#102796=CARTESIAN_POINT('Ctrl Pts',(-20.1599363469923,20.7808570304567,
-17.3952250866863));
#102797=CARTESIAN_POINT('Ctrl Pts',(-20.2513329036141,20.6927053916774,
-17.3867950043775));
#102798=CARTESIAN_POINT('Ctrl Pts',(-20.3724509589717,20.552850896293,-17.3748732027538));
#102799=CARTESIAN_POINT('Ctrl Pts',(-20.4087702461443,20.5072372297808,
-17.3711748545664));
#102800=CARTESIAN_POINT('Ctrl Pts',(-20.4642424642891,20.43133853269,-17.3653244785605));
#102801=CARTESIAN_POINT('Ctrl Pts',(-20.4845890000875,20.4019674707893,
-17.3631287712228));
#102802=CARTESIAN_POINT('Ctrl Pts',(-20.5101992674296,20.362922510238,-17.3602957191564));
#102803=CARTESIAN_POINT('Ctrl Pts',(-20.5161437703807,20.3537042031934,
-17.3596329248477));
#102804=CARTESIAN_POINT('Ctrl Pts',(-20.5257284845305,20.3385841907032,
-17.3585555425984));
#102805=CARTESIAN_POINT('Ctrl Pts',(-20.5294117639498,20.3327101537616,
-17.3581393588845));
#102806=CARTESIAN_POINT('Ctrl Pts',(-20.5364622496124,20.3213424492668,
-17.3573384630007));
#102807=CARTESIAN_POINT('Ctrl Pts',(-20.5398333574654,20.3158513033001,
-17.3569536098317));
#102808=CARTESIAN_POINT('Ctrl Pts',(-20.5475262959706,20.3031911209873,
-17.3560708879837));
#102809=CARTESIAN_POINT('Ctrl Pts',(-20.5518307988009,20.2960116409249,
-17.3555736579241));
#102810=CARTESIAN_POINT('Ctrl Pts',(-20.5632212069067,20.2767555181233,
-17.3542488382614));
#102811=CARTESIAN_POINT('Ctrl Pts',(-20.5702301503391,20.2646336636768,
-17.3534240412733));
#102812=CARTESIAN_POINT('Ctrl Pts',(-20.6269890232292,20.1641832970636,
-17.3466623069611));
#102813=CARTESIAN_POINT('Ctrl Pts',(-20.6704590839962,20.0724498634047,
-17.3409589440621));
#102814=CARTESIAN_POINT('Ctrl Pts',(-20.7617045426689,19.8376937515129,
-17.3270883305746));
#102815=CARTESIAN_POINT('Ctrl Pts',(-20.801105109675,19.6920424586304,-17.3191197810486));
#102816=CARTESIAN_POINT('Ctrl Pts',(-20.8309456068991,19.504382681921,-17.3084711625934));
#102817=CARTESIAN_POINT('Ctrl Pts',(-20.8360618079081,19.4651457553009,
-17.3062221924579));
#102818=CARTESIAN_POINT('Ctrl Pts',(-20.8416060196543,19.4107834663772,
-17.3030475437583));
#102819=CARTESIAN_POINT('Ctrl Pts',(-20.8429760799789,19.3957604796477,
-17.3021640596538));
#102820=CARTESIAN_POINT('Ctrl Pts',(-20.8450676744407,19.3697556892886,
-17.3006221200066));
#102821=CARTESIAN_POINT('Ctrl Pts',(-20.8458643545028,19.3587803486912,
-17.2999674604093));
#102822=CARTESIAN_POINT('Ctrl Pts',(-20.8468897379978,19.3429455029684,
-17.2990167057978));
#102823=CARTESIAN_POINT('Ctrl Pts',(-20.8471873277521,19.338090430167,-17.2987243535215));
#102824=CARTESIAN_POINT('Ctrl Pts',(-20.8476764825848,19.3296328035305,
-17.29821353356));
#102825=CARTESIAN_POINT('Ctrl Pts',(-20.8478755777301,19.3260306778402,
-17.2979954875501));
#102826=CARTESIAN_POINT('Ctrl Pts',(-20.8482735902958,19.3184793960689,
-17.2975373444059));
#102827=CARTESIAN_POINT('Ctrl Pts',(-20.8484706505186,19.3145302018941,
-17.2972971491645));
#102828=CARTESIAN_POINT('Ctrl Pts',(-20.8489642021392,19.3040493141564,
-17.2966581533865));
#102829=CARTESIAN_POINT('Ctrl Pts',(-20.8492414964717,19.2975168204044,
-17.2962583014388));
#102830=CARTESIAN_POINT('Ctrl Pts',(-20.8502933314452,19.2696966842009,
-17.29454901154));
#102831=CARTESIAN_POINT('Ctrl Pts',(-20.8507767753518,19.2484001129417,
-17.2932245199956));
#102832=CARTESIAN_POINT('Ctrl Pts',(-20.8509781232099,19.2219268983958,
-17.2915611593869));
#102833=CARTESIAN_POINT('Ctrl Pts',(-20.850998506442,19.216752877949,-17.2912352624917));
#102834=CARTESIAN_POINT('Ctrl Pts',(-20.8510131828748,19.1630721313074,
-17.287846074883));
#102835=CARTESIAN_POINT('Ctrl Pts',(-20.8493592891271,19.1145823847139,
-17.284717231432));
#102836=CARTESIAN_POINT('Ctrl Pts',(-20.8326138661285,18.8703421985657,
-17.2687465213729));
#102837=CARTESIAN_POINT('Ctrl Pts',(-20.7920024891764,18.6772600447215,
-17.2555538816513));
#102838=CARTESIAN_POINT('Ctrl Pts',(-20.7244363838141,18.4899872681561,
-17.2430396061983));
#102839=CARTESIAN_POINT('Ctrl Pts',(-20.723510942024,18.4874375847904,-17.2428692571384));
#102840=CARTESIAN_POINT('Ctrl Pts',(-20.7225806138883,18.484889717696,-17.2426990599955));
#102841=CARTESIAN_POINT('Origin',(-18.734,19.211,0.));
#102842=CARTESIAN_POINT('',(-20.7225806308032,18.4848897640204,-16.4437314734851));
#102843=CARTESIAN_POINT('',(-20.7225806137285,18.4848897172584,-16.6645990097762));
#102844=CARTESIAN_POINT('',(-20.7225806137986,18.4848897174502,0.));
#102845=CARTESIAN_POINT('',(-20.850999201232,19.209903974194,-16.7126929569557));
#102846=CARTESIAN_POINT('Ctrl Pts',(-20.7225806137285,18.4848897172584,
-16.6645990097762));
#102847=CARTESIAN_POINT('Ctrl Pts',(-20.7243922735201,18.4898512659733,
-16.6649340211793));
#102848=CARTESIAN_POINT('Ctrl Pts',(-20.7261853754752,18.4948196247617,
-16.665269794044));
#102849=CARTESIAN_POINT('Ctrl Pts',(-20.7539879299496,18.5727678309291,
-16.6705418857637));
#102850=CARTESIAN_POINT('Ctrl Pts',(-20.7759887406123,18.6471100343595,
-16.6756251051418));
#102851=CARTESIAN_POINT('Ctrl Pts',(-20.8317361364545,18.8821735502559,
-16.6915678158184));
#102852=CARTESIAN_POINT('Ctrl Pts',(-20.8509145479737,19.0457465062896,
-16.7024244527962));
#102853=CARTESIAN_POINT('Ctrl Pts',(-20.8509997150783,19.2099016565369,
-16.7126937055852));
#102854=CARTESIAN_POINT('Ctrl Pts',(-20.8509997162505,19.2099039182537,
-16.7126938470741));
#102855=CARTESIAN_POINT('Ctrl Pts',(-20.8510131380481,19.2358271139468,
-16.714315555052));
#102856=CARTESIAN_POINT('Ctrl Pts',(-20.8505504063664,19.2617494365499,
-16.7159232464005));
#102857=CARTESIAN_POINT('Ctrl Pts',(-20.8489736684266,19.3052644117491,
-16.7185990200433));
#102858=CARTESIAN_POINT('Ctrl Pts',(-20.8481159290052,19.3228627088576,
-16.7196748359838));
#102859=CARTESIAN_POINT('Ctrl Pts',(-20.8465415719745,19.3485615206045,
-16.7212369315558));
#102860=CARTESIAN_POINT('Ctrl Pts',(-20.8459978398512,19.3566715230364,
-16.7217285975398));
#102861=CARTESIAN_POINT('Ctrl Pts',(-20.84495266486,19.3710219903606,-16.7225963419054));
#102862=CARTESIAN_POINT('Ctrl Pts',(-20.8444702256611,19.3772637019614,
-16.7229730125008));
#102863=CARTESIAN_POINT('Ctrl Pts',(-20.8434611332646,19.3896063383327,
-16.7237163971605));
#102864=CARTESIAN_POINT('Ctrl Pts',(-20.8429356823552,19.3957072975211,
-16.7240831452476));
#102865=CARTESIAN_POINT('Ctrl Pts',(-20.8418361329149,19.4078571927139,
-16.724812137682));
#102866=CARTESIAN_POINT('Ctrl Pts',(-20.841262449406,19.4139061064936,-16.7251743913984));
#102867=CARTESIAN_POINT('Ctrl Pts',(-20.8398285581254,19.4283626221666,
-16.7260385677845));
#102868=CARTESIAN_POINT('Ctrl Pts',(-20.838944025948,19.4367677490365,-16.7265397217195));
#102869=CARTESIAN_POINT('Ctrl Pts',(-20.8360988515349,19.4623318192594,
-16.7280602165821));
#102870=CARTESIAN_POINT('Ctrl Pts',(-20.8339785214729,19.4794725319764,
-16.7290745437001));
#102871=CARTESIAN_POINT('Ctrl Pts',(-20.8260338095488,19.5378270308262,
-16.7325118514138));
#102872=CARTESIAN_POINT('Ctrl Pts',(-20.8192037326319,19.5788954855934,
-16.7349035867475));
#102873=CARTESIAN_POINT('Ctrl Pts',(-20.7779734636126,19.7884237590213,
-16.7470133767205));
#102874=CARTESIAN_POINT('Ctrl Pts',(-20.7243586254664,19.9524297643781,
-16.7561209403142));
#102875=CARTESIAN_POINT('Ctrl Pts',(-20.6249328324955,20.1649353425292,
-16.7690150952559));
#102876=CARTESIAN_POINT('Ctrl Pts',(-20.5958562969027,20.220509582028,-16.7725069378238));
#102877=CARTESIAN_POINT('Ctrl Pts',(-20.5488220085098,20.3014431597294,
-16.7778912905825));
#102878=CARTESIAN_POINT('Ctrl Pts',(-20.5327016379616,20.3278336482267,
-16.7796970938042));
#102879=CARTESIAN_POINT('Ctrl Pts',(-20.5121619834855,20.3598602049572,
-16.7819630195547));
#102880=CARTESIAN_POINT('Ctrl Pts',(-20.5082836600394,20.365840811746,-16.7823894181052));
#102881=CARTESIAN_POINT('Ctrl Pts',(-20.5021352904952,20.3752178846214,
-16.7830633112008));
#102882=CARTESIAN_POINT('Ctrl Pts',(-20.4998854488861,20.3786276243436,
-16.7833094737889));
#102883=CARTESIAN_POINT('Ctrl Pts',(-20.4956478283573,20.3850096740737,
-16.7837723623906));
#102884=CARTESIAN_POINT('Ctrl Pts',(-20.4936623833385,20.387983467156,-16.783988932216));
#102885=CARTESIAN_POINT('Ctrl Pts',(-20.4890946289215,20.3947876429835,
-16.7844864666896));
#102886=CARTESIAN_POINT('Ctrl Pts',(-20.486507317039,20.3986146020239,-16.7847677662195));
#102887=CARTESIAN_POINT('Ctrl Pts',(-20.4784512063112,20.410446948935,-16.7856419710095));
#102888=CARTESIAN_POINT('Ctrl Pts',(-20.4729400153029,20.4184231277742,
-16.7862376421043));
#102889=CARTESIAN_POINT('Ctrl Pts',(-20.4106715035772,20.5072318371383,
-16.7929390210152));
#102890=CARTESIAN_POINT('Ctrl Pts',(-20.3483849501997,20.5840261871356,
-16.7993722827136));
#102891=CARTESIAN_POINT('Ctrl Pts',(-20.1664593466636,20.7787658150669,
-16.8169267314158));
#102892=CARTESIAN_POINT('Ctrl Pts',(-20.0377573938488,20.887324133974,-16.8280724350466));
#102893=CARTESIAN_POINT('Ctrl Pts',(-19.8712093579943,20.9969003370978,
-16.8405985891722));
#102894=CARTESIAN_POINT('Ctrl Pts',(-19.8444569268267,21.0136565720525,
-16.8425612093817));
#102895=CARTESIAN_POINT('Ctrl Pts',(-19.8041717197435,21.0376516814561,
-16.845444733301));
#102896=CARTESIAN_POINT('Ctrl Pts',(-19.790919746447,21.0453512597232,-16.8463820414283));
#102897=CARTESIAN_POINT('Ctrl Pts',(-19.7666473240213,21.0591034986998,
-16.8480787412602));
#102898=CARTESIAN_POINT('Ctrl Pts',(-19.7556544347017,21.0652031346264,
-16.8488397949379));
#102899=CARTESIAN_POINT('Ctrl Pts',(-19.738262448279,21.0746518130283,-16.8500324793849));
#102900=CARTESIAN_POINT('Ctrl Pts',(-19.7318995651862,21.0780665775593,
-16.8504664503689));
#102901=CARTESIAN_POINT('Ctrl Pts',(-19.7254731420198,21.0814732052019,
-16.8509023944279));
#102902=CARTESIAN_POINT('Ctrl Pts',(-19.7254270100311,21.0814976574446,
-16.850905523724));
#102903=CARTESIAN_POINT('Ctrl Pts',(-19.7253331200524,21.0815474193421,
-16.8509118923652));
#102904=CARTESIAN_POINT('Ctrl Pts',(-19.7252853607656,21.0815727295276,
-16.8509151317894));
#102905=CARTESIAN_POINT('Ctrl Pts',(-19.7251881569115,21.08162423825,-16.8509217246807));
#102906=CARTESIAN_POINT('Ctrl Pts',(-19.7251387113115,21.0816504371662,
-16.8509250782086));
#102907=CARTESIAN_POINT('Ctrl Pts',(-19.7250380730387,21.0817037555805,
-16.8509319034698));
#102908=CARTESIAN_POINT('Ctrl Pts',(-19.7249868797228,21.081730875239,-16.8509353752367));
#102909=CARTESIAN_POINT('Ctrl Pts',(-19.7248826823109,21.0817860683394,
-16.8509424412658));
#102910=CARTESIAN_POINT('Ctrl Pts',(-19.7248296773664,21.0818141420373,
-16.8509460355747));
#102911=CARTESIAN_POINT('Ctrl Pts',(-19.724721790746,21.0818712775594,-16.8509533511273));
#102912=CARTESIAN_POINT('Ctrl Pts',(-19.7246669081625,21.0819003396568,
-16.8509570724209));
#102913=CARTESIAN_POINT('Ctrl Pts',(-19.7245551977369,21.0819594876347,
-16.8509646465542));
#102914=CARTESIAN_POINT('Ctrl Pts',(-19.7244983690897,21.0819895737188,
-16.850968499436));
#102915=CARTESIAN_POINT('Ctrl Pts',(-19.7243826953439,21.0820508066848,
-16.8509763415345));
#102916=CARTESIAN_POINT('Ctrl Pts',(-19.7243238497194,21.0820819536058,
-16.8509803307736));
#102917=CARTESIAN_POINT('Ctrl Pts',(-19.7242040684595,21.0821453464546,
-16.8509884505331));
#102918=CARTESIAN_POINT('Ctrl Pts',(-19.7241431321865,21.0821775924632,
-16.8509925810823));
#102919=CARTESIAN_POINT('Ctrl Pts',(-19.7240190935729,21.0822432229556,
-16.851000988574));
#102920=CARTESIAN_POINT('Ctrl Pts',(-19.7239559904609,21.0822766075722,
-16.8510052655535));
#102921=CARTESIAN_POINT('Ctrl Pts',(-19.7238275390494,21.0823445563028,
-16.8510139712215));
#102922=CARTESIAN_POINT('Ctrl Pts',(-19.7237621903787,21.0823791203179,
-16.8510183999188));
#102923=CARTESIAN_POINT('Ctrl Pts',(-19.7236291640709,21.0824494712604,
-16.8510274146503));
#102924=CARTESIAN_POINT('Ctrl Pts',(-19.7235614890042,21.0824852565114,
-16.8510320004925));
#102925=CARTESIAN_POINT('Ctrl Pts',(-19.7234348799324,21.0825521961239,
-16.851040579369));
#102926=CARTESIAN_POINT('Ctrl Pts',(-19.7233759451185,21.0825833520483,
-16.8510445725215));
#102927=CARTESIAN_POINT('Ctrl Pts',(-19.7232483244762,21.0826508110639,
-16.8510532190799));
#102928=CARTESIAN_POINT('Ctrl Pts',(-19.7231796369936,21.0826871137539,
-16.8510578725267));
#102929=CARTESIAN_POINT('Ctrl Pts',(-19.7230309145422,21.0827657060309,
-16.8510679476066));
#102930=CARTESIAN_POINT('Ctrl Pts',(-19.7229508780295,21.0828079947042,
-16.8510733692477));
#102931=CARTESIAN_POINT('Ctrl Pts',(-19.722777607617,21.0828995309025,-16.8510851057225));
#102932=CARTESIAN_POINT('Ctrl Pts',(-19.722684372029,21.0829487769765,-16.8510914205397));
#102933=CARTESIAN_POINT('Ctrl Pts',(-19.7224825634121,21.0830553509191,
-16.8511050878986));
#102934=CARTESIAN_POINT('Ctrl Pts',(-19.7223739885994,21.0831126765595,
-16.8511124403841));
#102935=CARTESIAN_POINT('Ctrl Pts',(-19.7221390309196,21.0832367040508,
-16.8511283498257));
#102936=CARTESIAN_POINT('Ctrl Pts',(-19.7220126465365,21.0833034024179,
-16.8511369066456));
#102937=CARTESIAN_POINT('Ctrl Pts',(-19.7217267223079,21.0834542596749,
-16.8511562630028));
#102938=CARTESIAN_POINT('Ctrl Pts',(-19.7215671784302,21.0835384109874,
-16.8511670622719));
#102939=CARTESIAN_POINT('Ctrl Pts',(-19.7156957196511,21.08663434892,-16.8515644384269));
#102940=CARTESIAN_POINT('Ctrl Pts',(-19.7099700173434,21.0896200316995,
-16.8519500877194));
#102941=CARTESIAN_POINT('Ctrl Pts',(-19.696713170044,21.0964558843378,-16.8528387449199));
#102942=CARTESIAN_POINT('Ctrl Pts',(-19.6891724004307,21.1002872275498,
-16.8533410856229));
#102943=CARTESIAN_POINT('Ctrl Pts',(-19.6688198113224,21.1104750486426,
-16.8546886005082));
#102944=CARTESIAN_POINT('Ctrl Pts',(-19.6559660662701,21.1167471310882,
-16.8555308270215));
#102945=CARTESIAN_POINT('Ctrl Pts',(-19.5375058173773,21.1730716635396,
-16.8632150173504));
#102946=CARTESIAN_POINT('Ctrl Pts',(-19.4279816947245,21.2144324256188,
-16.8697401399791));
#102947=CARTESIAN_POINT('Ctrl Pts',(-19.1589186075763,21.2913083686041,
-16.8850590384475));
#102948=CARTESIAN_POINT('Ctrl Pts',(-18.9976226529485,21.3178293447792,
-16.893669114829));
#102949=CARTESIAN_POINT('Ctrl Pts',(-18.8026638245846,21.3271323320097,
-16.9048789539896));
#102950=CARTESIAN_POINT('Ctrl Pts',(-18.7703950822212,21.3279331376575,
-16.9067618072207));
#102951=CARTESIAN_POINT('Ctrl Pts',(-18.7308990050844,21.3280100532676,
-16.909113528753));
#102952=CARTESIAN_POINT('Ctrl Pts',(-18.7236754149912,21.3279871471808,
-16.9095455751668));
#102953=CARTESIAN_POINT('Ctrl Pts',(-18.7123461453106,21.3278932357209,
-16.9102264093285));
#102954=CARTESIAN_POINT('Ctrl Pts',(-18.7082402359922,21.3278472535267,
-16.9104738190418));
#102955=CARTESIAN_POINT('Ctrl Pts',(-18.7005624300027,21.3277389284762,
-16.9109377461045));
#102956=CARTESIAN_POINT('Ctrl Pts',(-18.6969905485386,21.3276794897332,
-16.9111540993871));
#102957=CARTESIAN_POINT('Ctrl Pts',(-18.6888328761138,21.3275230851003,
-16.9116494082892));
#102958=CARTESIAN_POINT('Ctrl Pts',(-18.6842472546522,21.3274202565319,
-16.9119286875966));
#102959=CARTESIAN_POINT('Ctrl Pts',(-18.6701379119595,21.3270579866315,
-16.9127905463215));
#102960=CARTESIAN_POINT('Ctrl Pts',(-18.6606157325954,21.3267491605994,
-16.9133757823429));
#102961=CARTESIAN_POINT('Ctrl Pts',(-18.531580303092,21.3216921253335,-16.9213519302441));
#102962=CARTESIAN_POINT('Ctrl Pts',(-18.4126898090621,21.3068883823168,
-16.9292197319498));
#102963=CARTESIAN_POINT('Ctrl Pts',(-18.1890914981612,21.2595698134871,
-16.9443184106419));
#102964=CARTESIAN_POINT('Ctrl Pts',(-18.0843748731905,21.2288092643061,
-16.9515213934213));
#102965=CARTESIAN_POINT('Ctrl Pts',(-17.9123350918901,21.1634821687294,
-16.9633453241773));
#102966=CARTESIAN_POINT('Ctrl Pts',(-17.8436435457359,21.1331309454483,
-16.9680664510751));
#102967=CARTESIAN_POINT('Ctrl Pts',(-17.759926684429,21.0906871888177,-16.9738164513622));
#102968=CARTESIAN_POINT('Ctrl Pts',(-17.7432648938693,21.0819587748617,
-16.9749608276412));
#102969=CARTESIAN_POINT('Ctrl Pts',(-17.7191971258834,21.0689389939885,
-16.9766142771739));
#102970=CARTESIAN_POINT('Ctrl Pts',(-17.7116977028387,21.064823129447,-16.9771295464027));
#102971=CARTESIAN_POINT('Ctrl Pts',(-17.6985885393089,21.0575247627869,
-16.9780304226833));
#102972=CARTESIAN_POINT('Ctrl Pts',(-17.6929680489618,21.0543618936229,
-16.9784167256709));
#102973=CARTESIAN_POINT('Ctrl Pts',(-17.6820792410735,21.0481686512974,
-16.979165272827));
#102974=CARTESIAN_POINT('Ctrl Pts',(-17.6768093527798,21.0451411813123,
-16.9795276165287));
#102975=CARTESIAN_POINT('Ctrl Pts',(-17.6642374714318,21.0378466431114,
-16.9803922280677));
#102976=CARTESIAN_POINT('Ctrl Pts',(-17.6569478312777,21.0335584089353,
-16.9808937253888));
#102977=CARTESIAN_POINT('Ctrl Pts',(-17.6307063686194,21.0179090732608,
-16.9826998081923));
#102978=CARTESIAN_POINT('Ctrl Pts',(-17.6119065862974,21.006294867484,-16.9839951696617));
#102979=CARTESIAN_POINT('Ctrl Pts',(-17.4368620860328,20.8943311627244,
-16.9960803616487));
#102980=CARTESIAN_POINT('Ctrl Pts',(-17.2942802230183,20.7741326048051,
-17.0060124385862));
#102981=CARTESIAN_POINT('Ctrl Pts',(-17.1152684613226,20.5776780387714,
-17.0205016160832));
#102982=CARTESIAN_POINT('Ctrl Pts',(-17.0647424197582,20.5154837231388,
-17.0249052943029));
#102983=CARTESIAN_POINT('Ctrl Pts',(-16.9967780191285,20.4213906871449,
-17.031544840602));
#102984=CARTESIAN_POINT('Ctrl Pts',(-16.9764416504457,20.3916668142064,
-17.0336395237962));
#102985=CARTESIAN_POINT('Ctrl Pts',(-16.9528178017769,20.3551742457764,
-17.0362265788814));
#102986=CARTESIAN_POINT('Ctrl Pts',(-16.9487942786771,20.3488863109973,
-17.0366728863048));
#102987=CARTESIAN_POINT('Ctrl Pts',(-16.9425810575411,20.3390622635854,
-17.0373712331894));
#102988=CARTESIAN_POINT('Ctrl Pts',(-16.9403683357703,20.3355406841529,
-17.0376217752691));
#102989=CARTESIAN_POINT('Ctrl Pts',(-16.9362777634657,20.3289876905151,
-17.0380884186271));
#102990=CARTESIAN_POINT('Ctrl Pts',(-16.9343971895342,20.3259580439778,
-17.03830433641));
#102991=CARTESIAN_POINT('Ctrl Pts',(-16.930155003285,20.3190850941592,-17.0387945488531));
#102992=CARTESIAN_POINT('Ctrl Pts',(-16.9277980269234,20.3152390047697,
-17.0390691411588));
#102993=CARTESIAN_POINT('Ctrl Pts',(-16.9217436399011,20.3052882723997,
-17.0397802121716));
#102994=CARTESIAN_POINT('Ctrl Pts',(-16.91806481064,20.2991724691257,-17.0402178582158));
#102995=CARTESIAN_POINT('Ctrl Pts',(-16.8956528701362,20.2614839826538,
-17.042918049991));
#102996=CARTESIAN_POINT('Ctrl Pts',(-16.8777139434229,20.229449050776,-17.0452268991277));
#102997=CARTESIAN_POINT('Ctrl Pts',(-16.7812828198082,20.0462254354891,
-17.0584408825197));
#102998=CARTESIAN_POINT('Ctrl Pts',(-16.7204310367164,19.8864620716192,
-17.069934485297));
#102999=CARTESIAN_POINT('Ctrl Pts',(-16.6563717005341,19.6284539752063,
-17.0872114878343));
#103000=CARTESIAN_POINT('Ctrl Pts',(-16.6396560788146,19.5343186919745,
-17.0932786793386));
#103001=CARTESIAN_POINT('Ctrl Pts',(-16.6270441989163,19.4180854513586,
-17.1004603678851));
#103002=CARTESIAN_POINT('Ctrl Pts',(-16.6250580935117,19.3967719563002,
-17.1017650354998));
#103003=CARTESIAN_POINT('Ctrl Pts',(-16.6226955365492,19.3664467011526,
-17.1036045885643));
#103004=CARTESIAN_POINT('Ctrl Pts',(-16.6220529349184,19.3574575450612,
-17.1041477933856));
#103005=CARTESIAN_POINT('Ctrl Pts',(-16.6210439417596,19.341951495327,-17.1050812903387));
#103006=CARTESIAN_POINT('Ctrl Pts',(-16.6206502556039,19.3354365602431,
-17.1054724341047));
#103007=CARTESIAN_POINT('Ctrl Pts',(-16.6199544833816,19.3229648433948,
-17.1062192021889));
#103008=CARTESIAN_POINT('Ctrl Pts',(-16.6196474299979,19.3170084116352,
-17.1065749786924));
#103009=CARTESIAN_POINT('Ctrl Pts',(-16.6189150554614,19.301529217575,-17.1074973131409));
#103010=CARTESIAN_POINT('Ctrl Pts',(-16.6185288681592,19.2920046709398,
-17.1080626404137));
#103011=CARTESIAN_POINT('Ctrl Pts',(-16.6174336282252,19.2595847652786,
-17.1099796902197));
#103012=CARTESIAN_POINT('Ctrl Pts',(-16.6170318197903,19.236680143847,-17.1113218040137));
#103013=CARTESIAN_POINT('Ctrl Pts',(-16.6167704938624,19.0371634066197,
-17.1229164096785));
#103014=CARTESIAN_POINT('Ctrl Pts',(-16.6386380699323,18.86122154183,-17.1324066911915));
#103015=CARTESIAN_POINT('Ctrl Pts',(-16.7033215799155,18.606461136644,-17.1467108838563));
#103016=CARTESIAN_POINT('Ctrl Pts',(-16.7296217467567,18.5242776749342,
-17.1514331796244));
#103017=CARTESIAN_POINT('Ctrl Pts',(-16.7744878690877,18.4088674171645,
-17.1585043311072));
#103018=CARTESIAN_POINT('Ctrl Pts',(-16.7890513907631,18.3741732642092,
-17.1606900626565));
#103019=CARTESIAN_POINT('Ctrl Pts',(-16.8076413207388,18.3329974966708,
-17.1633780849125));
#103020=CARTESIAN_POINT('Ctrl Pts',(-16.8107890696741,18.3261238105902,
-17.1638300088621));
#103021=CARTESIAN_POINT('Ctrl Pts',(-16.8157341398824,18.315476376396,-17.1645352467976));
#103022=CARTESIAN_POINT('Ctrl Pts',(-16.8175059704469,18.3116907625741,
-17.1647870152137));
#103023=CARTESIAN_POINT('Ctrl Pts',(-16.8208093462708,18.3046870162201,
-17.1652547600238));
#103024=CARTESIAN_POINT('Ctrl Pts',(-16.8223378114088,18.3014674946924,
-17.165470545438));
#103025=CARTESIAN_POINT('Ctrl Pts',(-16.8258074075702,18.2942066041377,
-17.1659589357799));
#103026=CARTESIAN_POINT('Ctrl Pts',(-16.82775324015,18.2901675558462,-17.1662318288778));
#103027=CARTESIAN_POINT('Ctrl Pts',(-16.833521780004,18.2782901908661,-17.1670378210301));
#103028=CARTESIAN_POINT('Ctrl Pts',(-16.8373800541377,18.2704693903541,
-17.1675730571942));
#103029=CARTESIAN_POINT('Ctrl Pts',(-16.8651906123301,18.2149638428839,
-17.171402806243));
#103030=CARTESIAN_POINT('Ctrl Pts',(-16.8908880166505,18.1681799131341,
-17.1747944450502));
#103031=CARTESIAN_POINT('Ctrl Pts',(-16.92737026789,18.1073299326637,-17.1793798262357));
#103032=CARTESIAN_POINT('Ctrl Pts',(-16.9366057134555,18.0923524411188,
-17.1805230519075));
#103033=CARTESIAN_POINT('Ctrl Pts',(-16.9719970248176,18.0365268713673,
-17.1848350321887));
#103034=CARTESIAN_POINT('Ctrl Pts',(-16.9993670063192,17.9964672694417,
-17.1880325456117));
#103035=CARTESIAN_POINT('Ctrl Pts',(-17.092860645783,17.8692417428287,-17.198461929987));
#103036=CARTESIAN_POINT('Ctrl Pts',(-17.16437244302,17.7862451443228,-17.2056947298553));
#103037=CARTESIAN_POINT('Ctrl Pts',(-17.2810732630817,17.6703088986067,
-17.2162683797988));
#103038=CARTESIAN_POINT('Ctrl Pts',(-17.3216673655765,17.6330131421397,
-17.2197576070219));
#103039=CARTESIAN_POINT('Ctrl Pts',(-17.3898211512651,17.5751366283048,
-17.2253153036747));
#103040=CARTESIAN_POINT('Ctrl Pts',(-17.416505748954,17.5535698014598,-17.2274222140389));
#103041=CARTESIAN_POINT('Ctrl Pts',(-17.4522728821646,17.5260722807138,
-17.2301587913689));
#103042=CARTESIAN_POINT('Ctrl Pts',(-17.4608922230727,17.5195502020674,
-17.2308118006939));
#103043=CARTESIAN_POINT('Ctrl Pts',(-17.47509371396,17.508974281704,-17.2318773062803));
#103044=CARTESIAN_POINT('Ctrl Pts',(-17.4806463190806,17.5048812658405,
-17.2322913320175));
#103045=CARTESIAN_POINT('Ctrl Pts',(-17.4914348492334,17.4970097621399,
-17.2330908478878));
#103046=CARTESIAN_POINT('Ctrl Pts',(-17.4966682435219,17.4932279501588,
-17.2334764643715));
#103047=CARTESIAN_POINT('Ctrl Pts',(-17.5087941182849,17.4845495872985,
-17.2343648817411));
#103048=CARTESIAN_POINT('Ctrl Pts',(-17.5156988228576,17.479670243702,-17.2348670165765));
#103049=CARTESIAN_POINT('Ctrl Pts',(-17.5343516749213,17.4666556849718,
-17.2362136146957));
#103050=CARTESIAN_POINT('Ctrl Pts',(-17.5461533940615,17.4585977491154,
-17.2370551366544));
#103051=CARTESIAN_POINT('Ctrl Pts',(-17.6551778851291,17.3857658766104,
-17.2447362189286));
#103052=CARTESIAN_POINT('Ctrl Pts',(-17.7575303306774,17.3290199236885,
-17.2512591698624));
#103053=CARTESIAN_POINT('Ctrl Pts',(-18.0124241071135,17.2141266389694,
-17.2665653225836));
#103054=CARTESIAN_POINT('Ctrl Pts',(-18.1679915624739,17.164589097064,-17.2751654339514));
#103055=CARTESIAN_POINT('Ctrl Pts',(-18.359578288624,17.1271204164737,-17.286374450996));
#103056=CARTESIAN_POINT('Ctrl Pts',(-18.3916189142075,17.1216171563284,
-17.2882704403549));
#103057=CARTESIAN_POINT('Ctrl Pts',(-18.4309328911563,17.1157931513323,
-17.2906367771272));
#103058=CARTESIAN_POINT('Ctrl Pts',(-18.438099569571,17.1147690148756,-17.2910697605058));
#103059=CARTESIAN_POINT('Ctrl Pts',(-18.4493425258526,17.1132211718275,
-17.2917517458983));
#103060=CARTESIAN_POINT('Ctrl Pts',(-18.4534153935769,17.1126725309201,
-17.2919993621683));
#103061=CARTESIAN_POINT('Ctrl Pts',(-18.4610311400588,17.1116692113184,
-17.2924634637215));
#103062=CARTESIAN_POINT('Ctrl Pts',(-18.4645735807839,17.1112116385749,
-17.2926797836414));
#103063=CARTESIAN_POINT('Ctrl Pts',(-18.4726624110747,17.1101876202075,
-17.2931747353383));
#103064=CARTESIAN_POINT('Ctrl Pts',(-18.4772094761604,17.1096269687584,
-17.2934536889974));
#103065=CARTESIAN_POINT('Ctrl Pts',(-18.4911909812095,17.1079491119574,
-17.2943135670052));
#103066=CARTESIAN_POINT('Ctrl Pts',(-18.5006309991433,17.1068806690185,
-17.294897130639));
#103067=CARTESIAN_POINT('Ctrl Pts',(-18.5854881532004,17.0978544031714,
-17.3001677509269));
#103068=CARTESIAN_POINT('Ctrl Pts',(-18.6612672861743,17.0938917141039,
-17.3050495259045));
#103069=CARTESIAN_POINT('Ctrl Pts',(-18.9220107228818,17.0942718487392,
-17.3221024429291));
#103070=CARTESIAN_POINT('Ctrl Pts',(-19.1061424033332,17.1187724827416,
-17.3344993698907));
#103071=CARTESIAN_POINT('Ctrl Pts',(-19.3361780933514,17.1807519209795,
-17.349526425177));
#103072=CARTESIAN_POINT('Ctrl Pts',(-19.3870669939627,17.1965447340662,
-17.3528279642546));
#103073=CARTESIAN_POINT('Ctrl Pts',(-19.4491380982266,17.2184077771642,
-17.3568295944672));
#103074=CARTESIAN_POINT('Ctrl Pts',(-19.4609293340424,17.222679095327,-17.3575886440234));
#103075=CARTESIAN_POINT('Ctrl Pts',(-19.4795055394213,17.2295955727872,
-17.3587828706293));
#103076=CARTESIAN_POINT('Ctrl Pts',(-19.4863158701772,17.2321713447019,
-17.3592203514209));
#103077=CARTESIAN_POINT('Ctrl Pts',(-19.4990579924253,17.2370659007478,
-17.3600382827464));
#103078=CARTESIAN_POINT('Ctrl Pts',(-19.5049928552492,17.2393764105466,
-17.3604190051709));
#103079=CARTESIAN_POINT('Ctrl Pts',(-19.5182500967761,17.2446066198789,
-17.3612689560568));
#103080=CARTESIAN_POINT('Ctrl Pts',(-19.5255668007745,17.247540516802,-17.361737700704));
#103081=CARTESIAN_POINT('Ctrl Pts',(-19.5440621451908,17.2550770817718,
-17.362921827671));
#103082=CARTESIAN_POINT('Ctrl Pts',(-19.5552181562344,17.2597347976033,
-17.3636353444181));
#103083=CARTESIAN_POINT('Ctrl Pts',(-19.618639505344,17.2868539377761,-17.3676884237337));
#103084=CARTESIAN_POINT('Ctrl Pts',(-19.6700252934956,17.3113203944047,
-17.3709588771089));
#103085=CARTESIAN_POINT('Ctrl Pts',(-19.7441244366506,17.3503392135024,
-17.3756896458241));
#103086=CARTESIAN_POINT('Ctrl Pts',(-19.7676426166676,17.3633006331428,
-17.377193573104));
#103087=CARTESIAN_POINT('Ctrl Pts',(-19.8912833375688,17.4345416336196,
-17.3851309615017));
#103088=CARTESIAN_POINT('Ctrl Pts',(-19.9867413041996,17.5005178870648,
-17.3913558622935));
#103089=CARTESIAN_POINT('Ctrl Pts',(-20.1382147131518,17.6247226157745,
-17.4020347573932));
#103090=CARTESIAN_POINT('Ctrl Pts',(-20.1971729278717,17.6789367236937,
-17.4064365656863));
#103091=CARTESIAN_POINT('Ctrl Pts',(-20.2779937140936,17.7621837456945,
-17.4130735689769));
#103092=CARTESIAN_POINT('Ctrl Pts',(-20.3024069513658,17.7886482801445,
-17.4151677035097));
#103093=CARTESIAN_POINT('Ctrl Pts',(-20.3310516861282,17.8213343455992,
-17.4177541498842));
#103094=CARTESIAN_POINT('Ctrl Pts',(-20.3359416236859,17.8269740790997,
-17.4182004225804));
#103095=CARTESIAN_POINT('Ctrl Pts',(-20.3435094062188,17.8357960994264,
-17.418898726846));
#103096=CARTESIAN_POINT('Ctrl Pts',(-20.3462079277635,17.8389606806536,
-17.4191492613297));
#103097=CARTESIAN_POINT('Ctrl Pts',(-20.3512028449127,17.8448533481459,
-17.4196158979282));
#103098=CARTESIAN_POINT('Ctrl Pts',(-20.3535016791178,17.8475792921132,
-17.4198318165941));
#103099=CARTESIAN_POINT('Ctrl Pts',(-20.3586930694697,17.8537668661355,
-17.42032204061));
#103100=CARTESIAN_POINT('Ctrl Pts',(-20.361581440374,17.8572319239539,-17.4205966436654));
#103101=CARTESIAN_POINT('Ctrl Pts',(-20.3701034444459,17.8675221104456,
-17.42141228901));
#103102=CARTESIAN_POINT('Ctrl Pts',(-20.375705297689,17.8743732645519,-17.4219555439972));
#103103=CARTESIAN_POINT('Ctrl Pts',(-20.4168969112017,17.9254008472913,
-17.4260019210848));
#103104=CARTESIAN_POINT('Ctrl Pts',(-20.4507379835476,17.9709529555637,
-17.4296147387959));
#103105=CARTESIAN_POINT('Ctrl Pts',(-20.5175955942822,18.0689371151353,
-17.4372974290447));
#103106=CARTESIAN_POINT('Ctrl Pts',(-20.5502244118431,18.1215739265789,
-17.4413750935863));
#103107=CARTESIAN_POINT('Ctrl Pts',(-20.6341053691248,18.2711590612222,
-17.452703249606));
#103108=CARTESIAN_POINT('Ctrl Pts',(-20.6802112962647,18.3707819009973,
-17.4599518298351));
#103109=CARTESIAN_POINT('Ctrl Pts',(-20.7198023055324,18.4773144540793,
-17.4672585983927));
#103110=CARTESIAN_POINT('Ctrl Pts',(-20.7211968892606,18.4811001446346,
-17.4675177024312));
#103111=CARTESIAN_POINT('Ctrl Pts',(-20.7225806135343,18.4848897167264,
-17.4677765237272));
#103112=CARTESIAN_POINT('',(-20.8509993557841,19.2126515476976,-16.4878149913274));
#103113=CARTESIAN_POINT('Ctrl Pts',(-20.7225806138883,18.484889717696,-17.2426990599955));
#103114=CARTESIAN_POINT('Ctrl Pts',(-20.7071867113841,18.4427308103813,
-17.239882851258));
#103115=CARTESIAN_POINT('Ctrl Pts',(-20.6904549548032,18.4010691626674,
-17.2371086158738));
#103116=CARTESIAN_POINT('Ctrl Pts',(-20.6673796328444,18.3485101301596,
-17.2336176480217));
#103117=CARTESIAN_POINT('Ctrl Pts',(-20.6622477660772,18.3370971773503,
-17.2328601224428));
#103118=CARTESIAN_POINT('Ctrl Pts',(-20.6539422346179,18.3190556029706,
-17.2316632936934));
#103119=CARTESIAN_POINT('Ctrl Pts',(-20.6508347897754,18.3123969828176,
-17.2312217238274));
#103120=CARTESIAN_POINT('Ctrl Pts',(-20.6449719435814,18.300002900346,-17.2304000269476));
#103121=CARTESIAN_POINT('Ctrl Pts',(-20.6422252387044,18.2942634378015,
-17.2300196046811));
#103122=CARTESIAN_POINT('Ctrl Pts',(-20.6360566868268,18.2815215977503,
-17.2291752107988));
#103123=CARTESIAN_POINT('Ctrl Pts',(-20.6326219525082,18.2745255347363,
-17.228711693585));
#103124=CARTESIAN_POINT('Ctrl Pts',(-20.6224963106263,18.2541857537887,
-17.227364305645));
#103125=CARTESIAN_POINT('Ctrl Pts',(-20.6157027256542,18.2408934665018,
-17.2264840324975));
#103126=CARTESIAN_POINT('Ctrl Pts',(-20.5587597755292,18.132328387959,-17.2192940048285));
#103127=CARTESIAN_POINT('Ctrl Pts',(-20.5015469952183,18.0409304560815,
-17.2132500513549));
#103128=CARTESIAN_POINT('Ctrl Pts',(-20.3582443594567,17.846669251552,-17.1999840335387));
#103129=CARTESIAN_POINT('Ctrl Pts',(-20.2688562436721,17.7468341966682,
-17.192865009603));
#103130=CARTESIAN_POINT('Ctrl Pts',(-20.1586015668276,17.6449640266721,
-17.1845188886493));
#103131=CARTESIAN_POINT('Ctrl Pts',(-20.1464197126941,17.6339683485899,
-17.1836017627802));
#103132=CARTESIAN_POINT('Ctrl Pts',(-20.0943089420233,17.5880198594671,
-17.1796936555183));
#103133=CARTESIAN_POINT('Ctrl Pts',(-20.053204350568,17.5544361373716,-17.1766480658313));
#103134=CARTESIAN_POINT('Ctrl Pts',(-20.0039431423795,17.5171850233622,
-17.1729829188183));
#103135=CARTESIAN_POINT('Ctrl Pts',(-19.996968451099,17.5119780914886,-17.1724636408047));
#103136=CARTESIAN_POINT('Ctrl Pts',(-19.9863557939277,17.5041567050613,
-17.1716726575752));
#103137=CARTESIAN_POINT('Ctrl Pts',(-19.9827412141084,17.5015104716903,
-17.1714031071031));
#103138=CARTESIAN_POINT('Ctrl Pts',(-19.9762361175234,17.4967797315891,
-17.1709176823085));
#103139=CARTESIAN_POINT('Ctrl Pts',(-19.9733487146159,17.4946910349267,
-17.1707021028946));
#103140=CARTESIAN_POINT('Ctrl Pts',(-19.9670609884658,17.4901667446976,
-17.1702323873001));
#103141=CARTESIAN_POINT('Ctrl Pts',(-19.9636587615153,17.4877339661674,
-17.1699780688898));
#103142=CARTESIAN_POINT('Ctrl Pts',(-19.9540761433167,17.4809246965056,
-17.1692613665436));
#103143=CARTESIAN_POINT('Ctrl Pts',(-19.9478795178131,17.4765713149553,
-17.1687974480133));
#103144=CARTESIAN_POINT('Ctrl Pts',(-19.9105751044534,17.4506612792974,
-17.166002506873));
#103145=CARTESIAN_POINT('Ctrl Pts',(-19.8789192103176,17.429910170921,-17.1636221473655));
#103146=CARTESIAN_POINT('Ctrl Pts',(-19.7726318910349,17.364241070351,-17.1556453005459));
#103147=CARTESIAN_POINT('Ctrl Pts',(-19.6957872426308,17.3230810053705,
-17.1499056945703));
#103148=CARTESIAN_POINT('Ctrl Pts',(-19.4572798279054,17.2136790136048,
-17.1325684497204));
#103149=CARTESIAN_POINT('Ctrl Pts',(-19.2894316466971,17.160647855784,-17.1210588431207));
#103150=CARTESIAN_POINT('Ctrl Pts',(-19.0943199638128,17.1247623385175,
-17.1088478016649));
#103151=CARTESIAN_POINT('Ctrl Pts',(-19.0716312042711,17.1209705045342,
-17.1074436467772));
#103152=CARTESIAN_POINT('Ctrl Pts',(-19.0394428363058,17.1161289218101,
-17.1054732096206));
#103153=CARTESIAN_POINT('Ctrl Pts',(-19.0299916262415,17.1147726453569,
-17.1048972686811));
#103154=CARTESIAN_POINT('Ctrl Pts',(-19.0146192467303,17.1126727031556,
-17.1039646760883));
#103155=CARTESIAN_POINT('Ctrl Pts',(-19.00870361759,17.111890062447,-17.1036067962195));
#103156=CARTESIAN_POINT('Ctrl Pts',(-18.9963132670565,17.1103040877661,
-17.1028592798134));
#103157=CARTESIAN_POINT('Ctrl Pts',(-18.9898379734459,17.1095056510752,
-17.1024698016247));
#103158=CARTESIAN_POINT('Ctrl Pts',(-18.9744234451177,17.1076772631884,
-17.1015453993111));
#103159=CARTESIAN_POINT('Ctrl Pts',(-18.9654810848497,17.106674340955,-17.1010113324702));
#103160=CARTESIAN_POINT('Ctrl Pts',(-18.9353274390045,17.1034870247805,
-17.0992176712833));
#103161=CARTESIAN_POINT('Ctrl Pts',(-18.9140891868463,17.1015660446221,
-17.0979663603395));
#103162=CARTESIAN_POINT('Ctrl Pts',(-18.798277175956,17.0928528555167,-17.0912031111308));
#103163=CARTESIAN_POINT('Ctrl Pts',(-18.7033525915127,17.0920987165368,
-17.0858843512766));
#103164=CARTESIAN_POINT('Ctrl Pts',(-18.4395270354852,17.1077428381018,
-17.0713425025402));
#103165=CARTESIAN_POINT('Ctrl Pts',(-18.2722026975441,17.1380463670778,
-17.0624253753528));
#103166=CARTESIAN_POINT('Ctrl Pts',(-18.0737616979252,17.1992256097341,
-17.050582336029));
#103167=CARTESIAN_POINT('Ctrl Pts',(-18.0375393841443,17.2114768031053,
-17.0483639154203));
#103168=CARTESIAN_POINT('Ctrl Pts',(-17.9948887057446,17.227201685988,-17.0456619415993));
#103169=CARTESIAN_POINT('Ctrl Pts',(-17.9881191384273,17.2297370207558,
-17.0452303515146));
#103170=CARTESIAN_POINT('Ctrl Pts',(-17.9771205158353,17.233920576392,-17.0445244842911));
#103171=CARTESIAN_POINT('Ctrl Pts',(-17.9728834784367,17.235547838968,-17.0442514307876));
#103172=CARTESIAN_POINT('Ctrl Pts',(-17.9653249718972,17.2384786610419,
-17.0437622510861));
#103173=CARTESIAN_POINT('Ctrl Pts',(-17.9620015356182,17.2397770034293,
-17.0435464397254));
#103174=CARTESIAN_POINT('Ctrl Pts',(-17.9548299797033,17.2425995808095,
-17.0430791717802));
#103175=CARTESIAN_POINT('Ctrl Pts',(-17.9509830972108,17.2441266792019,
-17.0428275489283));
#103176=CARTESIAN_POINT('Ctrl Pts',(-17.9402960506349,17.2484054416186,
-17.0421258453779));
#103177=CARTESIAN_POINT('Ctrl Pts',(-17.9334658233721,17.2511815420306,
-17.0416743294713));
#103178=CARTESIAN_POINT('Ctrl Pts',(-17.894731808093,17.2671609928011,-17.0390970123892));
#103179=CARTESIAN_POINT('Ctrl Pts',(-17.8631422551203,17.2811068283179,
-17.0369302217592));
#103180=CARTESIAN_POINT('Ctrl Pts',(-17.7643243603082,17.3276520781118,
-17.0299765195953));
#103181=CARTESIAN_POINT('Ctrl Pts',(-17.6984756342572,17.3630395037646,
-17.0250816208564));
#103182=CARTESIAN_POINT('Ctrl Pts',(-17.4687841841863,17.5026137963652,
-17.0073544895979));
#103183=CARTESIAN_POINT('Ctrl Pts',(-17.3175337167249,17.6257525923294,
-16.9945292851593));
#103184=CARTESIAN_POINT('Ctrl Pts',(-17.1707664458559,17.783261773556,-16.9813025167347));
#103185=CARTESIAN_POINT('Ctrl Pts',(-17.1565918516148,17.7989379715176,
-16.9800140347842));
#103186=CARTESIAN_POINT('Ctrl Pts',(-17.1371797250755,17.8210637037834,
-16.9782332452673));
#103187=CARTESIAN_POINT('Ctrl Pts',(-17.1317421870163,17.8273353723708,
-16.977732599134));
#103188=CARTESIAN_POINT('Ctrl Pts',(-17.122414129,17.8382230989188,-16.9768705062795));
#103189=CARTESIAN_POINT('Ctrl Pts',(-17.118506237229,17.8428240817167,-16.9765083432027));
#103190=CARTESIAN_POINT('Ctrl Pts',(-17.1104489428885,17.8523930437213,
-16.9757595252879));
#103191=CARTESIAN_POINT('Ctrl Pts',(-17.1063025336129,17.8573634697416,
-16.9753729954568));
#103192=CARTESIAN_POINT('Ctrl Pts',(-17.0966354339348,17.8690603595251,
-16.9744690045393));
#103193=CARTESIAN_POINT('Ctrl Pts',(-17.0911332646778,17.8758020317935,
-16.9739522991281));
#103194=CARTESIAN_POINT('Ctrl Pts',(-17.0733610097538,17.8978541216328,
-16.9722759722131));
#103195=CARTESIAN_POINT('Ctrl Pts',(-17.0612619401687,17.9133015083381,
-16.9711232061933));
#103196=CARTESIAN_POINT('Ctrl Pts',(-17.0002276133366,17.9934987853206,
-16.9652438486283));
#103197=CARTESIAN_POINT('Ctrl Pts',(-16.9548276551289,18.0608592497496,
-16.9606564668553));
#103198=CARTESIAN_POINT('Ctrl Pts',(-16.8273632954993,18.2756643202835,
-16.9468136257089));
#103199=CARTESIAN_POINT('Ctrl Pts',(-16.7589599285342,18.4304070669432,
-16.9379421871519));
#103200=CARTESIAN_POINT('Ctrl Pts',(-16.6938873449351,18.643085417118,-16.9254391539659));
#103201=CARTESIAN_POINT('Ctrl Pts',(-16.6801083694984,18.6951368935616,
-16.9223514123593));
#103202=CARTESIAN_POINT('Ctrl Pts',(-16.666416362408,18.7561777806655,-16.9186391868716));
#103203=CARTESIAN_POINT('Ctrl Pts',(-16.6645567538077,18.7647153436713,
-16.9181179175073));
#103204=CARTESIAN_POINT('Ctrl Pts',(-16.6618222983134,18.7776540573983,
-16.9173244912749));
#103205=CARTESIAN_POINT('Ctrl Pts',(-16.6609084785371,18.7820470001002,
-16.9170545091197));
#103206=CARTESIAN_POINT('Ctrl Pts',(-16.6592938471777,18.7899345856513,
-16.9165686253111));
#103207=CARTESIAN_POINT('Ctrl Pts',(-16.658587889457,18.7934281201549,-16.9163530210267));
#103208=CARTESIAN_POINT('Ctrl Pts',(-16.6570737503213,18.801019755965,-16.9158836238743));
#103209=CARTESIAN_POINT('Ctrl Pts',(-16.6562688847687,18.8051184172599,
-16.91562965081));
#103210=CARTESIAN_POINT('Ctrl Pts',(-16.6540437725974,18.8166295469774,
-16.9149148758286));
#103211=CARTESIAN_POINT('Ctrl Pts',(-16.6526510446535,18.8240471808273,
-16.9144525522565));
#103212=CARTESIAN_POINT('Ctrl Pts',(-16.6445932495909,18.8682652212819,
-16.9116868942807));
#103213=CARTESIAN_POINT('Ctrl Pts',(-16.6388650967294,18.9052271479884,
-16.9093353927574));
#103214=CARTESIAN_POINT('Ctrl Pts',(-16.6232881090554,19.0269691751384,
-16.9015022194512));
#103215=CARTESIAN_POINT('Ctrl Pts',(-16.617586258404,19.112191936991,-16.8958826046338));
#103216=CARTESIAN_POINT('Ctrl Pts',(-16.615910509217,19.3753571119182,-16.8784969082499));
#103217=CARTESIAN_POINT('Ctrl Pts',(-16.6371917536044,19.5526663831567,
-16.8668109489057));
#103218=CARTESIAN_POINT('Ctrl Pts',(-16.6859482611975,19.7473704050032,
-16.8544587546291));
#103219=CARTESIAN_POINT('Ctrl Pts',(-16.6918455597985,19.7694034763491,
-16.8530666616067));
#103220=CARTESIAN_POINT('Ctrl Pts',(-16.7007065194646,19.8004889076983,
-16.8511100590181));
#103221=CARTESIAN_POINT('Ctrl Pts',(-16.7033768078006,19.8096225907979,
-16.8505360737049));
#103222=CARTESIAN_POINT('Ctrl Pts',(-16.7078199692388,19.8244484657939,
-16.8496057825708));
#103223=CARTESIAN_POINT('Ctrl Pts',(-16.7095554395363,19.8301516453819,
-16.8492482605189));
#103224=CARTESIAN_POINT('Ctrl Pts',(-16.713242176425,19.8420859299351,-16.8485008050157));
#103225=CARTESIAN_POINT('Ctrl Pts',(-16.7151982296767,19.848315499666,-16.8481110329277));
#103226=CARTESIAN_POINT('Ctrl Pts',(-16.7199269485865,19.863135122253,-16.8471846832048));
#103227=CARTESIAN_POINT('Ctrl Pts',(-16.7227258076438,19.8717167328822,
-16.8466489726007));
#103228=CARTESIAN_POINT('Ctrl Pts',(-16.7323733050803,19.900667580712,-16.8448439076605));
#103229=CARTESIAN_POINT('Ctrl Pts',(-16.739477314475,19.9209507762255,-16.843582983214));
#103230=CARTESIAN_POINT('Ctrl Pts',(-16.8087247777823,20.1094154794984,
-16.8318925501622));
#103231=CARTESIAN_POINT('Ctrl Pts',(-16.8916862556132,20.2691692318284,
-16.8222582197732));
#103232=CARTESIAN_POINT('Ctrl Pts',(-17.0625168907625,20.5157583398618,
-16.8059327876054));
#103233=CARTESIAN_POINT('Ctrl Pts',(-17.1395800171256,20.6088792948023,
-16.7993132713628));
#103234=CARTESIAN_POINT('Ctrl Pts',(-17.2307915423774,20.7016855505723,
-16.7916011596479));
#103235=CARTESIAN_POINT('Ctrl Pts',(-17.2374895389496,20.708409599987,-16.7910354319514));
#103236=CARTESIAN_POINT('Ctrl Pts',(-17.2474861560193,20.7183110379497,
-16.7901915586537));
#103237=CARTESIAN_POINT('Ctrl Pts',(-17.2507503458532,20.7215232325391,
-16.7899160814427));
#103238=CARTESIAN_POINT('Ctrl Pts',(-17.2565788173557,20.7272217537287,
-16.7894242662379));
#103239=CARTESIAN_POINT('Ctrl Pts',(-17.2591389934707,20.7297122072974,
-16.7892082568314));
#103240=CARTESIAN_POINT('Ctrl Pts',(-17.2646594467497,20.7350551952702,
-16.7887425119715));
#103241=CARTESIAN_POINT('Ctrl Pts',(-17.2676216903343,20.7379055478104,
-16.7884926206246));
#103242=CARTESIAN_POINT('Ctrl Pts',(-17.2758275556728,20.7457555554688,
-16.787800500386));
#103243=CARTESIAN_POINT('Ctrl Pts',(-17.2810885127126,20.7507368928004,
-16.7873568982264));
#103244=CARTESIAN_POINT('Ctrl Pts',(-17.3101542708379,20.7779762056212,
-16.7849073280805));
#103245=CARTESIAN_POINT('Ctrl Pts',(-17.3344436483625,20.7997079145158,
-16.7828648986443));
#103246=CARTESIAN_POINT('Ctrl Pts',(-17.4829168238425,20.9264992702536,
-16.7704577413008));
#103247=CARTESIAN_POINT('Ctrl Pts',(-17.6183682463526,21.0175194677178,
-16.7595039646589));
#103248=CARTESIAN_POINT('Ctrl Pts',(-17.8667255663329,21.1457287814896,
-16.7412474600421));
#103249=CARTESIAN_POINT('Ctrl Pts',(-17.9748185377253,21.1906443420851,
-16.7338049997294));
#103250=CARTESIAN_POINT('Ctrl Pts',(-18.0996629589965,21.2307794421858,
-16.7257980292985));
#103251=CARTESIAN_POINT('Ctrl Pts',(-18.1132870171746,21.2350078767764,
-16.7249315812421));
#103252=CARTESIAN_POINT('Ctrl Pts',(-18.1350456189993,21.2415206245296,
-16.7235592271816));
#103253=CARTESIAN_POINT('Ctrl Pts',(-18.143152713155,21.2438944497979,-16.7230504060531));
#103254=CARTESIAN_POINT('Ctrl Pts',(-18.1574800530819,21.2479966678452,
-16.7221555389638));
#103255=CARTESIAN_POINT('Ctrl Pts',(-18.1636943625298,21.2497452404134,
-16.7217688392333));
#103256=CARTESIAN_POINT('Ctrl Pts',(-18.1765681302003,21.2533041727919,
-16.7209706722368));
#103257=CARTESIAN_POINT('Ctrl Pts',(-18.1832286444323,21.2551104518327,
-16.7205593415882));
#103258=CARTESIAN_POINT('Ctrl Pts',(-18.2003563993105,21.2596655713613,
-16.7195056745142));
#103259=CARTESIAN_POINT('Ctrl Pts',(-18.2108361826824,21.2623667986662,
-16.7188648848971));
#103260=CARTESIAN_POINT('Ctrl Pts',(-18.2547333722116,21.273323287774,-16.7161966199843));
#103261=CARTESIAN_POINT('Ctrl Pts',(-18.2883299930917,21.2808435417425,
-16.7141928453244));
#103262=CARTESIAN_POINT('Ctrl Pts',(-18.3764011492549,21.2983133654515,
-16.7090277642644));
#103263=CARTESIAN_POINT('Ctrl Pts',(-18.4311098697273,21.3069513939323,
-16.7059062700289));
#103264=CARTESIAN_POINT('Ctrl Pts',(-18.5949037264779,21.3262646694435,
-16.6967375565202));
#103265=CARTESIAN_POINT('Ctrl Pts',(-18.7045446938713,21.3306286558589,
-16.6908389834021));
#103266=CARTESIAN_POINT('Ctrl Pts',(-18.8743201135194,21.3242059362996,
-16.6815879088552));
#103267=CARTESIAN_POINT('Ctrl Pts',(-18.9344822662438,21.3193489445556,
-16.6782842403984));
#103268=CARTESIAN_POINT('Ctrl Pts',(-19.0521688847756,21.3047649593261,
-16.6716413980506));
#103269=CARTESIAN_POINT('Ctrl Pts',(-19.1096601591585,21.2952171903307,
-16.6683100094204));
#103270=CARTESIAN_POINT('Ctrl Pts',(-19.1753962908968,21.2814921207549,
-16.66432638293));
#103271=CARTESIAN_POINT('Ctrl Pts',(-19.1841020488695,21.2796170373071,
-16.6637952399934));
#103272=CARTESIAN_POINT('Ctrl Pts',(-19.1972109821879,21.2767069111776,
-16.662989710264));
#103273=CARTESIAN_POINT('Ctrl Pts',(-19.2016232210985,21.2757125657397,
-16.6627175984626));
#103274=CARTESIAN_POINT('Ctrl Pts',(-19.2095092346167,21.2739087934581,
-16.6622294347398));
#103275=CARTESIAN_POINT('Ctrl Pts',(-19.2129841798264,21.2731047203139,
-16.662013692306));
#103276=CARTESIAN_POINT('Ctrl Pts',(-19.2204981936619,21.2713460225014,
-16.6615457961641));
#103277=CARTESIAN_POINT('Ctrl Pts',(-19.2245364361732,21.2703883142762,
-16.6612934720148));
#103278=CARTESIAN_POINT('Ctrl Pts',(-19.2357911658836,21.267684164843,-16.6605878759697));
#103279=CARTESIAN_POINT('Ctrl Pts',(-19.2430012379439,21.2659116438646,
-16.6601331433608));
#103280=CARTESIAN_POINT('Ctrl Pts',(-19.2844887482649,21.2554806318736,
-16.6575015298148));
#103281=CARTESIAN_POINT('Ctrl Pts',(-19.3185521936582,21.246003024397,-16.6552816515936));
#103282=CARTESIAN_POINT('Ctrl Pts',(-19.4266352137431,21.2129932221847,
-16.6480819461551));
#103283=CARTESIAN_POINT('Ctrl Pts',(-19.4996010915503,21.1862401713975,
-16.6429860613657));
#103284=CARTESIAN_POINT('Ctrl Pts',(-19.7409861171084,21.0823485349081,
-16.6256430936995));
#103285=CARTESIAN_POINT('Ctrl Pts',(-19.9007479225477,20.987145413116,-16.6134216776107));
#103286=CARTESIAN_POINT('Ctrl Pts',(-20.0655029094118,20.8570256499575,
-16.6004774142145));
#103287=CARTESIAN_POINT('Ctrl Pts',(-20.084638660179,20.8413606131972,-16.5989662136807));
#103288=CARTESIAN_POINT('Ctrl Pts',(-20.1109989140703,20.8189986909739,
-16.5968726456078));
#103289=CARTESIAN_POINT('Ctrl Pts',(-20.1184572411664,20.8125817031984,
-16.5962789308566));
#103290=CARTESIAN_POINT('Ctrl Pts',(-20.130407174693,20.8021543771936,-16.5953253637832));
#103291=CARTESIAN_POINT('Ctrl Pts',(-20.1349268158889,20.7981765205181,
-16.5949641726114));
#103292=CARTESIAN_POINT('Ctrl Pts',(-20.1439814152561,20.7901385175708,
-16.5942394507293));
#103293=CARTESIAN_POINT('Ctrl Pts',(-20.1485159557699,20.7860779857233,
-16.5938759411892));
#103294=CARTESIAN_POINT('Ctrl Pts',(-20.1592298922481,20.7764004242386,
-16.5930156685046));
#103295=CARTESIAN_POINT('Ctrl Pts',(-20.1653937195489,20.7707662506442,
-16.5925196350218));
#103296=CARTESIAN_POINT('Ctrl Pts',(-20.184588461652,20.7530112920262,-16.5909712942578));
#103297=CARTESIAN_POINT('Ctrl Pts',(-20.1975001920023,20.7407623758299,
-16.5899244623274));
#103298=CARTESIAN_POINT('Ctrl Pts',(-20.227213982116,20.7118533467546,-16.5875016062618));
#103299=CARTESIAN_POINT('Ctrl Pts',(-20.24389441538,20.6950713198551,-16.586130917355));
#103300=CARTESIAN_POINT('Ctrl Pts',(-20.3005974538237,20.6360770734237,
-16.5814288147065));
#103301=CARTESIAN_POINT('Ctrl Pts',(-20.339160850276,20.5924961570511,-16.5781560024563));
#103302=CARTESIAN_POINT('Ctrl Pts',(-20.4801364601401,20.4192928289693,
-16.5657682510421));
#103303=CARTESIAN_POINT('Ctrl Pts',(-20.569035385705,20.2794581754388,-16.5570654750764));
#103304=CARTESIAN_POINT('Ctrl Pts',(-20.6663071211393,20.0777938445973,
-16.5445283610871));
#103305=CARTESIAN_POINT('Ctrl Pts',(-20.6896202179217,20.0238287764598,
-16.5411692222945));
#103306=CARTESIAN_POINT('Ctrl Pts',(-20.7138514252563,19.9606378849833,
-16.5371546651799));
#103307=CARTESIAN_POINT('Ctrl Pts',(-20.7169935338606,19.9522862220692,
-16.536622475451));
#103308=CARTESIAN_POINT('Ctrl Pts',(-20.721649858507,19.939668327278,-16.5358156634409));
#103309=CARTESIAN_POINT('Ctrl Pts',(-20.7232033880908,19.9354165729295,
-16.5355433269061));
#103310=CARTESIAN_POINT('Ctrl Pts',(-20.7259567193341,19.9278055194853,
-16.5350549211475));
#103311=CARTESIAN_POINT('Ctrl Pts',(-20.7271616776866,19.9244481416342,
-16.5348391626884));
#103312=CARTESIAN_POINT('Ctrl Pts',(-20.7297493394559,19.9171804133919,
-16.5343714183857));
#103313=CARTESIAN_POINT('Ctrl Pts',(-20.7311290194295,19.9132690946268,
-16.5341192631044));
#103314=CARTESIAN_POINT('Ctrl Pts',(-20.7349423505326,19.9023563858777,
-16.5334146049514));
#103315=CARTESIAN_POINT('Ctrl Pts',(-20.7373507096332,19.8953463106673,
-16.5329606475306));
#103316=CARTESIAN_POINT('Ctrl Pts',(-20.7509691776094,19.8550186845975,
-16.5303422500017));
#103317=CARTESIAN_POINT('Ctrl Pts',(-20.7613841536692,19.8214407331623,
-16.5281353059032));
#103318=CARTESIAN_POINT('Ctrl Pts',(-20.7919130222082,19.7135952627408,
-16.5209960174452));
#103319=CARTESIAN_POINT('Ctrl Pts',(-20.8088160422474,19.6384865911504,
-16.5159496203879));
#103320=CARTESIAN_POINT('Ctrl Pts',(-20.8410710378816,19.4469921103544,
-16.5031356999716));
#103321=CARTESIAN_POINT('Ctrl Pts',(-20.8509078633986,19.3299290089427,
-16.4953606780472));
#103322=CARTESIAN_POINT('Ctrl Pts',(-20.8509993557841,19.2126515476976,
-16.4878149913274));
#103323=CARTESIAN_POINT('Ctrl Pts',(-20.8509993578195,19.2126489366114,
-16.487814823329));
#103324=CARTESIAN_POINT('Ctrl Pts',(-20.8510649772153,19.1284029942412,
-16.4823944024007));
#103325=CARTESIAN_POINT('Ctrl Pts',(-20.8461018020696,19.0442181851613,
-16.4770995077269));
#103326=CARTESIAN_POINT('Ctrl Pts',(-20.8349011956226,18.9502100090101,
-16.4713271189853));
#103327=CARTESIAN_POINT('Ctrl Pts',(-20.833594095754,18.9398876758388,-16.4706951411389));
#103328=CARTESIAN_POINT('Ctrl Pts',(-20.8312616517224,18.9224977355724,
-16.4696334764133));
#103329=CARTESIAN_POINT('Ctrl Pts',(-20.8302765596053,18.9154250011086,
-16.4692025271686));
#103330=CARTESIAN_POINT('Ctrl Pts',(-20.8283990632567,18.9024267191727,
-16.4684120439715));
#103331=CARTESIAN_POINT('Ctrl Pts',(-20.8275172537553,18.8964997373783,
-16.4680521786698));
#103332=CARTESIAN_POINT('Ctrl Pts',(-20.8256463309034,18.884281180415,-16.4673114810221));
#103333=CARTESIAN_POINT('Ctrl Pts',(-20.8246539665023,18.8779901587472,
-16.4669307557886));
#103334=CARTESIAN_POINT('Ctrl Pts',(-20.8223696978179,18.8639219737229,
-16.4660807594744));
#103335=CARTESIAN_POINT('Ctrl Pts',(-20.8210627053305,18.8561473296156,
-16.4656119724461));
#103336=CARTESIAN_POINT('Ctrl Pts',(-20.8176411999454,18.8364675613506,
-16.4644276657821));
#103337=CARTESIAN_POINT('Ctrl Pts',(-20.8154680492599,18.8245728183502,
-16.4637140127177));
#103338=CARTESIAN_POINT('Ctrl Pts',(-20.8024833903227,18.7567911956213,
-16.4596587181026));
#103339=CARTESIAN_POINT('Ctrl Pts',(-20.7895226775756,18.7013368482678,
-16.4563862764759));
#103340=CARTESIAN_POINT('Ctrl Pts',(-20.7635221427499,18.6073651777507,
-16.4508784635452));
#103341=CARTESIAN_POINT('Ctrl Pts',(-20.7515806204613,18.5685797404864,
-16.4486162141156));
#103342=CARTESIAN_POINT('Ctrl Pts',(-20.7333842942261,18.5150060471336,
-16.4454901482646));
#103343=CARTESIAN_POINT('Ctrl Pts',(-20.728066946463,18.4999150047001,-16.4446094023785));
#103344=CARTESIAN_POINT('Ctrl Pts',(-20.7225806308032,18.4848897640204,
-16.4437314734851));
#103345=CARTESIAN_POINT('Origin',(-18.734,19.211,0.));
#103346=CARTESIAN_POINT('',(-20.7225806137986,18.4848897174502,-15.646496294977));
#103347=CARTESIAN_POINT('',(-20.722580613579,18.4848897168489,-15.866216451952));
#103348=CARTESIAN_POINT('',(-20.7225806137986,18.4848897174502,0.));
#103349=CARTESIAN_POINT('Ctrl Pts',(-20.722580613579,18.4848897168488,-15.866216451952));
#103350=CARTESIAN_POINT('Ctrl Pts',(-20.7307297100332,18.5072074495721,
-15.8675066849164));
#103351=CARTESIAN_POINT('Ctrl Pts',(-20.7385063121739,18.5296711603929,
-15.868797221955));
#103352=CARTESIAN_POINT('Ctrl Pts',(-20.7729860000107,18.6349799787421,
-15.8748264466111));
#103353=CARTESIAN_POINT('Ctrl Pts',(-20.794937948196,18.7192730939136,-15.8795907956239));
#103354=CARTESIAN_POINT('Ctrl Pts',(-20.8189001290662,18.8417961064723,
-15.8867186669764));
#103355=CARTESIAN_POINT('Ctrl Pts',(-20.8251640448533,18.8791075455718,
-15.8889160607276));
#103356=CARTESIAN_POINT('Ctrl Pts',(-20.8314778226034,18.9240625158185,
-15.8916170096321));
#103357=CARTESIAN_POINT('Ctrl Pts',(-20.8324907017386,18.931566453459,-15.8920696325401));
#103358=CARTESIAN_POINT('Ctrl Pts',(-20.834000499107,18.9432232351928,-15.8927757277816));
#103359=CARTESIAN_POINT('Ctrl Pts',(-20.8345254154019,18.9473724775823,
-15.8930276485012));
#103360=CARTESIAN_POINT('Ctrl Pts',(-20.8354748337427,18.9550601170607,
-15.8934955314825));
#103361=CARTESIAN_POINT('Ctrl Pts',(-20.8359026977821,18.9585980408009,
-15.8937113018391));
#103362=CARTESIAN_POINT('Ctrl Pts',(-20.8368482734237,18.9665859874486,
-15.8941994721526));
#103363=CARTESIAN_POINT('Ctrl Pts',(-20.837360790736,18.9710365575475,-15.8944721591287));
#103364=CARTESIAN_POINT('Ctrl Pts',(-20.8388276186419,18.9841399585073,
-15.8952769913044));
#103365=CARTESIAN_POINT('Ctrl Pts',(-20.8397426747612,18.9927969653412,
-15.8958112646172));
#103366=CARTESIAN_POINT('Ctrl Pts',(-20.8458591845623,19.0542888830302,
-15.8996231613316));
#103367=CARTESIAN_POINT('Ctrl Pts',(-20.8491244445647,19.1072929582799,
-15.9029969361203));
#103368=CARTESIAN_POINT('Ctrl Pts',(-20.8507874983447,19.1767948294316,
-15.90748929889));
#103369=CARTESIAN_POINT('Ctrl Pts',(-20.8509892979912,19.1932348606781,
-15.9085569697079));
#103370=CARTESIAN_POINT('Ctrl Pts',(-20.8510113338606,19.2284498580906,
-15.910852706117));
#103371=CARTESIAN_POINT('Ctrl Pts',(-20.8507733280713,19.2472234825081,
-15.9120819250805));
#103372=CARTESIAN_POINT('Ctrl Pts',(-20.8462294560163,19.4220903742844,
-15.9235687404762));
#103373=CARTESIAN_POINT('Ctrl Pts',(-20.8249133703867,19.5772840818688,
-15.9339904580781));
#103374=CARTESIAN_POINT('Ctrl Pts',(-20.7855430759336,19.7333821023551,
-15.9442509355322));
#103375=CARTESIAN_POINT('Ctrl Pts',(-20.784353024173,19.7380337086545,-15.9445565309553));
#103376=CARTESIAN_POINT('Ctrl Pts',(-20.7672421603605,19.8039805098056,
-15.9488867117748));
#103377=CARTESIAN_POINT('Ctrl Pts',(-20.7485934598733,19.864539659252,-15.9528332812358));
#103378=CARTESIAN_POINT('Ctrl Pts',(-20.7230405459961,19.9359574164032,
-15.9574537212672));
#103379=CARTESIAN_POINT('Ctrl Pts',(-20.718721079733,19.9477006145155,-15.9582123980706));
#103380=CARTESIAN_POINT('Ctrl Pts',(-20.7114648628223,19.9669007387437,
-15.9594512520348));
#103381=CARTESIAN_POINT('Ctrl Pts',(-20.7085894774242,19.9743803828571,
-15.9599334664468));
#103382=CARTESIAN_POINT('Ctrl Pts',(-20.7033486448,19.9877854382339,-15.9607970376303));
#103383=CARTESIAN_POINT('Ctrl Pts',(-20.7009987608544,19.9937167929752,
-15.9611789113749));
#103384=CARTESIAN_POINT('Ctrl Pts',(-20.6959424920753,20.0063127670094,
-15.9619894127401));
#103385=CARTESIAN_POINT('Ctrl Pts',(-20.6932288753261,20.0129744108306,
-15.9624177907137));
#103386=CARTESIAN_POINT('Ctrl Pts',(-20.6858435314514,20.0308434331864,
-15.9635662045171));
#103387=CARTESIAN_POINT('Ctrl Pts',(-20.6811092070372,20.0420247717955,
-15.9642841130527));
#103388=CARTESIAN_POINT('Ctrl Pts',(-20.6571530390825,20.0972747076518,
-15.9678287989931));
#103389=CARTESIAN_POINT('Ctrl Pts',(-20.6365292042092,20.140722332489,-15.9706072964359));
#103390=CARTESIAN_POINT('Ctrl Pts',(-20.537430530737,20.3323544925586,-15.9828819631902));
#103391=CARTESIAN_POINT('Ctrl Pts',(-20.4430046554724,20.4715959672653,
-15.9918001711245));
#103392=CARTESIAN_POINT('Ctrl Pts',(-20.2684506691017,20.6728123011067,
-16.006384006276));
#103393=CARTESIAN_POINT('Ctrl Pts',(-20.1986341131656,20.7427558065264,
-16.0118767442219));
#103394=CARTESIAN_POINT('Ctrl Pts',(-20.1168931570434,20.8139315365527,
-16.0182979854958));
#103395=CARTESIAN_POINT('Ctrl Pts',(-20.1095379821638,20.8202477268045,
-16.0188757238266));
#103396=CARTESIAN_POINT('Ctrl Pts',(-20.0986146029711,20.829498478691,-16.0197341066941));
#103397=CARTESIAN_POINT('Ctrl Pts',(-20.0950796402505,20.832472340848,-16.0200119478965));
#103398=CARTESIAN_POINT('Ctrl Pts',(-20.0887912537901,20.8377275261928,
-16.02050636037));
#103399=CARTESIAN_POINT('Ctrl Pts',(-20.0860417540102,20.840013468644,-16.0207225896597));
#103400=CARTESIAN_POINT('Ctrl Pts',(-20.0801385590999,20.8448961619581,
-16.0211869705248));
#103401=CARTESIAN_POINT('Ctrl Pts',(-20.0769831828514,20.8474907143895,
-16.0214352683525));
#103402=CARTESIAN_POINT('Ctrl Pts',(-20.0683014447642,20.8545873765871,
-16.0221186008423));
#103403=CARTESIAN_POINT('Ctrl Pts',(-20.0627598822913,20.8590706847272,
-16.0225549530334));
#103404=CARTESIAN_POINT('Ctrl Pts',(-20.0330577939349,20.8828534781246,
-16.0248942170763));
#103405=CARTESIAN_POINT('Ctrl Pts',(-20.0085005716585,20.901648770122,-16.0268299014795));
#103406=CARTESIAN_POINT('Ctrl Pts',(-19.932933751769,20.9569030366703,-16.0327692717061));
#103407=CARTESIAN_POINT('Ctrl Pts',(-19.8807099081991,20.9916388860111,
-16.0368503877224));
#103408=CARTESIAN_POINT('Ctrl Pts',(-19.7118261425579,21.0934557365582,
-16.0498094075512));
#103409=CARTESIAN_POINT('Ctrl Pts',(-19.5902575871588,21.1517760577781,
-16.0587750607433));
#103410=CARTESIAN_POINT('Ctrl Pts',(-19.4256423433035,21.2122464581395,
-16.070068511563));
#103411=CARTESIAN_POINT('Ctrl Pts',(-19.3869104230107,21.2252156826393,
-16.0726704582485));
#103412=CARTESIAN_POINT('Ctrl Pts',(-19.3014161601891,21.2511175062419,
-16.0782894329313));
#103413=CARTESIAN_POINT('Ctrl Pts',(-19.2545345849612,21.263580056514,-16.0812910430167));
#103414=CARTESIAN_POINT('Ctrl Pts',(-19.1949880136887,21.2772375603902,
-16.0850069101745));
#103415=CARTESIAN_POINT('Ctrl Pts',(-19.182687825865,21.279943414016,-16.0857693783274));
#103416=CARTESIAN_POINT('Ctrl Pts',(-19.1631556912682,21.2840578038541,
-16.0869722487119));
#103417=CARTESIAN_POINT('Ctrl Pts',(-19.1559394242275,21.2855385968664,
-16.0874149563323));
#103418=CARTESIAN_POINT('Ctrl Pts',(-19.1424772963141,21.2882279043537,
-16.0882377213378));
#103419=CARTESIAN_POINT('Ctrl Pts',(-19.1362334522104,21.2894459866734,
-16.0886180804136));
#103420=CARTESIAN_POINT('Ctrl Pts',(-19.1223512244561,21.2920893062284,
-16.0894610260287));
#103421=CARTESIAN_POINT('Ctrl Pts',(-19.1147102694432,21.2935006764078,
-16.0899231659309));
#103422=CARTESIAN_POINT('Ctrl Pts',(-19.0924792090676,21.2974805580513,
-16.0912625446952));
#103423=CARTESIAN_POINT('Ctrl Pts',(-19.0778695114745,21.2999380647179,
-16.0921362521435));
#103424=CARTESIAN_POINT('Ctrl Pts',(-18.9612382451843,21.3182999217235,
-16.099061874341));
#103425=CARTESIAN_POINT('Ctrl Pts',(-18.8581967684149,21.3268755546564,
-16.1048707616966));
#103426=CARTESIAN_POINT('Ctrl Pts',(-18.5952918642965,21.3294748462361,
-16.1193460729866));
#103427=CARTESIAN_POINT('Ctrl Pts',(-18.43600367459,21.3129909410084,-16.1277744129058));
#103428=CARTESIAN_POINT('Ctrl Pts',(-18.2326864338793,21.268359863854,-16.1395294966699));
#103429=CARTESIAN_POINT('Ctrl Pts',(-18.1856534243482,21.2563264154215,
-16.1423242868963));
#103430=CARTESIAN_POINT('Ctrl Pts',(-18.1316337975706,21.240508352135,-16.1456660238248));
#103431=CARTESIAN_POINT('Ctrl Pts',(-18.1242001908566,21.2382871976641,
-16.1461288129868));
#103432=CARTESIAN_POINT('Ctrl Pts',(-18.1123333597317,21.2346702273449,
-16.1468725470988));
#103433=CARTESIAN_POINT('Ctrl Pts',(-18.1078921519508,21.2333005618189,
-16.147152004985));
#103434=CARTESIAN_POINT('Ctrl Pts',(-18.1000300681276,21.2308475193983,
-16.1476487500638));
#103435=CARTESIAN_POINT('Ctrl Pts',(-18.0966073939111,21.2297700566625,
-16.1478656887423));
#103436=CARTESIAN_POINT('Ctrl Pts',(-18.0893538583262,21.227466347509,-16.1483269153705));
#103437=CARTESIAN_POINT('Ctrl Pts',(-18.0855238073938,21.2262379029809,
-16.1485713256125));
#103438=CARTESIAN_POINT('Ctrl Pts',(-18.075186052926,21.222889665751,-16.1492333274271));
#103439=CARTESIAN_POINT('Ctrl Pts',(-18.0686851558668,21.2207492378983,
-16.1496521053904));
#103440=CARTESIAN_POINT('Ctrl Pts',(-18.036345475416,21.2099272570659,-16.1517473413617));
#103441=CARTESIAN_POINT('Ctrl Pts',(-18.0106669607787,21.2007791751567,
-16.1534491360682));
#103442=CARTESIAN_POINT('Ctrl Pts',(-17.9367523830499,21.1728269973373,
-16.1584445029613));
#103443=CARTESIAN_POINT('Ctrl Pts',(-17.8890221570268,21.1527468047928,
-16.161791281838));
#103444=CARTESIAN_POINT('Ctrl Pts',(-17.7166761289524,21.0726822901161,
-16.1742133112566));
#103445=CARTESIAN_POINT('Ctrl Pts',(-17.5972714955827,21.0022736173384,
-16.1834597839596));
#103446=CARTESIAN_POINT('Ctrl Pts',(-17.4529915619666,20.8969226903731,
-16.1950273585044));
#103447=CARTESIAN_POINT('Ctrl Pts',(-17.4210820545858,20.8721937561901,
-16.1976159110248));
#103448=CARTESIAN_POINT('Ctrl Pts',(-17.3444281223032,20.8091998424504,
-16.2039028856977));
#103449=CARTESIAN_POINT('Ctrl Pts',(-17.3005335187298,20.7699508192764,
-16.2075631952157));
#103450=CARTESIAN_POINT('Ctrl Pts',(-17.2495685115031,20.7204043217027,
-16.2118911509734));
#103451=CARTESIAN_POINT('Ctrl Pts',(-17.240882618768,20.7118126952076,-16.2126317007576));
#103452=CARTESIAN_POINT('Ctrl Pts',(-17.2266874285987,20.6975263456261,
-16.2138470137106));
#103453=CARTESIAN_POINT('Ctrl Pts',(-17.221134949198,20.6918751145416,-16.2143236849716));
#103454=CARTESIAN_POINT('Ctrl Pts',(-17.2111742270243,20.6816227471235,
-16.2151812099355));
#103455=CARTESIAN_POINT('Ctrl Pts',(-17.2067548074559,20.6770326471202,
-16.2155625508318));
#103456=CARTESIAN_POINT('Ctrl Pts',(-17.1973490510837,20.6671749449462,
-16.21637605918));
#103457=CARTESIAN_POINT('Ctrl Pts',(-17.1923689165333,20.6619015175376,
-16.2168079553886));
#103458=CARTESIAN_POINT('Ctrl Pts',(-17.1789387457425,20.6475331919123,
-16.2179759198169));
#103459=CARTESIAN_POINT('Ctrl Pts',(-17.1705413646107,20.6383893026341,
-16.2187097318021));
#103460=CARTESIAN_POINT('Ctrl Pts',(-17.1276891071625,20.5908956837354,
-16.2224736412004));
#103461=CARTESIAN_POINT('Ctrl Pts',(-17.0945613355072,20.5513687107548,
-16.225447785162));
#103462=CARTESIAN_POINT('Ctrl Pts',(-16.9568346737977,20.3742821172794,
-16.2381786686098));
#103463=CARTESIAN_POINT('Ctrl Pts',(-16.8678615545447,20.2254304265473,
-16.247331349834));
#103464=CARTESIAN_POINT('Ctrl Pts',(-16.7616825013397,19.9854006088846,
-16.2617545809859));
#103465=CARTESIAN_POINT('Ctrl Pts',(-16.7306535929744,19.9011679363643,
-16.26677469244));
#103466=CARTESIAN_POINT('Ctrl Pts',(-16.7023069985309,19.8059837817041,
-16.2726590244218));
#103467=CARTESIAN_POINT('Ctrl Pts',(-16.6996155989034,19.7967151639812,
-16.2732342028016));
#103468=CARTESIAN_POINT('Ctrl Pts',(-16.6957321970007,19.7829918053178,
-16.2740894950867));
#103469=CARTESIAN_POINT('Ctrl Pts',(-16.6944911781576,19.778550902386,-16.2743668346848));
#103470=CARTESIAN_POINT('Ctrl Pts',(-16.6923138083745,19.7706599632556,
-16.2748606939627));
#103471=CARTESIAN_POINT('Ctrl Pts',(-16.6913716771482,19.7672115730687,
-16.2750768745022));
#103472=CARTESIAN_POINT('Ctrl Pts',(-16.6893702219578,19.7598121744544,
-16.2755415352424));
#103473=CARTESIAN_POINT('Ctrl Pts',(-16.6883136293299,19.7558605365472,
-16.2757901637037));
#103474=CARTESIAN_POINT('Ctrl Pts',(-16.6854410361121,19.7449909435058,
-16.2764753171759));
#103475=CARTESIAN_POINT('Ctrl Pts',(-16.683648651203,19.7380668832247,-16.2769131711832));
#103476=CARTESIAN_POINT('Ctrl Pts',(-16.6742110604741,19.7008323217873,
-16.2792747866716));
#103477=CARTESIAN_POINT('Ctrl Pts',(-16.6672032640702,19.6703660748689,
-16.2812320516721));
#103478=CARTESIAN_POINT('Ctrl Pts',(-16.6276983622846,19.4793522263671,
-16.2936116224414));
#103479=CARTESIAN_POINT('Ctrl Pts',(-16.6132527178837,19.3156433572303,
-16.3046448268863));
#103480=CARTESIAN_POINT('Ctrl Pts',(-16.6210948451834,19.0348061329448,
-16.3229983368271));
#103481=CARTESIAN_POINT('Ctrl Pts',(-16.6340792518069,18.9181635375945,
-16.3304615466166));
#103482=CARTESIAN_POINT('Ctrl Pts',(-16.6594067217434,18.7891516385093,
-16.3384894193511));
#103483=CARTESIAN_POINT('Ctrl Pts',(-16.6623023195749,18.7751536429743,
-16.3393576643713));
#103484=CARTESIAN_POINT('Ctrl Pts',(-16.6671361852646,18.7529230724605,
-16.3407323170003));
#103485=CARTESIAN_POINT('Ctrl Pts',(-16.6689823540701,18.7446711187955,
-16.3412416549584));
#103486=CARTESIAN_POINT('Ctrl Pts',(-16.672325390675,18.7301377565633,-16.3421371230851));
#103487=CARTESIAN_POINT('Ctrl Pts',(-16.6738016388605,18.7238517616893,
-16.3425239097957));
#103488=CARTESIAN_POINT('Ctrl Pts',(-16.67691430618,18.7108649938352,-16.3433219614256));
#103489=CARTESIAN_POINT('Ctrl Pts',(-16.6785547625418,18.7041652600187,
-16.3437330911813));
#103490=CARTESIAN_POINT('Ctrl Pts',(-16.6828492642127,18.6869900426648,
-16.3447856330288));
#103491=CARTESIAN_POINT('Ctrl Pts',(-16.6855508476377,18.6765265646941,
-16.3454255047846));
#103492=CARTESIAN_POINT('Ctrl Pts',(-16.6971573633127,18.6329545722423,
-16.3480848382461));
#103493=CARTESIAN_POINT('Ctrl Pts',(-16.7067860851717,18.6000430596461,
-16.350080801271));
#103494=CARTESIAN_POINT('Ctrl Pts',(-16.7339499873085,18.514924902796,-16.3552212001254));
#103495=CARTESIAN_POINT('Ctrl Pts',(-16.7527303146239,18.4631419438977,
-16.3583263208017));
#103496=CARTESIAN_POINT('Ctrl Pts',(-16.8147573454043,18.3109194007014,
-16.3674664772092));
#103497=CARTESIAN_POINT('Ctrl Pts',(-16.8637846761917,18.2130355803018,
-16.3733527694772));
#103498=CARTESIAN_POINT('Ctrl Pts',(-16.9417130856346,18.0835493053502,
-16.381580605132));
#103499=CARTESIAN_POINT('Ctrl Pts',(-16.9643308080253,18.0483701229774,
-16.3838660861657));
#103500=CARTESIAN_POINT('Ctrl Pts',(-17.0313688610994,17.9505932973252,
-16.3904244396197));
#103501=CARTESIAN_POINT('Ctrl Pts',(-17.0781674680437,17.8897150961318,
-16.3947571235019));
#103502=CARTESIAN_POINT('Ctrl Pts',(-17.1343529255045,17.8243102223344,
-16.3998672466576));
#103503=CARTESIAN_POINT('Ctrl Pts',(-17.140593455917,17.8171438811401,-16.4004336703677));
#103504=CARTESIAN_POINT('Ctrl Pts',(-17.1499141495439,17.8065848145464,
-16.4012783851386));
#103505=CARTESIAN_POINT('Ctrl Pts',(-17.1529575211923,17.803159570815,-16.4015540000756));
#103506=CARTESIAN_POINT('Ctrl Pts',(-17.1583931390188,17.797081763818,-16.4020459658933));
#103507=CARTESIAN_POINT('Ctrl Pts',(-17.160781002238,17.7944253483032,-16.4022619874058));
#103508=CARTESIAN_POINT('Ctrl Pts',(-17.1659305135167,17.7887257744956,
-16.4027276495945));
#103509=CARTESIAN_POINT('Ctrl Pts',(-17.1686942620905,17.7856846548296,
-16.4029774455902));
#103510=CARTESIAN_POINT('Ctrl Pts',(-17.176350428545,17.7773092371958,-16.4036690391799));
#103511=CARTESIAN_POINT('Ctrl Pts',(-17.1812613228103,17.7719920126428,
-16.404112206673));
#103512=CARTESIAN_POINT('Ctrl Pts',(-17.2083631610853,17.7429480128418,
-16.4065549887513));
#103513=CARTESIAN_POINT('Ctrl Pts',(-17.2310694535619,17.7197106565648,
-16.4085908318708));
#103514=CARTESIAN_POINT('Ctrl Pts',(-17.370688834416,17.5832537899217,-16.4209957699345));
#103515=CARTESIAN_POINT('Ctrl Pts',(-17.4998028544643,17.4833043126514,
-16.4319555752646));
#103516=CARTESIAN_POINT('Ctrl Pts',(-17.7390722945051,17.3387140770515,
-16.4502166179063));
#103517=CARTESIAN_POINT('Ctrl Pts',(-17.8438954085251,17.2866670401905,
-16.4576579831164));
#103518=CARTESIAN_POINT('Ctrl Pts',(-17.9657768170427,17.2382540960564,
-16.4656656888531));
#103519=CARTESIAN_POINT('Ctrl Pts',(-17.979112634985,17.2331126568417,-16.4665338263646));
#103520=CARTESIAN_POINT('Ctrl Pts',(-18.0004194121345,17.2251450171892,
-16.4679083414871));
#103521=CARTESIAN_POINT('Ctrl Pts',(-18.0083568249097,17.2222309140243,
-16.4684176485354));
#103522=CARTESIAN_POINT('Ctrl Pts',(-18.0223860568188,17.21717546241,-16.4693130807066));
#103523=CARTESIAN_POINT('Ctrl Pts',(-18.0284705731536,17.2150142986202,
-16.4696998622056));
#103524=CARTESIAN_POINT('Ctrl Pts',(-18.0410753379798,17.2106020416654,
-16.470497920687));
#103525=CARTESIAN_POINT('Ctrl Pts',(-18.0475968988859,17.2083549082632,
-16.4709090624189));
#103526=CARTESIAN_POINT('Ctrl Pts',(-18.0643641600255,17.2026689420415,
-16.4719616713599));
#103527=CARTESIAN_POINT('Ctrl Pts',(-18.0746255008292,17.199276591343,-16.4726015978474));
#103528=CARTESIAN_POINT('Ctrl Pts',(-18.1175537188811,17.1854484740681,
-16.4752614630592));
#103529=CARTESIAN_POINT('Ctrl Pts',(-18.1504468343376,17.1757282980023,
-16.4772578911056));
#103530=CARTESIAN_POINT('Ctrl Pts',(-18.2367466174557,17.1524904298777,
-16.4823997581472));
#103531=CARTESIAN_POINT('Ctrl Pts',(-18.2904712283545,17.1402500271525,
-16.4855058525303));
#103532=CARTESIAN_POINT('Ctrl Pts',(-18.4520739380687,17.11001013454,-16.4946477078393));
#103533=CARTESIAN_POINT('Ctrl Pts',(-18.5609318159898,17.0982555741269,
-16.5005347309068));
#103534=CARTESIAN_POINT('Ctrl Pts',(-18.7136383447923,17.0936521009622,
-16.5088523812844));
#103535=CARTESIAN_POINT('Ctrl Pts',(-18.7570954580702,17.0936802025071,
-16.5112275099705));
#103536=CARTESIAN_POINT('Ctrl Pts',(-18.8293122726157,17.0959504959802,
-16.5152284126781));
#103537=CARTESIAN_POINT('Ctrl Pts',(-18.8580825128274,17.0974432210305,
-16.51683663935));
#103538=CARTESIAN_POINT('Ctrl Pts',(-18.9344037809975,17.1029667625486,
-16.5211610610238));
#103539=CARTESIAN_POINT('Ctrl Pts',(-18.9818612852048,17.1080188216196,
-16.5239101472252));
#103540=CARTESIAN_POINT('Ctrl Pts',(-19.0367559107812,17.1157464166713,
-16.527201522163));
#103541=CARTESIAN_POINT('Ctrl Pts',(-19.0444022413434,17.1168655333508,
-16.5276625120003));
#103542=CARTESIAN_POINT('Ctrl Pts',(-19.0566281874649,17.1187233523931,
-16.5284039007429));
#103543=CARTESIAN_POINT('Ctrl Pts',(-19.0612118812146,17.1194352983179,
-16.5286828273594));
#103544=CARTESIAN_POINT('Ctrl Pts',(-19.0693359648415,17.1207245018154,
-16.5291789709452));
#103545=CARTESIAN_POINT('Ctrl Pts',(-19.0728772703606,17.1212956996041,
-16.5293958423454));
#103546=CARTESIAN_POINT('Ctrl Pts',(-19.0803914668496,17.1225273113743,
-16.5298573134428));
#103547=CARTESIAN_POINT('Ctrl Pts',(-19.0843638679602,17.1231900520296,
-16.5301020373918));
#103548=CARTESIAN_POINT('Ctrl Pts',(-19.0951045385767,17.1250135021463,
-16.5307657556233));
#103549=CARTESIAN_POINT('Ctrl Pts',(-19.1018690225466,17.126195803853,-16.5311859466335));
#103550=CARTESIAN_POINT('Ctrl Pts',(-19.1357278993662,17.1322836009826,
-16.5332996893001));
#103551=CARTESIAN_POINT('Ctrl Pts',(-19.1627291616918,17.1376842231241,
-16.5350191066817));
#103552=CARTESIAN_POINT('Ctrl Pts',(-19.2409367409709,17.1549197745823,
-16.5400829862256));
#103553=CARTESIAN_POINT('Ctrl Pts',(-19.2918153599703,17.168136316274,-16.5434822691979));
#103554=CARTESIAN_POINT('Ctrl Pts',(-19.4882268235893,17.2270418490906,
-16.5568920889005));
#103555=CARTESIAN_POINT('Ctrl Pts',(-19.6291636099585,17.2865162912103,
-16.5671007364737));
#103556=CARTESIAN_POINT('Ctrl Pts',(-19.8338772340138,17.4003011684494,
-16.582152932376));
#103557=CARTESIAN_POINT('Ctrl Pts',(-19.9029181156154,17.4440836420308,
-16.5872827356465));
#103558=CARTESIAN_POINT('Ctrl Pts',(-19.980145983803,17.4995711363689,-16.5930824131077));
#103559=CARTESIAN_POINT('Ctrl Pts',(-19.9909542816557,17.5074934649361,
-16.5938956881502));
#103560=CARTESIAN_POINT('Ctrl Pts',(-20.0082492474889,17.5204246554479,
-16.59519982845));
#103561=CARTESIAN_POINT('Ctrl Pts',(-20.0147831966166,17.5253693920239,
-16.5956931745885));
#103562=CARTESIAN_POINT('Ctrl Pts',(-20.0262334353305,17.5341396751493,
-16.5965589317974));
#103563=CARTESIAN_POINT('Ctrl Pts',(-20.0311618251205,17.5379491934851,
-16.5969319672758));
#103564=CARTESIAN_POINT('Ctrl Pts',(-20.0413907327298,17.5459282446111,
-16.5977070716508));
#103565=CARTESIAN_POINT('Ctrl Pts',(-20.0466882917616,17.5501014694114,
-16.5981089881652));
#103566=CARTESIAN_POINT('Ctrl Pts',(-20.0602606723611,17.5608987978843,
-16.5991400248028));
#103567=CARTESIAN_POINT('Ctrl Pts',(-20.0685059138941,17.5675599127918,
-16.5997676569238));
#103568=CARTESIAN_POINT('Ctrl Pts',(-20.0863401697637,17.5821904615574,
-16.6011282274808));
#103569=CARTESIAN_POINT('Ctrl Pts',(-20.0959095466504,17.5901832787685,
-16.6018602022666));
#103570=CARTESIAN_POINT('Ctrl Pts',(-20.1234422522698,17.6135959659674,
-16.6039724090936));
#103571=CARTESIAN_POINT('Ctrl Pts',(-20.1412185737194,17.6292334655892,
-16.6053438806744));
#103572=CARTESIAN_POINT('Ctrl Pts',(-20.2017877841306,17.6843445119854,
-16.6100495124582));
#103573=CARTESIAN_POINT('Ctrl Pts',(-20.243213840497,17.7252839156753,-16.6133249691915));
#103574=CARTESIAN_POINT('Ctrl Pts',(-20.3957047322489,17.8889526915444,
-16.6257330304248));
#103575=CARTESIAN_POINT('Ctrl Pts',(-20.49391370683,18.0228211486623,-16.6344517680048));
#103576=CARTESIAN_POINT('Ctrl Pts',(-20.604329376699,18.2175383461647,-16.6469895627226));
#103577=CARTESIAN_POINT('Ctrl Pts',(-20.631013692211,18.2694928112654,-16.6503279516777));
#103578=CARTESIAN_POINT('Ctrl Pts',(-20.6592540855346,18.3305653946573,
-16.6543193806578));
#103579=CARTESIAN_POINT('Ctrl Pts',(-20.6629425174268,18.3386760084038,
-16.6548507894081));
#103580=CARTESIAN_POINT('Ctrl Pts',(-20.668426287038,18.3509393011937,-16.6556566447636));
#103581=CARTESIAN_POINT('Ctrl Pts',(-20.670259744806,18.3550749650901,-16.6559288136484));
#103582=CARTESIAN_POINT('Ctrl Pts',(-20.6735150751846,18.3624818823369,
-16.6564170388211));
#103583=CARTESIAN_POINT('Ctrl Pts',(-20.6749419487363,18.3657508803674,
-16.6566327852967));
#103584=CARTESIAN_POINT('Ctrl Pts',(-20.6780109534993,18.3728307857159,
-16.6571006427445));
#103585=CARTESIAN_POINT('Ctrl Pts',(-20.679650120897,18.3766428669508,-16.6573529239024));
#103586=CARTESIAN_POINT('Ctrl Pts',(-20.6841897084988,18.3872863472987,
-16.658058281148));
#103587=CARTESIAN_POINT('Ctrl Pts',(-20.6870653953247,18.3941281381909,
-16.6585128163782));
#103588=CARTESIAN_POINT('Ctrl Pts',(-20.7013913801506,18.4287204088161,
-16.6608160793144));
#103589=CARTESIAN_POINT('Ctrl Pts',(-20.7122856338737,18.4566951057172,
-16.6626952662248));
#103590=CARTESIAN_POINT('Ctrl Pts',(-20.7225806137285,18.4848897172584,
-16.6645990097762));
#103591=CARTESIAN_POINT('Ctrl Pts',(-20.7225806308032,18.4848897640204,
-16.4437314734851));
#103592=CARTESIAN_POINT('Ctrl Pts',(-20.6771293833756,18.3604135263889,
-16.436458293116));
#103593=CARTESIAN_POINT('Ctrl Pts',(-20.6200812694952,18.2404523288822,
-16.4293983522549));
#103594=CARTESIAN_POINT('Ctrl Pts',(-20.5206824853801,18.0737957523732,
-16.4185943630028));
#103595=CARTESIAN_POINT('Ctrl Pts',(-20.4869124077141,18.0224023035683,
-16.4151049135036));
#103596=CARTESIAN_POINT('Ctrl Pts',(-20.4434978721318,17.9622131288376,
-16.4107316457269));
#103597=CARTESIAN_POINT('Ctrl Pts',(-20.4359446106736,17.9519383856621,
-16.4099745467869));
#103598=CARTESIAN_POINT('Ctrl Pts',(-20.4252035008078,17.9376004639855,
-16.4089021658407));
#103599=CARTESIAN_POINT('Ctrl Pts',(-20.4220927372145,17.9334795231593,
-16.4085920806201));
#103600=CARTESIAN_POINT('Ctrl Pts',(-20.4167518697292,17.9264578510226,
-16.4080604506043));
#103601=CARTESIAN_POINT('Ctrl Pts',(-20.4145292380405,17.9235514117181,
-16.407839430319));
#103602=CARTESIAN_POINT('Ctrl Pts',(-20.4102412287356,17.9179741913383,
-16.4074134205317));
#103603=CARTESIAN_POINT('Ctrl Pts',(-20.4081769867017,17.9153025755965,
-16.4072085158136));
#103604=CARTESIAN_POINT('Ctrl Pts',(-20.4026652060468,17.9082041940133,
-16.4066618876494));
#103605=CARTESIAN_POINT('Ctrl Pts',(-20.3992064723666,17.9037862130834,
-16.4063193790731));
#103606=CARTESIAN_POINT('Ctrl Pts',(-20.3867300072992,17.8879793843973,
-16.4050858505679));
#103607=CARTESIAN_POINT('Ctrl Pts',(-20.3776129039418,17.8766699727079,
-16.4041881384434));
#103608=CARTESIAN_POINT('Ctrl Pts',(-20.2674959835265,17.7429152295266,
-16.3933979815739));
#103609=CARTESIAN_POINT('Ctrl Pts',(-20.1531580344548,17.6321183781371,
-16.3827537690552));
#103610=CARTESIAN_POINT('Ctrl Pts',(-19.950393656403,17.47561281834,-16.3658987455293));
#103611=CARTESIAN_POINT('Ctrl Pts',(-19.8692390903128,17.4214698469529,
-16.359573034508));
#103612=CARTESIAN_POINT('Ctrl Pts',(-19.7557131161288,17.3565725621692,
-16.3513405752646));
#103613=CARTESIAN_POINT('Ctrl Pts',(-19.7264039572586,17.3407237121442,
-16.3492658339167));
#103614=CARTESIAN_POINT('Ctrl Pts',(-19.6825420963165,17.3183270938211,
-16.3462343591232));
#103615=CARTESIAN_POINT('Ctrl Pts',(-19.668270949049,17.3112419486188,-16.3452592206358));
#103616=CARTESIAN_POINT('Ctrl Pts',(-19.6422520423826,17.2986885492985,
-16.3435012913826));
#103617=CARTESIAN_POINT('Ctrl Pts',(-19.6305315871073,17.2931658095658,
-16.3427166413518));
#103618=CARTESIAN_POINT('Ctrl Pts',(-19.6120993731491,17.2846863549306,
-16.3414937453226));
#103619=CARTESIAN_POINT('Ctrl Pts',(-19.605421842518,17.2816563958703,-16.3410529780408));
#103620=CARTESIAN_POINT('Ctrl Pts',(-19.5986901532814,17.2786439405234,
-16.3406108755786));
#103621=CARTESIAN_POINT('Ctrl Pts',(-19.5986516685325,17.2786267198386,
-16.3406083481732));
#103622=CARTESIAN_POINT('Ctrl Pts',(-19.5985733693193,17.2785916862717,
-16.3406032061855));
#103623=CARTESIAN_POINT('Ctrl Pts',(-19.5985335547086,17.2785738734209,
-16.3406005915987));
#103624=CARTESIAN_POINT('Ctrl Pts',(-19.5984525465977,17.2785376338161,
-16.3405952720348));
#103625=CARTESIAN_POINT('Ctrl Pts',(-19.5984113529341,17.2785192070928,
-16.3405925670524));
#103626=CARTESIAN_POINT('Ctrl Pts',(-19.5983275352937,17.2784817170559,
-16.3405870633372));
#103627=CARTESIAN_POINT('Ctrl Pts',(-19.5982849113589,17.2784626538725,
-16.3405842646131));
#103628=CARTESIAN_POINT('Ctrl Pts',(-19.598198170761,17.2784238633397,-16.3405785693342));
#103629=CARTESIAN_POINT('Ctrl Pts',(-19.5981540675683,17.2784041421348,
-16.3405756736706));
#103630=CARTESIAN_POINT('Ctrl Pts',(-19.598064318164,17.2783640134328,-16.3405697812296));
#103631=CARTESIAN_POINT('Ctrl Pts',(-19.5980186708474,17.2783436055714,
-16.3405667843869));
#103632=CARTESIAN_POINT('Ctrl Pts',(-19.597925780192,17.2783020802525,-16.3405606861292));
#103633=CARTESIAN_POINT('Ctrl Pts',(-19.59787853576,17.2782809624444,-16.3405575846498));
#103634=CARTESIAN_POINT('Ctrl Pts',(-19.5977823906201,17.2782379907184,
-16.3405512731856));
#103635=CARTESIAN_POINT('Ctrl Pts',(-19.5977334888798,17.2782161364872,
-16.340548063141));
#103636=CARTESIAN_POINT('Ctrl Pts',(-19.5976339663508,17.2781716643121,
-16.3405415304496));
#103637=CARTESIAN_POINT('Ctrl Pts',(-19.5975833446291,17.2781490461103,
-16.3405382077501));
#103638=CARTESIAN_POINT('Ctrl Pts',(-19.5974803168117,17.2781030172893,
-16.3405314454869));
#103639=CARTESIAN_POINT('Ctrl Pts',(-19.5974279098204,17.2780796064409,
-16.3405280058735));
#103640=CARTESIAN_POINT('Ctrl Pts',(-19.5973212434366,17.2780319624573,
-16.3405210053453));
#103641=CARTESIAN_POINT('Ctrl Pts',(-19.5972669832314,17.2780077291429,
-16.340517444387));
#103642=CARTESIAN_POINT('Ctrl Pts',(-19.5971565396027,17.2779584091577,
-16.3405101965509));
#103643=CARTESIAN_POINT('Ctrl Pts',(-19.5971003554038,17.277933322338,-16.3405065096329));
#103644=CARTESIAN_POINT('Ctrl Pts',(-19.5969859901241,17.2778822630506,
-16.3404990050754));
#103645=CARTESIAN_POINT('Ctrl Pts',(-19.5969278082144,17.277856290425,-16.3404951873928));
#103646=CARTESIAN_POINT('Ctrl Pts',(-19.5968093706668,17.2778034258661,
-16.3404874162982));
#103647=CARTESIAN_POINT('Ctrl Pts',(-19.5967491144018,17.2777765338812,
-16.3404834628571));
#103648=CARTESIAN_POINT('Ctrl Pts',(-19.5966264481866,17.2777217956127,
-16.3404754150362));
#103649=CARTESIAN_POINT('Ctrl Pts',(-19.5965640376004,17.2776939492908,
-16.3404713206277));
#103650=CARTESIAN_POINT('Ctrl Pts',(-19.5964369795317,17.2776372659672,
-16.3404629854526));
#103651=CARTESIAN_POINT('Ctrl Pts',(-19.5963723314514,17.2776084289628,
-16.3404587446608));
#103652=CARTESIAN_POINT('Ctrl Pts',(-19.5962407116536,17.2775497263845,
-16.3404501110717));
#103653=CARTESIAN_POINT('Ctrl Pts',(-19.5961737395157,17.2775198609072,
-16.3404457182618));
#103654=CARTESIAN_POINT('Ctrl Pts',(-19.5960373796211,17.277459061228,-16.3404367746491));
#103655=CARTESIAN_POINT('Ctrl Pts',(-19.59596799408,17.27742812832,-16.3404322240079));
#103656=CARTESIAN_POINT('Ctrl Pts',(-19.5958399344728,17.2773710460707,
-16.340423825675));
#103657=CARTESIAN_POINT('Ctrl Pts',(-19.5957812596592,17.2773448951206,
-16.3404199778665));
#103658=CARTESIAN_POINT('Ctrl Pts',(-19.5956540361996,17.277288199464,-16.3404116351068));
#103659=CARTESIAN_POINT('Ctrl Pts',(-19.5955854859827,17.277257655225,-16.3404071401146));
#103660=CARTESIAN_POINT('Ctrl Pts',(-19.5954368396001,17.2771914316386,
-16.3403973935395));
#103661=CARTESIAN_POINT('Ctrl Pts',(-19.5953567419957,17.2771557532451,
-16.340392141947));
#103662=CARTESIAN_POINT('Ctrl Pts',(-19.5951830437577,17.2770783946493,
-16.3403807541239));
#103663=CARTESIAN_POINT('Ctrl Pts',(-19.5950894416536,17.2770367159713,
-16.3403746179126));
#103664=CARTESIAN_POINT('Ctrl Pts',(-19.5948864441817,17.2769463439288,
-16.3403613110791));
#103665=CARTESIAN_POINT('Ctrl Pts',(-19.594777047193,17.2768976528207,-16.3403541405089));
#103666=CARTESIAN_POINT('Ctrl Pts',(-19.5945397803289,17.2767920726926,
-16.3403385898189));
#103667=CARTESIAN_POINT('Ctrl Pts',(-19.5944119093255,17.276735187241,-16.3403302098415));
#103668=CARTESIAN_POINT('Ctrl Pts',(-19.5941384637297,17.276613573095,-16.3403122914124));
#103669=CARTESIAN_POINT('Ctrl Pts',(-19.5939928874732,17.2765488481542,
-16.3403027530904));
#103670=CARTESIAN_POINT('Ctrl Pts',(-19.5879466551029,17.2738614384986,
-16.3399066404347));
#103671=CARTESIAN_POINT('Ctrl Pts',(-19.5820339878978,17.2712657261848,
-16.3395209938398));
#103672=CARTESIAN_POINT('Ctrl Pts',(-19.5683496169495,17.2653326976684,
-16.3386323563755));
#103673=CARTESIAN_POINT('Ctrl Pts',(-19.5605695715526,17.2620148073379,
-16.3381300326161));
#103674=CARTESIAN_POINT('Ctrl Pts',(-19.5395818879779,17.2532126435049,
-16.3367825932059));
#103675=CARTESIAN_POINT('Ctrl Pts',(-19.5263380737549,17.2478153669833,
-16.3359404247015));
#103676=CARTESIAN_POINT('Ctrl Pts',(-19.4044111537354,17.1995610985438,
-16.3282585996343));
#103677=CARTESIAN_POINT('Ctrl Pts',(-19.2924031978274,17.16563238037,-16.3217355538195));
#103678=CARTESIAN_POINT('Ctrl Pts',(-19.0189625714433,17.1069576579037,
-16.3064254854089));
#103679=CARTESIAN_POINT('Ctrl Pts',(-18.8563815570725,17.0912809823326,
-16.2978217993399));
#103680=CARTESIAN_POINT('Ctrl Pts',(-18.6612137518337,17.0950031886249,
-16.2866124962614));
#103681=CARTESIAN_POINT('Ctrl Pts',(-18.6288156799317,17.096366144434,-16.2847212281513));
#103682=CARTESIAN_POINT('Ctrl Pts',(-18.5892451537753,17.0989423863501,
-16.2823601438526));
#103683=CARTESIAN_POINT('Ctrl Pts',(-18.5820291404291,17.0994493415292,
-16.2819274963755));
#103684=CARTESIAN_POINT('Ctrl Pts',(-18.5707191812515,17.1003021880258,
-16.2812459236871));
#103685=CARTESIAN_POINT('Ctrl Pts',(-18.5666233246019,17.1006230367261,
-16.2809983814537));
#103686=CARTESIAN_POINT('Ctrl Pts',(-18.5589680781428,17.1012451359411,
-16.2805343425187));
#103687=CARTESIAN_POINT('Ctrl Pts',(-18.5554085080156,17.1015434732086,
-16.280318010716));
#103688=CARTESIAN_POINT('Ctrl Pts',(-18.547283294754,17.1022451826382,-16.2798229313329));
#103689=CARTESIAN_POINT('Ctrl Pts',(-18.5427182116542,17.1026543726659,
-16.2795438612244));
#103690=CARTESIAN_POINT('Ctrl Pts',(-18.5286853279181,17.1039581576354,
-16.2786832752382));
#103691=CARTESIAN_POINT('Ctrl Pts',(-18.5192223498878,17.1049017132848,
-16.2780991138915));
#103692=CARTESIAN_POINT('Ctrl Pts',(-18.4339755954835,17.1139821752215,
-16.2728041206773));
#103693=CARTESIAN_POINT('Ctrl Pts',(-18.3586841778058,17.1261417642554,
-16.2678966319496));
#103694=CARTESIAN_POINT('Ctrl Pts',(-18.1463146241132,17.1723160567457,
-16.2536806632996));
#103695=CARTESIAN_POINT('Ctrl Pts',(-18.0117386262373,17.2160188825045,
-16.2442435460687));
#103696=CARTESIAN_POINT('Ctrl Pts',(-17.8258254012171,17.2976935426875,
-16.2311229307906));
#103697=CARTESIAN_POINT('Ctrl Pts',(-17.7702537487403,17.3250739673241,
-16.2271842608108));
#103698=CARTESIAN_POINT('Ctrl Pts',(-17.6832499524569,17.3727929968713,
-16.2210008794221));
#103699=CARTESIAN_POINT('Ctrl Pts',(-17.6510201800112,17.3915947026587,
-16.218706056465));
#103700=CARTESIAN_POINT('Ctrl Pts',(-17.6098319690349,17.4171049824945,
-16.2157658600642));
#103701=CARTESIAN_POINT('Ctrl Pts',(-17.6004077915956,17.4230453562378,
-16.2150925815631));
#103702=CARTESIAN_POINT('Ctrl Pts',(-17.5851630853068,17.4328235918107,
-16.2140024688672));
#103703=CARTESIAN_POINT('Ctrl Pts',(-17.5793139433328,17.4366162456926,
-16.2135839667249));
#103704=CARTESIAN_POINT('Ctrl Pts',(-17.5681054991215,17.4439628292598,
-16.2127814967892));
#103705=CARTESIAN_POINT('Ctrl Pts',(-17.5627434554788,17.4475124161817,
-16.212397372646));
#103706=CARTESIAN_POINT('Ctrl Pts',(-17.5505086939385,17.4556920504556,
-16.2115203352037));
#103707=CARTESIAN_POINT('Ctrl Pts',(-17.5436467939402,17.4603381488533,
-16.2110280330906));
#103708=CARTESIAN_POINT('Ctrl Pts',(-17.5255013264748,17.4727802080444,
-16.2097249746757));
#103709=CARTESIAN_POINT('Ctrl Pts',(-17.5142658178665,17.4806458087434,
-16.2089168661951));
#103710=CARTESIAN_POINT('Ctrl Pts',(-17.4292845650414,17.5413773612578,
-16.2027930763984));
#103711=CARTESIAN_POINT('Ctrl Pts',(-17.3589250296735,17.5988294597261,
-16.1976619162658));
#103712=CARTESIAN_POINT('Ctrl Pts',(-17.1896366131574,17.7562337572102,
-16.1848680665584));
#103713=CARTESIAN_POINT('Ctrl Pts',(-17.0965815619116,17.8618291740648,
-16.1774026230317));
#103714=CARTESIAN_POINT('Ctrl Pts',(-16.9829794112793,18.0199644921558,
-16.1666393735447));
#103715=CARTESIAN_POINT('Ctrl Pts',(-16.9530034134662,18.0652735806959,
-16.1635936993806));
#103716=CARTESIAN_POINT('Ctrl Pts',(-16.9101883323203,18.1357361888307,
-16.158835922541));
#103717=CARTESIAN_POINT('Ctrl Pts',(-16.8960540260014,18.1600786492588,
-16.1571885311306));
#103718=CARTESIAN_POINT('Ctrl Pts',(-16.8790567968164,18.1907438779622,
-16.1550994406237));
#103719=CARTESIAN_POINT('Ctrl Pts',(-16.875733323864,18.1968097816774,-16.1546855345475));
#103720=CARTESIAN_POINT('Ctrl Pts',(-16.8705166336183,18.2064428579688,
-16.1540270028819));
#103721=CARTESIAN_POINT('Ctrl Pts',(-16.8686037616162,18.2099994097988,
-16.1537836097099));
#103722=CARTESIAN_POINT('Ctrl Pts',(-16.8650121395518,18.216723264081,-16.1533229267435));
#103723=CARTESIAN_POINT('Ctrl Pts',(-16.86333125366,18.2198893649859,-16.1531057752928));
#103724=CARTESIAN_POINT('Ctrl Pts',(-16.8595026039966,18.2271454106509,
-16.1526076040898));
#103725=CARTESIAN_POINT('Ctrl Pts',(-16.8573601830321,18.2312381222744,
-16.1523262515481));
#103726=CARTESIAN_POINT('Ctrl Pts',(-16.8516996201043,18.2421382972362,
-16.1515760239232));
#103727=CARTESIAN_POINT('Ctrl Pts',(-16.8482050523272,18.2489578333071,
-16.1511057276699));
#103728=CARTESIAN_POINT('Ctrl Pts',(-16.8237586672676,18.2973091739464,
-16.1477655338939));
#103729=CARTESIAN_POINT('Ctrl Pts',(-16.8041453398379,18.3394994849612,
-16.1448213375566));
#103730=CARTESIAN_POINT('Ctrl Pts',(-16.7578584182424,18.4483078538434,
-16.1372153721465));
#103731=CARTESIAN_POINT('Ctrl Pts',(-16.7331524756047,18.5156993492254,
-16.1324938667296));
#103732=CARTESIAN_POINT('Ctrl Pts',(-16.6793506439932,18.689269391624,-16.1204918437005));
#103733=CARTESIAN_POINT('Ctrl Pts',(-16.655020052626,18.7967143134445,-16.113215157046));
#103734=CARTESIAN_POINT('Ctrl Pts',(-16.6280926791828,18.9814003830941,
-16.1012114343839));
#103735=CARTESIAN_POINT('Ctrl Pts',(-16.6211610826707,19.057782449653,-16.0963862281508));
#103736=CARTESIAN_POINT('Ctrl Pts',(-16.617698500051,19.1533906761853,-16.0905240376858));
#103737=CARTESIAN_POINT('Ctrl Pts',(-16.6172662600462,19.1724100518565,
-16.0893664208595));
#103738=CARTESIAN_POINT('Ctrl Pts',(-16.6170109972927,19.2000265936093,
-16.0876974929599));
#103739=CARTESIAN_POINT('Ctrl Pts',(-16.6169838936139,19.208620517816,-16.0871798217261));
#103740=CARTESIAN_POINT('Ctrl Pts',(-16.6170280710807,19.2236697994176,
-16.0862761713489));
#103741=CARTESIAN_POINT('Ctrl Pts',(-16.6170765472014,19.2301250639966,
-16.0858894830808));
#103742=CARTESIAN_POINT('Ctrl Pts',(-16.6172278474771,19.2426457256806,
-16.085141219004));
#103743=CARTESIAN_POINT('Ctrl Pts',(-16.6173272165513,19.2487110943414,
-16.0847795388207));
#103744=CARTESIAN_POINT('Ctrl Pts',(-16.6176266400319,19.2631880670412,
-16.0839181418249));
#103745=CARTESIAN_POINT('Ctrl Pts',(-16.6178507746571,19.2715991114692,
-16.0834191823888));
#103746=CARTESIAN_POINT('Ctrl Pts',(-16.618836410441,19.301819683382,-16.0816316780201));
#103747=CARTESIAN_POINT('Ctrl Pts',(-16.6198849956165,19.3236189415175,
-16.080352107594));
#103748=CARTESIAN_POINT('Ctrl Pts',(-16.6332258364744,19.5333351579009,
-16.0681267730325));
#103749=CARTESIAN_POINT('Ctrl Pts',(-16.6702009845931,19.7188301038407,
-16.0580678304988));
#103750=CARTESIAN_POINT('Ctrl Pts',(-16.7338899023924,19.9047694489388,
-16.0473468765687));
#103751=CARTESIAN_POINT('Ctrl Pts',(-16.7365964021646,19.9125235685369,
-16.0468983949908));
#103752=CARTESIAN_POINT('Ctrl Pts',(-16.7635062156403,19.988201860216,-16.0425061094997));
#103753=CARTESIAN_POINT('Ctrl Pts',(-16.7911181414163,20.0548583904252,
-16.03851835394));
#103754=CARTESIAN_POINT('Ctrl Pts',(-16.8365787807688,20.1504801333401,
-16.0324474626111));
#103755=CARTESIAN_POINT('Ctrl Pts',(-16.8518108267229,20.1806359260491,
-16.0304791075487));
#103756=CARTESIAN_POINT('Ctrl Pts',(-16.8712146971588,20.2168695578073,
-16.028032312617));
#103757=CARTESIAN_POINT('Ctrl Pts',(-16.8747060574799,20.223308591068,-16.0275942967341));
#103758=CARTESIAN_POINT('Ctrl Pts',(-16.8802173408241,20.233348226445,-16.0269061294324));
#103759=CARTESIAN_POINT('Ctrl Pts',(-16.882214539102,20.2369613295415,-16.0266574054815));
#103760=CARTESIAN_POINT('Ctrl Pts',(-16.8859582051346,20.2436873995666,
-16.0261923566797));
#103761=CARTESIAN_POINT('Ctrl Pts',(-16.8877019816805,20.2468017994313,
-16.0259762041059));
#103762=CARTESIAN_POINT('Ctrl Pts',(-16.8916884439503,20.2538796040716,
-16.0254831153073));
#103763=CARTESIAN_POINT('Ctrl Pts',(-16.8939360379762,20.2578401754368,
-16.025205866663));
#103764=CARTESIAN_POINT('Ctrl Pts',(-16.8998091730102,20.2681120982282,
-16.024483415622));
#103765=CARTESIAN_POINT('Ctrl Pts',(-16.9034544805502,20.2744119971818,
-16.0240369841845));
#103766=CARTESIAN_POINT('Ctrl Pts',(-16.9267971713586,20.314277656614,-16.0211913093439));
#103767=CARTESIAN_POINT('Ctrl Pts',(-16.9473832047431,20.3473114176137,
-16.0187400319804));
#103768=CARTESIAN_POINT('Ctrl Pts',(-16.9758135989824,20.3902488851156,
-16.0154472396442));
#103769=CARTESIAN_POINT('Ctrl Pts',(-16.9828542120191,20.4006788522976,
-16.0146387986469));
#103770=CARTESIAN_POINT('Ctrl Pts',(-16.9904245042244,20.4116806759051,
-16.0137773451498));
#103771=CARTESIAN_POINT('Ctrl Pts',(-16.9908620922761,20.4123158742041,
-16.0137275775549));
#103772=CARTESIAN_POINT('Ctrl Pts',(-17.0042646762541,20.4317481854973,
-16.0122041174098));
#103773=CARTESIAN_POINT('Ctrl Pts',(-17.0175322919634,20.4503340862889,
-16.0107199756703));
#103774=CARTESIAN_POINT('Ctrl Pts',(-17.0582311857513,20.505439576628,-16.0062452323129));
#103775=CARTESIAN_POINT('Ctrl Pts',(-17.0865459466897,20.541289400095,-16.0032339605214));
#103776=CARTESIAN_POINT('Ctrl Pts',(-17.1865153883683,20.6597712945726,
-15.9929935655849));
#103777=CARTESIAN_POINT('Ctrl Pts',(-17.263408725544,20.7377650956525,-15.9857629846217));
#103778=CARTESIAN_POINT('Ctrl Pts',(-17.3875659455602,20.8455753095296,
-15.9751939953206));
#103779=CARTESIAN_POINT('Ctrl Pts',(-17.4305385328928,20.8800446754882,
-15.971707194325));
#103780=CARTESIAN_POINT('Ctrl Pts',(-17.5023719664899,20.9331953982135,
-15.9661529096575));
#103781=CARTESIAN_POINT('Ctrl Pts',(-17.5304269993849,20.9529175786369,
-15.9640470438692));
#103782=CARTESIAN_POINT('Ctrl Pts',(-17.5679391532657,20.9779487496927,
-15.9613116042486));
#103783=CARTESIAN_POINT('Ctrl Pts',(-17.5769741492196,20.9838781598675,
-15.9606587123239));
#103784=CARTESIAN_POINT('Ctrl Pts',(-17.591849766667,20.9934784490865,-15.9595933491927));
#103785=CARTESIAN_POINT('Ctrl Pts',(-17.5976635456929,20.9971903709641,
-15.9591793492999));
#103786=CARTESIAN_POINT('Ctrl Pts',(-17.6089545755137,21.004321913216,-15.958379849413));
#103787=CARTESIAN_POINT('Ctrl Pts',(-17.6144295268014,21.0077450148938,
-15.957994223246));
#103788=CARTESIAN_POINT('Ctrl Pts',(-17.627110153192,21.0155928528859,-15.9571057350838));
#103789=CARTESIAN_POINT('Ctrl Pts',(-17.6343268788482,21.019999592989,-15.9566035394799));
#103790=CARTESIAN_POINT('Ctrl Pts',(-17.6538130496318,21.031738709375,-15.955256670784));
#103791=CARTESIAN_POINT('Ctrl Pts',(-17.6661308039446,21.0389903420421,
-15.9544149408887));
#103792=CARTESIAN_POINT('Ctrl Pts',(-17.7800282815023,21.1044991766738,
-15.9467175539741));
#103793=CARTESIAN_POINT('Ctrl Pts',(-17.8862102169174,21.1543627927072,
-15.9401801184914));
#103794=CARTESIAN_POINT('Ctrl Pts',(-18.149351189169,21.2522374261536,-15.9248117443155));
#103795=CARTESIAN_POINT('Ctrl Pts',(-18.3087951046561,21.2913011832654,
-15.9161664957415));
#103796=CARTESIAN_POINT('Ctrl Pts',(-18.50235256656,21.3155234582328,-15.9049531343579));
#103797=CARTESIAN_POINT('Ctrl Pts',(-18.5336629100701,21.3187344072621,
-15.9031160160048));
#103798=CARTESIAN_POINT('Ctrl Pts',(-18.5721758821249,21.3218181655332,
-15.9008152056053));
#103799=CARTESIAN_POINT('Ctrl Pts',(-18.5793232595021,21.3223539437233,
-15.9003864797161));
#103800=CARTESIAN_POINT('Ctrl Pts',(-18.5905569754538,21.3231386929154,
-15.8997097260526));
#103801=CARTESIAN_POINT('Ctrl Pts',(-18.5946416269823,21.3234121289697,
-15.8994630491412));
#103802=CARTESIAN_POINT('Ctrl Pts',(-18.6022940386029,21.3239021074384,
-15.8989997354534));
#103803=CARTESIAN_POINT('Ctrl Pts',(-18.6058615626866,21.3241214626936,
-15.8987832581252));
#103804=CARTESIAN_POINT('Ctrl Pts',(-18.6140274890591,21.3246028033999,
-15.8982866560618));
#103805=CARTESIAN_POINT('Ctrl Pts',(-18.6186261878211,21.3248588165862,
-15.8980062011227));
#103806=CARTESIAN_POINT('Ctrl Pts',(-18.6328371777069,21.3256034424395,
-15.8971371701318));
#103807=CARTESIAN_POINT('Ctrl Pts',(-18.6424518363504,21.3260415033971,
-15.896545874289));
#103808=CARTESIAN_POINT('Ctrl Pts',(-18.7385987729991,21.3297653233294,
-15.8906017610589));
#103809=CARTESIAN_POINT('Ctrl Pts',(-18.8252432442561,21.3278039214104,
-15.8849959527821));
#103810=CARTESIAN_POINT('Ctrl Pts',(-19.0379878403697,21.3099019842061,
-15.8709783137679));
#103811=CARTESIAN_POINT('Ctrl Pts',(-19.1632592867183,21.2879059161919,
-15.8625169320018));
#103812=CARTESIAN_POINT('Ctrl Pts',(-19.3790107608838,21.2296555508022,
-15.8480526990988));
#103813=CARTESIAN_POINT('Ctrl Pts',(-19.4703935014274,21.1981432415498,
-15.8419580184891));
#103814=CARTESIAN_POINT('Ctrl Pts',(-19.5727827760602,21.1547968694471,
-15.8351790868987));
#103815=CARTESIAN_POINT('Ctrl Pts',(-19.5861890623735,21.1489568194085,
-15.8342923275355));
#103816=CARTESIAN_POINT('Ctrl Pts',(-19.6065883425571,21.1398178596174,
-15.8329440589035));
#103817=CARTESIAN_POINT('Ctrl Pts',(-19.6136253611061,21.1366188557751,
-15.8324791452786));
#103818=CARTESIAN_POINT('Ctrl Pts',(-19.6264196539959,21.1307178450611,
-15.8316341617966));
#103819=CARTESIAN_POINT('Ctrl Pts',(-19.632182550925,21.1280283122751,-15.8312536680764));
#103820=CARTESIAN_POINT('Ctrl Pts',(-19.6446241845002,21.1221534068775,
-15.8304324110532));
#103821=CARTESIAN_POINT('Ctrl Pts',(-19.6512985327573,21.1189588973426,
-15.8299919700129));
#103822=CARTESIAN_POINT('Ctrl Pts',(-19.669415281113,21.1101707307961,-15.8287966965718));
#103823=CARTESIAN_POINT('Ctrl Pts',(-19.680824287376,21.1045086459663,-15.8280442518747));
#103824=CARTESIAN_POINT('Ctrl Pts',(-19.7368646365838,21.0760636656641,
-15.8243487489689));
#103825=CARTESIAN_POINT('Ctrl Pts',(-19.7807305047689,21.0518030280639,
-15.8214580571016));
#103826=CARTESIAN_POINT('Ctrl Pts',(-19.9725201961351,20.9366560268146,
-15.8087586900135));
#103827=CARTESIAN_POINT('Ctrl Pts',(-20.1097822015029,20.8293461344433,
-15.7995652052348));
#103828=CARTESIAN_POINT('Ctrl Pts',(-20.2767028284257,20.6620992837642,
-15.7865789601383));
#103829=CARTESIAN_POINT('Ctrl Pts',(-20.3190029595376,20.6157724433836,
-15.7830864700019));
#103830=CARTESIAN_POINT('Ctrl Pts',(-20.3790002882388,20.5438989080495,
-15.7777012142349));
#103831=CARTESIAN_POINT('Ctrl Pts',(-20.3982951617297,20.5197271812692,
-15.7758951897647));
#103832=CARTESIAN_POINT('Ctrl Pts',(-20.4213765010813,20.489475794707,-15.773629017466));
#103833=CARTESIAN_POINT('Ctrl Pts',(-20.4256717671369,20.4837868804455,
-15.7732026023112));
#103834=CARTESIAN_POINT('Ctrl Pts',(-20.4323832435559,20.4748038007864,
-15.772528688803));
#103835=CARTESIAN_POINT('Ctrl Pts',(-20.4348188352532,20.471524088573,-15.7722825225411));
#103836=CARTESIAN_POINT('Ctrl Pts',(-20.4393684431166,20.4653604980719,
-15.7718196309149));
#103837=CARTESIAN_POINT('Ctrl Pts',(-20.4414846510052,20.4624783065653,
-15.7716030617624));
#103838=CARTESIAN_POINT('Ctrl Pts',(-20.4463180504728,20.4558603268095,
-15.7711055340077));
#103839=CARTESIAN_POINT('Ctrl Pts',(-20.4490303153541,20.4521210076871,
-15.7708242405577));
#103840=CARTESIAN_POINT('Ctrl Pts',(-20.4573967032765,20.4405067253994,
-15.7699500730901));
#103841=CARTESIAN_POINT('Ctrl Pts',(-20.4630088935388,20.4326019083675,
-15.7693544335711));
#103842=CARTESIAN_POINT('Ctrl Pts',(-20.5258583159912,20.3427772533996,
-15.762581057254));
#103843=CARTESIAN_POINT('Ctrl Pts',(-20.5772738099576,20.256950713446,-15.7560681325924));
#103844=CARTESIAN_POINT('Ctrl Pts',(-20.6995936298735,20.0155355212111,
-15.7382366497741));
#103845=CARTESIAN_POINT('Ctrl Pts',(-20.7580649026369,19.8544399609954,
-15.7269007947659));
#103846=CARTESIAN_POINT('Ctrl Pts',(-20.8065479238249,19.6448237985732,
-15.7134188741454));
#103847=CARTESIAN_POINT('Ctrl Pts',(-20.8151860530158,19.6012858729815,
-15.7106796434028));
#103848=CARTESIAN_POINT('Ctrl Pts',(-20.8243855575939,19.5458388959596,
-15.7072653515632));
#103849=CARTESIAN_POINT('Ctrl Pts',(-20.8262235205536,19.5341557125939,
-15.7065500432523));
#103850=CARTESIAN_POINT('Ctrl Pts',(-20.8290114867026,19.5154119083165,
-15.7054088837522));
#103851=CARTESIAN_POINT('Ctrl Pts',(-20.8300239034832,19.5083609545634,
-15.7049810632564));
#103852=CARTESIAN_POINT('Ctrl Pts',(-20.8318772340356,19.4949735307227,
-15.7041714885603));
#103853=CARTESIAN_POINT('Ctrl Pts',(-20.8327250735324,19.4886381140026,
-15.7037895194621));
#103854=CARTESIAN_POINT('Ctrl Pts',(-20.8345859303437,19.47423720362,-15.7029238434145));
#103855=CARTESIAN_POINT('Ctrl Pts',(-20.8355812167359,19.4661694895691,
-15.7024407011398));
#103856=CARTESIAN_POINT('Ctrl Pts',(-20.8380346046374,19.4452937228268,
-15.7011951507269));
#103857=CARTESIAN_POINT('Ctrl Pts',(-20.8394222487898,19.4324776091554,
-15.7004349637519));
#103858=CARTESIAN_POINT('Ctrl Pts',(-20.8476032826776,19.3498752888383,
-15.6955629874776));
#103859=CARTESIAN_POINT('Ctrl Pts',(-20.8510436184249,19.2797966553481,
-15.6915583274132));
#103860=CARTESIAN_POINT('Ctrl Pts',(-20.8508787727055,19.0172834305071,
-15.6768593416721));
#103861=CARTESIAN_POINT('Ctrl Pts',(-20.8245352158017,18.8258343963927,
-15.6668250131367));
#103862=CARTESIAN_POINT('Ctrl Pts',(-20.7592947702424,18.5926573079251,
-15.6531662906187));
#103863=CARTESIAN_POINT('Ctrl Pts',(-20.7441979123084,18.5452146740884,
-15.6503027919625));
#103864=CARTESIAN_POINT('Ctrl Pts',(-20.7258385779948,18.4938592559299,
-15.6470652940501));
#103865=CARTESIAN_POINT('Ctrl Pts',(-20.7242171643571,18.4893716987585,
-15.6467812224719));
#103866=CARTESIAN_POINT('Ctrl Pts',(-20.7225806137986,18.4848897174503,
-15.646496294977));
#103867=CARTESIAN_POINT('Origin',(-18.734,19.211,0.));
#103868=CARTESIAN_POINT('',(-20.7225806190038,18.4848897317057,-14.8438386123028));
#103869=CARTESIAN_POINT('',(-20.7193263794245,18.4860708438863,-15.0663814102382));
#103870=CARTESIAN_POINT('',(-20.7225806137986,18.4848897174502,0.));
#103871=CARTESIAN_POINT('',(-20.8523540121835,19.212740575366,-15.110942953294));
#103872=CARTESIAN_POINT('Ctrl Pts',(-20.7193263794245,18.4860708438863,
-15.0663814102382));
#103873=CARTESIAN_POINT('Ctrl Pts',(-20.8041092769325,18.7190474195728,
-15.0812352579235));
#103874=CARTESIAN_POINT('Ctrl Pts',(-20.8501557500904,18.9662442220235,
-15.0960891056087));
#103875=CARTESIAN_POINT('Ctrl Pts',(-20.8523540121835,19.212740575366,-15.110942953294));
#103876=CARTESIAN_POINT('Ctrl Pts',(-20.8509992391722,19.2127948104318,
-15.1101643277519));
#103877=CARTESIAN_POINT('Ctrl Pts',(-20.8509308762891,19.293429605496,-15.1145734088296));
#103878=CARTESIAN_POINT('Ctrl Pts',(-20.8462555791837,19.3739894416571,
-15.1190372239295));
#103879=CARTESIAN_POINT('Ctrl Pts',(-20.8342736513811,19.4776506928941,
-15.125070444969));
#103880=CARTESIAN_POINT('Ctrl Pts',(-20.831153212252,19.5011728849275,-15.1264590656482));
#103881=CARTESIAN_POINT('Ctrl Pts',(-20.8267556721879,19.5305280666389,
-15.128222132077));
#103882=CARTESIAN_POINT('Ctrl Pts',(-20.8258482444011,19.5364157484879,
-15.1285772658009));
#103883=CARTESIAN_POINT('Ctrl Pts',(-20.8242835005995,19.5462912490265,
-15.129175609063));
#103884=CARTESIAN_POINT('Ctrl Pts',(-20.8236395868589,19.5502811974942,
-15.1294180879065));
#103885=CARTESIAN_POINT('Ctrl Pts',(-20.822439937094,19.5575817335751,-15.1298631422263));
#103886=CARTESIAN_POINT('Ctrl Pts',(-20.821887742758,19.5608929010099,-15.1300655186597));
#103887=CARTESIAN_POINT('Ctrl Pts',(-20.8207312363697,19.5677275251417,
-15.1304843497052));
#103888=CARTESIAN_POINT('Ctrl Pts',(-20.8201258792699,19.5712507393469,
-15.130700865115));
#103889=CARTESIAN_POINT('Ctrl Pts',(-20.8187191843601,19.5793153386286,
-15.1311978541401));
#103890=CARTESIAN_POINT('Ctrl Pts',(-20.8179119319051,19.5838556361952,
-15.1314786599025));
#103891=CARTESIAN_POINT('Ctrl Pts',(-20.8153688766512,19.5978924881345,
-15.1323498378207));
#103892=CARTESIAN_POINT('Ctrl Pts',(-20.8135829728089,19.6073796780452,
-15.1329429488265));
#103893=CARTESIAN_POINT('Ctrl Pts',(-20.7944801201428,19.7051749508872,
-15.1390989358417));
#103894=CARTESIAN_POINT('Ctrl Pts',(-20.7716158268014,19.7922961060446,
-15.1449346741224));
#103895=CARTESIAN_POINT('Ctrl Pts',(-20.7285347464531,19.9221351934489,
-15.1539258486894));
#103896=CARTESIAN_POINT('Ctrl Pts',(-20.7123161216645,19.9660810243259,
-15.1570231572921));
#103897=CARTESIAN_POINT('Ctrl Pts',(-20.6795753796455,20.0464781316713,
-15.1627587620049));
#103898=CARTESIAN_POINT('Ctrl Pts',(-20.6634510471132,20.0830699643245,
-15.1653968831636));
#103899=CARTESIAN_POINT('Ctrl Pts',(-20.6009607306979,20.2146515176478,
-15.1749557043506));
#103900=CARTESIAN_POINT('Ctrl Pts',(-20.5485314129769,20.3066001941314,
-15.1817659660048));
#103901=CARTESIAN_POINT('Ctrl Pts',(-20.4701931586325,20.4228204414318,
-15.190478866321));
#103902=CARTESIAN_POINT('Ctrl Pts',(-20.4502456482645,20.45090990002,-15.1925946173668));
#103903=CARTESIAN_POINT('Ctrl Pts',(-20.4231395493703,20.487171523434,-15.1953408209963));
#103904=CARTESIAN_POINT('Ctrl Pts',(-20.4165920234465,20.4957919146388,
-15.195994821804));
#103905=CARTESIAN_POINT('Ctrl Pts',(-20.4057621089003,20.5098256554026,
-15.1970615305458));
#103906=CARTESIAN_POINT('Ctrl Pts',(-20.4015189162918,20.5152688746768,
-15.197475774627));
#103907=CARTESIAN_POINT('Ctrl Pts',(-20.3932555401393,20.5257629913607,
-15.1982754261272));
#103908=CARTESIAN_POINT('Ctrl Pts',(-20.3892387286754,20.5308164355138,
-15.1986609613961));
#103909=CARTESIAN_POINT('Ctrl Pts',(-20.3799132798929,20.5424389988433,
-15.1995487834451));
#103910=CARTESIAN_POINT('Ctrl Pts',(-20.3745882971521,20.5489949084246,
-15.2000504070404));
#103911=CARTESIAN_POINT('Ctrl Pts',(-20.3601678655803,20.5665332554568,
-15.2013947294498));
#103912=CARTESIAN_POINT('Ctrl Pts',(-20.3510003542833,20.5774560742156,
-15.2022345026572));
#103913=CARTESIAN_POINT('Ctrl Pts',(-20.2485615925972,20.6970341414247,
-15.211459206279));
#103914=CARTESIAN_POINT('Ctrl Pts',(-20.1446034879664,20.7960551416562,
-15.2193503669587));
#103915=CARTESIAN_POINT('Ctrl Pts',(-19.9525871115183,20.944980926329,-15.2325685024283));
#103916=CARTESIAN_POINT('Ctrl Pts',(-19.8695239176921,21.0004770268959,
-15.2379407463332));
#103917=CARTESIAN_POINT('Ctrl Pts',(-19.7435196494029,21.0723464026377,
-15.2460221682943));
#103918=CARTESIAN_POINT('Ctrl Pts',(-19.7034698356571,21.0935164202032,
-15.2485825476238));
#103919=CARTESIAN_POINT('Ctrl Pts',(-19.6404725697104,21.1242726983585,
-15.25264384672));
#103920=CARTESIAN_POINT('Ctrl Pts',(-19.6179818126113,21.1347673901187,
-15.2541002780795));
#103921=CARTESIAN_POINT('Ctrl Pts',(-19.5892751475924,21.1475528931052,
-15.2559738092091));
#103922=CARTESIAN_POINT('Ctrl Pts',(-19.5832249218171,21.1502136848249,
-15.2563694856048));
#103923=CARTESIAN_POINT('Ctrl Pts',(-19.5740558157435,21.1541949714397,
-15.2569705007484));
#103924=CARTESIAN_POINT('Ctrl Pts',(-19.5709459972217,21.1555364146649,
-15.2571745797304));
#103925=CARTESIAN_POINT('Ctrl Pts',(-19.5645603854714,21.1582727396786,
-15.2575941419284));
#103926=CARTESIAN_POINT('Ctrl Pts',(-19.5612843186643,21.1596668089167,
-15.257809672999));
#103927=CARTESIAN_POINT('Ctrl Pts',(-19.5539356860413,21.1627720113518,
-15.2582937606435));
#103928=CARTESIAN_POINT('Ctrl Pts',(-19.5498613024546,21.1644786530387,
-15.2585625825862));
#103929=CARTESIAN_POINT('Ctrl Pts',(-19.5394715451773,21.1687924484995,
-15.259249105988));
#103930=CARTESIAN_POINT('Ctrl Pts',(-19.5331488917613,21.1713817810249,
-15.2596678465849));
#103931=CARTESIAN_POINT('Ctrl Pts',(-19.4970328859625,21.1859687097063,
-15.2620647569134));
#103932=CARTESIAN_POINT('Ctrl Pts',(-19.4669837927748,21.1973169663692,
-15.2640783175986));
#103933=CARTESIAN_POINT('Ctrl Pts',(-19.2681647179833,21.2672768294484,
-15.2774734486702));
#103934=CARTESIAN_POINT('Ctrl Pts',(-19.0928126952863,21.3050066048381,
-15.2895530637602));
#103935=CARTESIAN_POINT('Ctrl Pts',(-18.8223031740019,21.328193932115,-15.3071745412507));
#103936=CARTESIAN_POINT('Ctrl Pts',(-18.7293755047119,21.3300304739467,
-15.3130657906812));
#103937=CARTESIAN_POINT('Ctrl Pts',(-18.6155530486077,21.3247889952998,
-15.320062630398));
#103938=CARTESIAN_POINT('Ctrl Pts',(-18.5945049993098,21.3235043886848,
-15.3213476054317));
#103939=CARTESIAN_POINT('Ctrl Pts',(-18.5645469881221,21.3212262721467,
-15.3231644411897));
#103940=CARTESIAN_POINT('Ctrl Pts',(-18.5556192325636,21.3204903528001,
-15.323704344491));
#103941=CARTESIAN_POINT('Ctrl Pts',(-18.5402049144886,21.3191211861481,
-15.3246339506053));
#103942=CARTESIAN_POINT('Ctrl Pts',(-18.5337161622062,21.3185146159511,
-15.3250244863652));
#103943=CARTESIAN_POINT('Ctrl Pts',(-18.5212831731226,21.3172944381121,
-15.3257713111947));
#103944=CARTESIAN_POINT('Ctrl Pts',(-18.5153385403187,21.3166856070259,
-15.3261277465956));
#103945=CARTESIAN_POINT('Ctrl Pts',(-18.4998558430929,21.315033643864,-15.3270544325623));
#103946=CARTESIAN_POINT('Ctrl Pts',(-18.4903220825626,21.3139508168013,
-15.3276234288962));
#103947=CARTESIAN_POINT('Ctrl Pts',(-18.4576767400547,21.310018034307,-15.3295664486316));
#103948=CARTESIAN_POINT('Ctrl Pts',(-18.4346044783592,21.3068515303342,
-15.3309305008786));
#103949=CARTESIAN_POINT('Ctrl Pts',(-18.2424793265693,21.2772462057837,
-15.3422230489624));
#103950=CARTESIAN_POINT('Ctrl Pts',(-18.0771536862297,21.2307835874841,
-15.3514435394357));
#103951=CARTESIAN_POINT('Ctrl Pts',(-17.8360461671051,21.1302412468535,
-15.3656482801688));
#103952=CARTESIAN_POINT('Ctrl Pts',(-17.755186825856,21.0902898235673,-15.3705714861155));
#103953=CARTESIAN_POINT('Ctrl Pts',(-17.6436818181249,21.0260440874248,
-15.3779131172016));
#103954=CARTESIAN_POINT('Ctrl Pts',(-17.6107737720088,21.0058652304271,
-15.3801538389643));
#103955=CARTESIAN_POINT('Ctrl Pts',(-17.5720572298016,20.9806428997978,
-15.3829028032305));
#103956=CARTESIAN_POINT('Ctrl Pts',(-17.56569901276,20.9764517249826,-15.3833579837891));
#103957=CARTESIAN_POINT('Ctrl Pts',(-17.5558763608704,20.9699005832118,
-15.3840672155997));
#103958=CARTESIAN_POINT('Ctrl Pts',(-17.5523960148206,20.9675644287095,
-15.3843196930339));
#103959=CARTESIAN_POINT('Ctrl Pts',(-17.5459702208747,20.9632234272667,
-15.3847880835773));
#103960=CARTESIAN_POINT('Ctrl Pts',(-17.5430228872354,20.9612214749711,
-15.385003801407));
#103961=CARTESIAN_POINT('Ctrl Pts',(-17.5363909910637,20.9566923051825,
-15.3854911788369));
#103962=CARTESIAN_POINT('Ctrl Pts',(-17.5327093894604,20.9541608734829,
-15.3857631212966));
#103963=CARTESIAN_POINT('Ctrl Pts',(-17.5219242170672,20.946694705068,-15.3865637700496));
#103964=CARTESIAN_POINT('Ctrl Pts',(-17.5148429428926,20.9417281349256,
-15.3870945721637));
#103965=CARTESIAN_POINT('Ctrl Pts',(-17.4656337775459,20.906762609763,-15.3908179403918));
#103966=CARTESIAN_POINT('Ctrl Pts',(-17.4245905926597,20.8752745424576,
-15.3941017659741));
#103967=CARTESIAN_POINT('Ctrl Pts',(-17.36792480951,20.8284065797107,-15.3988492516395));
#103968=CARTESIAN_POINT('Ctrl Pts',(-17.3513209985764,20.8142355420827,
-15.4002679591068));
#103969=CARTESIAN_POINT('Ctrl Pts',(-17.2968372836858,20.7662587725617,
-15.4050090025746));
#103970=CARTESIAN_POINT('Ctrl Pts',(-17.2599550183476,20.7313478792839,
-15.4083593014268));
#103971=CARTESIAN_POINT('Ctrl Pts',(-17.1593371371747,20.6290019140577,
-15.4178426493096));
#103972=CARTESIAN_POINT('Ctrl Pts',(-17.0987236173138,20.5586518900657,
-15.4239710749371));
#103973=CARTESIAN_POINT('Ctrl Pts',(-17.0051196442341,20.434359884108,-15.4340313087819));
#103974=CARTESIAN_POINT('Ctrl Pts',(-16.9695724088146,20.382508919724,-15.4380304668877));
#103975=CARTESIAN_POINT('Ctrl Pts',(-16.9232015395132,20.3079597301001,
-15.4435029450439));
#103976=CARTESIAN_POINT('Ctrl Pts',(-16.9103965770584,20.2865381687643,
-15.4450452248955));
#103977=CARTESIAN_POINT('Ctrl Pts',(-16.8886448095702,20.248643640418,-15.4477217150988));
#103978=CARTESIAN_POINT('Ctrl Pts',(-16.8795326393471,20.2322692823418,
-15.4488617409194));
#103979=CARTESIAN_POINT('Ctrl Pts',(-16.8665848612835,20.2082575677118,
-15.4505101004298));
#103980=CARTESIAN_POINT('Ctrl Pts',(-16.86257638092,20.2007149074131,-15.4510245765895));
#103981=CARTESIAN_POINT('Ctrl Pts',(-16.8556225263117,20.1874367020347,
-15.4519245384563));
#103982=CARTESIAN_POINT('Ctrl Pts',(-16.8526575199355,20.1817116157084,
-15.452310715752));
#103983=CARTESIAN_POINT('Ctrl Pts',(-16.8469466664498,20.1705601594194,
-15.4530593626258));
#103984=CARTESIAN_POINT('Ctrl Pts',(-16.8441979596499,20.1651353324785,
-15.4534219301234));
#103985=CARTESIAN_POINT('Ctrl Pts',(-16.8376761363859,20.1521251649403,
-15.4542876228486));
#103986=CARTESIAN_POINT('Ctrl Pts',(-16.8339250828848,20.1445288342177,
-15.45478997313));
#103987=CARTESIAN_POINT('Ctrl Pts',(-16.8205146696674,20.1169554440092,
-15.4566023922238));
#103988=CARTESIAN_POINT('Ctrl Pts',(-16.8111237292017,20.0968489024758,
-15.4579031508943));
#103989=CARTESIAN_POINT('Ctrl Pts',(-16.7265023657435,19.9079803521537,
-15.4699389098787));
#103990=CARTESIAN_POINT('Ctrl Pts',(-16.6733539663025,19.7302035952761,
-15.4798262352747));
#103991=CARTESIAN_POINT('Ctrl Pts',(-16.6311238172708,19.468118820722,-15.4942953529183));
#103992=CARTESIAN_POINT('Ctrl Pts',(-16.6228541218484,19.3878032036988,
-15.4987306268947));
#103993=CARTESIAN_POINT('Ctrl Pts',(-16.6175435583974,19.271081242806,-15.5054131239299));
#103994=CARTESIAN_POINT('Ctrl Pts',(-16.6168260371573,19.2349099032179,
-15.5075170520817));
#103995=CARTESIAN_POINT('Ctrl Pts',(-16.6170787854484,19.1912655893302,
-15.5101143634216));
#103996=CARTESIAN_POINT('Ctrl Pts',(-16.617161662064,19.1837911255862,-15.5105612543756));
#103997=CARTESIAN_POINT('Ctrl Pts',(-16.617352293182,19.1721567113908,-15.5112603173794));
#103998=CARTESIAN_POINT('Ctrl Pts',(-16.6174327329262,19.1679962895193,
-15.5115109870723));
#103999=CARTESIAN_POINT('Ctrl Pts',(-16.6176048767735,19.1602713423011,
-15.5119777441079));
#104000=CARTESIAN_POINT('Ctrl Pts',(-16.6176933203464,19.1567068017264,
-15.5121936471735));
#104001=CARTESIAN_POINT('Ctrl Pts',(-16.6179139712989,19.1486362213743,
-15.5126836657305));
#104002=CARTESIAN_POINT('Ctrl Pts',(-16.6180515657088,19.1441303933021,
-15.5129580778639));
#104003=CARTESIAN_POINT('Ctrl Pts',(-16.6185014370032,19.1307946699384,
-15.5137726427061));
#104004=CARTESIAN_POINT('Ctrl Pts',(-16.6188545976371,19.1219663792137,
-15.5143149995884));
#104005=CARTESIAN_POINT('Ctrl Pts',(-16.6218674308755,19.0568591049924,
-15.5183364794709));
#104006=CARTESIAN_POINT('Ctrl Pts',(-16.626717417804,19.0007089470725,-15.5219238152531));
#104007=CARTESIAN_POINT('Ctrl Pts',(-16.6548174068893,18.7789918878224,
-15.5363951828686));
#104008=CARTESIAN_POINT('Ctrl Pts',(-16.6954012390558,18.6162278000266,
-15.5476444985705));
#104009=CARTESIAN_POINT('Ctrl Pts',(-16.7754762364667,18.4052096757778,
-15.5621909727667));
#104010=CARTESIAN_POINT('Ctrl Pts',(-16.7984984579841,18.3513790770242,
-15.5659051320982));
#104011=CARTESIAN_POINT('Ctrl Pts',(-16.8391656876571,18.2662378032368,
-15.5717775253957));
#104012=CARTESIAN_POINT('Ctrl Pts',(-16.8554267749238,18.2343037504129,
-15.5739798485299));
#104013=CARTESIAN_POINT('Ctrl Pts',(-16.877720624992,18.1931412449418,-15.5768200697672));
#104014=CARTESIAN_POINT('Ctrl Pts',(-16.8830249343894,18.1835269458855,
-15.5774835779558));
#104015=CARTESIAN_POINT('Ctrl Pts',(-16.8918014861631,18.1679076068336,
-15.5785618268884));
#104016=CARTESIAN_POINT('Ctrl Pts',(-16.8952288134719,18.161877685663,-15.5789781682825));
#104017=CARTESIAN_POINT('Ctrl Pts',(-16.901896685097,18.1502795149001,-15.5797791683223));
#104018=CARTESIAN_POINT('Ctrl Pts',(-16.905133130337,18.1447090085468,-15.5801639690235));
#104019=CARTESIAN_POINT('Ctrl Pts',(-16.9126301840842,18.1319397765896,
-15.5810462905161));
#104020=CARTESIAN_POINT('Ctrl Pts',(-16.9169081493606,18.1247513261319,
-15.581543174618));
#104021=CARTESIAN_POINT('Ctrl Pts',(-16.928449973859,18.1056160914496,-15.5828664627004));
#104022=CARTESIAN_POINT('Ctrl Pts',(-16.9357898428663,18.0937154673312,
-15.5836900843806));
#104023=CARTESIAN_POINT('Ctrl Pts',(-16.9968414899234,17.9968885552311,
-15.5903986846492));
#104024=CARTESIAN_POINT('Ctrl Pts',(-17.0564229172238,17.9158069053196,
-15.5960544393299));
#104025=CARTESIAN_POINT('Ctrl Pts',(-17.2326520132677,17.7086535594027,
-15.6110382220004));
#104026=CARTESIAN_POINT('Ctrl Pts',(-17.3591999744398,17.5920485162329,
-15.6200522704073));
#104027=CARTESIAN_POINT('Ctrl Pts',(-17.5308011486323,17.4687046231591,
-15.6320928078035));
#104028=CARTESIAN_POINT('Ctrl Pts',(-17.5638458944849,17.4463415167844,
-15.6344066297458));
#104029=CARTESIAN_POINT('Ctrl Pts',(-17.603984818917,17.4208006346096,-15.6372365700519));
#104030=CARTESIAN_POINT('Ctrl Pts',(-17.6104918134872,17.4167097703938,
-15.6376959303295));
#104031=CARTESIAN_POINT('Ctrl Pts',(-17.6205946336153,17.4104347583439,
-15.6384102861626));
#104032=CARTESIAN_POINT('Ctrl Pts',(-17.6241750129557,17.4082256944421,
-15.6386636713128));
#104033=CARTESIAN_POINT('Ctrl Pts',(-17.6307988481412,17.4041660547059,
-15.6391328976393));
#104034=CARTESIAN_POINT('Ctrl Pts',(-17.6338403990617,17.4023124815941,
-15.6393485380588));
#104035=CARTESIAN_POINT('Ctrl Pts',(-17.6406913639609,17.3981610612338,
-15.6398346599955));
#104036=CARTESIAN_POINT('Ctrl Pts',(-17.6445033266221,17.3958675559601,
-15.6401054177427));
#104037=CARTESIAN_POINT('Ctrl Pts',(-17.6542753583027,17.3900299889312,
-15.6408001508312));
#104038=CARTESIAN_POINT('Ctrl Pts',(-17.6602456092922,17.3865031958119,
-15.6412252074449));
#104039=CARTESIAN_POINT('Ctrl Pts',(-17.6952194998654,17.3660742645413,
-15.6437182468139));
#104040=CARTESIAN_POINT('Ctrl Pts',(-17.7246028171321,17.3498355978042,
-15.6458249132462));
#104041=CARTESIAN_POINT('Ctrl Pts',(-17.7705504057268,17.3258507941892,
-15.6491234501822));
#104042=CARTESIAN_POINT('Ctrl Pts',(-17.7868513488715,17.3176083222549,
-15.6502945011103));
#104043=CARTESIAN_POINT('Ctrl Pts',(-17.8254406850437,17.2987188928704,
-15.6530653765505));
#104044=CARTESIAN_POINT('Ctrl Pts',(-17.847812677376,17.2882490997966,-15.6546707154741));
#104045=CARTESIAN_POINT('Ctrl Pts',(-17.9113738267982,17.2598483010576,
-15.6592195973515));
#104046=CARTESIAN_POINT('Ctrl Pts',(-17.952957538278,17.2428335266386,-15.6621813712387));
#104047=CARTESIAN_POINT('Ctrl Pts',(-18.097516943307,17.1889875012088,-15.6723715840893));
#104048=CARTESIAN_POINT('Ctrl Pts',(-18.2027950029202,17.1588133748115,
-15.6796016161337));
#104049=CARTESIAN_POINT('Ctrl Pts',(-18.3638784493342,17.1258788673889,
-15.690169452627));
#104050=CARTESIAN_POINT('Ctrl Pts',(-18.4182309640556,17.1169582537551,
-15.6936556535534));
#104051=CARTESIAN_POINT('Ctrl Pts',(-18.5068944721206,17.1059376735066,
-15.6992090942802));
#104052=CARTESIAN_POINT('Ctrl Pts',(-18.5410147457956,17.1025358132481,
-15.7013147016574));
#104053=CARTESIAN_POINT('Ctrl Pts',(-18.5859799021831,17.09915345664,-15.7040498598085));
#104054=CARTESIAN_POINT('Ctrl Pts',(-18.5967617721105,17.0984253983241,
-15.7047027226738));
#104055=CARTESIAN_POINT('Ctrl Pts',(-18.6144340885846,17.0973679202973,
-15.7057680505384));
#104056=CARTESIAN_POINT('Ctrl Pts',(-18.6213213088794,17.0969895719652,
-15.7061820440289));
#104057=CARTESIAN_POINT('Ctrl Pts',(-18.6346591959332,17.0963222238912,
-15.7069815399475));
#104058=CARTESIAN_POINT('Ctrl Pts',(-18.6411095693041,17.096029063691,-15.7073671685044));
#104059=CARTESIAN_POINT('Ctrl Pts',(-18.6560100722666,17.0954201567498,
-15.7082556741727));
#104060=CARTESIAN_POINT('Ctrl Pts',(-18.6644609903024,17.0951255161779,
-15.7087578848085));
#104061=CARTESIAN_POINT('Ctrl Pts',(-18.6872016752728,17.0944690558154,
-15.7101048204557));
#104062=CARTESIAN_POINT('Ctrl Pts',(-18.701493872113,17.094201311541,-15.7109466018071));
#104063=CARTESIAN_POINT('Ctrl Pts',(-18.8329520761609,17.0930703659304,
-15.7186481019253));
#104064=CARTESIAN_POINT('Ctrl Pts',(-18.9500047665745,17.1017905072283,
-15.7251891916009));
#104065=CARTESIAN_POINT('Ctrl Pts',(-19.2275947590501,17.1458348607374,
-15.740574114917));
#104066=CARTESIAN_POINT('Ctrl Pts',(-19.385891996478,17.1902161640664,-15.7492315332679));
#104067=CARTESIAN_POINT('Ctrl Pts',(-19.5663317158214,17.2642369783433,
-15.7604463348995));
#104068=CARTESIAN_POINT('Ctrl Pts',(-19.5949289438936,17.2767137056503,
-15.7622678532734));
#104069=CARTESIAN_POINT('Ctrl Pts',(-19.6297251036186,17.2928194474207,
-15.764551288169));
#104070=CARTESIAN_POINT('Ctrl Pts',(-19.6361965560468,17.2958547145226,
-15.7649788602261));
#104071=CARTESIAN_POINT('Ctrl Pts',(-19.6463460677891,17.3006779389942,
-15.7656541957518));
#104072=CARTESIAN_POINT('Ctrl Pts',(-19.6500345982701,17.3024439127191,
-15.7659006177446));
#104073=CARTESIAN_POINT('Ctrl Pts',(-19.6569379755142,17.3057736947616,
-15.7663637201713));
#104074=CARTESIAN_POINT('Ctrl Pts',(-19.6601539858711,17.3073349626055,
-15.7665802427708));
#104075=CARTESIAN_POINT('Ctrl Pts',(-19.667510377405,17.3109293035762,-15.7670773043563));
#104076=CARTESIAN_POINT('Ctrl Pts',(-19.67164806648,17.3129677614361,-15.7673581758534));
#104077=CARTESIAN_POINT('Ctrl Pts',(-19.6824718143487,17.3183441773327,
-15.7680962340777));
#104078=CARTESIAN_POINT('Ctrl Pts',(-19.6891468506394,17.3217040105861,
-15.7685547368358));
#104079=CARTESIAN_POINT('Ctrl Pts',(-19.7338277385277,17.34449112986,-15.7716456005952));
#104080=CARTESIAN_POINT('Ctrl Pts',(-19.7712535947661,17.3650272804875,
-15.7743405593274));
#104081=CARTESIAN_POINT('Ctrl Pts',(-19.8142373262288,17.3903330337849,
-15.7775396770944));
#104082=CARTESIAN_POINT('Ctrl Pts',(-19.8204257247185,17.3940189804479,
-15.7780028388094));
#104083=CARTESIAN_POINT('Ctrl Pts',(-19.9612667857937,17.4788837828544,
-15.7886010872205));
#104084=CARTESIAN_POINT('Ctrl Pts',(-20.0864795944153,17.5747810010984,
-15.7991743407422));
#104085=CARTESIAN_POINT('Ctrl Pts',(-20.2683631241046,17.7493510044569,
-15.8155534689647));
#104086=CARTESIAN_POINT('Ctrl Pts',(-20.3323175753978,17.8195715623013,
-15.8215790948944));
#104087=CARTESIAN_POINT('Ctrl Pts',(-20.4046232446554,17.9105531873314,
-15.828717173166));
#104088=CARTESIAN_POINT('Ctrl Pts',(-20.4176410421793,17.9274514689708,
-15.8300172200694));
#104089=CARTESIAN_POINT('Ctrl Pts',(-20.4357852628147,17.9517554224721,
-15.8318514462579));
#104090=CARTESIAN_POINT('Ctrl Pts',(-20.441122932127,17.959001084153,-15.832393879567));
#104091=CARTESIAN_POINT('Ctrl Pts',(-20.4502504309324,17.9715581794512,
-15.8333264665723));
#104092=CARTESIAN_POINT('Ctrl Pts',(-20.4540621751043,17.9768534594887,
-15.8337174675283));
#104093=CARTESIAN_POINT('Ctrl Pts',(-20.4613129506172,17.9870250924257,
-15.8344642456815));
#104094=CARTESIAN_POINT('Ctrl Pts',(-20.4647559588594,17.991898521149,-15.8348201737037));
#104095=CARTESIAN_POINT('Ctrl Pts',(-20.4736538394492,18.004606757036,-15.8357435117079));
#104096=CARTESIAN_POINT('Ctrl Pts',(-20.4790764406837,18.0124640770974,
-15.8363096855944));
#104097=CARTESIAN_POINT('Ctrl Pts',(-20.497378061547,18.0393705632119,-15.8382327433023));
#104098=CARTESIAN_POINT('Ctrl Pts',(-20.5100000812378,18.0585931718865,
-15.8395799350522));
#104099=CARTESIAN_POINT('Ctrl Pts',(-20.603475270823,18.2061350947592,-15.84972915068));
#104100=CARTESIAN_POINT('Ctrl Pts',(-20.6706038614521,18.342542247002,-15.8579870587477));
#104101=CARTESIAN_POINT('Ctrl Pts',(-20.722580613579,18.4848897168488,-15.866216451952));
#104102=CARTESIAN_POINT('',(-20.8509997481126,19.2099672893213,-14.890777245922));
#104103=CARTESIAN_POINT('Ctrl Pts',(-20.7225806137986,18.4848897174503,
-15.646496294977));
#104104=CARTESIAN_POINT('Ctrl Pts',(-20.7215382221587,18.4820349447569,
-15.6463148120176));
#104105=CARTESIAN_POINT('Ctrl Pts',(-20.7204896894983,18.4791824341809,
-15.6461329818143));
#104106=CARTESIAN_POINT('Ctrl Pts',(-20.7178168245224,18.4719590336516,
-15.6456712648569));
#104107=CARTESIAN_POINT('Ctrl Pts',(-20.7161841991896,18.4675912680562,
-15.6453908991577));
#104108=CARTESIAN_POINT('Ctrl Pts',(-20.7132689666859,18.4598700189149,
-15.6448931238288));
#104109=CARTESIAN_POINT('Ctrl Pts',(-20.7119922426294,18.4565143613628,
-15.644676067746));
#104110=CARTESIAN_POINT('Ctrl Pts',(-20.7092701406456,18.4494141666352,
-15.6442152476536));
#104111=CARTESIAN_POINT('Ctrl Pts',(-20.7078226709235,18.4456705459495,
-15.6439713646552));
#104112=CARTESIAN_POINT('Ctrl Pts',(-20.7038921035767,18.4355901593818,
-15.6433122460093));
#104113=CARTESIAN_POINT('Ctrl Pts',(-20.701389104223,18.4292612774484,-15.6428958412505));
#104114=CARTESIAN_POINT('Ctrl Pts',(-20.6888792566542,18.3980705169074,
-15.6408312811603));
#104115=CARTESIAN_POINT('Ctrl Pts',(-20.6784319270672,18.3733893636911,
-15.639158653442));
#104116=CARTESIAN_POINT('Ctrl Pts',(-20.6469617702776,18.3028068447989,
-15.6342757929205));
#104117=CARTESIAN_POINT('Ctrl Pts',(-20.6247626518491,18.2574521743443,
-15.6310149539161));
#104118=CARTESIAN_POINT('Ctrl Pts',(-20.5384183036578,18.0959373215245,
-15.6190524213131));
#104119=CARTESIAN_POINT('Ctrl Pts',(-20.4650106812556,17.9850737743559,
-15.6101842164035));
#104120=CARTESIAN_POINT('Ctrl Pts',(-20.3168836929744,17.8014515478031,
-15.5948582914854));
#104121=CARTESIAN_POINT('Ctrl Pts',(-20.2462642085409,17.7259376877789,
-15.588317349334));
#104122=CARTESIAN_POINT('Ctrl Pts',(-20.1600892183973,17.6463416523253,
-15.5811566985589));
#104123=CARTESIAN_POINT('Ctrl Pts',(-20.1496786642714,17.6369160955586,
-15.5803038902374));
#104124=CARTESIAN_POINT('Ctrl Pts',(-20.1329049473999,17.6220304532301,
-15.5789489976508));
#104125=CARTESIAN_POINT('Ctrl Pts',(-20.126601939419,17.6165034920371,-15.5784441126503));
#104126=CARTESIAN_POINT('Ctrl Pts',(-20.1153950599303,17.6067935828766,
-15.577553811901));
#104127=CARTESIAN_POINT('Ctrl Pts',(-20.1105046335844,17.6025953446085,
-15.5771677634495));
#104128=CARTESIAN_POINT('Ctrl Pts',(-20.100317799796,17.5939308402806,-15.5763686612151));
#104129=CARTESIAN_POINT('Ctrl Pts',(-20.0950184815007,17.589468103267,-15.5759557553197));
#104130=CARTESIAN_POINT('Ctrl Pts',(-20.0812910591526,17.5780224765368,
-15.5748932788432));
#104131=CARTESIAN_POINT('Ctrl Pts',(-20.0728304717354,17.5710787320826,
-15.574245306069));
#104132=CARTESIAN_POINT('Ctrl Pts',(-20.0366931601273,17.5418863115454,
-15.571506101957));
#104133=CARTESIAN_POINT('Ctrl Pts',(-20.0085118658596,17.5202694787388,
-15.5694402091633));
#104134=CARTESIAN_POINT('Ctrl Pts',(-19.9330683079436,17.4653583460582,
-15.5640774022604));
#104135=CARTESIAN_POINT('Ctrl Pts',(-19.8849623675776,17.4332722515722,
-15.5608244187097));
#104136=CARTESIAN_POINT('Ctrl Pts',(-19.6972064712897,17.3188617762681,
-15.5486249040022));
#104137=CARTESIAN_POINT('Ctrl Pts',(-19.5495977439552,17.2507069971801,
-15.5400738720789));
#104138=CARTESIAN_POINT('Ctrl Pts',(-19.3750770759619,17.1932836901734,
-15.5298129570923));
#104139=CARTESIAN_POINT('Ctrl Pts',(-19.354383064877,17.1868251740805,-15.5285932223095));
#104140=CARTESIAN_POINT('Ctrl Pts',(-19.2933187371631,17.1687916054464,
-15.5249755503349));
#104141=CARTESIAN_POINT('Ctrl Pts',(-19.2527013419445,17.1580993778045,
-15.5225457863281));
#104142=CARTESIAN_POINT('Ctrl Pts',(-19.2045508106125,17.1469442240961,
-15.5196093219412));
#104143=CARTESIAN_POINT('Ctrl Pts',(-19.1972968655522,17.1453039134232,
-15.5191654544914));
#104144=CARTESIAN_POINT('Ctrl Pts',(-19.1855407644069,17.1427105824222,
-15.5184434787778));
#104145=CARTESIAN_POINT('Ctrl Pts',(-19.1810438079709,17.1417339442152,
-15.5181666883292));
#104146=CARTESIAN_POINT('Ctrl Pts',(-19.1730488029286,17.1400248863221,
-15.5176734334068));
#104147=CARTESIAN_POINT('Ctrl Pts',(-19.1695520474956,17.1392866543535,
-15.5174573049624));
#104148=CARTESIAN_POINT('Ctrl Pts',(-19.1620431914255,17.1377212423538,
-15.5169923320035));
#104149=CARTESIAN_POINT('Ctrl Pts',(-19.1580306141694,17.1368968641308,
-15.5167433370069));
#104150=CARTESIAN_POINT('Ctrl Pts',(-19.1469791602293,17.1346597689485,
-15.5160561634185));
#104151=CARTESIAN_POINT('Ctrl Pts',(-19.1399355269112,17.1332712192264,
-15.5156166430582));
#104152=CARTESIAN_POINT('Ctrl Pts',(-19.1018128282342,17.1259571354745,
-15.5132299278544));
#104153=CARTESIAN_POINT('Ctrl Pts',(-19.0706127150178,17.1206934064988,
-15.5112483986433));
#104154=CARTESIAN_POINT('Ctrl Pts',(-18.877547017244,17.0925558083017,-15.4988612161596));
#104155=CARTESIAN_POINT('Ctrl Pts',(-18.7136042464353,17.0877959674838,
-15.4878509710221));
#104156=CARTESIAN_POINT('Ctrl Pts',(-18.4341371774074,17.1120783583669,
-15.4695259829435));
#104157=CARTESIAN_POINT('Ctrl Pts',(-18.3185529945875,17.1318652262092,
-15.4620692347016));
#104158=CARTESIAN_POINT('Ctrl Pts',(-18.1913415431482,17.1646825578858,
-15.4540473729411));
#104159=CARTESIAN_POINT('Ctrl Pts',(-18.1775384202955,17.1683928912456,
-15.4531792045577));
#104160=CARTESIAN_POINT('Ctrl Pts',(-18.1556307474793,17.1745203163682,
-15.4518046499447));
#104161=CARTESIAN_POINT('Ctrl Pts',(-18.1475014623248,17.1768466226335,
-15.4512953340162));
#104162=CARTESIAN_POINT('Ctrl Pts',(-18.1331892988731,17.1810351745544,
-15.4503998915104));
#104163=CARTESIAN_POINT('Ctrl Pts',(-18.1270006352785,17.1828771083103,
-15.4500131085094));
#104164=CARTESIAN_POINT('Ctrl Pts',(-18.1142184279995,17.1867452282034,
-15.4492150519824));
#104165=CARTESIAN_POINT('Ctrl Pts',(-18.1076261587662,17.1887753856502,
-15.4488039136819));
#104166=CARTESIAN_POINT('Ctrl Pts',(-18.0907312353962,17.1940688937844,
-15.4477513239841));
#104167=CARTESIAN_POINT('Ctrl Pts',(-18.0804433536745,17.1973790060356,
-15.4471114131979));
#104168=CARTESIAN_POINT('Ctrl Pts',(-18.0376199732079,17.2115201427185,
-15.4444517005992));
#104169=CARTESIAN_POINT('Ctrl Pts',(-18.0053236262562,17.2230624305338,
-15.4424554060208));
#104170=CARTESIAN_POINT('Ctrl Pts',(-17.9219258269259,17.2551734368749,
-15.4373139603988));
#104171=CARTESIAN_POINT('Ctrl Pts',(-17.8713205594662,17.2769610048102,
-15.4342081455096));
#104172=CARTESIAN_POINT('Ctrl Pts',(-17.7229737688609,17.3478130148979,
-15.4250667778362));
#104173=CARTESIAN_POINT('Ctrl Pts',(-17.6281227471287,17.402498916286,-15.4191799645209));
#104174=CARTESIAN_POINT('Ctrl Pts',(-17.5024497821501,17.4885537432272,
-15.4108875588415));
#104175=CARTESIAN_POINT('Ctrl Pts',(-17.4677286027148,17.5139161467976,
-15.4085376252849));
#104176=CARTESIAN_POINT('Ctrl Pts',(-17.3741844465812,17.5867161333536,
-15.4019757123918));
#104177=CARTESIAN_POINT('Ctrl Pts',(-17.3170972177541,17.6362681650533,
-15.3977069332045));
#104178=CARTESIAN_POINT('Ctrl Pts',(-17.2559602276638,17.6953557283412,
-15.3926678520874));
#104179=CARTESIAN_POINT('Ctrl Pts',(-17.2491784579698,17.7019989703284,
-15.3921019723114));
#104180=CARTESIAN_POINT('Ctrl Pts',(-17.239191448581,17.7119144878543,-15.3912579151437));
#104181=CARTESIAN_POINT('Ctrl Pts',(-17.2359516702604,17.7151520200969,
-15.3909824078313));
#104182=CARTESIAN_POINT('Ctrl Pts',(-17.2302041462665,17.7209329585408,
-15.3904905597153));
#104183=CARTESIAN_POINT('Ctrl Pts',(-17.2276923059737,17.723472222634,-15.3902745476699));
#104184=CARTESIAN_POINT('Ctrl Pts',(-17.2223034774305,17.7289475311138,
-15.3898088209111));
#104185=CARTESIAN_POINT('Ctrl Pts',(-17.2194286529396,17.7318855585587,
-15.3895589504298));
#104186=CARTESIAN_POINT('Ctrl Pts',(-17.2115115029251,17.7400240496662,
-15.3888669454493));
#104187=CARTESIAN_POINT('Ctrl Pts',(-17.2064873394198,17.7452419918485,
-15.3884234384197));
#104188=CARTESIAN_POINT('Ctrl Pts',(-17.1790220933158,17.7740611246418,
-15.3859753558713));
#104189=CARTESIAN_POINT('Ctrl Pts',(-17.1571024501804,17.7981505850561,
-15.3839343700123));
#104190=CARTESIAN_POINT('Ctrl Pts',(-17.0290693836037,17.94554963541,-15.3715277002518));
#104191=CARTESIAN_POINT('Ctrl Pts',(-16.9369043730513,18.0802479167928,
-15.3605726038094));
#104192=CARTESIAN_POINT('Ctrl Pts',(-16.8066265435636,18.3275051615477,
-15.3423172877665));
#104193=CARTESIAN_POINT('Ctrl Pts',(-16.7608184932714,18.4351816475996,
-15.3348771273156));
#104194=CARTESIAN_POINT('Ctrl Pts',(-16.7196357887292,18.5596705857064,
-15.3268707027267));
#104195=CARTESIAN_POINT('Ctrl Pts',(-16.7152852961941,18.5732820827928,
-15.3260027349164));
#104196=CARTESIAN_POINT('Ctrl Pts',(-16.7085806010559,18.5950156361407,
-15.3246284368454));
#104197=CARTESIAN_POINT('Ctrl Pts',(-16.7061367255544,18.6031093671289,
-15.3241191785866));
#104198=CARTESIAN_POINT('Ctrl Pts',(-16.7019120764584,18.6174097708592,
-15.3232238031621));
#104199=CARTESIAN_POINT('Ctrl Pts',(-16.7001111017637,18.6236103165708,
-15.3228370298821));
#104200=CARTESIAN_POINT('Ctrl Pts',(-16.6964447759263,18.6364520974938,
-15.3220389605593));
#104201=CARTESIAN_POINT('Ctrl Pts',(-16.6945834588316,18.6430944121029,
-15.3216277999039));
#104202=CARTESIAN_POINT('Ctrl Pts',(-16.6898890396264,18.6601677113828,
-15.3205750849723));
#104203=CARTESIAN_POINT('Ctrl Pts',(-16.6871032748519,18.6706115918716,
-15.319935072027));
#104204=CARTESIAN_POINT('Ctrl Pts',(-16.6758102279252,18.7142900780257,
-15.3172743666684));
#104205=CARTESIAN_POINT('Ctrl Pts',(-16.6680311460616,18.7477087572289,
-15.3152772038945));
#104206=CARTESIAN_POINT('Ctrl Pts',(-16.6498821954173,18.8352624750939,
-15.3101330168604));
#104207=CARTESIAN_POINT('Ctrl Pts',(-16.6408076226018,18.8896403453458,
-15.3070253837888));
#104208=CARTESIAN_POINT('Ctrl Pts',(-16.6200900076392,19.052789931724,-15.2978808439784));
#104209=CARTESIAN_POINT('Ctrl Pts',(-16.6147400481349,19.1621735582841,
-15.2919926661931));
#104210=CARTESIAN_POINT('Ctrl Pts',(-16.6191737846339,19.3173043946737,
-15.283543238948));
#104211=CARTESIAN_POINT('Ctrl Pts',(-16.6219715227188,19.3630724080842,
-15.2810366307503));
#104212=CARTESIAN_POINT('Ctrl Pts',(-16.6283562011198,19.4311374961686,
-15.2772455466786));
#104213=CARTESIAN_POINT('Ctrl Pts',(-16.6308174730751,19.4535273869175,
-15.2759881540931));
#104214=CARTESIAN_POINT('Ctrl Pts',(-16.6343130939643,19.4812466090109,
-15.2744141699683));
#104215=CARTESIAN_POINT('Ctrl Pts',(-16.635011342242,19.4866173921058,-15.2741083914689));
#104216=CARTESIAN_POINT('Ctrl Pts',(-16.641870248778,19.5378365537514,-15.2711840885424));
#104217=CARTESIAN_POINT('Ctrl Pts',(-16.6495110780611,19.5834704979407,
-15.2685159661971));
#104218=CARTESIAN_POINT('Ctrl Pts',(-16.6601495111548,19.6363136234963,
-15.2653150264971));
#104219=CARTESIAN_POINT('Ctrl Pts',(-16.6617000185425,19.6438051654805,
-15.2648585993042));
#104220=CARTESIAN_POINT('Ctrl Pts',(-16.6642510783471,19.6558029991519,
-15.2641231606477));
#104221=CARTESIAN_POINT('Ctrl Pts',(-16.6652258393206,19.6603147871134,
-15.2638455843075));
#104222=CARTESIAN_POINT('Ctrl Pts',(-16.6669836884761,19.6683241896854,
-15.2633509645767));
#104223=CARTESIAN_POINT('Ctrl Pts',(-16.6677609120144,19.6718230437841,
-15.2631342592713));
#104224=CARTESIAN_POINT('Ctrl Pts',(-16.6694332321476,19.6792620920397,
-15.262672144375));
#104225=CARTESIAN_POINT('Ctrl Pts',(-16.6703307107583,19.6832016410085,
-15.2624266054654));
#104226=CARTESIAN_POINT('Ctrl Pts',(-16.6727972955143,19.6938875508798,
-15.26175842468));
#104227=CARTESIAN_POINT('Ctrl Pts',(-16.674388225969,19.70062875016,-15.2613345590264));
#104228=CARTESIAN_POINT('Ctrl Pts',(-16.6826401178331,19.7348422796405,
-15.2591718208114));
#104229=CARTESIAN_POINT('Ctrl Pts',(-16.6898174407134,19.7621856161581,
-15.2574056543473));
#104230=CARTESIAN_POINT('Ctrl Pts',(-16.7124737584914,19.8419585274427,
-15.2521580326998));
#104231=CARTESIAN_POINT('Ctrl Pts',(-16.7294379277261,19.8939400342096,
-15.2486173147502));
#104232=CARTESIAN_POINT('Ctrl Pts',(-16.7969574938312,20.0765425478217,
-15.2358708234296));
#104233=CARTESIAN_POINT('Ctrl Pts',(-16.8584386647835,20.2027520771617,
-15.2265121793544));
#104234=CARTESIAN_POINT('Ctrl Pts',(-16.9794654213565,20.3990661126379,
-15.2116199811475));
#104235=CARTESIAN_POINT('Ctrl Pts',(-17.0319007420379,20.4730437999755,
-15.2059105313524));
#104236=CARTESIAN_POINT('Ctrl Pts',(-17.0975634218495,20.5541131212728,
-15.1995450771182));
#104237=CARTESIAN_POINT('Ctrl Pts',(-17.106309273107,20.5646988004627,-15.1987114833928));
#104238=CARTESIAN_POINT('Ctrl Pts',(-17.1205006703183,20.5815391861825,
-15.1973812319582));
#104239=CARTESIAN_POINT('Ctrl Pts',(-17.1258809419757,20.587848156486,-15.1968819311436));
#104240=CARTESIAN_POINT('Ctrl Pts',(-17.1354999104626,20.5989941724697,
-15.1959980725814));
#104241=CARTESIAN_POINT('Ctrl Pts',(-17.1397238194306,20.6038437889962,
-15.19561291189));
#104242=CARTESIAN_POINT('Ctrl Pts',(-17.1485707201346,20.6139082518532,
-15.1948123003579));
#104243=CARTESIAN_POINT('Ctrl Pts',(-17.1531975003402,20.6191196765284,
-15.1943970140317));
#104244=CARTESIAN_POINT('Ctrl Pts',(-17.165280276463,20.6325946339432,-15.193321264405));
#104245=CARTESIAN_POINT('Ctrl Pts',(-17.1727759166771,20.6408224515919,
-15.1926624768624));
#104246=CARTESIAN_POINT('Ctrl Pts',(-17.2056123325233,20.6763002495685,
-15.1898128466431));
#104247=CARTESIAN_POINT('Ctrl Pts',(-17.2316051358671,20.7029395445369,
-15.187650012579));
#104248=CARTESIAN_POINT('Ctrl Pts',(-17.3025263697019,20.7718904824002,
-15.1819733226059));
#104249=CARTESIAN_POINT('Ctrl Pts',(-17.3486259695994,20.8129474098401,
-15.1785104452991));
#104250=CARTESIAN_POINT('Ctrl Pts',(-17.5104278068789,20.9448338876838,
-15.166961709866));
#104251=CARTESIAN_POINT('Ctrl Pts',(-17.6337607069408,21.0256016578497,
-15.1591629772735));
#104252=CARTESIAN_POINT('Ctrl Pts',(-17.8274744164432,21.1253993391489,
-15.147064796921));
#104253=CARTESIAN_POINT('Ctrl Pts',(-17.8920713264597,21.1546736852139,
-15.1430467139788));
#104254=CARTESIAN_POINT('Ctrl Pts',(-17.9667282691337,21.1840866584231,
-15.1382899589672));
#104255=CARTESIAN_POINT('Ctrl Pts',(-17.9754722938887,21.187464667627,-15.1377311162406));
#104256=CARTESIAN_POINT('Ctrl Pts',(-17.9884995634204,21.1923982088129,
-15.1368955711384));
#104257=CARTESIAN_POINT('Ctrl Pts',(-17.9927659989993,21.1939982142445,
-15.1366214612221));
#104258=CARTESIAN_POINT('Ctrl Pts',(-18.0003838887938,21.1968270679341,
-15.1361311363564));
#104259=CARTESIAN_POINT('Ctrl Pts',(-18.0037333166834,21.1980612253662,
-15.1359152422406));
#104260=CARTESIAN_POINT('Ctrl Pts',(-18.0109615227773,21.2007038444484,
-15.1354486543612));
#104261=CARTESIAN_POINT('Ctrl Pts',(-18.0148412467138,21.202109418153,-15.1351977989155));
#104262=CARTESIAN_POINT('Ctrl Pts',(-18.0256109851437,21.2059755714557,
-15.1345003473762));
#104263=CARTESIAN_POINT('Ctrl Pts',(-18.0325096063712,21.2084117630383,
-15.1340523437058));
#104264=CARTESIAN_POINT('Ctrl Pts',(-18.0712095170149,21.2218531061725,
-15.1315327162058));
#104265=CARTESIAN_POINT('Ctrl Pts',(-18.1032551577965,21.2321338617533,
-15.1294221817715));
#104266=CARTESIAN_POINT('Ctrl Pts',(-18.2042671095229,21.261904007625,-15.122723616981));
#104267=CARTESIAN_POINT('Ctrl Pts',(-18.2739839520058,21.2786576104987,
-15.118035704664));
#104268=CARTESIAN_POINT('Ctrl Pts',(-18.3777810722535,21.298091207421,-15.1110758457956));
#104269=CARTESIAN_POINT('Ctrl Pts',(-18.4112969631768,21.3035353902479,
-15.1088312050503));
#104270=CARTESIAN_POINT('Ctrl Pts',(-18.6037233048588,21.3300591482202,
-15.0959961469476));
#104271=CARTESIAN_POINT('Ctrl Pts',(-18.7645182794458,21.3338448929013,
-15.0855309903439));
#104272=CARTESIAN_POINT('Ctrl Pts',(-18.9479199692896,21.3172985122424,
-15.0741875086963));
#104273=CARTESIAN_POINT('Ctrl Pts',(-18.971581157919,21.3147610229872,-15.0727341904368));
#104274=CARTESIAN_POINT('Ctrl Pts',(-19.0048009697951,21.3106308079139,
-15.0707072975702));
#104275=CARTESIAN_POINT('Ctrl Pts',(-19.0143984375491,21.3093706574082,
-15.0701233031633));
#104276=CARTESIAN_POINT('Ctrl Pts',(-19.0299217774807,21.3072240328976,
-15.0691812189221));
#104277=CARTESIAN_POINT('Ctrl Pts',(-19.035853039956,21.3063781610729,-15.0688218511279));
#104278=CARTESIAN_POINT('Ctrl Pts',(-19.0482160149348,21.3045614640503,
-15.0680739952793));
#104279=CARTESIAN_POINT('Ctrl Pts',(-19.0546470125605,21.3035861517726,
-15.0676856534539));
#104280=CARTESIAN_POINT('Ctrl Pts',(-19.0698542357747,21.301208104374,-15.0667689114509));
#104281=CARTESIAN_POINT('Ctrl Pts',(-19.078626368772,21.2997797052096,-15.0662413303213));
#104282=CARTESIAN_POINT('Ctrl Pts',(-19.1077750250325,21.294844696358,-15.0644921567071));
#104283=CARTESIAN_POINT('Ctrl Pts',(-19.1281095506223,21.2910947561702,
-15.0632782892737));
#104284=CARTESIAN_POINT('Ctrl Pts',(-19.2361434660464,21.2695308036851,
-15.0568586383729));
#104285=CARTESIAN_POINT('Ctrl Pts',(-19.3227069606713,21.2464665043813,
-15.0518238437803));
#104286=CARTESIAN_POINT('Ctrl Pts',(-19.5301703330354,21.1768404390375,
-15.0397511342009));
#104287=CARTESIAN_POINT('Ctrl Pts',(-19.6487483414779,21.1245437973843,
-15.0328533531562));
#104288=CARTESIAN_POINT('Ctrl Pts',(-19.8334989142043,21.0219432352675,
-15.0211964060819));
#104289=CARTESIAN_POINT('Ctrl Pts',(-19.9028057015225,20.9780040494487,
-15.0165828658396));
#104290=CARTESIAN_POINT('Ctrl Pts',(-19.9771545516593,20.9245773642244,
-15.0111575673033));
#104291=CARTESIAN_POINT('Ctrl Pts',(-19.9848895678032,20.918939080845,-15.0105870717844));
#104292=CARTESIAN_POINT('Ctrl Pts',(-19.9962811381506,20.9105165334373,
-15.0097374358223));
#104293=CARTESIAN_POINT('Ctrl Pts',(-19.9999674132718,20.9077724145501,
-15.0094610169595));
#104294=CARTESIAN_POINT('Ctrl Pts',(-20.0063837373337,20.902963457562,-15.0089772389423));
#104295=CARTESIAN_POINT('Ctrl Pts',(-20.0091177490575,20.9009039743805,
-15.008770255574));
#104296=CARTESIAN_POINT('Ctrl Pts',(-20.0150075412379,20.8964448658886,
-15.0083225160251));
#104297=CARTESIAN_POINT('Ctrl Pts',(-20.0181615319694,20.8940430404099,
-15.0080816086366));
#104298=CARTESIAN_POINT('Ctrl Pts',(-20.0265244494044,20.8876373227478,
-15.0074398345719));
#104299=CARTESIAN_POINT('Ctrl Pts',(-20.0317214665898,20.8836180546893,
-15.0070379060703));
#104300=CARTESIAN_POINT('Ctrl Pts',(-20.0432646057647,20.8746046426172,
-15.0061383884991));
#104301=CARTESIAN_POINT('Ctrl Pts',(-20.0496009979838,20.8695982709328,
-15.0056399955571));
#104302=CARTESIAN_POINT('Ctrl Pts',(-20.0687009852409,20.8543290951319,
-15.0041240226512));
#104303=CARTESIAN_POINT('Ctrl Pts',(-20.081373976043,20.8439545519783,-15.0030995363081));
#104304=CARTESIAN_POINT('Ctrl Pts',(-20.1281089704422,20.8047812675753,
-14.9992554749572));
#104305=CARTESIAN_POINT('Ctrl Pts',(-20.1613768482111,20.7750567053641,
-14.9963865431328));
#104306=CARTESIAN_POINT('Ctrl Pts',(-20.2445526816772,20.6958748397315,
-14.9889148943829));
#104307=CARTESIAN_POINT('Ctrl Pts',(-20.2929831227089,20.6449434280133,
-14.9842691881742));
#104308=CARTESIAN_POINT('Ctrl Pts',(-20.4440854126164,20.4693169760868,
-14.9689598573328));
#104309=CARTESIAN_POINT('Ctrl Pts',(-20.5350536727807,20.3352677094884,
-14.9584150521823));
#104310=CARTESIAN_POINT('Ctrl Pts',(-20.620913479345,20.1711097446328,-14.9470037008193));
#104311=CARTESIAN_POINT('Ctrl Pts',(-20.6315674586002,20.1498775279336,
-14.9455529591341));
#104312=CARTESIAN_POINT('Ctrl Pts',(-20.646054146623,20.1197527168517,-14.9435290278956));
#104313=CARTESIAN_POINT('Ctrl Pts',(-20.6501863570855,20.1110068942963,
-14.9429454590489));
#104314=CARTESIAN_POINT('Ctrl Pts',(-20.6567802224698,20.0967996924775,
-14.9420038768959));
#104315=CARTESIAN_POINT('Ctrl Pts',(-20.6592788587166,20.0913557215352,
-14.9416445882744));
#104316=CARTESIAN_POINT('Ctrl Pts',(-20.6644429061992,20.0799772762732,
-14.940896753786));
#104317=CARTESIAN_POINT('Ctrl Pts',(-20.6671041392669,20.074040965992,-14.9405083547772));
#104318=CARTESIAN_POINT('Ctrl Pts',(-20.6733384837056,20.0599607373865,
-14.9395912218884));
#104319=CARTESIAN_POINT('Ctrl Pts',(-20.6768877434239,20.0518063440148,
-14.9390633090039));
#104320=CARTESIAN_POINT('Ctrl Pts',(-20.6885303668951,20.0245901237712,
-14.9373118791438));
#104321=CARTESIAN_POINT('Ctrl Pts',(-20.6963955738974,20.005431558431,-14.936096115036));
#104322=CARTESIAN_POINT('Ctrl Pts',(-20.7368428455887,19.9026395615762,
-14.9296592930422));
#104323=CARTESIAN_POINT('Ctrl Pts',(-20.7643644939504,19.8171084338586,
-14.9246102958648));
#104324=CARTESIAN_POINT('Ctrl Pts',(-20.8293843562145,19.5600283275059,
-14.9099831155574));
#104325=CARTESIAN_POINT('Ctrl Pts',(-20.8510852885873,19.3853205293609,
-14.9007777448692));
#104326=CARTESIAN_POINT('Ctrl Pts',(-20.8509997481126,19.2099672893213,
-14.890777245922));
#104327=CARTESIAN_POINT('Ctrl Pts',(-20.8509997467292,19.2099644573727,
-14.8907770844143));
#104328=CARTESIAN_POINT('Ctrl Pts',(-20.8509866388053,19.1831674228977,
-14.8892488323634));
#104329=CARTESIAN_POINT('Ctrl Pts',(-20.8504647358832,19.1563740229349,
-14.8877018835943));
#104330=CARTESIAN_POINT('Ctrl Pts',(-20.8488772352135,19.1151184590359,
-14.8852810654424));
#104331=CARTESIAN_POINT('Ctrl Pts',(-20.848171390759,19.1006446878675,-14.8844243778208));
#104332=CARTESIAN_POINT('Ctrl Pts',(-20.8470399811955,19.0814889254113,
-14.8832794438788));
#104333=CARTESIAN_POINT('Ctrl Pts',(-20.846747309812,19.0767990890141,-14.8829982498832));
#104334=CARTESIAN_POINT('Ctrl Pts',(-20.8462061822037,19.0685688227447,
-14.8825031657956));
#104335=CARTESIAN_POINT('Ctrl Pts',(-20.845964430718,19.0650279500911,-14.8822896436915));
#104336=CARTESIAN_POINT('Ctrl Pts',(-20.8454718256797,19.0580703882878,
-14.8818690285064));
#104337=CARTESIAN_POINT('Ctrl Pts',(-20.8452215797105,19.054653660018,-14.8816619690076));
#104338=CARTESIAN_POINT('Ctrl Pts',(-20.8446669325024,19.0473250308869,
-14.8812167390628));
#104339=CARTESIAN_POINT('Ctrl Pts',(-20.8443599503408,19.0434133809311,
-14.8809784276841));
#104340=CARTESIAN_POINT('Ctrl Pts',(-20.8435234722957,19.0331216543962,
-14.8803496960766));
#104341=CARTESIAN_POINT('Ctrl Pts',(-20.842975911369,19.0267431444018,-14.8799582825531));
#104342=CARTESIAN_POINT('Ctrl Pts',(-20.840583202641,19.0002797620154,-14.8783274067943));
#104343=CARTESIAN_POINT('Ctrl Pts',(-20.8384800650701,18.980220028178,-14.8770745123902));
#104344=CARTESIAN_POINT('Ctrl Pts',(-20.8355857356411,18.9559616381952,
-14.8755416340987));
#104345=CARTESIAN_POINT('Ctrl Pts',(-20.8350679505098,18.9517305706445,
-14.87527361885));
#104346=CARTESIAN_POINT('Ctrl Pts',(-20.8313092224031,18.9217670685447,
-14.8733710788059));
#104347=CARTESIAN_POINT('Ctrl Pts',(-20.8276085450745,18.8960955537747,
-14.8717174824157));
#104348=CARTESIAN_POINT('Ctrl Pts',(-20.8020052665551,18.7389842819775,
-14.8614773236772));
#104349=CARTESIAN_POINT('Ctrl Pts',(-20.7682207967035,18.6098833818227,
-14.8525677679027));
#104350=CARTESIAN_POINT('Ctrl Pts',(-20.7225806190038,18.4848897317057,
-14.8438386123028));
#104351=CARTESIAN_POINT('Origin',(-18.734,19.211,0.));
#104352=CARTESIAN_POINT('',(-20.7225806179957,18.4848897289449,-14.042655348398));
#104353=CARTESIAN_POINT('',(-20.7225806137986,18.4848897174502,-14.2664527203653));
#104354=CARTESIAN_POINT('',(-20.7225806137986,18.4848897174502,0.));
#104355=CARTESIAN_POINT('',(-20.8484261613494,19.2114672066158,-14.3109440134323));
#104356=CARTESIAN_POINT('Ctrl Pts',(-20.7225806137986,18.4848897174502,
-14.2664527203653));
#104357=CARTESIAN_POINT('Ctrl Pts',(-20.7483493632785,18.5554619664447,
-14.2709758355722));
#104358=CARTESIAN_POINT('Ctrl Pts',(-20.7703907027832,18.6274990086842,
-14.2754989507791));
#104359=CARTESIAN_POINT('Ctrl Pts',(-20.7885479544131,18.7005867331105,
-14.280022065986));
#104360=CARTESIAN_POINT('Ctrl Pts',(-20.8066819175929,18.7735807153857,
-14.2845393798555));
#104361=CARTESIAN_POINT('Ctrl Pts',(-20.8209415894746,18.8476222797955,
-14.289056693725));
#104362=CARTESIAN_POINT('Ctrl Pts',(-20.8312196705739,18.9222810131672,
-14.2935740075945));
#104363=CARTESIAN_POINT('Ctrl Pts',(-20.8414842530404,18.9968416941083,
-14.2980853886872));
#104364=CARTESIAN_POINT('Ctrl Pts',(-20.8477775921481,19.0720174996117,
-14.3025967697798));
#104365=CARTESIAN_POINT('Ctrl Pts',(-20.8500434728548,19.1473680819993,
-14.3071081508725));
#104366=CARTESIAN_POINT('Ctrl Pts',(-20.8506856224259,19.1687224030869,
-14.3083866742408));
#104367=CARTESIAN_POINT('Ctrl Pts',(-20.8510046224853,19.1900907116534,
-14.3096651976092));
#104368=CARTESIAN_POINT('Ctrl Pts',(-20.850999949394,19.2114628884564,-14.3109437209775));
#104369=CARTESIAN_POINT('Ctrl Pts',(-20.8476071148151,19.2114685807669,
-14.310944106499));
#104370=CARTESIAN_POINT('Ctrl Pts',(-20.8482399645881,19.5369557946072,
-14.3304466040373));
#104371=CARTESIAN_POINT('Ctrl Pts',(-20.6243347143573,20.5691167586125,
-14.3923410371361));
#104372=CARTESIAN_POINT('Ctrl Pts',(-19.0148744787981,21.6984565315257,
-14.4966274057954));
#104373=CARTESIAN_POINT('Ctrl Pts',(-16.7944747336858,20.7935840294886,
-14.6238032124768));
#104374=CARTESIAN_POINT('Ctrl Pts',(-16.3534690399024,18.4367889066407,
-14.7509790191583));
#104375=CARTESIAN_POINT('Ctrl Pts',(-18.0964527495932,16.7902844089888,
-14.8781548258396));
#104376=CARTESIAN_POINT('Ctrl Pts',(-20.0208839008303,17.2650915259889,
-14.9832889561996));
#104377=CARTESIAN_POINT('Ctrl Pts',(-20.6031710249408,18.1668852825214,
-15.0460311509992));
#104378=CARTESIAN_POINT('Ctrl Pts',(-20.7193263794245,18.4860708438863,
-15.0663814102382));
#104379=CARTESIAN_POINT('Ctrl Pts',(-20.7225806190038,18.4848897317057,
-14.8438386123028));
#104380=CARTESIAN_POINT('Ctrl Pts',(-20.7074810939562,18.4435370278851,
-14.8409506721092));
#104381=CARTESIAN_POINT('Ctrl Pts',(-20.6910839087439,18.4026340477406,
-14.8380800866817));
#104382=CARTESIAN_POINT('Ctrl Pts',(-20.6498725442178,18.3084662526309,
-14.8314542563252));
#104383=CARTESIAN_POINT('Ctrl Pts',(-20.6241100173458,18.2556885989155,
-14.8277280609254));
#104384=CARTESIAN_POINT('Ctrl Pts',(-20.5791049394694,18.1724595813546,
-14.8218389175388));
#104385=CARTESIAN_POINT('Ctrl Pts',(-20.5612232428029,18.1413113033745,
-14.8196315672646));
#104386=CARTESIAN_POINT('Ctrl Pts',(-20.5368450703277,18.1012435357112,
-14.816785900081));
#104387=CARTESIAN_POINT('Ctrl Pts',(-20.5310601569201,18.0919001129576,
-14.8161218507982));
#104388=CARTESIAN_POINT('Ctrl Pts',(-20.5215047349287,18.0767319740383,
-14.8150429449288));
#104389=CARTESIAN_POINT('Ctrl Pts',(-20.5177779362274,18.0708800904631,
-14.8146264839918));
#104390=CARTESIAN_POINT('Ctrl Pts',(-20.5105354664624,18.0596302803133,
-14.8138254046825));
#104391=CARTESIAN_POINT('Ctrl Pts',(-20.5070237974983,18.0542298802567,
-14.8134406434552));
#104392=CARTESIAN_POINT('Ctrl Pts',(-20.4988979148387,18.0418574733217,
-14.8125586240517));
#104393=CARTESIAN_POINT('Ctrl Pts',(-20.494266920987,18.0348965745188,-14.8120620011086));
#104394=CARTESIAN_POINT('Ctrl Pts',(-20.481790053944,18.0163812394956,-14.8107398688276));
#104395=CARTESIAN_POINT('Ctrl Pts',(-20.4738707904637,18.0048765809252,
-14.8099171340184));
#104396=CARTESIAN_POINT('Ctrl Pts',(-20.4096460920631,17.9135235647273,
-14.8033723417588));
#104397=CARTESIAN_POINT('Ctrl Pts',(-20.3479848091841,17.8375767418352,
-14.7978661273312));
#104398=CARTESIAN_POINT('Ctrl Pts',(-20.1877542516837,17.665985351725,-14.7849162800294));
#104399=CARTESIAN_POINT('Ctrl Pts',(-20.0847171457458,17.5751416781252,
-14.7776254632276));
#104400=CARTESIAN_POINT('Ctrl Pts',(-19.9319513590194,17.4647913235688,
-14.7671839048302));
#104401=CARTESIAN_POINT('Ctrl Pts',(-19.8891950784322,17.4362166838002,
-14.7642935827439));
#104402=CARTESIAN_POINT('Ctrl Pts',(-19.8301035963785,17.3997653948343,
-14.7602823390455));
#104403=CARTESIAN_POINT('Ctrl Pts',(-19.8146431415058,17.390498902606,-14.7592313479842));
#104404=CARTESIAN_POINT('Ctrl Pts',(-19.7915920186869,17.3770799012701,
-14.757659271722));
#104405=CARTESIAN_POINT('Ctrl Pts',(-19.7840907938231,17.3727744627639,
-14.7571469071607));
#104406=CARTESIAN_POINT('Ctrl Pts',(-19.7704624556153,17.3650629156234,
-14.7562142311961));
#104407=CARTESIAN_POINT('Ctrl Pts',(-19.764344362987,17.3616410213517,-14.7557948778035));
#104408=CARTESIAN_POINT('Ctrl Pts',(-19.7546790594241,17.3562979941646,
-14.7551311818541));
#104409=CARTESIAN_POINT('Ctrl Pts',(-19.7511430959116,17.3543564707753,
-14.754888122013));
#104410=CARTESIAN_POINT('Ctrl Pts',(-19.7475925566865,17.3524201310848,
-14.7546437854131));
#104411=CARTESIAN_POINT('Ctrl Pts',(-19.7475834744231,17.352415178023,-14.7546431603994));
#104412=CARTESIAN_POINT('Ctrl Pts',(-19.7475652544736,17.3524052418474,
-14.7546419065543));
#104413=CARTESIAN_POINT('Ctrl Pts',(-19.7475561170615,17.3524002588843,
-14.7546412777418));
#104414=CARTESIAN_POINT('Ctrl Pts',(-19.7475377863691,17.3523902626663,
-14.7546400162684));
#104415=CARTESIAN_POINT('Ctrl Pts',(-19.747528593265,17.3523852495087,-14.7546393836196));
#104416=CARTESIAN_POINT('Ctrl Pts',(-19.7475101508872,17.3523751927407,
-14.7546381144528));
#104417=CARTESIAN_POINT('Ctrl Pts',(-19.747500901695,17.3523701491759,-14.7546374779405));
#104418=CARTESIAN_POINT('Ctrl Pts',(-19.7474823468813,17.3523600314552,
-14.7546362010287));
#104419=CARTESIAN_POINT('Ctrl Pts',(-19.7474730411775,17.3523549572555,
-14.7546355606235));
#104420=CARTESIAN_POINT('Ctrl Pts',(-19.7474543727597,17.3523447779515,
-14.754634275886));
#104421=CARTESIAN_POINT('Ctrl Pts',(-19.7474450103116,17.3523396729934,
-14.754633631572));
#104422=CARTESIAN_POINT('Ctrl Pts',(-19.7474262281966,17.3523294320622,
-14.7546323390023));
#104423=CARTESIAN_POINT('Ctrl Pts',(-19.7474168083247,17.3523242959784,
-14.7546316907326));
#104424=CARTESIAN_POINT('Ctrl Pts',(-19.7473979109353,17.3523139925667,
-14.7546303902221));
#104425=CARTESIAN_POINT('Ctrl Pts',(-19.7473884334741,17.3523088252705,
-14.7546297379852));
#104426=CARTESIAN_POINT('Ctrl Pts',(-19.7473694205619,17.3522984592496,
-14.7546284295165));
#104427=CARTESIAN_POINT('Ctrl Pts',(-19.7473598849335,17.3522932604293,
-14.7546277732726));
#104428=CARTESIAN_POINT('Ctrl Pts',(-19.7473407551873,17.3522828310914,
-14.7546264567555));
#104429=CARTESIAN_POINT('Ctrl Pts',(-19.7473311611348,17.3522776006104,
-14.7546257964868));
#104430=CARTESIAN_POINT('Ctrl Pts',(-19.7473119141314,17.3522671077316,
-14.7546244718919));
#104431=CARTESIAN_POINT('Ctrl Pts',(-19.7473022611091,17.3522618452961,
-14.7546238075608));
#104432=CARTESIAN_POINT('Ctrl Pts',(-19.747282895701,17.3522512882581,-14.754622474809));
#104433=CARTESIAN_POINT('Ctrl Pts',(-19.7472731833765,17.3522459936903,
-14.7546218063925));
#104434=CARTESIAN_POINT('Ctrl Pts',(-19.7472537367182,17.3522353927542,
-14.7546204680408));
#104435=CARTESIAN_POINT('Ctrl Pts',(-19.7472439456494,17.3522300554586,
-14.7546197942006));
#104436=CARTESIAN_POINT('Ctrl Pts',(-19.7472243210675,17.3522193579327,
-14.7546184435955));
#104437=CARTESIAN_POINT('Ctrl Pts',(-19.7472144893949,17.3522139987059,
-14.7546177669569));
#104438=CARTESIAN_POINT('Ctrl Pts',(-19.7471947638124,17.3522032465298,
-14.7546164093922));
#104439=CARTESIAN_POINT('Ctrl Pts',(-19.7471848713441,17.3521978543676,
-14.7546157285652));
#104440=CARTESIAN_POINT('Ctrl Pts',(-19.7471650238516,17.3521870361508,
-14.7546143626018));
#104441=CARTESIAN_POINT('Ctrl Pts',(-19.7471550703389,17.3521816109215,
-14.7546136775693));
#104442=CARTESIAN_POINT('Ctrl Pts',(-19.7471350678491,17.3521707086376,
-14.7546123009297));
#104443=CARTESIAN_POINT('Ctrl Pts',(-19.7471250690313,17.3521652589243,
-14.754611612775));
#104444=CARTESIAN_POINT('Ctrl Pts',(-19.7441124399662,17.3505232996412,
-14.7544042720479));
#104445=CARTESIAN_POINT('Ctrl Pts',(-19.7411059130456,17.3488941025673,
-14.7541971504298));
#104446=CARTESIAN_POINT('Ctrl Pts',(-19.7340553278126,17.345095553937,-14.7537109715613));
#104447=CARTESIAN_POINT('Ctrl Pts',(-19.7300081664629,17.3429320697717,
-14.7534315464017));
#104448=CARTESIAN_POINT('Ctrl Pts',(-19.7175267213398,17.3363119759748,
-14.7525687997221));
#104449=CARTESIAN_POINT('Ctrl Pts',(-19.7090694601547,17.3318992738382,
-14.7519828138157));
#104450=CARTESIAN_POINT('Ctrl Pts',(-19.5956003752683,17.2736673480883,
-14.7441050453644));
#104451=CARTESIAN_POINT('Ctrl Pts',(-19.4863089443862,17.2286686009833,
-14.7363487722729));
#104452=CARTESIAN_POINT('Ctrl Pts',(-19.2694538392336,17.1599092270964,
-14.721321551487));
#104453=CARTESIAN_POINT('Ctrl Pts',(-19.1626341486267,17.1349555878662,
-14.7140786555689));
#104454=CARTESIAN_POINT('Ctrl Pts',(-18.9793306433264,17.1068938237246,
-14.7021574895197));
#104455=CARTESIAN_POINT('Ctrl Pts',(-18.9037343106975,17.0994502355644,
-14.6973801126354));
#104456=CARTESIAN_POINT('Ctrl Pts',(-18.8089876374995,17.0952438713994,
-14.6915694461902));
#104457=CARTESIAN_POINT('Ctrl Pts',(-18.7900707676563,17.0946580505478,
-14.6904178947741));
#104458=CARTESIAN_POINT('Ctrl Pts',(-18.7625736042103,17.0941754693399,
-14.6887560549823));
#104459=CARTESIAN_POINT('Ctrl Pts',(-18.7539981860228,17.0940770868078,
-14.6882394819095));
#104460=CARTESIAN_POINT('Ctrl Pts',(-18.7389698607122,17.0939960000606,
-14.6873371006462));
#104461=CARTESIAN_POINT('Ctrl Pts',(-18.7325172344247,17.0939906853981,
-14.6869505893649));
#104462=CARTESIAN_POINT('Ctrl Pts',(-18.7199933870443,17.0940376301673,
-14.6862021993523));
#104463=CARTESIAN_POINT('Ctrl Pts',(-18.7139222233543,17.0940865051778,
-14.6858402184515));
#104464=CARTESIAN_POINT('Ctrl Pts',(-18.6994183944424,17.0942656667909,
-14.6849773628794));
#104465=CARTESIAN_POINT('Ctrl Pts',(-18.6909860909016,17.0944202279193,
-14.6844772515407));
#104466=CARTESIAN_POINT('Ctrl Pts',(-18.6606154304775,17.0951584825035,
-14.6826813631511));
#104467=CARTESIAN_POINT('Ctrl Pts',(-18.6386850642242,17.09603292263,-14.68139467265));
#104468=CARTESIAN_POINT('Ctrl Pts',(-18.4298946557656,17.1076124082181,
-14.6692307348517));
#104469=CARTESIAN_POINT('Ctrl Pts',(-18.245223051317,17.1427102761129,-14.6592274597903));
#104470=CARTESIAN_POINT('Ctrl Pts',(-17.9924737538082,17.2265388712724,
-14.6447059452045));
#104471=CARTESIAN_POINT('Ctrl Pts',(-17.9188479796461,17.2556298614884,
-14.6403524532702));
#104472=CARTESIAN_POINT('Ctrl Pts',(-17.8145678378771,17.3037476375967,
-14.6337811992519));
#104473=CARTESIAN_POINT('Ctrl Pts',(-17.7824935359329,17.3195449562838,
-14.6317013004945));
#104474=CARTESIAN_POINT('Ctrl Pts',(-17.7442395922749,17.3396051122237,
-14.6291306492335));
#104475=CARTESIAN_POINT('Ctrl Pts',(-17.7376608529344,17.3430993626594,
-14.6286852813754));
#104476=CARTESIAN_POINT('Ctrl Pts',(-17.7274410974989,17.3485968629561,
-14.6279880876208));
#104477=CARTESIAN_POINT('Ctrl Pts',(-17.7237872320985,17.350576276231,-14.6277377511103));
#104478=CARTESIAN_POINT('Ctrl Pts',(-17.7170085455672,17.3542743605943,
-14.6272712903984));
#104479=CARTESIAN_POINT('Ctrl Pts',(-17.7138822307273,17.3559901739827,
-14.6270553484315));
#104480=CARTESIAN_POINT('Ctrl Pts',(-17.7068071634323,17.3598964731108,
-14.6265648215043));
#104481=CARTESIAN_POINT('Ctrl Pts',(-17.7028610945467,17.3620916876317,
-14.6262899372727));
#104482=CARTESIAN_POINT('Ctrl Pts',(-17.6926827798906,17.3677966453459,
-14.6255776181735));
#104483=CARTESIAN_POINT('Ctrl Pts',(-17.686461302725,17.371325345643,-14.6251390092721));
#104484=CARTESIAN_POINT('Ctrl Pts',(-17.6481989292703,17.3932840369426,
-14.622422289333));
#104485=CARTESIAN_POINT('Ctrl Pts',(-17.6166294671786,17.4125178627682,
-14.6200972369997));
#104486=CARTESIAN_POINT('Ctrl Pts',(-17.4423708657676,17.5250448420197,
-14.6068559426971));
#104487=CARTESIAN_POINT('Ctrl Pts',(-17.3108550832063,17.6344809421486,
-14.5953532433733));
#104488=CARTESIAN_POINT('Ctrl Pts',(-17.1286102227943,17.8277199462038,
-14.578093569771));
#104489=CARTESIAN_POINT('Ctrl Pts',(-17.0680690264989,17.9012602334922,
-14.5720497573367));
#104490=CARTESIAN_POINT('Ctrl Pts',(-17.0002387241461,17.9960032205012,
-14.5648925934082));
#104491=CARTESIAN_POINT('Ctrl Pts',(-16.988066558422,18.0135603122002,-14.5635905223771));
#104492=CARTESIAN_POINT('Ctrl Pts',(-16.9711439254845,18.0387762385067,
-14.5617539624484));
#104493=CARTESIAN_POINT('Ctrl Pts',(-16.9661736864758,18.0462853501422,
-14.5612111909313));
#104494=CARTESIAN_POINT('Ctrl Pts',(-16.9576845789646,18.059290355027,-14.5602782050805));
#104495=CARTESIAN_POINT('Ctrl Pts',(-16.9541429611953,18.0647711815569,
-14.5598871415699));
#104496=CARTESIAN_POINT('Ctrl Pts',(-16.9474121127944,18.0752939150927,
-14.5591403680547));
#104497=CARTESIAN_POINT('Ctrl Pts',(-16.9442187474406,18.0803330909973,
-14.5587845066282));
#104498=CARTESIAN_POINT('Ctrl Pts',(-16.9359741214643,18.0934656798873,
-14.5578616095128));
#104499=CARTESIAN_POINT('Ctrl Pts',(-16.9309561569804,18.1015799167171,
-14.5572958075361));
#104500=CARTESIAN_POINT('Ctrl Pts',(-16.9140516762329,18.1293327463225,
-14.555375388746));
#104501=CARTESIAN_POINT('Ctrl Pts',(-16.9024295377536,18.1491310573651,
-14.5540304273604));
#104502=CARTESIAN_POINT('Ctrl Pts',(-16.8045313749223,18.3222916902474,
-14.5424711530142));
#104503=CARTESIAN_POINT('Ctrl Pts',(-16.7373660541129,18.4856647684759,
-14.5330125310625));
#104504=CARTESIAN_POINT('Ctrl Pts',(-16.6684448818761,18.7391079634928,
-14.5187205459973));
#104505=CARTESIAN_POINT('Ctrl Pts',(-16.6508614700646,18.8240484142426,
-14.5139749289586));
#104506=CARTESIAN_POINT('Ctrl Pts',(-16.633164796856,18.9471732202117,-14.5068723156672));
#104507=CARTESIAN_POINT('Ctrl Pts',(-16.628796097937,18.984661195206,-14.5046801066245));
#104508=CARTESIAN_POINT('Ctrl Pts',(-16.6247571231889,19.029779848697,-14.5019849044099));
#104509=CARTESIAN_POINT('Ctrl Pts',(-16.6241228721184,19.0373199552581,
-14.5015325916766));
#104510=CARTESIAN_POINT('Ctrl Pts',(-16.6232009377204,19.0490314809562,
-14.5008268768696));
#104511=CARTESIAN_POINT('Ctrl Pts',(-16.6228851602042,19.0532007129879,
-14.5005750237261));
#104512=CARTESIAN_POINT('Ctrl Pts',(-16.6223231110824,19.0609252918407,
-14.5001072020833));
#104513=CARTESIAN_POINT('Ctrl Pts',(-16.6220734651768,19.0644803352983,
-14.4998914250786));
#104514=CARTESIAN_POINT('Ctrl Pts',(-16.6215301551055,19.0725072628519,
-14.4994031572928));
#104515=CARTESIAN_POINT('Ctrl Pts',(-16.6212417150351,19.076979433336,-14.4991303789823));
#104516=CARTESIAN_POINT('Ctrl Pts',(-16.6204343472392,19.0901482987605,
-14.4983250329178));
#104517=CARTESIAN_POINT('Ctrl Pts',(-16.6199549094181,19.0988471970192,
-14.4977903330675));
#104518=CARTESIAN_POINT('Ctrl Pts',(-16.6169286455891,19.1607018320226,
-14.4939701668306));
#104519=CARTESIAN_POINT('Ctrl Pts',(-16.6163334980486,19.2139295643992,
-14.4905880962561));
#104520=CARTESIAN_POINT('Ctrl Pts',(-16.6182286927023,19.2853989561472,
-14.485967869652));
#104521=CARTESIAN_POINT('Ctrl Pts',(-16.6189503069181,19.3036725319898,
-14.4847795540402));
#104522=CARTESIAN_POINT('Ctrl Pts',(-16.6224232250216,19.3698565795093,
-14.4804550299526));
#104523=CARTESIAN_POINT('Ctrl Pts',(-16.626566576587,19.4176785584734,-14.4772914046414));
#104524=CARTESIAN_POINT('Ctrl Pts',(-16.6454707351015,19.5739019566192,
-14.4668964299862));
#104525=CARTESIAN_POINT('Ctrl Pts',(-16.667006818079,19.6813136955979,-14.4596640531949));
#104526=CARTESIAN_POINT('Ctrl Pts',(-16.7117288233571,19.8396045538036,
-14.449091291971));
#104527=CARTESIAN_POINT('Ctrl Pts',(-16.7287731956925,19.8920217918751,
-14.4456025274249));
#104528=CARTESIAN_POINT('Ctrl Pts',(-16.7597164155145,19.975898593138,-14.4400454813959));
#104529=CARTESIAN_POINT('Ctrl Pts',(-16.7723690934829,20.0077872568148,
-14.4379387701988));
#104530=CARTESIAN_POINT('Ctrl Pts',(-16.7900208109303,20.0493022893744,
-14.435202409783));
#104531=CARTESIAN_POINT('Ctrl Pts',(-16.7943260709846,20.0592162883305,
-14.4345494228329));
#104532=CARTESIAN_POINT('Ctrl Pts',(-16.8015031187555,20.0754029070089,
-14.4334839443931));
#104533=CARTESIAN_POINT('Ctrl Pts',(-16.8043299359631,20.0816951403201,
-14.4330699235782));
#104534=CARTESIAN_POINT('Ctrl Pts',(-16.809862216762,20.0938502029877,-14.432270410746));
#104535=CARTESIAN_POINT('Ctrl Pts',(-16.8125638443236,20.0997146847468,
-14.431884792412));
#104536=CARTESIAN_POINT('Ctrl Pts',(-16.8188649676653,20.1132296223118,
-14.430996361538));
#104537=CARTESIAN_POINT('Ctrl Pts',(-16.8224835642167,20.1208710910598,
-14.4304942151134));
#104538=CARTESIAN_POINT('Ctrl Pts',(-16.8323411847198,20.1413692616423,
-14.4291475654056));
#104539=CARTESIAN_POINT('Ctrl Pts',(-16.8386648370025,20.1541849487556,
-14.4283060038041));
#104540=CARTESIAN_POINT('Ctrl Pts',(-16.8978932610095,20.2712173931745,
-14.4206218509398));
#104541=CARTESIAN_POINT('Ctrl Pts',(-16.9592165448794,20.3709559613255,
-14.4140961722568));
#104542=CARTESIAN_POINT('Ctrl Pts',(-17.1249750309179,20.5963756919772,
-14.3987786755774));
#104543=CARTESIAN_POINT('Ctrl Pts',(-17.2362957730824,20.7160240140932,
-14.3901704072727));
#104544=CARTESIAN_POINT('Ctrl Pts',(-17.3848033511061,20.8426868177589,
-14.3789607229529));
#104545=CARTESIAN_POINT('Ctrl Pts',(-17.4098681336797,20.8630920108258,
-14.3770754920012));
#104546=CARTESIAN_POINT('Ctrl Pts',(-17.4410957648968,20.8873471783227,
-14.374721124771));
#104547=CARTESIAN_POINT('Ctrl Pts',(-17.4468255676913,20.891750784859,-14.3742889082093));
#104548=CARTESIAN_POINT('Ctrl Pts',(-17.4558467345305,20.8986107655607,
-14.3736078649816));
#104549=CARTESIAN_POINT('Ctrl Pts',(-17.4591229535437,20.9010870929708,
-14.3733604177488));
#104550=CARTESIAN_POINT('Ctrl Pts',(-17.4652624476059,20.9056996149459,
-14.3728964590385));
#104551=CARTESIAN_POINT('Ctrl Pts',(-17.4681239311548,20.9078381005326,
-14.3726801118633));
#104552=CARTESIAN_POINT('Ctrl Pts',(-17.4746711169923,20.9127052607457,
-14.3721848680646));
#104553=CARTESIAN_POINT('Ctrl Pts',(-17.4783602689436,20.9154291991472,
-14.3719056480819));
#104554=CARTESIAN_POINT('Ctrl Pts',(-17.4897370124984,20.9237723998262,
-14.3710441503994));
#104555=CARTESIAN_POINT('Ctrl Pts',(-17.497453566851,20.9293517063032,-14.3704592192566));
#104556=CARTESIAN_POINT('Ctrl Pts',(-17.6027126014085,21.004381077153,-14.3624752158412));
#104557=CARTESIAN_POINT('Ctrl Pts',(-17.7059278904727,21.0654778131456,
-14.3545981896885));
#104558=CARTESIAN_POINT('Ctrl Pts',(-17.9118352095968,21.1648677277371,
-14.3394934700293));
#104559=CARTESIAN_POINT('Ctrl Pts',(-18.0134478427727,21.2045802231746,
-14.3322936454142));
#104560=CARTESIAN_POINT('Ctrl Pts',(-18.1893948081644,21.2581235480728,
-14.3204773940205));
#104561=CARTESIAN_POINT('Ctrl Pts',(-18.2622328660778,21.2761265211801,
-14.315760705147));
#104562=CARTESIAN_POINT('Ctrl Pts',(-18.3543438138816,21.2937634493328,
-14.3100154945869));
#104563=CARTESIAN_POINT('Ctrl Pts',(-18.3728541999036,21.2970527683627,
-14.3088716863477));
#104564=CARTESIAN_POINT('Ctrl Pts',(-18.3998464503934,21.3014792644285,
-14.3072189012943));
#104565=CARTESIAN_POINT('Ctrl Pts',(-18.4082948797795,21.3028122113937,
-14.3067037355036));
#104566=CARTESIAN_POINT('Ctrl Pts',(-18.4231273933581,21.3050603648378,
-14.3058029785259));
#104567=CARTESIAN_POINT('Ctrl Pts',(-18.4295079701632,21.3059976597453,
-14.3054166919703));
#104568=CARTESIAN_POINT('Ctrl Pts',(-18.4419102531478,21.307761675116,-14.3046681319736));
#104569=CARTESIAN_POINT('Ctrl Pts',(-18.4479314263017,21.3085916463361,
-14.3043057592092));
#104570=CARTESIAN_POINT('Ctrl Pts',(-18.4623409382361,21.3105146846798,
-14.3034410071946));
#104571=CARTESIAN_POINT('Ctrl Pts',(-18.4707324596797,21.3115834338094,
-14.3029393990358));
#104572=CARTESIAN_POINT('Ctrl Pts',(-18.5010776134917,21.3152635131433,
-14.301132495736));
#104573=CARTESIAN_POINT('Ctrl Pts',(-18.5230658965378,21.3175812657428,
-14.2998364357305));
#104574=CARTESIAN_POINT('Ctrl Pts',(-18.7299334077737,21.3361152662931,
-14.2877568201063));
#104575=CARTESIAN_POINT('Ctrl Pts',(-18.9161494182181,21.3282999399898,
-14.2778298586475));
#104576=CARTESIAN_POINT('Ctrl Pts',(-19.2067678941241,21.2774353700723,
-14.2617461892765));
#104577=CARTESIAN_POINT('Ctrl Pts',(-19.3129236077801,21.2502414434953,
-14.255713645448));
#104578=CARTESIAN_POINT('Ctrl Pts',(-19.4276535289006,21.2111682311234,
-14.2485600409417));
#104579=CARTESIAN_POINT('Ctrl Pts',(-19.4387884746274,21.2072718659285,
-14.2478588884412));
#104580=CARTESIAN_POINT('Ctrl Pts',(-19.4545987856627,21.2015907228319,
-14.2468527465442));
#104581=CARTESIAN_POINT('Ctrl Pts',(-19.4593015164607,21.1998820339005,
-14.2465521309908));
#104582=CARTESIAN_POINT('Ctrl Pts',(-19.4674056668768,21.1969049086939,
-14.246031694697));
#104583=CARTESIAN_POINT('Ctrl Pts',(-19.4708099975528,21.195644352508,-14.2458123430376));
#104584=CARTESIAN_POINT('Ctrl Pts',(-19.4774125708833,21.1931802205314,
-14.2453854722866));
#104585=CARTESIAN_POINT('Ctrl Pts',(-19.4806111475846,21.1919776553842,
-14.245178019509));
#104586=CARTESIAN_POINT('Ctrl Pts',(-19.489250696036,21.1887055578311,-14.2446159245346));
#104587=CARTESIAN_POINT('Ctrl Pts',(-19.4946860188193,21.1866213367628,
-14.2442604157527));
#104588=CARTESIAN_POINT('Ctrl Pts',(-19.514929398964,21.1787629163425,-14.2429295063666));
#104589=CARTESIAN_POINT('Ctrl Pts',(-19.529680450471,21.1728445930577,-14.2419459861255));
#104590=CARTESIAN_POINT('Ctrl Pts',(-19.6585595515571,21.1194439722711,
-14.2332409824132));
#104591=CARTESIAN_POINT('Ctrl Pts',(-19.7683817729444,21.0622205094752,
-14.2250614637882));
#104592=CARTESIAN_POINT('Ctrl Pts',(-20.0134987630084,20.9058493352509,
-14.2058482408526));
#104593=CARTESIAN_POINT('Ctrl Pts',(-20.1433070245278,20.799554649955,-14.1949304646484));
#104594=CARTESIAN_POINT('Ctrl Pts',(-20.2740376622133,20.6637306971835,
-14.1833518380511));
#104595=CARTESIAN_POINT('Ctrl Pts',(-20.2885731834927,20.6481655258684,
-14.1820539067332));
#104596=CARTESIAN_POINT('Ctrl Pts',(-20.3089101436537,20.6257183189353,
-14.1802221201685));
#104597=CARTESIAN_POINT('Ctrl Pts',(-20.3149060239489,20.6190149252966,
-14.1796800407352));
#104598=CARTESIAN_POINT('Ctrl Pts',(-20.3251769992412,20.6073836548643,
-14.1787478709533));
#104599=CARTESIAN_POINT('Ctrl Pts',(-20.3294723330081,20.6024738914441,
-14.1783569353496));
#104600=CARTESIAN_POINT('Ctrl Pts',(-20.3376537895791,20.593034421189,-14.1776101519217));
#104601=CARTESIAN_POINT('Ctrl Pts',(-20.3415435794725,20.5885079888707,
-14.177254153898));
#104602=CARTESIAN_POINT('Ctrl Pts',(-20.3516099194524,20.5766933820188,
-14.1763303528689));
#104603=CARTESIAN_POINT('Ctrl Pts',(-20.3577564141384,20.569379688192,-14.1757637884633));
#104604=CARTESIAN_POINT('Ctrl Pts',(-20.3785534567884,20.5442904860486,
-14.1738379611169));
#104605=CARTESIAN_POINT('Ctrl Pts',(-20.3929636275252,20.5263171998545,
-14.172488428772));
#104606=CARTESIAN_POINT('Ctrl Pts',(-20.5142339457141,20.3698968294222,
-14.1609878779454));
#104607=CARTESIAN_POINT('Ctrl Pts',(-20.6038503965437,20.2189389781553,
-14.1515818203584));
#104608=CARTESIAN_POINT('Ctrl Pts',(-20.7088877048325,19.9785607387108,
-14.1373097913567));
#104609=CARTESIAN_POINT('Ctrl Pts',(-20.7388927332316,19.8963711717698,
-14.1325253074778));
#104610=CARTESIAN_POINT('Ctrl Pts',(-20.774507313731,19.7762056476618,-14.1253702987708));
#104611=CARTESIAN_POINT('Ctrl Pts',(-20.7843050112086,19.7395607630782,
-14.1231673499135));
#104612=CARTESIAN_POINT('Ctrl Pts',(-20.7948724782272,19.6953047074352,
-14.1204602440323));
#104613=CARTESIAN_POINT('Ctrl Pts',(-20.7965927840851,19.6879249671223,
-14.1200072897686));
#104614=CARTESIAN_POINT('Ctrl Pts',(-20.7992012898457,19.676456909532,-14.1193007881222));
#104615=CARTESIAN_POINT('Ctrl Pts',(-20.8001170725569,19.6723748411057,
-14.1190487952217));
#104616=CARTESIAN_POINT('Ctrl Pts',(-20.8017905255752,19.6648105795938,
-14.1185808466496));
#104617=CARTESIAN_POINT('Ctrl Pts',(-20.8025515054841,19.6613291778122,
-14.1183650833212));
#104618=CARTESIAN_POINT('Ctrl Pts',(-20.8042489796066,19.6534683252953,
-14.1178770167999));
#104619=CARTESIAN_POINT('Ctrl Pts',(-20.8051803639459,19.6490878400551,
-14.1176044271311));
#104620=CARTESIAN_POINT('Ctrl Pts',(-20.8078797709372,19.6361909583271,
-14.1168001423127));
#104621=CARTESIAN_POINT('Ctrl Pts',(-20.8096091896308,19.6276667029089,
-14.1162663232883));
#104622=CARTESIAN_POINT('Ctrl Pts',(-20.8214936993915,19.5671776614161,
-14.1124637251107));
#104623=CARTESIAN_POINT('Ctrl Pts',(-20.8297477800314,19.5148629594319,
-14.1090993050803));
#104624=CARTESIAN_POINT('Ctrl Pts',(-20.8378088383535,19.4474349197908,
-14.1047116242331));
#104625=CARTESIAN_POINT('Ctrl Pts',(-20.8394281081353,19.4325526253307,
-14.103739991965));
#104626=CARTESIAN_POINT('Ctrl Pts',(-20.8475637100768,19.3496083921713,
-14.0983109135824));
#104627=CARTESIAN_POINT('Ctrl Pts',(-20.8509374101805,19.2812805401817,
-14.0937882933207));
#104628=CARTESIAN_POINT('Ctrl Pts',(-20.8511442879771,19.0521414075599,
-14.0786473323232));
#104629=CARTESIAN_POINT('Ctrl Pts',(-20.8329752264163,18.8918491684336,
-14.068149332205));
#104630=CARTESIAN_POINT('Ctrl Pts',(-20.7914795967818,18.711968850762,-14.0567778297863));
#104631=CARTESIAN_POINT('Ctrl Pts',(-20.7857446857667,18.688890628449,-14.0553255502215));
#104632=CARTESIAN_POINT('Ctrl Pts',(-20.7771304028878,18.6565626300262,
-14.0532998512992));
#104633=CARTESIAN_POINT('Ctrl Pts',(-20.7745746989702,18.6472291749167,
-14.0527160284796));
#104634=CARTESIAN_POINT('Ctrl Pts',(-20.7703333352122,18.6321464466819,
-14.0517741466886));
#104635=CARTESIAN_POINT('Ctrl Pts',(-20.7686871311575,18.6263863089748,
-14.0514148108242));
#104636=CARTESIAN_POINT('Ctrl Pts',(-20.7652024820197,18.6143863980278,
-14.0506669636328));
#104637=CARTESIAN_POINT('Ctrl Pts',(-20.7633596813769,18.608147946773,-14.050278598788));
#104638=CARTESIAN_POINT('Ctrl Pts',(-20.758930467693,18.593404154119,-14.0493616993591));
#104639=CARTESIAN_POINT('Ctrl Pts',(-20.7563191638836,18.5849063720951,
-14.0488339846072));
#104640=CARTESIAN_POINT('Ctrl Pts',(-20.7474528177427,18.5566875481663,
-14.0470839024837));
#104641=CARTESIAN_POINT('Ctrl Pts',(-20.740962098308,18.5370413850976,-14.0458692713577));
#104642=CARTESIAN_POINT('Ctrl Pts',(-20.7304048691224,18.5065926607223,
-14.0439913314941));
#104643=CARTESIAN_POINT('Ctrl Pts',(-20.7265368450947,18.4957245523086,
-14.0433219475054));
#104644=CARTESIAN_POINT('Ctrl Pts',(-20.7225806179957,18.4848897289449,
-14.042655348398));
#104645=CARTESIAN_POINT('Origin',(-18.734,19.211,0.));
#104646=CARTESIAN_POINT('',(-20.7225806137986,18.4848897174502,-13.2445592988469));
#104647=CARTESIAN_POINT('',(-20.722580578415,18.4848896205462,-13.4647888589437));
#104648=CARTESIAN_POINT('',(-20.7225806137986,18.4848897174502,0.));
#104649=CARTESIAN_POINT('',(-20.8509991049198,19.2090532671894,-13.5109437209775));
#104650=CARTESIAN_POINT('Ctrl Pts',(-20.722580578415,18.4848896205462,-13.4647888589437));
#104651=CARTESIAN_POINT('Ctrl Pts',(-20.7382333493556,18.5277574780669,
-13.4673502679699));
#104652=CARTESIAN_POINT('Ctrl Pts',(-20.7525027540004,18.5711391169453,
-13.469956309288));
#104653=CARTESIAN_POINT('Ctrl Pts',(-20.7697993266343,18.630088286143,-13.4735579249014));
#104654=CARTESIAN_POINT('Ctrl Pts',(-20.7740668388379,18.6452574987151,
-13.4744900199622));
#104655=CARTESIAN_POINT('Ctrl Pts',(-20.7796729209201,18.6660734476574,
-13.4757780950466));
#104656=CARTESIAN_POINT('Ctrl Pts',(-20.7811583220313,18.6716805681512,
-13.4761259490076));
#104657=CARTESIAN_POINT('Ctrl Pts',(-20.7834811070311,18.6805965296512,
-13.476680591069));
#104658=CARTESIAN_POINT('Ctrl Pts',(-20.7843335776018,18.6839014611929,
-13.4768865132768));
#104659=CARTESIAN_POINT('Ctrl Pts',(-20.7860768721339,18.6907282364931,
-13.4773125806241));
#104660=CARTESIAN_POINT('Ctrl Pts',(-20.786966621664,18.6942503056574,-13.4775327886363));
#104661=CARTESIAN_POINT('Ctrl Pts',(-20.7890638353797,18.7026430250298,
-13.4780584284453));
#104662=CARTESIAN_POINT('Ctrl Pts',(-20.7902630515217,18.7075156971233,
-13.4783643314232));
#104663=CARTESIAN_POINT('Ctrl Pts',(-20.7927674039711,18.7178496121134,
-13.4790145549943));
#104664=CARTESIAN_POINT('Ctrl Pts',(-20.7940681569147,18.7233118660594,
-13.4793591136575));
#104665=CARTESIAN_POINT('Ctrl Pts',(-20.7975804759611,18.7383259597019,
-13.4803084562977));
#104666=CARTESIAN_POINT('Ctrl Pts',(-20.7997474095153,18.7478879604707,
-13.4809155631972));
#104667=CARTESIAN_POINT('Ctrl Pts',(-20.8343835380824,18.9058077632302,
-13.4909794453464));
#104668=CARTESIAN_POINT('Ctrl Pts',(-20.8508585305076,19.0572035887683,
-13.5011356069027));
#104669=CARTESIAN_POINT('Ctrl Pts',(-20.8509990928573,19.2090401934883,
-13.5111420888258));
#104670=CARTESIAN_POINT('Ctrl Pts',(-20.8509991049198,19.2090532671894,
-13.5109437209775));
#104671=CARTESIAN_POINT('Ctrl Pts',(-20.8510652701871,19.2810055201563,
-13.5152699622426));
#104672=CARTESIAN_POINT('Ctrl Pts',(-20.84745892973,19.3530526998716,-13.5195962035077));
#104673=CARTESIAN_POINT('Ctrl Pts',(-20.8401777557621,19.424785549402,-13.5239224447729));
#104674=CARTESIAN_POINT('Ctrl Pts',(-20.8329012160598,19.4964727429599,
-13.5282459325052));
#104675=CARTESIAN_POINT('Ctrl Pts',(-20.8219545300652,19.5678455121802,
-13.5325694202376));
#104676=CARTESIAN_POINT('Ctrl Pts',(-20.8073873938026,19.6384970353352,
-13.5368929079699));
#104677=CARTESIAN_POINT('Ctrl Pts',(-20.7928244565269,19.7091281931407,
-13.541215149454));
#104678=CARTESIAN_POINT('Ctrl Pts',(-20.7746432396996,19.7790380332555,
-13.5455373909381));
#104679=CARTESIAN_POINT('Ctrl Pts',(-20.7529446959791,19.8478291093989,
-13.5498596324221));
#104680=CARTESIAN_POINT('Ctrl Pts',(-20.7312448511872,19.91662431034,-13.5541821330731));
#104681=CARTESIAN_POINT('Ctrl Pts',(-20.7060274126677,19.9843001434093,
-13.5585046337241));
#104682=CARTESIAN_POINT('Ctrl Pts',(-20.6774428750096,20.0504753073047,
-13.5628271343751));
#104683=CARTESIAN_POINT('Ctrl Pts',(-20.6488284904874,20.1167195687362,
-13.5671541484135));
#104684=CARTESIAN_POINT('Ctrl Pts',(-20.6168401898343,20.1814595804048,
-13.5714811624518));
#104685=CARTESIAN_POINT('Ctrl Pts',(-20.5816757716208,20.2443359777756,
-13.5758081764901));
#104686=CARTESIAN_POINT('Ctrl Pts',(-20.5464899011033,20.3072507333408,
-13.5801378302542));
#104687=CARTESIAN_POINT('Ctrl Pts',(-20.5081243239342,20.3682991960122,
-13.5844674840182));
#104688=CARTESIAN_POINT('Ctrl Pts',(-20.4668202589893,20.4271508747011,
-13.5887971377823));
#104689=CARTESIAN_POINT('Ctrl Pts',(-20.4254474059594,20.4861005653963,
-13.5931340021827));
#104690=CARTESIAN_POINT('Ctrl Pts',(-20.3811266092583,20.5428457872319,
-13.5974708665831));
#104691=CARTESIAN_POINT('Ctrl Pts',(-20.334138776401,20.5970897865066,-13.6018077309835));
#104692=CARTESIAN_POINT('Ctrl Pts',(-20.317565474994,20.6162224447893,-13.6033374069975));
#104693=CARTESIAN_POINT('Ctrl Pts',(-20.3006606978845,20.6350442778647,
-13.6048670830114));
#104694=CARTESIAN_POINT('Ctrl Pts',(-20.2834377820479,20.6535434342032,
-13.6063967590254));
#104695=CARTESIAN_POINT('Ctrl Pts',(-20.2340300954521,20.7066122947448,
-13.6107849679563));
#104696=CARTESIAN_POINT('Ctrl Pts',(-20.1817963672775,20.757243459066,-13.6151731768872));
#104697=CARTESIAN_POINT('Ctrl Pts',(-20.1270066890246,20.8051208750696,
-13.6195613858181));
#104698=CARTESIAN_POINT('Ctrl Pts',(-20.0722983277385,20.8529272330497,
-13.6239430819193));
#104699=CARTESIAN_POINT('Ctrl Pts',(-20.0150419071299,20.8979876412174,
-13.6283247780206));
#104700=CARTESIAN_POINT('Ctrl Pts',(-19.9555455237305,20.9400215537853,
-13.6327064741219));
#104701=CARTESIAN_POINT('Ctrl Pts',(-19.8961190533166,20.9820060731606,
-13.6370830213815));
#104702=CARTESIAN_POINT('Ctrl Pts',(-19.834458240882,21.0209708847355,-13.6414595686412));
#104703=CARTESIAN_POINT('Ctrl Pts',(-19.7709042257781,21.0566756558408,
-13.6458361159008));
#104704=CARTESIAN_POINT('Ctrl Pts',(-19.7073905157069,21.0923577834992,
-13.6502098876178));
#104705=CARTESIAN_POINT('Ctrl Pts',(-19.6419864047143,21.1247837371303,
-13.6545836593348));
#104706=CARTESIAN_POINT('Ctrl Pts',(-19.5750607832518,21.1537572568069,
-13.6589574310518));
#104707=CARTESIAN_POINT('Ctrl Pts',(-19.5081555274806,21.1827219597441,
-13.6633298718153));
#104708=CARTESIAN_POINT('Ctrl Pts',(-19.4397301228475,21.2082361229382,
-13.6677023125789));
#104709=CARTESIAN_POINT('Ctrl Pts',(-19.3701752330585,21.2301508296417,
-13.6720747533424));
#104710=CARTESIAN_POINT('Ctrl Pts',(-19.3006185647433,21.2520660967068,
-13.6764473059098));
#104711=CARTESIAN_POINT('Ctrl Pts',(-19.2299328146144,21.2703815814965,
-13.6808198584771));
#104712=CARTESIAN_POINT('Ctrl Pts',(-19.1585240564091,21.2849981498376,
-13.6851924110445));
#104713=CARTESIAN_POINT('Ctrl Pts',(-19.0870411875011,21.2996298878047,
-13.6895695016118));
#104714=CARTESIAN_POINT('Ctrl Pts',(-19.0148342859528,21.3105549478118,
-13.6939465921791));
#104715=CARTESIAN_POINT('Ctrl Pts',(-18.94231905461,21.3177254618213,-13.6983236827465));
#104716=CARTESIAN_POINT('Ctrl Pts',(-18.869764220008,21.3248998919147,-13.7027031638054));
#104717=CARTESIAN_POINT('Ctrl Pts',(-18.7969012025304,21.3283156708867,
-13.7070826448644));
#104718=CARTESIAN_POINT('Ctrl Pts',(-18.7241475303624,21.3279770732915,
-13.7114621259233));
#104719=CARTESIAN_POINT('Ctrl Pts',(-18.6512649027988,21.3276378755344,
-13.715849369583));
#104720=CARTESIAN_POINT('Ctrl Pts',(-18.5784924896188,21.3235310394329,
-13.7202366132427));
#104721=CARTESIAN_POINT('Ctrl Pts',(-18.5062439309,21.3157128481073,-13.7246238569025));
#104722=CARTESIAN_POINT('Ctrl Pts',(-18.4571218728267,21.3103972313652,
-13.7276067598372));
#104723=CARTESIAN_POINT('Ctrl Pts',(-18.408241843935,21.3033670563133,-13.730589662772));
#104724=CARTESIAN_POINT('Ctrl Pts',(-18.3597305432933,21.2946533717911,
-13.7335725657068));
#104725=CARTESIAN_POINT('Ctrl Pts',(-18.2883645862437,21.2818344939807,
-13.7379607746377));
#104726=CARTESIAN_POINT('Ctrl Pts',(-18.2175186632351,21.2653198837036,
-13.7423489835686));
#104727=CARTESIAN_POINT('Ctrl Pts',(-18.1476047194716,21.2451655721632,
-13.7467371924995));
#104728=CARTESIAN_POINT('Ctrl Pts',(-18.0777945395925,21.2250411729628,
-13.7511188886007));
#104729=CARTESIAN_POINT('Ctrl Pts',(-18.0089140527663,21.201287928559,-13.755500584702));
#104730=CARTESIAN_POINT('Ctrl Pts',(-17.9413659204117,21.1740130452636,
-13.7598822808033));
#104731=CARTESIAN_POINT('Ctrl Pts',(-17.8738971624885,21.1467702121269,
-13.7642588280629));
#104732=CARTESIAN_POINT('Ctrl Pts',(-17.8077580939881,21.116014140384,-13.7686353753226));
#104733=CARTESIAN_POINT('Ctrl Pts',(-17.7433354489126,21.0819015867273,
-13.7730119225822));
#104734=CARTESIAN_POINT('Ctrl Pts',(-17.6789536597423,21.0478106667564,
-13.7773856942992));
#104735=CARTESIAN_POINT('Ctrl Pts',(-17.6162865594638,21.0103677135303,
-13.7817594660161));
#104736=CARTESIAN_POINT('Ctrl Pts',(-17.5556988450219,20.9697766737642,
-13.7861332377331));
#104737=CARTESIAN_POINT('Ctrl Pts',(-17.4951295676249,20.9291979859878,
-13.7905056784967));
#104738=CARTESIAN_POINT('Ctrl Pts',(-17.4366388203451,20.885473381869,-13.7948781192602));
#104739=CARTESIAN_POINT('Ctrl Pts',(-17.380563277455,20.8388507419498,-13.7992505600238));
#104740=CARTESIAN_POINT('Ctrl Pts',(-17.3244863007071,20.7922269098846,
-13.8036231125911));
#104741=CARTESIAN_POINT('Ctrl Pts',(-17.2708250206039,20.7427052048249,
-13.8079956651585));
#104742=CARTESIAN_POINT('Ctrl Pts',(-17.2198825933089,20.6905734110732,
-13.8123682177258));
#104743=CARTESIAN_POINT('Ctrl Pts',(-17.1688872960413,20.6383875129797,
-13.8167453082932));
#104744=CARTESIAN_POINT('Ctrl Pts',(-17.1206168232076,20.5835864635392,
-13.8211223988605));
#104745=CARTESIAN_POINT('Ctrl Pts',(-17.0753364363183,20.5264938929979,
-13.8254994894278));
#104746=CARTESIAN_POINT('Ctrl Pts',(-17.0300313201292,20.4693701420848,
-13.8298789704868));
#104747=CARTESIAN_POINT('Ctrl Pts',(-16.9877198211683,20.409952771581,-13.8342584515457));
#104748=CARTESIAN_POINT('Ctrl Pts',(-16.9486243452996,20.3485951703497,
-13.8386379326047));
#104749=CARTESIAN_POINT('Ctrl Pts',(-16.9094595729623,20.2871288131822,
-13.8430251762644));
#104750=CARTESIAN_POINT('Ctrl Pts',(-16.8735224451864,20.2237157776925,
-13.8474124199241));
#104751=CARTESIAN_POINT('Ctrl Pts',(-16.8409895323034,20.1587343347116,
-13.8517996635838));
#104752=CARTESIAN_POINT('Ctrl Pts',(-16.8188702864072,20.1145532150819,
-13.8547825665186));
#104753=CARTESIAN_POINT('Ctrl Pts',(-16.7983237185204,20.0696475457982,
-13.8577654694534));
#104754=CARTESIAN_POINT('Ctrl Pts',(-16.7793923012851,20.0241406668741,
-13.8607483723882));
#104755=CARTESIAN_POINT('Ctrl Pts',(-16.7515419099038,19.9571945754736,
-13.8651365813191));
#104756=CARTESIAN_POINT('Ctrl Pts',(-16.7270805292279,19.8886853205153,
-13.86952479025));
#104757=CARTESIAN_POINT('Ctrl Pts',(-16.706184024008,19.8189896113517,-13.8739129991809));
#104758=CARTESIAN_POINT('Ctrl Pts',(-16.6853185326666,19.7493973421762,
-13.8782946952822));
#104759=CARTESIAN_POINT('Ctrl Pts',(-16.6680075510805,19.6786225726489,
-13.8826763913834));
#104760=CARTESIAN_POINT('Ctrl Pts',(-16.6543788886961,19.6070619060438,
-13.8870580874847));
#104761=CARTESIAN_POINT('Ctrl Pts',(-16.6407662410746,19.5355853289171,
-13.8914346347443));
#104762=CARTESIAN_POINT('Ctrl Pts',(-16.6308274068039,19.4633251607434,
-13.895811182004));
#104763=CARTESIAN_POINT('Ctrl Pts',(-16.6246399100932,19.390691433041,-13.9001877292636));
#104764=CARTESIAN_POINT('Ctrl Pts',(-16.618456337403,19.318103768593,-13.9045615009806));
#104765=CARTESIAN_POINT('Ctrl Pts',(-16.6160194227851,19.2451434941229,
-13.9089352726976));
#104766=CARTESIAN_POINT('Ctrl Pts',(-16.6173550828665,19.1722276545356,
-13.9133090444145));
#104767=CARTESIAN_POINT('Ctrl Pts',(-16.618690336502,19.099334003483,-13.9176814851781));
#104768=CARTESIAN_POINT('Ctrl Pts',(-16.6237958768595,19.0264852424754,
-13.9220539259417));
#104769=CARTESIAN_POINT('Ctrl Pts',(-16.6326455110292,18.9540986343319,
-13.9264263667052));
#104770=CARTESIAN_POINT('Ctrl Pts',(-16.6414953714849,18.8817101752551,
-13.9307989192725));
#104771=CARTESIAN_POINT('Ctrl Pts',(-16.6540894553072,18.8097843710746,
-13.9351714718399));
#104772=CARTESIAN_POINT('Ctrl Pts',(-16.6703498741218,18.7387319003334,
-13.9395440244072));
#104773=CARTESIAN_POINT('Ctrl Pts',(-16.6866271686123,18.6676056886579,
-13.9439211149745));
#104774=CARTESIAN_POINT('Ctrl Pts',(-16.7065782873147,18.5973550912947,
-13.9482982055419));
#104775=CARTESIAN_POINT('Ctrl Pts',(-16.7300746894319,18.5283783261097,
-13.9526752961092));
#104776=CARTESIAN_POINT('Ctrl Pts',(-16.7535839238065,18.4593638901532,
-13.9570547771681));
#104777=CARTESIAN_POINT('Ctrl Pts',(-16.7806421175109,18.3916251197528,
-13.9614342582271));
#104778=CARTESIAN_POINT('Ctrl Pts',(-16.811072510512,18.325540305733,-13.965813739286));
#104779=CARTESIAN_POINT('Ctrl Pts',(-16.8415568411804,18.2593383568239,
-13.9702009829457));
#104780=CARTESIAN_POINT('Ctrl Pts',(-16.8754250830332,18.1947966461509,
-13.9745882266055));
#104781=CARTESIAN_POINT('Ctrl Pts',(-16.9124547443357,18.1322683922463,
-13.9789754702652));
#104782=CARTESIAN_POINT('Ctrl Pts',(-16.9376313458519,18.0897552047992,
-13.9819583732));
#104783=CARTESIAN_POINT('Ctrl Pts',(-16.9642684397429,18.0481722056908,
-13.9849412761348));
#104784=CARTESIAN_POINT('Ctrl Pts',(-16.992285306212,18.0076218693017,-13.9879241790697));
#104785=CARTESIAN_POINT('Ctrl Pts',(-17.033501486001,17.9479674480279,-13.9923123880006));
#104786=CARTESIAN_POINT('Ctrl Pts',(-17.0778664461833,17.8903165376486,
-13.9967005969315));
#104787=CARTESIAN_POINT('Ctrl Pts',(-17.1251586260628,17.8350209182157,
-14.0010888058624));
#104788=CARTESIAN_POINT('Ctrl Pts',(-17.1723806165062,17.7798073666503,
-14.0054705019636));
#104789=CARTESIAN_POINT('Ctrl Pts',(-17.2225208913247,17.7269425302633,
-14.0098521980649));
#104790=CARTESIAN_POINT('Ctrl Pts',(-17.2753151507578,17.6767485504028,
-14.0142338941661));
#104791=CARTESIAN_POINT('Ctrl Pts',(-17.3280473727346,17.6266135524631,
-14.0186104414258));
#104792=CARTESIAN_POINT('Ctrl Pts',(-17.3834270362633,17.5791435071861,
-14.0229869886854));
#104793=CARTESIAN_POINT('Ctrl Pts',(-17.4411513321101,17.5346255424472,
-14.0273635359451));
#104794=CARTESIAN_POINT('Ctrl Pts',(-17.4988390200475,17.4901358103546,
-14.031737307662));
#104795=CARTESIAN_POINT('Ctrl Pts',(-17.5588680090001,17.4485947380414,
-14.036111079379));
#104796=CARTESIAN_POINT('Ctrl Pts',(-17.6209016583806,17.4102498557867,
-14.040484851096));
#104797=CARTESIAN_POINT('Ctrl Pts',(-17.6829164307132,17.3719166420085,
-14.0448572918595));
#104798=CARTESIAN_POINT('Ctrl Pts',(-17.7469342423155,17.3367779408325,
-14.0492297326231));
#104799=CARTESIAN_POINT('Ctrl Pts',(-17.8125900634645,17.3050375846167,
-14.0536021733866));
#104800=CARTESIAN_POINT('Ctrl Pts',(-17.87824756344,17.2732964167966,-14.057974725954));
#104801=CARTESIAN_POINT('Ctrl Pts',(-17.9455427209579,17.244953974612,-14.0623472785213));
#104802=CARTESIAN_POINT('Ctrl Pts',(-18.0140880608552,17.2201670587724,
-14.0667198310887));
#104803=CARTESIAN_POINT('Ctrl Pts',(-18.0827045396917,17.1953544181367,
-14.071096921656));
#104804=CARTESIAN_POINT('Ctrl Pts',(-18.1525733368268,17.1741048356876,
-14.0754740122233));
#104805=CARTESIAN_POINT('Ctrl Pts',(-18.2232900373592,17.1565257767352,
-14.0798511027906));
#104806=CARTESIAN_POINT('Ctrl Pts',(-18.2940453589065,17.1389371172062,
-14.0842305838496));
#104807=CARTESIAN_POINT('Ctrl Pts',(-18.3656490319735,17.1250230644093,
-14.0886100649085));
#104808=CARTESIAN_POINT('Ctrl Pts',(-18.4376872969892,17.1148397527779,
-14.0929895459675));
#104809=CARTESIAN_POINT('Ctrl Pts',(-18.5098532493459,17.1046383912949,
-14.0973767896272));
#104810=CARTESIAN_POINT('Ctrl Pts',(-18.5824548510276,17.0981810190706,
-14.1017640332869));
#104811=CARTESIAN_POINT('Ctrl Pts',(-18.6550746705905,17.0954717462587,
-14.1061512769466));
#104812=CARTESIAN_POINT('Ctrl Pts',(-18.7044491502642,17.0936297018115,
-14.1091341798814));
#104813=CARTESIAN_POINT('Ctrl Pts',(-18.7538320255728,17.093519193629,-14.1121170828162));
#104814=CARTESIAN_POINT('Ctrl Pts',(-18.8030934396837,17.0951278165748,
-14.1150999857511));
#104815=CARTESIAN_POINT('Ctrl Pts',(-18.8755629038515,17.0974942943756,
-14.119488194682));
#104816=CARTESIAN_POINT('Ctrl Pts',(-18.9480521075248,17.1035928606293,
-14.1238764036129));
#104817=CARTESIAN_POINT('Ctrl Pts',(-19.0201453327482,17.1134276297237,
-14.1282646125438));
#104818=CARTESIAN_POINT('Ctrl Pts',(-19.0921315596719,17.1232478023901,
-14.132646308645));
#104819=CARTESIAN_POINT('Ctrl Pts',(-19.1637225008055,17.1367931053666,
-14.1370280047463));
#104820=CARTESIAN_POINT('Ctrl Pts',(-19.2345042258075,17.1540156733828,
-14.1414097008476));
#104821=CARTESIAN_POINT('Ctrl Pts',(-19.3052027766498,17.171218003511,-14.1457862481072));
#104822=CARTESIAN_POINT('Ctrl Pts',(-19.37509353394,17.1920889013491,-14.1501627953669));
#104823=CARTESIAN_POINT('Ctrl Pts',(-19.4437711636788,17.2165291691253,
-14.1545393426265));
#104824=CARTESIAN_POINT('Ctrl Pts',(-19.512405239063,17.2409539372389,-14.1589131143435));
#104825=CARTESIAN_POINT('Ctrl Pts',(-19.5798272600414,17.2689434226003,
-14.1632868860605));
#104826=CARTESIAN_POINT('Ctrl Pts',(-19.6456468756569,17.3003485471952,
-14.1676606577774));
#104827=CARTESIAN_POINT('Ctrl Pts',(-19.7114464621424,17.3317441151053,
-14.172033098541));
#104828=CARTESIAN_POINT('Ctrl Pts',(-19.775644176238,17.3665530511362,-14.1764055393046));
#104829=CARTESIAN_POINT('Ctrl Pts',(-19.837871043522,17.4045787536475,-14.1807779800681));
#104830=CARTESIAN_POINT('Ctrl Pts',(-19.9000995019538,17.4426054284802,
-14.1851505326355));
#104831=CARTESIAN_POINT('Ctrl Pts',(-19.9603566029532,17.4838487798657,
-14.1895230852028));
#104832=CARTESIAN_POINT('Ctrl Pts',(-20.018300768981,17.5280678757612,-14.1938956377702));
#104833=CARTESIAN_POINT('Ctrl Pts',(-20.0763050716499,17.5723328639025,
-14.1982727283375));
#104834=CARTESIAN_POINT('Ctrl Pts',(-20.131991262393,17.6195794693668,-14.2026498189048));
#104835=CARTESIAN_POINT('Ctrl Pts',(-20.1850500777755,17.6695258121565,
-14.2070269094722));
#104836=CARTESIAN_POINT('Ctrl Pts',(-20.2381378705463,17.7194994324977,
-14.2114063905311));
#104837=CARTESIAN_POINT('Ctrl Pts',(-20.2885950971619,17.772175377142,-14.21578587159));
#104838=CARTESIAN_POINT('Ctrl Pts',(-20.3361505972391,17.8272361242732,
-14.220165352649));
#104839=CARTESIAN_POINT('Ctrl Pts',(-20.383790389121,17.8823944662092,-14.2245525963087));
#104840=CARTESIAN_POINT('Ctrl Pts',(-20.4285178872523,17.9399456706598,
-14.2289398399684));
#104841=CARTESIAN_POINT('Ctrl Pts',(-20.470103687921,17.9995409685891,-14.2333270836282));
#104842=CARTESIAN_POINT('Ctrl Pts',(-20.4983780251772,18.0400600285913,
-14.2363099865629));
#104843=CARTESIAN_POINT('Ctrl Pts',(-20.5252009588543,18.0815233957326,
-14.2392928894977));
#104844=CARTESIAN_POINT('Ctrl Pts',(-20.5505126306683,18.1238151663023,
-14.2422757924325));
#104845=CARTESIAN_POINT('Ctrl Pts',(-20.5890177730692,18.1881511240427,
-14.2468135054337));
#104846=CARTESIAN_POINT('Ctrl Pts',(-20.6241652163586,18.2546416816847,
-14.2513512184349));
#104847=CARTESIAN_POINT('Ctrl Pts',(-20.6557165770165,18.3229153206929,
-14.255888931436));
#104848=CARTESIAN_POINT('Ctrl Pts',(-20.680200416808,18.37589562977,-14.2594101944124));
#104849=CARTESIAN_POINT('Ctrl Pts',(-20.7025195409889,18.4299489440717,
-14.2629314573889));
#104850=CARTESIAN_POINT('Ctrl Pts',(-20.7225806137986,18.4848897174502,
-14.2664527203653));
#104851=CARTESIAN_POINT('',(-20.8509999987372,19.2109341274623,-13.2889033777666));
#104852=CARTESIAN_POINT('Ctrl Pts',(-20.7225806179957,18.4848897289449,
-14.042655348398));
#104853=CARTESIAN_POINT('Ctrl Pts',(-20.6958130730314,18.411582101675,-14.0381451872939));
#104854=CARTESIAN_POINT('Ctrl Pts',(-20.6650078049974,18.3397979900317,
-14.0337656578687));
#104855=CARTESIAN_POINT('Ctrl Pts',(-20.5703572068461,18.1490855410707,
-14.0220205677548));
#104856=CARTESIAN_POINT('Ctrl Pts',(-20.4990149242829,18.0343138383552,
-14.0148421229976));
#104857=CARTESIAN_POINT('Ctrl Pts',(-20.3708541763278,17.8662886020928,
-14.0031498605669));
#104858=CARTESIAN_POINT('Ctrl Pts',(-20.3212057311274,17.808033269361,-13.9988302806948));
#104859=CARTESIAN_POINT('Ctrl Pts',(-20.2619779462149,17.7457141564181,
-13.9937349088717));
#104860=CARTESIAN_POINT('Ctrl Pts',(-20.2553888180463,17.7388738966237,
-13.9931687790576));
#104861=CARTESIAN_POINT('Ctrl Pts',(-20.2455537543989,17.7288005419894,
-13.9923244195925));
#104862=CARTESIAN_POINT('Ctrl Pts',(-20.2423428873456,17.7255331646068,
-13.9920488627986));
#104863=CARTESIAN_POINT('Ctrl Pts',(-20.2366096472776,17.7197367750051,
-13.9915569605736));
#104864=CARTESIAN_POINT('Ctrl Pts',(-20.2340914540627,17.7172036994518,
-13.991340944181));
#104865=CARTESIAN_POINT('Ctrl Pts',(-20.228661806659,17.7117695387174,-13.9908752471347));
#104866=CARTESIAN_POINT('Ctrl Pts',(-20.2257483539505,17.7088705980691,
-13.9906254109197));
#104867=CARTESIAN_POINT('Ctrl Pts',(-20.2176786501626,17.7008877204961,
-13.9899335952082));
#104868=CARTESIAN_POINT('Ctrl Pts',(-20.2125047848917,17.6958217823571,
-13.9894902443921));
#104869=CARTESIAN_POINT('Ctrl Pts',(-20.1839451579348,17.6681434754153,
-13.9870446022492));
#104870=CARTESIAN_POINT('Ctrl Pts',(-20.1600679286851,17.6460472178848,
-13.9850059843469));
#104871=CARTESIAN_POINT('Ctrl Pts',(-20.0137580372223,17.5167796681214,
-13.9726001129272));
#104872=CARTESIAN_POINT('Ctrl Pts',(-19.8798138254873,17.4234671266425,
-13.9616428496239));
#104873=CARTESIAN_POINT('Ctrl Pts',(-19.633621638164,17.2911002983456,-13.9433847645602));
#104874=CARTESIAN_POINT('Ctrl Pts',(-19.5263234271556,17.2443873413246,
-13.935943923391));
#104875=CARTESIAN_POINT('Ctrl Pts',(-19.4021738970265,17.2021603277574,
-13.9279368651318));
#104876=CARTESIAN_POINT('Ctrl Pts',(-19.3885991772499,17.1976959697293,
-13.9270688889833));
#104877=CARTESIAN_POINT('Ctrl Pts',(-19.3669223603483,17.1908094731998,
-13.9256945802473));
#104878=CARTESIAN_POINT('Ctrl Pts',(-19.3588493390738,17.1882978999614,
-13.9251853195911));
#104879=CARTESIAN_POINT('Ctrl Pts',(-19.3445847673627,17.1839536435782,
-13.9242899413779));
#104880=CARTESIAN_POINT('Ctrl Pts',(-19.3383995130135,17.1821008109519,
-13.9239031676938));
#104881=CARTESIAN_POINT('Ctrl Pts',(-19.3255888907522,17.1783270879104,
-13.9231050989033));
#104882=CARTESIAN_POINT('Ctrl Pts',(-19.3189624097634,17.1764102221578,
-13.9226939391777));
#104883=CARTESIAN_POINT('Ctrl Pts',(-19.301929102279,17.1715730310412,-13.9216412294542));
#104884=CARTESIAN_POINT('Ctrl Pts',(-19.2915089843051,17.1686999324512,
-13.9210012207575));
#104885=CARTESIAN_POINT('Ctrl Pts',(-19.2479272724313,17.1570417239593,
-13.9183405566925));
#104886=CARTESIAN_POINT('Ctrl Pts',(-19.2145755213211,17.1489832187947,
-13.9163434300315));
#104887=CARTESIAN_POINT('Ctrl Pts',(-19.1271788443181,17.1301021281015,
-13.9111993570371));
#104888=CARTESIAN_POINT('Ctrl Pts',(-19.0728802628434,17.1205726825023,
-13.9080917996022));
#104889=CARTESIAN_POINT('Ctrl Pts',(-18.9099124733886,17.098489543352,-13.8989473917473));
#104890=CARTESIAN_POINT('Ctrl Pts',(-18.8005786658719,17.092223515184,-13.8930592707198));
#104891=CARTESIAN_POINT('Ctrl Pts',(-18.6455299772278,17.0953551150471,
-13.8846160489244));
#104892=CARTESIAN_POINT('Ctrl Pts',(-18.5998525756087,17.0977597260572,
-13.8821156305693));
#104893=CARTESIAN_POINT('Ctrl Pts',(-18.5315820550036,17.1035761262075,
-13.8783162737223));
#104894=CARTESIAN_POINT('Ctrl Pts',(-18.5089070656659,17.1058773129884,
-13.8770439999209));
#104895=CARTESIAN_POINT('Ctrl Pts',(-18.485247947572,17.1086649923696,-13.8757017357188));
#104896=CARTESIAN_POINT('Ctrl Pts',(-18.484221746921,17.1087866682521,-13.8756434866502));
#104897=CARTESIAN_POINT('Ctrl Pts',(-18.4649615763543,17.1110846349086,
-13.8745496898693));
#104898=CARTESIAN_POINT('Ctrl Pts',(-18.4467570686057,17.113497276096,-13.8735065358503));
#104899=CARTESIAN_POINT('Ctrl Pts',(-18.3954595014673,17.1209760597273,
-13.870535093925));
#104900=CARTESIAN_POINT('Ctrl Pts',(-18.3624535443507,17.1265905657932,
-13.8685854768916));
#104901=CARTESIAN_POINT('Ctrl Pts',(-18.3227963977621,17.134308257534,-13.8661823321725));
#104902=CARTESIAN_POINT('Ctrl Pts',(-18.3160027248365,17.1356650220548,
-13.865768486132));
#104903=CARTESIAN_POINT('Ctrl Pts',(-18.3048595476132,17.1379473604288,
-13.8650859480077));
#104904=CARTESIAN_POINT('Ctrl Pts',(-18.3005060229945,17.1388533484867,
-13.8648183489069));
#104905=CARTESIAN_POINT('Ctrl Pts',(-18.2926706296167,17.1405097021833,
-13.8643349850882));
#104906=CARTESIAN_POINT('Ctrl Pts',(-18.2891877760491,17.1412551433535,
-13.8641195041359));
#104907=CARTESIAN_POINT('Ctrl Pts',(-18.281593592813,17.1429005934615,-13.8636482859043));
#104908=CARTESIAN_POINT('Ctrl Pts',(-18.2774831116099,17.1438040628687,
-13.8633923569547));
#104909=CARTESIAN_POINT('Ctrl Pts',(-18.2658662574508,17.1463937449515,
-13.8626666425523));
#104910=CARTESIAN_POINT('Ctrl Pts',(-18.2583664340568,17.1481086077841,
-13.8621952613406));
#104911=CARTESIAN_POINT('Ctrl Pts',(-18.2119004766103,17.1590000823457,
-13.8592577122704));
#104912=CARTESIAN_POINT('Ctrl Pts',(-18.1731944931754,17.1692389272465,
-13.856736303602));
#104913=CARTESIAN_POINT('Ctrl Pts',(-17.9690531403683,17.2294824916377,
-13.843121949756));
#104914=CARTESIAN_POINT('Ctrl Pts',(-17.8099143250524,17.2985080203104,
-13.8314565276146));
#104915=CARTESIAN_POINT('Ctrl Pts',(-17.5755719392057,17.4363059996227,
-13.8138298892532));
#104916=CARTESIAN_POINT('Ctrl Pts',(-17.4938310886263,17.4924307398264,
-13.807566759031));
#104917=CARTESIAN_POINT('Ctrl Pts',(-17.4053921742042,17.5627631149222,
-13.8006702907172));
#104918=CARTESIAN_POINT('Ctrl Pts',(-17.3945602821391,17.5715534955558,
-13.7998232416422));
#104919=CARTESIAN_POINT('Ctrl Pts',(-17.3773802816722,17.5857794750148,
-13.7984757295764));
#104920=CARTESIAN_POINT('Ctrl Pts',(-17.3709762400321,17.5911465967939,
-13.7979725135282));
#104921=CARTESIAN_POINT('Ctrl Pts',(-17.359692170942,17.6007178892845,-13.7970841427596));
#104922=CARTESIAN_POINT('Ctrl Pts',(-17.3547992702955,17.6049066547349,
-13.7966983642457));
#104923=CARTESIAN_POINT('Ctrl Pts',(-17.3446742698157,17.6136549597503,
-13.7958988340944));
#104924=CARTESIAN_POINT('Ctrl Pts',(-17.3394453146628,17.6182180332734,
-13.7954852352326));
#104925=CARTESIAN_POINT('Ctrl Pts',(-17.3259874393489,17.6300791915124,
-13.7944188904457));
#104926=CARTESIAN_POINT('Ctrl Pts',(-17.3177927204877,17.6374158992849,
-13.7937677649064));
#104927=CARTESIAN_POINT('Ctrl Pts',(-17.2830234651263,17.6690363268499,
-13.7909968280477));
#104928=CARTESIAN_POINT('Ctrl Pts',(-17.2570125373051,17.6939327189636,
-13.7889031074881));
#104929=CARTESIAN_POINT('Ctrl Pts',(-17.1901468282785,17.7612841007466,
-13.7834508714955));
#104930=CARTESIAN_POINT('Ctrl Pts',(-17.1504065275373,17.8048025452666,
-13.7801382302178));
#104931=CARTESIAN_POINT('Ctrl Pts',(-17.0043329347156,17.9788221669772,
-13.7675424840969));
#104932=CARTESIAN_POINT('Ctrl Pts',(-16.91190054555,18.1201487556587,-13.7586861849334));
#104933=CARTESIAN_POINT('Ctrl Pts',(-16.8128696027153,18.3199647629898,
-13.7461588532331));
#104934=CARTESIAN_POINT('Ctrl Pts',(-16.7904740252312,18.369934313279,-13.7430207505521));
#104935=CARTESIAN_POINT('Ctrl Pts',(-16.7667664136729,18.4288503968053,
-13.7392524561609));
#104936=CARTESIAN_POINT('Ctrl Pts',(-16.7635416844412,18.4370103323876,
-13.7387290500662));
#104937=CARTESIAN_POINT('Ctrl Pts',(-16.7587418676888,18.4493803350026,
-13.7379330031894));
#104938=CARTESIAN_POINT('Ctrl Pts',(-16.7571292660949,18.4535758757834,
-13.7376625586426));
#104939=CARTESIAN_POINT('Ctrl Pts',(-16.7542617223017,18.4611079682206,
-13.7371761819725));
#104940=CARTESIAN_POINT('Ctrl Pts',(-16.753001835874,18.4644425802715,-13.7369605498521));
#104941=CARTESIAN_POINT('Ctrl Pts',(-16.7502860217403,18.4716859597222,
-13.7364914883805));
#104942=CARTESIAN_POINT('Ctrl Pts',(-16.7488332412056,18.4755958004064,
-13.7362378809895));
#104943=CARTESIAN_POINT('Ctrl Pts',(-16.7447936058274,18.4865667916328,
-13.7355251449198));
#104944=CARTESIAN_POINT('Ctrl Pts',(-16.7422328372145,18.4936373878204,
-13.7350645082201));
#104945=CARTESIAN_POINT('Ctrl Pts',(-16.7273185026433,18.5355132218763,
-13.732329386372));
#104946=CARTESIAN_POINT('Ctrl Pts',(-16.7158405901155,18.5706210247756,
-13.7300079385062));
#104947=CARTESIAN_POINT('Ctrl Pts',(-16.6814134294518,18.686065294998,-13.7223225020622));
#104948=CARTESIAN_POINT('Ctrl Pts',(-16.6623005532234,18.7674600858583,
-13.7168258124974));
#104949=CARTESIAN_POINT('Ctrl Pts',(-16.6172530614757,19.0275869716926,
-13.6993884806524));
#104950=CARTESIAN_POINT('Ctrl Pts',(-16.6093169881871,19.2086559989151,
-13.6875186961139));
#104951=CARTESIAN_POINT('Ctrl Pts',(-16.6263536592911,19.4110650139397,
-13.675020974006));
#104952=CARTESIAN_POINT('Ctrl Pts',(-16.628608071998,19.4335398814456,-13.673642563196));
#104953=CARTESIAN_POINT('Ctrl Pts',(-16.6323187098712,19.4653906668255,
-13.6717016683274));
#104954=CARTESIAN_POINT('Ctrl Pts',(-16.6334788743084,19.4747989039789,
-13.6711299140231));
#104955=CARTESIAN_POINT('Ctrl Pts',(-16.635470666768,19.4901040960875,-13.6702022466815));
#104956=CARTESIAN_POINT('Ctrl Pts',(-16.6362640432706,19.4960058172362,
-13.6698451310404));
#104957=CARTESIAN_POINT('Ctrl Pts',(-16.6379803606692,19.5083775079965,
-13.6690977341825));
#104958=CARTESIAN_POINT('Ctrl Pts',(-16.6389083829206,19.5148467183352,
-13.6687076178036));
#104959=CARTESIAN_POINT('Ctrl Pts',(-16.641194218732,19.5302726512531,-13.6677790026042));
#104960=CARTESIAN_POINT('Ctrl Pts',(-16.6425796019414,19.5392252068562,
-13.6672413821677));
#104961=CARTESIAN_POINT('Ctrl Pts',(-16.647475947128,19.5695757453257,-13.6654230010135));
#104962=CARTESIAN_POINT('Ctrl Pts',(-16.6512582543336,19.5909290204605,
-13.6641508429832));
#104963=CARTESIAN_POINT('Ctrl Pts',(-16.6739143739679,19.7083050591278,
-13.6571919846735));
#104964=CARTESIAN_POINT('Ctrl Pts',(-16.6991014204847,19.8029933598678,
-13.6517118025733));
#104965=CARTESIAN_POINT('Ctrl Pts',(-16.7845100294689,20.0529092843735,
-13.6372003899247));
#104966=CARTESIAN_POINT('Ctrl Pts',(-16.8566009285505,20.2033124793429,
-13.6284399588336));
#104967=CARTESIAN_POINT('Ctrl Pts',(-16.965822299614,20.3757640498268,-13.6167945096372));
#104968=CARTESIAN_POINT('Ctrl Pts',(-16.9869731290592,20.4072543143438,
-13.6145932087564));
#104969=CARTESIAN_POINT('Ctrl Pts',(-17.0131367931583,20.4440331797615,
-13.6119102370081));
#104970=CARTESIAN_POINT('Ctrl Pts',(-17.0173467283316,20.4498876222483,
-13.6114796956935));
#104971=CARTESIAN_POINT('Ctrl Pts',(-17.0242519025832,20.4593873578055,
-13.6107752057976));
#104972=CARTESIAN_POINT('Ctrl Pts',(-17.0269291255608,20.4630457581544,
-13.6105024729501));
#104973=CARTESIAN_POINT('Ctrl Pts',(-17.0317342109016,20.4695678017357,
-13.610013639717));
#104974=CARTESIAN_POINT('Ctrl Pts',(-17.0338575797378,20.4724346906857,
-13.6097978523477));
#104975=CARTESIAN_POINT('Ctrl Pts',(-17.0384623229055,20.478619086361,-13.6093303728619));
#104976=CARTESIAN_POINT('Ctrl Pts',(-17.0409461565695,20.4819346344795,
-13.609078513066));
#104977=CARTESIAN_POINT('Ctrl Pts',(-17.0478880593633,20.4911445786532,
-13.6083754951136));
#104978=CARTESIAN_POINT('Ctrl Pts',(-17.0523672361996,20.4970228857299,
-13.6079228931589));
#104979=CARTESIAN_POINT('Ctrl Pts',(-17.0781160324881,20.5304501241866,
-13.605327403509));
#104980=CARTESIAN_POINT('Ctrl Pts',(-17.1000303869053,20.55749297156,-13.6031428598908));
#104981=CARTESIAN_POINT('Ctrl Pts',(-17.1716866032175,20.6415923157882,
-13.5961074696339));
#104982=CARTESIAN_POINT('Ctrl Pts',(-17.2238244848166,20.6965254523574,
-13.5911459833851));
#104983=CARTESIAN_POINT('Ctrl Pts',(-17.4185998537363,20.8808709963673,
-13.5734542658346));
#104984=CARTESIAN_POINT('Ctrl Pts',(-17.5758436885065,20.993540735882,-13.5607397498693));
#104985=CARTESIAN_POINT('Ctrl Pts',(-17.7650385167635,21.0933542291536,
-13.5475951513949));
#104986=CARTESIAN_POINT('Ctrl Pts',(-17.7840503645629,21.1030199635231,
-13.5462947035357));
#104987=CARTESIAN_POINT('Ctrl Pts',(-17.81068968032,21.1160607570359,-13.5445001456819));
#104988=CARTESIAN_POINT('Ctrl Pts',(-17.8181954248019,21.1196802816547,
-13.5439975280646));
#104989=CARTESIAN_POINT('Ctrl Pts',(-17.8311827020417,21.1258489411309,
-13.5431329578895));
#104990=CARTESIAN_POINT('Ctrl Pts',(-17.836654101312,21.1284190674262,-13.5427702793366));
#104991=CARTESIAN_POINT('Ctrl Pts',(-17.8480021265544,21.1336904582237,
-13.5420212440518));
#104992=CARTESIAN_POINT('Ctrl Pts',(-17.8538802796671,21.136388300891,-13.5416350086013));
#104993=CARTESIAN_POINT('Ctrl Pts',(-17.8676672067033,21.1426396311931,
-13.5407331680261));
#104994=CARTESIAN_POINT('Ctrl Pts',(-17.8755856676788,21.1461715714667,
-13.5402183079099));
#104995=CARTESIAN_POINT('Ctrl Pts',(-17.901332332674,21.1574664533431,-13.5385541310275));
#104996=CARTESIAN_POINT('Ctrl Pts',(-17.9192461697134,21.1650325819966,
-13.537411530066));
#104997=CARTESIAN_POINT('Ctrl Pts',(-18.0112101433606,21.2023900855222,
-13.5316196923666));
#104998=CARTESIAN_POINT('Ctrl Pts',(-18.0868022542763,21.2282250056676,
-13.527104866799));
#104999=CARTESIAN_POINT('Ctrl Pts',(-18.3235024776175,21.2944401897104,
-13.5134723877485));
#105000=CARTESIAN_POINT('Ctrl Pts',(-18.4880137295316,21.3201978023287,
-13.5047300554365));
#105001=CARTESIAN_POINT('Ctrl Pts',(-18.7116111523022,21.3286710825945,
-13.4921915777757));
#105002=CARTESIAN_POINT('Ctrl Pts',(-18.7694491256858,21.3284924244502,
-13.4888843237578));
#105003=CARTESIAN_POINT('Ctrl Pts',(-18.8360826012219,21.3255560220886,
-13.4849275967332));
#105004=CARTESIAN_POINT('Ctrl Pts',(-18.844961023476,21.3251087183569,-13.4843973792927));
#105005=CARTESIAN_POINT('Ctrl Pts',(-18.8583485193683,21.3243496805579,
-13.4835929834094));
#105006=CARTESIAN_POINT('Ctrl Pts',(-18.8628599713676,21.3240793959273,
-13.4833210704686));
#105007=CARTESIAN_POINT('Ctrl Pts',(-18.8709299673567,21.3235699762403,
-13.4828331206923));
#105008=CARTESIAN_POINT('Ctrl Pts',(-18.8744888027043,21.3233362934241,
-13.482617392214));
#105009=CARTESIAN_POINT('Ctrl Pts',(-18.8821901688445,21.3228110518978,
-13.4821493606945));
#105010=CARTESIAN_POINT('Ctrl Pts',(-18.8863323802574,21.322516301216,-13.4818968863199));
#105011=CARTESIAN_POINT('Ctrl Pts',(-18.8978892799454,21.321659754074,-13.4811904555982));
#105012=CARTESIAN_POINT('Ctrl Pts',(-18.9053018304987,21.3210710823677,
-13.4807350330425));
#105013=CARTESIAN_POINT('Ctrl Pts',(-18.9481185441162,21.3174436715999,
-13.4780915854121));
#105014=CARTESIAN_POINT('Ctrl Pts',(-18.9834426064714,21.3135531465626,
-13.4758601188409));
#105015=CARTESIAN_POINT('Ctrl Pts',(-19.096255821416,21.2982453979133,-13.4686060143291));
#105016=CARTESIAN_POINT('Ctrl Pts',(-19.1732129525762,21.2834171772923,
-13.4634655010647));
#105017=CARTESIAN_POINT('Ctrl Pts',(-19.4318699454908,21.2185229676173,
-13.4458644097813));
#105018=CARTESIAN_POINT('Ctrl Pts',(-19.607682314076,21.1484929743937,-13.4334408226361));
#105019=CARTESIAN_POINT('Ctrl Pts',(-19.7909251529856,21.0454136871527,
-13.4205151030088));
#105020=CARTESIAN_POINT('Ctrl Pts',(-19.8097618252229,21.0344310806344,
-13.4191851636067));
#105021=CARTESIAN_POINT('Ctrl Pts',(-19.8362649764433,21.0184249039051,
-13.4173115756307));
#105022=CARTESIAN_POINT('Ctrl Pts',(-19.8440732020395,21.0136398286361,
-13.4167592887449));
#105023=CARTESIAN_POINT('Ctrl Pts',(-19.857337529036,21.0053922501973,-13.4158204933659));
#105024=CARTESIAN_POINT('Ctrl Pts',(-19.8628092252545,21.0019551881963,
-13.41543305558));
#105025=CARTESIAN_POINT('Ctrl Pts',(-19.8737393797323,20.9950193889556,
-13.4146587325803));
#105026=CARTESIAN_POINT('Ctrl Pts',(-19.8791976724626,20.9915205211706,
-13.4142718577985));
#105027=CARTESIAN_POINT('Ctrl Pts',(-19.8901575575369,20.9844237824799,
-13.4134946063724));
#105028=CARTESIAN_POINT('Ctrl Pts',(-19.8956586381718,20.9808252512499,
-13.4131042599969));
#105029=CARTESIAN_POINT('Ctrl Pts',(-19.9156418476291,20.9676199254016,
-13.4116853938145));
#105030=CARTESIAN_POINT('Ctrl Pts',(-19.930022557703,20.9578603512038,-13.4106626064586));
#105031=CARTESIAN_POINT('Ctrl Pts',(-19.9629011623044,20.9349506769682,
-13.4083190648746));
#105032=CARTESIAN_POINT('Ctrl Pts',(-19.9813111987015,20.9216778869677,
-13.4070029965833));
#105033=CARTESIAN_POINT('Ctrl Pts',(-20.043425193603,20.8753606191372,-13.4025447853776));
#105034=CARTESIAN_POINT('Ctrl Pts',(-20.0860597034314,20.8409158881622,
-13.3994544338268));
#105035=CARTESIAN_POINT('Ctrl Pts',(-20.2094383406355,20.7330609753651,
-13.3903400574244));
#105036=CARTESIAN_POINT('Ctrl Pts',(-20.2858949755795,20.6550259029552,
-13.3844648581662));
#105037=CARTESIAN_POINT('Ctrl Pts',(-20.4326298357147,20.48008075314,-13.3720352395967));
#105038=CARTESIAN_POINT('Ctrl Pts',(-20.5013951255844,20.3824160193898,
-13.3654876689711));
#105039=CARTESIAN_POINT('Ctrl Pts',(-20.5663658998535,20.2712898997211,
-13.3578588092128));
#105040=CARTESIAN_POINT('Ctrl Pts',(-20.5711109271987,20.2630470027188,
-13.3572918904577));
#105041=CARTESIAN_POINT('Ctrl Pts',(-20.5780600881861,20.2507847859239,
-13.3564465772265));
#105042=CARTESIAN_POINT('Ctrl Pts',(-20.5803070459711,20.246789699201,-13.3561708643815));
#105043=CARTESIAN_POINT('Ctrl Pts',(-20.5842819781142,20.2396682466034,
-13.3556787914355));
#105044=CARTESIAN_POINT('Ctrl Pts',(-20.5860150316978,20.2365447733964,
-13.3554627612576));
#105045=CARTESIAN_POINT('Ctrl Pts',(-20.5897243136761,20.2298194882414,
-13.3549971575745));
#105046=CARTESIAN_POINT('Ctrl Pts',(-20.59169793634,20.2262163585386,-13.3547474291575));
#105047=CARTESIAN_POINT('Ctrl Pts',(-20.5971174093858,20.2162536185894,
-13.3540562087744));
#105048=CARTESIAN_POINT('Ctrl Pts',(-20.6005411355865,20.2098821274447,
-13.3536133492945));
#105049=CARTESIAN_POINT('Ctrl Pts',(-20.6191285946934,20.1748619561541,
-13.3511753636231));
#105050=CARTESIAN_POINT('Ctrl Pts',(-20.6336645794219,20.1458871099919,
-13.3491441730077));
#105051=CARTESIAN_POINT('Ctrl Pts',(-20.7171728107169,19.9694330184984,
-13.3367407938375));
#105052=CARTESIAN_POINT('Ctrl Pts',(-20.7696074828148,19.8147359774947,
-13.3257767183171));
#105053=CARTESIAN_POINT('Ctrl Pts',(-20.8169122812128,19.5944926868546,
-13.3110623029466));
#105054=CARTESIAN_POINT('Ctrl Pts',(-20.8273203164416,19.5328715338825,
-13.3070312374439));
#105055=CARTESIAN_POINT('Ctrl Pts',(-20.838240896145,19.4445832687708,-13.3013963914024));
#105056=CARTESIAN_POINT('Ctrl Pts',(-20.8409993766864,19.4182308218197,
-13.2997319479751));
#105057=CARTESIAN_POINT('Ctrl Pts',(-20.8463154919444,19.3562227468594,
-13.2958566623018));
#105058=CARTESIAN_POINT('Ctrl Pts',(-20.8484662878358,19.3205396989405,
-13.2936585268251));
#105059=CARTESIAN_POINT('Ctrl Pts',(-20.8501018463093,19.2736623165284,
-13.2908109024725));
#105060=CARTESIAN_POINT('Ctrl Pts',(-20.8504028278496,19.2625040543427,
-13.2901360432393));
#105061=CARTESIAN_POINT('Ctrl Pts',(-20.8507477574777,19.2444074923976,
-13.2890462302954));
#105062=CARTESIAN_POINT('Ctrl Pts',(-20.8508458708876,19.237470550147,-13.2886295872446));
#105063=CARTESIAN_POINT('Ctrl Pts',(-20.8509497984026,19.2262074011857,
-13.2879548791866));
#105064=CARTESIAN_POINT('Ctrl Pts',(-20.8509764542477,19.2218814795907,
-13.287696163653));
#105065=CARTESIAN_POINT('Ctrl Pts',(-20.8509965706155,19.2153852145476,
-13.287308277758));
#105066=CARTESIAN_POINT('Ctrl Pts',(-20.8509999537594,19.2132149334439,
-13.2871787977096));
#105067=CARTESIAN_POINT('Ctrl Pts',(-20.8509999995292,19.2110446460074,
-13.2870494219157));
#105068=CARTESIAN_POINT('Ctrl Pts',(-20.8509999986719,19.2109250126718,
-13.2890562789747));
#105069=CARTESIAN_POINT('Ctrl Pts',(-20.8509972774554,19.1341011600837,
-13.2844612169106));
#105070=CARTESIAN_POINT('Ctrl Pts',(-20.8468084619602,19.0573628290618,
-13.2798661548465));
#105071=CARTESIAN_POINT('Ctrl Pts',(-20.8384871131119,18.9811674723936,
-13.2752710927824));
#105072=CARTESIAN_POINT('Ctrl Pts',(-20.8301538008465,18.9048625713658,
-13.2706694245004));
#105073=CARTESIAN_POINT('Ctrl Pts',(-20.8176761741998,18.8291026018815,
-13.2660677562184));
#105074=CARTESIAN_POINT('Ctrl Pts',(-20.8011589270513,18.7543349473497,
-13.2614660879363));
#105075=CARTESIAN_POINT('Ctrl Pts',(-20.7846027399158,18.679391025461,-13.2568535710606));
#105076=CARTESIAN_POINT('Ctrl Pts',(-20.763988012731,18.6054444843118,-13.2522410541849));
#105077=CARTESIAN_POINT('Ctrl Pts',(-20.7394693419458,18.5329279400275,
-13.2476285373092));
#105078=CARTESIAN_POINT('Ctrl Pts',(-20.734030977206,18.5168434050645,-13.2466054578218));
#105079=CARTESIAN_POINT('Ctrl Pts',(-20.7284007341625,18.5008291398821,
-13.2455823783344));
#105080=CARTESIAN_POINT('Ctrl Pts',(-20.7225806137986,18.4848897174502,
-13.2445592988469));
#105081=CARTESIAN_POINT('Origin',(-18.734,19.211,0.));
#105082=CARTESIAN_POINT('',(-20.7242505411024,18.4842642021379,-12.4443820858314));
#105083=CARTESIAN_POINT('',(-20.7225805288028,18.4848894846743,-12.6679318969538));
#105084=CARTESIAN_POINT('',(-20.7225806137986,18.4848897174502,0.));
#105085=CARTESIAN_POINT('Ctrl Pts',(-20.7225805288028,18.4848894846743,
-12.6679318969538));
#105086=CARTESIAN_POINT('Ctrl Pts',(-20.7627961214462,18.5950269125135,
-12.6745735586325));
#105087=CARTESIAN_POINT('Ctrl Pts',(-20.7938157091376,18.7083782681631,
-12.6809438446479));
#105088=CARTESIAN_POINT('Ctrl Pts',(-20.8390879891312,18.9517192360552,
-12.6943852386175));
#105089=CARTESIAN_POINT('Ctrl Pts',(-20.8510398088253,19.0815565850429,
-12.7014276439781));
#105090=CARTESIAN_POINT('Ctrl Pts',(-20.8509988957047,19.2149244778125,
-12.7092186304204));
#105091=CARTESIAN_POINT('Ctrl Pts',(-20.8509902911661,19.218199498468,-12.7094102988555));
#105092=CARTESIAN_POINT('Ctrl Pts',(-20.8508966099817,19.2371332231321,
-12.7105204774892));
#105093=CARTESIAN_POINT('Ctrl Pts',(-20.8506454015414,19.2527901243868,
-12.7114468030206));
#105094=CARTESIAN_POINT('Ctrl Pts',(-20.8500635586938,19.2742256918366,
-12.7127281078718));
#105095=CARTESIAN_POINT('Ctrl Pts',(-20.849882869319,19.2800083623479,-12.7130750707398));
#105096=CARTESIAN_POINT('Ctrl Pts',(-20.8495580050343,19.2891981881347,
-12.7136286418556));
#105097=CARTESIAN_POINT('Ctrl Pts',(-20.8494292955161,19.292605910229,-12.713834390178));
#105098=CARTESIAN_POINT('Ctrl Pts',(-20.8491463964198,19.2996449787777,
-12.7142603993217));
#105099=CARTESIAN_POINT('Ctrl Pts',(-20.8489910889964,19.303276233328,-12.7144807243681));
#105100=CARTESIAN_POINT('Ctrl Pts',(-20.8485986103281,19.311930701008,-12.7150071394247));
#105101=CARTESIAN_POINT('Ctrl Pts',(-20.8483528906747,19.3169534884063,
-12.7153137043087));
#105102=CARTESIAN_POINT('Ctrl Pts',(-20.8474631220289,19.3339036609023,
-12.7163516895652));
#105103=CARTESIAN_POINT('Ctrl Pts',(-20.8467360360084,19.345826203305,-12.7170875375017));
#105104=CARTESIAN_POINT('Ctrl Pts',(-20.8368854509554,19.4875959922649,
-12.7259006911209));
#105105=CARTESIAN_POINT('Ctrl Pts',(-20.8159065091064,19.6163281873859,
-12.7345181394112));
#105106=CARTESIAN_POINT('Ctrl Pts',(-20.7425052049445,19.8994378314436,
-12.7538447946671));
#105107=CARTESIAN_POINT('Ctrl Pts',(-20.6838198863416,20.0513933538053,
-12.7644508258067));
#105108=CARTESIAN_POINT('Ctrl Pts',(-20.5973016052834,20.2161660124741,
-12.7759141602397));
#105109=CARTESIAN_POINT('Ctrl Pts',(-20.5859225279541,20.2369798278505,
-12.7773627919499));
#105110=CARTESIAN_POINT('Ctrl Pts',(-20.5694165603161,20.2660016587093,
-12.7793842980244));
#105111=CARTESIAN_POINT('Ctrl Pts',(-20.5645798741583,20.2743718911735,
-12.7799675185626));
#105112=CARTESIAN_POINT('Ctrl Pts',(-20.5566541592534,20.287873568392,-12.7809086898092));
#105113=CARTESIAN_POINT('Ctrl Pts',(-20.5536004316783,20.2930254787789,
-12.7812679136698));
#105114=CARTESIAN_POINT('Ctrl Pts',(-20.5471836319514,20.3037472023617,
-12.7820157309393));
#105115=CARTESIAN_POINT('Ctrl Pts',(-20.543816658123,20.3093146165302,-12.7824041769744));
#105116=CARTESIAN_POINT('Ctrl Pts',(-20.5357844682834,20.3224589063981,
-12.7833216308878));
#105117=CARTESIAN_POINT('Ctrl Pts',(-20.5310970210085,20.3300221050202,
-12.783849816171));
#105118=CARTESIAN_POINT('Ctrl Pts',(-20.5153276311569,20.3551113721179,
-12.7856031001709));
#105119=CARTESIAN_POINT('Ctrl Pts',(-20.5040356777052,20.3725045010785,
-12.7868204231206));
#105120=CARTESIAN_POINT('Ctrl Pts',(-20.442393710235,20.4644651884676,-12.7932713762075));
#105121=CARTESIAN_POINT('Ctrl Pts',(-20.3875813317937,20.535936038902,-12.7983320606583));
#105122=CARTESIAN_POINT('Ctrl Pts',(-20.2392359525445,20.7057627660624,
-12.8107690126813));
#105123=CARTESIAN_POINT('Ctrl Pts',(-20.1405024887274,20.7990174772575,
-12.8179812878458));
#105124=CARTESIAN_POINT('Ctrl Pts',(-19.9740205527178,20.9284755678176,
-12.8296571181667));
#105125=CARTESIAN_POINT('Ctrl Pts',(-19.912079634336,20.9715394382112,-12.8339176887515));
#105126=CARTESIAN_POINT('Ctrl Pts',(-19.839912426887,21.0161971525049,-12.8389475073708));
#105127=CARTESIAN_POINT('Ctrl Pts',(-19.8318094457829,21.0211363121381,
-12.8395131656306));
#105128=CARTESIAN_POINT('Ctrl Pts',(-19.8197474895229,21.0283778804483,
-12.8403569549728));
#105129=CARTESIAN_POINT('Ctrl Pts',(-19.8158136803405,21.0307222676749,
-12.8406324184359));
#105130=CARTESIAN_POINT('Ctrl Pts',(-19.8087982317679,21.0348723963692,
-12.8411242186081));
#105131=CARTESIAN_POINT('Ctrl Pts',(-19.8057195989282,21.0366831209964,
-12.8413402268077));
#105132=CARTESIAN_POINT('Ctrl Pts',(-19.7990874991308,21.0405612917087,
-12.8418059799307));
#105133=CARTESIAN_POINT('Ctrl Pts',(-19.7955326400418,21.0426261502789,
-12.842055880805));
#105134=CARTESIAN_POINT('Ctrl Pts',(-19.7856956750312,21.0483017470527,
-12.8427480536842));
#105135=CARTESIAN_POINT('Ctrl Pts',(-19.7794010801632,21.0518905672797,
-12.8431916992939));
#105136=CARTESIAN_POINT('Ctrl Pts',(-19.7446853690071,21.0714480227753,
-12.8456419493298));
#105137=CARTESIAN_POINT('Ctrl Pts',(-19.7159183900048,21.086789904366,-12.8476850385778));
#105138=CARTESIAN_POINT('Ctrl Pts',(-19.5415656814313,21.1746653762207,
-12.8600924188335));
#105139=CARTESIAN_POINT('Ctrl Pts',(-19.3883725996815,21.2308862539321,
-12.8710455923524));
#105140=CARTESIAN_POINT('Ctrl Pts',(-19.1167165575343,21.2963914460537,
-12.8892984491996));
#105141=CARTESIAN_POINT('Ctrl Pts',(-19.0010936239427,21.3143302748905,
-12.8967380038184));
#105142=CARTESIAN_POINT('Ctrl Pts',(-18.8703108366637,21.3236553277636,
-12.904743864424));
#105143=CARTESIAN_POINT('Ctrl Pts',(-18.8560477411838,21.3245272751275,
-12.9056118247965));
#105144=CARTESIAN_POINT('Ctrl Pts',(-18.8333331545337,21.325685177977,-12.90698611335));
#105145=CARTESIAN_POINT('Ctrl Pts',(-18.8248870821312,21.3260650153331,
-12.907495369466));
#105146=CARTESIAN_POINT('Ctrl Pts',(-18.8099870549081,21.3266456831299,
-12.9083907423932));
#105147=CARTESIAN_POINT('Ctrl Pts',(-18.8035340746435,21.3268676005261,
-12.9087775153074));
#105148=CARTESIAN_POINT('Ctrl Pts',(-18.7901850990114,21.3272655358598,
-12.9095755850914));
#105149=CARTESIAN_POINT('Ctrl Pts',(-18.7832890487378,21.327437378007,-12.9099867465678));
#105150=CARTESIAN_POINT('Ctrl Pts',(-18.7655855976869,21.3277919548024,
-12.9110394661193));
#105151=CARTESIAN_POINT('Ctrl Pts',(-18.7547773300265,21.3279256337938,
-12.9116794828368));
#105152=CARTESIAN_POINT('Ctrl Pts',(-18.7096624265858,21.3281380695596,
-12.9143402249152));
#105153=CARTESIAN_POINT('Ctrl Pts',(-18.6753563225963,21.3274656951576,
-12.9163374198074));
#105154=CARTESIAN_POINT('Ctrl Pts',(-18.5860257135005,21.3235409957281,
-12.9214817082814));
#105155=CARTESIAN_POINT('Ctrl Pts',(-18.5310841572953,21.3189733523813,
-12.9245894086367));
#105156=CARTESIAN_POINT('Ctrl Pts',(-18.3678444128874,21.2989598160033,
-12.9337340658193));
#105157=CARTESIAN_POINT('Ctrl Pts',(-18.2604996768575,21.2772633991256,
-12.9396222940831));
#105158=CARTESIAN_POINT('Ctrl Pts',(-18.1111192258013,21.2348130471402,
-12.9480772179085));
#105159=CARTESIAN_POINT('Ctrl Pts',(-18.0673482912213,21.220819635332,-12.9505893087198));
#105160=CARTESIAN_POINT('Ctrl Pts',(-18.0030685432172,21.197938622132,-12.954373240686));
#105161=CARTESIAN_POINT('Ctrl Pts',(-17.9821883216845,21.1901323943882,
-12.9556176305286));
#105162=CARTESIAN_POINT('Ctrl Pts',(-17.9135820707828,21.1632410778597,
-12.9597685686341));
#105163=CARTESIAN_POINT('Ctrl Pts',(-17.8664314071896,21.1427491089816,
-12.9627219879601));
#105164=CARTESIAN_POINT('Ctrl Pts',(-17.8129719811901,21.1171632770823,
-12.9662396476612));
#105165=CARTESIAN_POINT('Ctrl Pts',(-17.8058857934373,21.1137230659092,
-12.9667094290941));
#105166=CARTESIAN_POINT('Ctrl Pts',(-17.7946183712581,21.1081750261986,
-12.9674622714523));
#105167=CARTESIAN_POINT('Ctrl Pts',(-17.7904245675576,21.1060926960909,
-12.9677437872589));
#105168=CARTESIAN_POINT('Ctrl Pts',(-17.7830248567056,21.1023878996941,
-12.9682428720952));
#105169=CARTESIAN_POINT('Ctrl Pts',(-17.7798161289571,21.1007711634908,
-12.9684600812003));
#105170=CARTESIAN_POINT('Ctrl Pts',(-17.7730410488711,21.0973358449092,
-12.9689204059536));
#105171=CARTESIAN_POINT('Ctrl Pts',(-17.7694757900858,21.0955153417838,
-12.969163636482));
#105172=CARTESIAN_POINT('Ctrl Pts',(-17.7599052790968,21.0905941456448,
-12.9698191897808));
#105173=CARTESIAN_POINT('Ctrl Pts',(-17.7539097354699,21.0874748194837,
-12.9702326604402));
#105174=CARTESIAN_POINT('Ctrl Pts',(-17.7247052097881,21.0721023148026,
-12.9722599812006));
#105175=CARTESIAN_POINT('Ctrl Pts',(-17.7017116378027,21.0594475622684,
-12.9738972755162));
#105176=CARTESIAN_POINT('Ctrl Pts',(-17.6365240884844,21.0219753017653,
-12.9786453038926));
#105177=CARTESIAN_POINT('Ctrl Pts',(-17.5949491518425,20.9961183301519,
-12.9818036102215));
#105178=CARTESIAN_POINT('Ctrl Pts',(-17.4740587952986,20.9149888710586,
-12.9913040435502));
#105179=CARTESIAN_POINT('Ctrl Pts',(-17.3975903533404,20.855700267134,-12.9977329730545));
#105180=CARTESIAN_POINT('Ctrl Pts',(-17.2201680483101,20.697569037905,-13.013368531114));
#105181=CARTESIAN_POINT('Ctrl Pts',(-17.1245175066716,20.5934449851206,
-13.0224360754053));
#105182=CARTESIAN_POINT('Ctrl Pts',(-17.0313564972683,20.46913277953,-13.0319214321291));
#105183=CARTESIAN_POINT('Ctrl Pts',(-17.0229070541902,20.4576169960404,
-13.0327889835561));
#105184=CARTESIAN_POINT('Ctrl Pts',(-17.0096436019779,20.439151235634,-13.0341627490327));
#105185=CARTESIAN_POINT('Ctrl Pts',(-17.004753675755,20.4322565653094,-13.0346718875507));
#105186=CARTESIAN_POINT('Ctrl Pts',(-16.9962016666346,20.4200441007411,
-13.0355671237013));
#105187=CARTESIAN_POINT('Ctrl Pts',(-16.9925223968725,20.4147385281789,
-13.0359538768059));
#105188=CARTESIAN_POINT('Ctrl Pts',(-16.9849620308511,20.4037291297265,
-13.0367519727492));
#105189=CARTESIAN_POINT('Ctrl Pts',(-16.9810844247459,20.3980229914313,
-13.037163179864));
#105190=CARTESIAN_POINT('Ctrl Pts',(-16.9712013907032,20.3833254539917,
-13.0382161550684));
#105191=CARTESIAN_POINT('Ctrl Pts',(-16.9652367807699,20.3743067471134,
-13.0388563803305));
#105192=CARTESIAN_POINT('Ctrl Pts',(-16.9406198273755,20.3364579564063,
-13.0415191501685));
#105193=CARTESIAN_POINT('Ctrl Pts',(-16.9226005855232,20.3072209693176,
-13.043518118474));
#105194=CARTESIAN_POINT('Ctrl Pts',(-16.8775016175344,20.2298950776539,
-13.0486680082594));
#105195=CARTESIAN_POINT('Ctrl Pts',(-16.8515761765729,20.1811621616415,
-13.0517794239177));
#105196=CARTESIAN_POINT('Ctrl Pts',(-16.7800136370308,20.032946388887,-13.0609305621458));
#105197=CARTESIAN_POINT('Ctrl Pts',(-16.74015199032,19.9308816318834,-13.0668215778965));
#105198=CARTESIAN_POINT('Ctrl Pts',(-16.6935657544593,19.777487575627,-13.0755499526949));
#105199=CARTESIAN_POINT('Ctrl Pts',(-16.6805355722498,19.728265481387,-13.0783345928624));
#105200=CARTESIAN_POINT('Ctrl Pts',(-16.6658182735494,19.6632838928989,
-13.0820414583301));
#105201=CARTESIAN_POINT('Ctrl Pts',(-16.6625152114379,19.647906313448,-13.0829209167307));
#105202=CARTESIAN_POINT('Ctrl Pts',(-16.6488821001186,19.5808033483538,
-13.0867737226768));
#105203=CARTESIAN_POINT('Ctrl Pts',(-16.6403167630758,19.5287431160823,
-13.0898016714684));
#105204=CARTESIAN_POINT('Ctrl Pts',(-16.632614976478,19.4677986341198,-13.0934472666022));
#105205=CARTESIAN_POINT('Ctrl Pts',(-16.6315783128438,19.4591684892992,
-13.0939658525503));
#105206=CARTESIAN_POINT('Ctrl Pts',(-16.6300882631347,19.4460839187503,
-13.0947559865968));
#105207=CARTESIAN_POINT('Ctrl Pts',(-16.6295957988882,19.4416339152661,
-13.0950253868715));
#105208=CARTESIAN_POINT('Ctrl Pts',(-16.6287367224732,19.4336392405892,
-13.095510652212));
#105209=CARTESIAN_POINT('Ctrl Pts',(-16.6283649410985,19.4300951792643,
-13.0957262232256));
#105210=CARTESIAN_POINT('Ctrl Pts',(-16.6275760431037,19.4223873790919,
-13.0961960507659));
#105211=CARTESIAN_POINT('Ctrl Pts',(-16.6271623281281,19.4182233913149,
-13.0964504902343));
#105212=CARTESIAN_POINT('Ctrl Pts',(-16.6260337072185,19.4065111162331,
-13.0971678686295));
#105213=CARTESIAN_POINT('Ctrl Pts',(-16.6253470121466,19.3989602641437,
-13.0976323467011));
#105214=CARTESIAN_POINT('Ctrl Pts',(-16.6214621588144,19.3535387328608,
-13.1004376574194));
#105215=CARTESIAN_POINT('Ctrl Pts',(-16.6192439488305,19.3155937351445,
-13.1028282446724));
#105216=CARTESIAN_POINT('Ctrl Pts',(-16.6152879465656,19.1899309489021,
-13.1108564482069));
#105217=CARTESIAN_POINT('Ctrl Pts',(-16.6179805452626,19.1021680075429,
-13.1166390515131));
#105218=CARTESIAN_POINT('Ctrl Pts',(-16.6422709220074,18.8411604074901,
-13.1339594037061));
#105219=CARTESIAN_POINT('Ctrl Pts',(-16.6798383629085,18.6701165724637,
-13.1454065499973));
#105220=CARTESIAN_POINT('Ctrl Pts',(-16.7456645979487,18.4838525846326,
-13.1575672194748));
#105221=CARTESIAN_POINT('Ctrl Pts',(-16.7537054574057,18.4622312604318,
-13.1589753793716));
#105222=CARTESIAN_POINT('Ctrl Pts',(-16.7655760968725,18.4318416712428,
-13.1609504102105));
#105223=CARTESIAN_POINT('Ctrl Pts',(-16.7691141661991,18.4229619117763,
-13.1615270009044));
#105224=CARTESIAN_POINT('Ctrl Pts',(-16.7749591997906,18.4085763136206,
-13.1624603584571));
#105225=CARTESIAN_POINT('Ctrl Pts',(-16.777229494256,18.4030558074147,-13.1628183575218));
#105226=CARTESIAN_POINT('Ctrl Pts',(-16.782029416633,18.3915231024568,-13.1635658960731));
#105227=CARTESIAN_POINT('Ctrl Pts',(-16.7845635461611,18.3855128360478,
-13.1639552782064));
#105228=CARTESIAN_POINT('Ctrl Pts',(-16.7906560120549,18.3712476872335,
-13.1648790412546));
#105229=CARTESIAN_POINT('Ctrl Pts',(-16.7942392456181,18.3630035248689,
-13.1654125680824));
#105230=CARTESIAN_POINT('Ctrl Pts',(-16.8064770418231,18.3353307669333,
-13.1672024943917));
#105231=CARTESIAN_POINT('Ctrl Pts',(-16.8153720255238,18.3160094390806,
-13.1684506581482));
#105232=CARTESIAN_POINT('Ctrl Pts',(-16.8912559679692,18.1575101867887,
-13.1786845740511));
#105233=CARTESIAN_POINT('Ctrl Pts',(-16.9730017473837,18.0259097224612,
-13.1871018353607));
#105234=CARTESIAN_POINT('Ctrl Pts',(-17.1527681058354,17.7967505041328,
-13.2029185394502));
#105235=CARTESIAN_POINT('Ctrl Pts',(-17.2474049029209,17.6975864496225,
-13.2103041823479));
#105236=CARTESIAN_POINT('Ctrl Pts',(-17.3627251652693,17.5980718354622,
-13.2192364398674));
#105237=CARTESIAN_POINT('Ctrl Pts',(-17.3746370899476,17.5880199067183,
-13.2201585438136));
#105238=CARTESIAN_POINT('Ctrl Pts',(-17.3911125781449,17.5744256150461,
-13.221434895136));
#105239=CARTESIAN_POINT('Ctrl Pts',(-17.3955815924742,17.5707687632893,
-13.2217812058135));
#105240=CARTESIAN_POINT('Ctrl Pts',(-17.4027118081886,17.5649828783026,
-13.2223339932691));
#105241=CARTESIAN_POINT('Ctrl Pts',(-17.4053633239805,17.5628418773269,
-13.2225396144794));
#105242=CARTESIAN_POINT('Ctrl Pts',(-17.4108544057981,17.5584298934262,
-13.2229655825414));
#105243=CARTESIAN_POINT('Ctrl Pts',(-17.4136946484201,17.5561598269292,
-13.2231859946132));
#105244=CARTESIAN_POINT('Ctrl Pts',(-17.4204832692697,17.5507626172451,
-13.2237129833849));
#105245=CARTESIAN_POINT('Ctrl Pts',(-17.4244369748889,17.5476422359986,
-13.2240200376908));
#105246=CARTESIAN_POINT('Ctrl Pts',(-17.4378411420571,17.5371406843449,
-13.2250613832602));
#105247=CARTESIAN_POINT('Ctrl Pts',(-17.4473429689936,17.5298258677562,
-13.2258001403894));
#105248=CARTESIAN_POINT('Ctrl Pts',(-17.5586203541307,17.4456568204853,
-13.2344534853721));
#105249=CARTESIAN_POINT('Ctrl Pts',(-17.6670681667437,17.3780778595741,
-13.2428870751563));
#105250=CARTESIAN_POINT('Ctrl Pts',(-17.9283053822837,17.2463655514479,
-13.2622208253673));
#105251=CARTESIAN_POINT('Ctrl Pts',(-18.0839003419188,17.1895345787758,
-13.2730160026197));
#105252=CARTESIAN_POINT('Ctrl Pts',(-18.2675081190578,17.1459015602301,
-13.2846391316875));
#105253=CARTESIAN_POINT('Ctrl Pts',(-18.2905648462791,17.1408281288342,
-13.2860807622327));
#105254=CARTESIAN_POINT('Ctrl Pts',(-18.3231583579266,17.1342257633574,
-13.2880942222899));
#105255=CARTESIAN_POINT('Ctrl Pts',(-18.3326274551369,17.1323749328234,
-13.2886762884125));
#105256=CARTESIAN_POINT('Ctrl Pts',(-18.3479909466912,17.1294808826901,
-13.2896160980607));
#105257=CARTESIAN_POINT('Ctrl Pts',(-18.3538776135144,17.1283978302616,
-13.289975107578));
#105258=CARTESIAN_POINT('Ctrl Pts',(-18.3661753404608,17.1261891244055,
-13.2907228696037));
#105259=CARTESIAN_POINT('Ctrl Pts',(-18.3725871659861,17.1250680423293,
-13.2911114730229));
#105260=CARTESIAN_POINT('Ctrl Pts',(-18.3877912144908,17.1224818832629,
-13.292029998264));
#105261=CARTESIAN_POINT('Ctrl Pts',(-18.3965877653347,17.1210427194072,
-13.2925590921504));
#105262=CARTESIAN_POINT('Ctrl Pts',(-18.4253806663287,17.1165185684773,
-13.2942834919966));
#105263=CARTESIAN_POINT('Ctrl Pts',(-18.4454125678985,17.1136646200445,
-13.2954714863958));
#105264=CARTESIAN_POINT('Ctrl Pts',(-18.4930781369422,17.1075695618615,
-13.2982724892917));
#105265=CARTESIAN_POINT('Ctrl Pts',(-18.5207411502495,17.104585103667,-13.2998775388874));
#105266=CARTESIAN_POINT('Ctrl Pts',(-18.717162968989,17.0873032415419,-13.3111481511594));
#105267=CARTESIAN_POINT('Ctrl Pts',(-18.8870363146644,17.0927568789407,
-13.3201752962323));
#105268=CARTESIAN_POINT('Ctrl Pts',(-19.1572080616372,17.1341296375417,
-13.3351121649151));
#105269=CARTESIAN_POINT('Ctrl Pts',(-19.2586530023032,17.1574107146535,
-13.340876541378));
#105270=CARTESIAN_POINT('Ctrl Pts',(-19.3672203731698,17.190897326067,-13.3476076127931));
#105271=CARTESIAN_POINT('Ctrl Pts',(-19.3764579487496,17.1938161634937,
-13.3481849249218));
#105272=CARTESIAN_POINT('Ctrl Pts',(-19.3900688516309,17.1982198358758,
-13.349042793318));
#105273=CARTESIAN_POINT('Ctrl Pts',(-19.3944580260683,17.1996557922505,
-13.3493205510939));
#105274=CARTESIAN_POINT('Ctrl Pts',(-19.4022370979242,17.2022289912175,
-13.3498148714842));
#105275=CARTESIAN_POINT('Ctrl Pts',(-19.4056288496289,17.2033604723697,
-13.3500310925898));
#105276=CARTESIAN_POINT('Ctrl Pts',(-19.4128905138955,17.2058034097045,
-13.3504955196564));
#105277=CARTESIAN_POINT('Ctrl Pts',(-19.4167594425726,17.2071174589025,
-13.3507438722025));
#105278=CARTESIAN_POINT('Ctrl Pts',(-19.4273710736423,17.2107559095394,
-13.3514275059744));
#105279=CARTESIAN_POINT('Ctrl Pts',(-19.4341057994913,17.2131031724918,
-13.3518641066235));
#105280=CARTESIAN_POINT('Ctrl Pts',(-19.4695225453469,17.2256480819157,
-13.3541740312793));
#105281=CARTESIAN_POINT('Ctrl Pts',(-19.4979924247592,17.2364289059917,
-13.356079057898));
#105282=CARTESIAN_POINT('Ctrl Pts',(-19.6765791196524,17.3084954324587,
-13.3682924914236));
#105283=CARTESIAN_POINT('Ctrl Pts',(-19.8194667209514,17.3862424093955,
-13.3792084853915));
#105284=CARTESIAN_POINT('Ctrl Pts',(-20.0499071873122,17.5483562663366,
-13.3976307427178));
#105285=CARTESIAN_POINT('Ctrl Pts',(-20.1417396488845,17.6253539665135,
-13.4052583534821));
#105286=CARTESIAN_POINT('Ctrl Pts',(-20.2377288048237,17.7207867658016,
-13.4135235396185));
#105287=CARTESIAN_POINT('Ctrl Pts',(-20.2487462301813,17.7319869233607,
-13.4144773462716));
#105288=CARTESIAN_POINT('Ctrl Pts',(-20.2652268074862,17.7491181839616,
-13.4159122741625));
#105289=CARTESIAN_POINT('Ctrl Pts',(-20.2707822499671,17.7549593759034,
-13.4163974120406));
#105290=CARTESIAN_POINT('Ctrl Pts',(-20.2806777383223,17.7654835745531,
-13.4172642015325));
#105291=CARTESIAN_POINT('Ctrl Pts',(-20.2850301952312,17.7701547281809,
-13.4176463858278));
#105292=CARTESIAN_POINT('Ctrl Pts',(-20.2942209541851,17.7801083598774,
-13.4184554450099));
#105293=CARTESIAN_POINT('Ctrl Pts',(-20.2990537196481,17.7853958585207,
-13.4188820811029));
#105294=CARTESIAN_POINT('Ctrl Pts',(-20.3088371051771,17.7962095080493,
-13.4197482916651));
#105295=CARTESIAN_POINT('Ctrl Pts',(-20.3137857009629,17.8017373612013,
-13.4201877778931));
#105296=CARTESIAN_POINT('Ctrl Pts',(-20.3355743552209,17.826335477678,-13.4221289725536));
#105297=CARTESIAN_POINT('Ctrl Pts',(-20.3520993606331,17.8456828954844,
-13.4236175747887));
#105298=CARTESIAN_POINT('Ctrl Pts',(-20.4222714004769,17.9309041675784,
-13.4300186951382));
#105299=CARTESIAN_POINT('Ctrl Pts',(-20.4722775254316,17.999678774767,-13.4347859189593));
#105300=CARTESIAN_POINT('Ctrl Pts',(-20.5551898586189,18.1294624410505,
-13.4432735653916));
#105301=CARTESIAN_POINT('Ctrl Pts',(-20.5894925754731,18.1894307911714,
-13.4470186963147));
#105302=CARTESIAN_POINT('Ctrl Pts',(-20.6594231137151,18.3268692777156,
-13.4553933096343));
#105303=CARTESIAN_POINT('Ctrl Pts',(-20.6934048953441,18.4049868972709,
-13.4600145695703));
#105304=CARTESIAN_POINT('Ctrl Pts',(-20.722580578415,18.4848896205462,-13.4647888589437));
#105305=CARTESIAN_POINT('',(-20.8509991540684,19.2091074689689,-12.4890563034288));
#105306=CARTESIAN_POINT('Ctrl Pts',(-20.7225806137986,18.4848897174502,
-13.2445592988469));
#105307=CARTESIAN_POINT('Ctrl Pts',(-20.69626082822,18.4128083592617,-13.2399327222378));
#105308=CARTESIAN_POINT('Ctrl Pts',(-20.6660544393632,18.342259704581,-13.2353061456286));
#105309=CARTESIAN_POINT('Ctrl Pts',(-20.6321742240321,18.2736507506697,
-13.2306795690195));
#105310=CARTESIAN_POINT('Ctrl Pts',(-20.6214444484106,18.251922474332,-13.2292143443027));
#105311=CARTESIAN_POINT('Ctrl Pts',(-20.6103465313864,18.2303885369089,
-13.227749119586));
#105312=CARTESIAN_POINT('Ctrl Pts',(-20.598888138009,18.209061262994,-13.2262838948692));
#105313=CARTESIAN_POINT('Ctrl Pts',(-20.5645713376047,18.145188102246,-13.2218956859383));
#105314=CARTESIAN_POINT('Ctrl Pts',(-20.5269022333029,18.0829553476818,
-13.2175074770074));
#105315=CARTESIAN_POINT('Ctrl Pts',(-20.4860618340581,18.0227372640543,
-13.2131192680765));
#105316=CARTESIAN_POINT('Ctrl Pts',(-20.4452820487372,17.9626085540473,
-13.2087375719752));
#105317=CARTESIAN_POINT('Ctrl Pts',(-20.4013405804882,17.9044889751324,
-13.2043558758739));
#105318=CARTESIAN_POINT('Ctrl Pts',(-20.3544642120277,17.8487280970608,
-13.1999741797727));
#105319=CARTESIAN_POINT('Ctrl Pts',(-20.3076429270307,17.7930327424586,
-13.195597632513));
#105320=CARTESIAN_POINT('Ctrl Pts',(-20.2578939016345,17.7396909501819,
-13.1912210852534));
#105321=CARTESIAN_POINT('Ctrl Pts',(-20.2054860875596,17.6890217826399,
-13.1868445379937));
#105322=CARTESIAN_POINT('Ctrl Pts',(-20.1531115097587,17.6383847487476,
-13.1824707662768));
#105323=CARTESIAN_POINT('Ctrl Pts',(-20.0980818347927,17.5904173110763,
-13.1780969945598));
#105324=CARTESIAN_POINT('Ctrl Pts',(-20.040704044844,17.5454029481329,-13.1737232228428));
#105325=CARTESIAN_POINT('Ctrl Pts',(-19.9833437151495,17.5004022832114,
-13.1693507820792));
#105326=CARTESIAN_POINT('Ctrl Pts',(-19.9236370683463,17.4583532065245,
-13.1649783413157));
#105327=CARTESIAN_POINT('Ctrl Pts',(-19.8619241653155,17.419498931818,-13.1606059005521));
#105328=CARTESIAN_POINT('Ctrl Pts',(-19.800209684279,17.3806436636034,-13.1562333479848));
#105329=CARTESIAN_POINT('Ctrl Pts',(-19.7364892544384,17.3449836148752,
-13.1518607954174));
#105330=CARTESIAN_POINT('Ctrl Pts',(-19.6711304798848,17.3127177597441,
-13.1474882428501));
#105331=CARTESIAN_POINT('Ctrl Pts',(-19.6057038735297,17.2804184178915,
-13.1431111522827));
#105332=CARTESIAN_POINT('Ctrl Pts',(-19.5386359610928,17.251520516779,-13.1387340617154));
#105333=CARTESIAN_POINT('Ctrl Pts',(-19.4703166749593,17.2261758883526,
-13.1343569711481));
#105334=CARTESIAN_POINT('Ctrl Pts',(-19.401960077128,17.200817418284,-13.1299774900891));
#105335=CARTESIAN_POINT('Ctrl Pts',(-19.3323512055622,17.1790162288383,
-13.1255980090302));
#105336=CARTESIAN_POINT('Ctrl Pts',(-19.2618949953256,17.1608741809562,
-13.1212185279712));
#105337=CARTESIAN_POINT('Ctrl Pts',(-19.1913139019294,17.1426999764159,
-13.1168312843115));
#105338=CARTESIAN_POINT('Ctrl Pts',(-19.1198829437749,17.1281979613856,
-13.1124440406518));
#105339=CARTESIAN_POINT('Ctrl Pts',(-19.0480164983068,17.1174187049959,
-13.108056796992));
#105340=CARTESIAN_POINT('Ctrl Pts',(-18.9991542404234,17.1100898493376,
-13.1050738940573));
#105341=CARTESIAN_POINT('Ctrl Pts',(-18.950090817836,17.1044808253816,-13.1020909911225));
#105342=CARTESIAN_POINT('Ctrl Pts',(-18.9009566611239,17.1005937658104,
-13.0991080881877));
#105343=CARTESIAN_POINT('Ctrl Pts',(-18.8286744078925,17.0948754337364,
-13.0947198792568));
#105344=CARTESIAN_POINT('Ctrl Pts',(-18.7559569381435,17.0928637794812,
-13.0903316703259));
#105345=CARTESIAN_POINT('Ctrl Pts',(-18.6832169260195,17.0946091855716,
-13.085943461395));
#105346=CARTESIAN_POINT('Ctrl Pts',(-18.6105848721339,17.0963520011899,
-13.0815617652938));
#105347=CARTESIAN_POINT('Ctrl Pts',(-18.537930820542,17.1018407963575,-13.0771800691925));
#105348=CARTESIAN_POINT('Ctrl Pts',(-18.4656714572671,17.1110740981752,
-13.0727983730912));
#105349=CARTESIAN_POINT('Ctrl Pts',(-18.3934970044947,17.1202965501284,
-13.0684218258316));
#105350=CARTESIAN_POINT('Ctrl Pts',(-18.3217167948296,17.1332547070803,
-13.064045278572));
#105351=CARTESIAN_POINT('Ctrl Pts',(-18.2507446877305,17.1498951256272,
-13.0596687313123));
#105352=CARTESIAN_POINT('Ctrl Pts',(-18.1798175901102,17.1665249910625,
-13.0552949595953));
#105353=CARTESIAN_POINT('Ctrl Pts',(-18.1096980467015,17.1868323748369,
-13.0509211878784));
#105354=CARTESIAN_POINT('Ctrl Pts',(-18.0407905817002,17.2107125950553,
-13.0465474161614));
#105355=CARTESIAN_POINT('Ctrl Pts',(-17.9719040854719,17.2345855484424,
-13.0421749753978));
#105356=CARTESIAN_POINT('Ctrl Pts',(-17.9042293909005,17.2620290219354,
-13.0378025346343));
#105357=CARTESIAN_POINT('Ctrl Pts',(-17.8381550707619,17.2928887251365,
-13.0334300938707));
#105358=CARTESIAN_POINT('Ctrl Pts',(-17.7720790610957,17.3237492174237,
-13.0290575413034));
#105359=CARTESIAN_POINT('Ctrl Pts',(-17.7076039433213,17.3580259069127,
-13.0246849887361));
#105360=CARTESIAN_POINT('Ctrl Pts',(-17.6450960002997,17.3955173976497,
-13.0203124361687));
#105361=CARTESIAN_POINT('Ctrl Pts',(-17.5825231841771,17.4330477984699,
-13.0159353456014));
#105362=CARTESIAN_POINT('Ctrl Pts',(-17.5219220335749,17.4737994133219,
-13.0115582550341));
#105363=CARTESIAN_POINT('Ctrl Pts',(-17.4636312781365,17.5175265545304,
-13.0071811644667));
#105364=CARTESIAN_POINT('Ctrl Pts',(-17.405308687953,17.5612775767536,-13.0028016834078));
#105365=CARTESIAN_POINT('Ctrl Pts',(-17.3492993758003,17.6080070515429,
-12.9984222023489));
#105366=CARTESIAN_POINT('Ctrl Pts',(-17.2959081742794,17.6574296279873,
-12.9940427212899));
#105367=CARTESIAN_POINT('Ctrl Pts',(-17.2424223372123,17.7069398056167,
-12.9896554776302));
#105368=CARTESIAN_POINT('Ctrl Pts',(-17.1915642147117,17.7591522715469,
-12.9852682339705));
#105369=CARTESIAN_POINT('Ctrl Pts',(-17.1436006220652,17.8137459720349,
-12.9808809903108));
#105370=CARTESIAN_POINT('Ctrl Pts',(-17.1109900008265,17.8508644277303,
-12.9778980873759));
#105371=CARTESIAN_POINT('Ctrl Pts',(-17.0797165992412,17.8890829433879,
-12.9749151844411));
#105372=CARTESIAN_POINT('Ctrl Pts',(-17.0498528101567,17.9282930019124,
-12.9719322815063));
#105373=CARTESIAN_POINT('Ctrl Pts',(-17.0059195850954,17.9859757132705,
-12.9675440725754));
#105374=CARTESIAN_POINT('Ctrl Pts',(-16.9648675150387,18.046030727246,-12.9631558636445));
#105375=CARTESIAN_POINT('Ctrl Pts',(-16.9269623364049,18.1081383212983,
-12.9587676547136));
#105376=CARTESIAN_POINT('Ctrl Pts',(-16.889113415341,18.1701537373834,-12.9543859586123));
#105377=CARTESIAN_POINT('Ctrl Pts',(-16.8544023633226,18.2342152777403,
-12.9500042625111));
#105378=CARTESIAN_POINT('Ctrl Pts',(-16.8230534861161,18.2999717781127,
-12.9456225664098));
#105379=CARTESIAN_POINT('Ctrl Pts',(-16.7917414463352,18.3656510093642,
-12.9412460191502));
#105380=CARTESIAN_POINT('Ctrl Pts',(-16.7637839395866,18.4330208108152,
-12.9368694718905));
#105381=CARTESIAN_POINT('Ctrl Pts',(-16.7393600427009,18.5017042642551,
-12.9324929246309));
#105382=CARTESIAN_POINT('Ctrl Pts',(-16.7149516350957,18.5703441596469,
-12.9281191529139));
#105383=CARTESIAN_POINT('Ctrl Pts',(-16.694072552212,18.6402956006724,-12.9237453811969));
#105384=CARTESIAN_POINT('Ctrl Pts',(-16.6768537344171,18.7111617841757,
-12.91937160948));
#105385=CARTESIAN_POINT('Ctrl Pts',(-16.6596401563663,18.7820064028615,
-12.9149991687164));
#105386=CARTESIAN_POINT('Ctrl Pts',(-16.6460847459306,18.8537647429385,
-12.9106267279528));
#105387=CARTESIAN_POINT('Ctrl Pts',(-16.6362680963764,18.9260265617294,
-12.9062542871893));
#105388=CARTESIAN_POINT('Ctrl Pts',(-16.6264511958094,18.998290228263,-12.9018817346219));
#105389=CARTESIAN_POINT('Ctrl Pts',(-16.620373308882,19.0710569208143,-12.8975091820546));
#105390=CARTESIAN_POINT('Ctrl Pts',(-16.6180633554341,19.1439096416525,
-12.8931366294872));
#105391=CARTESIAN_POINT('Ctrl Pts',(-16.6157510046294,19.2168379717925,
-12.8887595389199));
#105392=CARTESIAN_POINT('Ctrl Pts',(-16.6172144102078,19.2898520253128,
-12.8843824483526));
#105393=CARTESIAN_POINT('Ctrl Pts',(-16.6224303356468,19.3625339981098,
-12.8800053577853));
#105394=CARTESIAN_POINT('Ctrl Pts',(-16.6276491096962,19.4352556652298,
-12.8756258767263));
#105395=CARTESIAN_POINT('Ctrl Pts',(-16.6366244245267,19.5076444114932,
-12.8712463956674));
#105396=CARTESIAN_POINT('Ctrl Pts',(-16.6492813452851,19.5792894658875,
-12.8668669146084));
#105397=CARTESIAN_POINT('Ctrl Pts',(-16.6619607003506,19.6510615106598,
-12.8624796709487));
#105398=CARTESIAN_POINT('Ctrl Pts',(-16.678334584287,19.7220867607307,-12.858092427289));
#105399=CARTESIAN_POINT('Ctrl Pts',(-16.698277463759,19.791967086366,-12.8537051836293));
#105400=CARTESIAN_POINT('Ctrl Pts',(-16.7118367001087,19.8394789741459,
-12.8507222806944));
#105401=CARTESIAN_POINT('Ctrl Pts',(-16.7270447244344,19.88646191341,-12.8477393777596));
#105402=CARTESIAN_POINT('Ctrl Pts',(-16.7438494759074,19.9327962949848,
-12.8447564748248));
#105403=CARTESIAN_POINT('Ctrl Pts',(-16.7685712862064,20.0009597422968,
-12.8403682658939));
#105404=CARTESIAN_POINT('Ctrl Pts',(-16.7968473421402,20.0679846766149,
-12.835980056963));
#105405=CARTESIAN_POINT('Ctrl Pts',(-16.8285526457323,20.1334745959182,
-12.8315918480321));
#105406=CARTESIAN_POINT('Ctrl Pts',(-16.8602108933972,20.1988673173228,
-12.8272101519309));
#105407=CARTESIAN_POINT('Ctrl Pts',(-16.8952880767684,20.2627291156991,
-12.8228284558296));
#105408=CARTESIAN_POINT('Ctrl Pts',(-16.9336103347365,20.3246813068434,
-12.8184467597283));
#105409=CARTESIAN_POINT('Ctrl Pts',(-16.9718875610016,20.3865606992326,
-12.8140702124687));
#105410=CARTESIAN_POINT('Ctrl Pts',(-17.0134020343728,20.4465345337929,
-12.8096936652091));
#105411=CARTESIAN_POINT('Ctrl Pts',(-17.0579337571751,20.5042482165705,
-12.8053171179494));
#105412=CARTESIAN_POINT('Ctrl Pts',(-17.102437238606,20.5619252981693,-12.8009433462325));
#105413=CARTESIAN_POINT('Ctrl Pts',(-17.1499538788911,20.617344690981,-12.7965695745155));
#105414=CARTESIAN_POINT('Ctrl Pts',(-17.200220904909,20.6701815128564,-12.7921958027985));
#105415=CARTESIAN_POINT('Ctrl Pts',(-17.2504726345021,20.7230022563095,
-12.787823362035));
#105416=CARTESIAN_POINT('Ctrl Pts',(-17.3034727559332,20.7732416397748,
-12.7834509212714));
#105417=CARTESIAN_POINT('Ctrl Pts',(-17.3589199436394,20.8206098404891,
-12.7790784805079));
#105418=CARTESIAN_POINT('Ctrl Pts',(-17.4143685491363,20.8679792524135,
-12.7747059279405));
#105419=CARTESIAN_POINT('Ctrl Pts',(-17.4722639770756,20.9124770240216,
-12.7703333753732));
#105420=CARTESIAN_POINT('Ctrl Pts',(-17.5322712521179,20.9538531253418,
-12.7659608228058));
#105421=CARTESIAN_POINT('Ctrl Pts',(-17.5923408049737,20.9952721683407,
-12.7615837322385));
#105422=CARTESIAN_POINT('Ctrl Pts',(-17.6545261829437,21.0335627981877,
-12.7572066416712));
#105423=CARTESIAN_POINT('Ctrl Pts',(-17.7184635014066,21.068518403684,-12.7528295511039));
#105424=CARTESIAN_POINT('Ctrl Pts',(-17.7824357384122,21.1034930997338,
-12.7484500700449));
#105425=CARTESIAN_POINT('Ctrl Pts',(-17.8481613859397,21.135128935727,-12.744070588986));
#105426=CARTESIAN_POINT('Ctrl Pts',(-17.9152544897586,21.163266577458,-12.7396911079271));
#105427=CARTESIAN_POINT('Ctrl Pts',(-17.9824665156537,21.1914540929701,
-12.7353038642673));
#105428=CARTESIAN_POINT('Ctrl Pts',(-18.0510503837933,21.2161308685658,
-12.7309166206076));
#105429=CARTESIAN_POINT('Ctrl Pts',(-18.1206033812628,21.2371869578402,
-12.7265293769479));
#105430=CARTESIAN_POINT('Ctrl Pts',(-18.1678927174314,21.2515030695869,
-12.7235464740131));
#105431=CARTESIAN_POINT('Ctrl Pts',(-18.2156297492658,21.2641465017728,
-12.7205635710783));
#105432=CARTESIAN_POINT('Ctrl Pts',(-18.2636857248404,21.275096287139,-12.7175806681434));
#105433=CARTESIAN_POINT('Ctrl Pts',(-18.334381843959,21.2912047381968,-12.7131924592126));
#105434=CARTESIAN_POINT('Ctrl Pts',(-18.4060444995739,21.3037083756574,
-12.7088042502817));
#105435=CARTESIAN_POINT('Ctrl Pts',(-18.4782726371993,21.3124976840137,
-12.7044160413508));
#105436=CARTESIAN_POINT('Ctrl Pts',(-18.5503935762929,21.3212739475792,
-12.7000343452495));
#105437=CARTESIAN_POINT('Ctrl Pts',(-18.6230778564461,21.3263467676749,
-12.6956526491482));
#105438=CARTESIAN_POINT('Ctrl Pts',(-18.6959129564506,21.3276573594027,
-12.691270953047));
#105439=CARTESIAN_POINT('Ctrl Pts',(-18.7686624694161,21.3289664110809,
-12.6868944057873));
#105440=CARTESIAN_POINT('Ctrl Pts',(-18.8415619702678,21.3265220079374,
-12.6825178585277));
#105441=CARTESIAN_POINT('Ctrl Pts',(-18.9141942210374,21.3203171982195,
-12.6781413112681));
#105442=CARTESIAN_POINT('Ctrl Pts',(-18.9867804094892,21.3141163235018,
-12.6737675395511));
#105443=CARTESIAN_POINT('Ctrl Pts',(-19.0590992046968,21.3041598149105,
-12.6693937678341));
#105444=CARTESIAN_POINT('Ctrl Pts',(-19.1307351980796,21.2904927705103,
-12.6650199961171));
#105445=CARTESIAN_POINT('Ctrl Pts',(-19.2023493923891,21.2768298850377,
-12.6606475553536));
#105446=CARTESIAN_POINT('Ctrl Pts',(-19.2732807238325,21.2594587957697,
-12.65627511459));
#105447=CARTESIAN_POINT('Ctrl Pts',(-19.3431223955192,21.2384759942542,
-12.6519026738265));
#105448=CARTESIAN_POINT('Ctrl Pts',(-19.4129658530652,21.2174926562061,
-12.6475301212592));
#105449=CARTESIAN_POINT('Ctrl Pts',(-19.4817191341324,21.1928975632637,
-12.6431575686918));
#105450=CARTESIAN_POINT('Ctrl Pts',(-19.5489906872852,21.1648370401951,
-12.6387850161245));
#105451=CARTESIAN_POINT('Ctrl Pts',(-19.6163320573932,21.1367473948573,
-12.6344079255571));
#105452=CARTESIAN_POINT('Ctrl Pts',(-19.6821881831272,21.1051853247309,
-12.6300308349898));
#105453=CARTESIAN_POINT('Ctrl Pts',(-19.7461883733219,21.0703449644732,
-12.6256537444225));
#105454=CARTESIAN_POINT('Ctrl Pts',(-19.8102235163959,21.0354855766017,
-12.6212742633636));
#105455=CARTESIAN_POINT('Ctrl Pts',(-19.8724002944077,20.9973445863424,
-12.6168947823046));
#105456=CARTESIAN_POINT('Ctrl Pts',(-19.932375822801,20.9561602755409,-12.6125153012457));
#105457=CARTESIAN_POINT('Ctrl Pts',(-19.9924576574157,20.9149029658251,
-12.608128057586));
#105458=CARTESIAN_POINT('Ctrl Pts',(-20.0503300675354,20.87059185695,-12.6037408139262));
#105459=CARTESIAN_POINT('Ctrl Pts',(-20.1056826247701,20.8235060548425,
-12.5993535702665));
#105460=CARTESIAN_POINT('Ctrl Pts',(-20.1433170299302,20.7914922465863,
-12.5963706673317));
#105461=CARTESIAN_POINT('Ctrl Pts',(-20.1797873054598,20.758196607403,-12.5933877643969));
#105462=CARTESIAN_POINT('Ctrl Pts',(-20.2150061302367,20.7237160481073,
-12.590404861462));
#105463=CARTESIAN_POINT('Ctrl Pts',(-20.2660558507878,20.6737364440846,
-12.5860811407752));
#105464=CARTESIAN_POINT('Ctrl Pts',(-20.3146860821103,20.6210584681426,
-12.5817574200883));
#105465=CARTESIAN_POINT('Ctrl Pts',(-20.3605919747978,20.5659492785797,
-12.5774336994015));
#105466=CARTESIAN_POINT('Ctrl Pts',(-20.4064369112151,20.5109132659108,
-12.5731157199794));
#105467=CARTESIAN_POINT('Ctrl Pts',(-20.4495643625503,20.453452815078,-12.5687977405574));
#105468=CARTESIAN_POINT('Ctrl Pts',(-20.4897052944035,20.3938727400712,
-12.5644797611354));
#105469=CARTESIAN_POINT('Ctrl Pts',(-20.5298070691323,20.3343507849011,
-12.5601659938641));
#105470=CARTESIAN_POINT('Ctrl Pts',(-20.5669278234435,20.2727137148021,
-12.5558522265928));
#105471=CARTESIAN_POINT('Ctrl Pts',(-20.600839132399,20.2092988799672,-12.5515384593216));
#105472=CARTESIAN_POINT('Ctrl Pts',(-20.6347293023106,20.1459235755726,
-12.5472273810918));
#105473=CARTESIAN_POINT('Ctrl Pts',(-20.6654137615196,20.0807731423998,
-12.542916302862));
#105474=CARTESIAN_POINT('Ctrl Pts',(-20.6927087374024,20.0142117292615,
-12.5386052246321));
#105475=CARTESIAN_POINT('Ctrl Pts',(-20.720007692024,19.9476406135877,-12.5342935179843));
#105476=CARTESIAN_POINT('Ctrl Pts',(-20.7439159714602,19.8796585609649,
-12.5299818113365));
#105477=CARTESIAN_POINT('Ctrl Pts',(-20.7642975065946,19.8106507606231,
-12.5256701046887));
#105478=CARTESIAN_POINT('Ctrl Pts',(-20.7846795217662,19.7416413349712,
-12.5213582964892));
#105479=CARTESIAN_POINT('Ctrl Pts',(-20.8015344966335,19.671606594183,-12.5170464882896));
#105480=CARTESIAN_POINT('Ctrl Pts',(-20.8147766394152,19.6009456075709,
-12.5127346800901));
#105481=CARTESIAN_POINT('Ctrl Pts',(-20.8280335437791,19.5302058521392,
-12.5084180653338));
#105482=CARTESIAN_POINT('Ctrl Pts',(-20.8376694934189,19.4588389489561,
-12.5041014505775));
#105483=CARTESIAN_POINT('Ctrl Pts',(-20.8436502754156,19.3872518522996,
-12.4997848358213));
#105484=CARTESIAN_POINT('Ctrl Pts',(-20.8486051622892,19.3279442290249,
-12.4962086583571));
#105485=CARTESIAN_POINT('Ctrl Pts',(-20.8510522363726,19.2684857254966,
-12.4926324808929));
#105486=CARTESIAN_POINT('Ctrl Pts',(-20.8509991540684,19.2091074689689,
-12.4890563034288));
#105487=CARTESIAN_POINT('Ctrl Pts',(-20.8516474773841,19.2091064840258,
-12.4890562790225));
#105488=CARTESIAN_POINT('Ctrl Pts',(-20.8529701850388,19.0661177649361,
-12.4804472042752));
#105489=CARTESIAN_POINT('Ctrl Pts',(-20.8300642588143,18.8192068783604,
-12.4655558065448));
#105490=CARTESIAN_POINT('Ctrl Pts',(-20.7608947058963,18.581811275593,-12.4506644088145));
#105491=CARTESIAN_POINT('Ctrl Pts',(-20.7242505411024,18.4842642021379,
-12.4443820858314));
#105492=CARTESIAN_POINT('Origin',(-18.734,19.211,0.));
#105493=CARTESIAN_POINT('',(-20.7225806143616,18.4848897189921,-11.6425493859455));
#105494=CARTESIAN_POINT('',(-20.7225806137507,18.4848897173191,-11.8674650369494));
#105495=CARTESIAN_POINT('',(-20.7225806137986,18.4848897174502,0.));
#105496=CARTESIAN_POINT('',(-20.8509993992231,19.2125948947384,-11.912063495998));
#105497=CARTESIAN_POINT('Ctrl Pts',(-20.7225806137507,18.4848897173191,
-11.8674650369494));
#105498=CARTESIAN_POINT('Ctrl Pts',(-20.7358715688534,18.5212893335838,
-11.869979723211));
#105499=CARTESIAN_POINT('Ctrl Pts',(-20.7481612761736,18.5580488153306,
-11.8724726491891));
#105500=CARTESIAN_POINT('Ctrl Pts',(-20.7623061769257,18.6045674671939,
-11.8755657388135));
#105501=CARTESIAN_POINT('Ctrl Pts',(-20.765110754078,18.6140280798097,-11.8761916412424));
#105502=CARTESIAN_POINT('Ctrl Pts',(-20.7833787104828,18.6772702539463,
-11.8803545618301));
#105503=CARTESIAN_POINT('Ctrl Pts',(-20.7967715338951,18.7316305576149,
-11.8838304061372));
#105504=CARTESIAN_POINT('Ctrl Pts',(-20.8104072908029,18.7982453194696,
-11.8879694996));
#105505=CARTESIAN_POINT('Ctrl Pts',(-20.8127188548269,18.8100491357361,
-11.8886984336853));
#105506=CARTESIAN_POINT('Ctrl Pts',(-20.8163752084312,18.8296021335995,
-11.8898986409805));
#105507=CARTESIAN_POINT('Ctrl Pts',(-20.8177776152043,18.8373401357374,
-11.8903717414125));
#105508=CARTESIAN_POINT('Ctrl Pts',(-20.8202374454822,18.8513573114023,
-11.8912254139216));
#105509=CARTESIAN_POINT('Ctrl Pts',(-20.821309713366,18.8576337533753,-11.8916064539954));
#105510=CARTESIAN_POINT('Ctrl Pts',(-20.823336457162,18.8698283388792,-11.8923444756629));
#105511=CARTESIAN_POINT('Ctrl Pts',(-20.8242941443647,18.8757458803418,
-11.8927015558131));
#105512=CARTESIAN_POINT('Ctrl Pts',(-20.826339673241,18.8887347715827,-11.8934830704994));
#105513=CARTESIAN_POINT('Ctrl Pts',(-20.8274168317906,18.895807747638,-11.8939071640037));
#105514=CARTESIAN_POINT('Ctrl Pts',(-20.8299772014903,18.913212309321,-11.8949471940112));
#105515=CARTESIAN_POINT('Ctrl Pts',(-20.8314199118356,18.9235497310235,
-11.8955618545989));
#105516=CARTESIAN_POINT('Ctrl Pts',(-20.8449846042971,19.0262893038818,
-11.9016414009509));
#105517=CARTESIAN_POINT('Ctrl Pts',(-20.8510696179088,19.1193894235361,
-11.9069087635312));
#105518=CARTESIAN_POINT('Ctrl Pts',(-20.8509993992231,19.2125948947384,
-11.912063495998));
#105519=CARTESIAN_POINT('Ctrl Pts',(-20.8509994011049,19.2125923949245,
-11.9120633577456));
#105520=CARTESIAN_POINT('Ctrl Pts',(-20.8508903570202,19.3575603663925,
-11.9200808205576));
#105521=CARTESIAN_POINT('Ctrl Pts',(-20.8358914523054,19.5021322706615,
-11.9277753972783));
#105522=CARTESIAN_POINT('Ctrl Pts',(-20.7926402019966,19.709104411674,-11.9395053011385));
#105523=CARTESIAN_POINT('Ctrl Pts',(-20.7759875264153,19.7734879564716,
-11.9432643032825));
#105524=CARTESIAN_POINT('Ctrl Pts',(-20.7524080810177,19.8496660435697,
-11.947959439339));
#105525=CARTESIAN_POINT('Ctrl Pts',(-20.7483605177477,19.8623195691038,
-11.9487477000343));
#105526=CARTESIAN_POINT('Ctrl Pts',(-20.7425481574265,19.8799176689914,
-11.9498567939057));
#105527=CARTESIAN_POINT('Ctrl Pts',(-20.7408835583365,19.8848953409272,
-11.9501719417593));
#105528=CARTESIAN_POINT('Ctrl Pts',(-20.7380219445164,19.8933478240683,
-11.9507096166996));
#105529=CARTESIAN_POINT('Ctrl Pts',(-20.7368343462604,19.8968258440078,
-11.9509315890967));
#105530=CARTESIAN_POINT('Ctrl Pts',(-20.7345445651943,19.9034750637692,
-11.9513573813501));
#105531=CARTESIAN_POINT('Ctrl Pts',(-20.7334438881852,19.9066467558357,
-11.9515611071857));
#105532=CARTESIAN_POINT('Ctrl Pts',(-20.7305162330582,19.9150186870069,
-11.9521004766321));
#105533=CARTESIAN_POINT('Ctrl Pts',(-20.7286764966813,19.9202143910975,
-11.9524368680168));
#105534=CARTESIAN_POINT('Ctrl Pts',(-20.722118593999,19.9385075683665,-11.9536269312589));
#105535=CARTESIAN_POINT('Ctrl Pts',(-20.7172916623693,19.9515653005,-11.9544867064343));
#105536=CARTESIAN_POINT('Ctrl Pts',(-20.6531107493891,20.1200576144672,
-11.9657061258321));
#105537=CARTESIAN_POINT('Ctrl Pts',(-20.5757664590092,20.2680063725952,
-11.9768935660573));
#105538=CARTESIAN_POINT('Ctrl Pts',(-20.4366046845345,20.4716641432207,
-11.9930979794031));
#105539=CARTESIAN_POINT('Ctrl Pts',(-20.387563583073,20.5353361806168,-11.9983096747123));
#105540=CARTESIAN_POINT('Ctrl Pts',(-20.3092874391038,20.6258163447576,
-12.0058901418974));
#105541=CARTESIAN_POINT('Ctrl Pts',(-20.2827306186546,20.6548384915281,
-12.0083517684621));
#105542=CARTESIAN_POINT('Ctrl Pts',(-20.2369236281096,20.7021787174121,
-12.0124188879455));
#105543=CARTESIAN_POINT('Ctrl Pts',(-20.2181103922107,20.7209039186198,
-12.014042124923));
#105544=CARTESIAN_POINT('Ctrl Pts',(-20.1918823967089,20.7460451938731,
-12.0162427451026));
#105545=CARTESIAN_POINT('Ctrl Pts',(-20.184768487642,20.7527702909866,-12.0168335464193));
#105546=CARTESIAN_POINT('Ctrl Pts',(-20.1732500031756,20.7635089144527,
-12.0177805123631));
#105547=CARTESIAN_POINT('Ctrl Pts',(-20.1688747467957,20.7675535529602,
-12.0181380111008));
#105548=CARTESIAN_POINT('Ctrl Pts',(-20.1597234101342,20.7759419911736,
-12.0188812168942));
#105549=CARTESIAN_POINT('Ctrl Pts',(-20.1549444128617,20.7802825287135,
-12.019266783022));
#105550=CARTESIAN_POINT('Ctrl Pts',(-20.1438651762256,20.7902531695571,
-12.0201548315509));
#105551=CARTESIAN_POINT('Ctrl Pts',(-20.1375509102739,20.7958675762083,
-12.0206566496767));
#105552=CARTESIAN_POINT('Ctrl Pts',(-20.1204817448211,20.8108628165386,
-12.0220018378533));
#105553=CARTESIAN_POINT('Ctrl Pts',(-20.1096652052803,20.8201730541798,
-12.0228422763222));
#105554=CARTESIAN_POINT('Ctrl Pts',(-20.0094125557049,20.9047149290194,
-12.0305251328716));
#105555=CARTESIAN_POINT('Ctrl Pts',(-19.913979394313,20.9725338046926,-12.0370506413779));
#105556=CARTESIAN_POINT('Ctrl Pts',(-19.6733916488256,21.1151350699243,
-12.0523612625821));
#105557=CARTESIAN_POINT('Ctrl Pts',(-19.5242711950226,21.1816969838733,
-12.060963258126));
#105558=CARTESIAN_POINT('Ctrl Pts',(-19.3380509824021,21.2402523996148,
-12.0721724245961));
#105559=CARTESIAN_POINT('Ctrl Pts',(-19.3068642141171,21.2492760418074,
-12.0740659240699));
#105560=CARTESIAN_POINT('Ctrl Pts',(-19.2684884657816,21.2594295076322,
-12.0764294908508));
#105561=CARTESIAN_POINT('Ctrl Pts',(-19.2614832987398,21.2612445546577,
-12.0768622971979));
#105562=CARTESIAN_POINT('Ctrl Pts',(-19.2504861690386,21.2640338334509,
-12.0775440650814));
#105563=CARTESIAN_POINT('Ctrl Pts',(-19.2465003652833,21.2650324386501,
-12.0777916423319));
#105564=CARTESIAN_POINT('Ctrl Pts',(-19.239044257761,21.26687744216,-12.0782557108702));
#105565=CARTESIAN_POINT('Ctrl Pts',(-19.2355747105171,21.2677266635586,
-12.0784720370395));
#105566=CARTESIAN_POINT('Ctrl Pts',(-19.2276491610404,21.2696453082994,
-12.0789670559725));
#105567=CARTESIAN_POINT('Ctrl Pts',(-19.2231918407841,21.2707090429421,
-12.0792460709584));
#105568=CARTESIAN_POINT('Ctrl Pts',(-19.2094782326545,21.2739347550957,
-12.0801063217819));
#105569=CARTESIAN_POINT('Ctrl Pts',(-19.2002109578109,21.2760488344306,
-12.08069020016));
#105570=CARTESIAN_POINT('Ctrl Pts',(-19.1166836618199,21.2945124389833,
-12.0859737007823));
#105571=CARTESIAN_POINT('Ctrl Pts',(-19.0416148126414,21.3069106466933,
-12.0908690648959));
#105572=CARTESIAN_POINT('Ctrl Pts',(-18.8155829400092,21.3318369175994,
-12.1057426640404));
#105573=CARTESIAN_POINT('Ctrl Pts',(-18.6637507285478,21.3322442579105,
-12.1158740241582));
#105574=CARTESIAN_POINT('Ctrl Pts',(-18.4580865450591,21.3106734585856,
-12.1291691800293));
#105575=CARTESIAN_POINT('Ctrl Pts',(-18.4032449808158,21.3027358384152,
-12.1326772615108));
#105576=CARTESIAN_POINT('Ctrl Pts',(-18.3149154988974,21.2863898039453,
-12.1382614599131));
#105577=CARTESIAN_POINT('Ctrl Pts',(-18.2812134722424,21.2792986332837,
-12.1403764763748));
#105578=CARTESIAN_POINT('Ctrl Pts',(-18.2371638692775,21.2689018452238,
-12.1431218803234));
#105579=CARTESIAN_POINT('Ctrl Pts',(-18.2266490042642,21.2663347949438,
-12.1437757988958));
#105580=CARTESIAN_POINT('Ctrl Pts',(-18.2094624986717,21.2619990340104,
-12.1448424078432));
#105581=CARTESIAN_POINT('Ctrl Pts',(-18.2027790982131,21.2602781614682,
-12.1452566338115));
#105582=CARTESIAN_POINT('Ctrl Pts',(-18.1898606024616,21.256884402527,-12.146056274025));
#105583=CARTESIAN_POINT('Ctrl Pts',(-18.1836245171632,21.2552156201765,
-12.1464418159959));
#105584=CARTESIAN_POINT('Ctrl Pts',(-18.1692466990184,21.2512975405058,
-12.1473296872615));
#105585=CARTESIAN_POINT('Ctrl Pts',(-18.1611105649305,21.2490279789796,
-12.1478313531342));
#105586=CARTESIAN_POINT('Ctrl Pts',(-18.1392737832821,21.2427955438061,
-12.149175863685));
#105587=CARTESIAN_POINT('Ctrl Pts',(-18.1255990886412,21.2387427722877,
-12.1500157814584));
#105588=CARTESIAN_POINT('Ctrl Pts',(-18.0002992283032,21.2002259690837,
-12.1576955283891));
#105589=CARTESIAN_POINT('Ctrl Pts',(-17.891658331607,21.1567138937895,-12.1642187007505));
#105590=CARTESIAN_POINT('Ctrl Pts',(-17.6417216234923,21.0317293321491,
-12.1795170892452));
#105591=CARTESIAN_POINT('Ctrl Pts',(-17.50517311852,20.9425022547793,-12.1881097439642));
#105592=CARTESIAN_POINT('Ctrl Pts',(-17.3550700894167,20.8176453786321,
-12.1993181973251));
#105593=CARTESIAN_POINT('Ctrl Pts',(-17.3304336058437,20.7961681876,-12.2012240685647));
#105594=CARTESIAN_POINT('Ctrl Pts',(-17.3009514224285,20.7692404683417,
-12.2036013977632));
#105595=CARTESIAN_POINT('Ctrl Pts',(-17.2956224480114,20.7643227601928,
-12.2040350811563));
#105596=CARTESIAN_POINT('Ctrl Pts',(-17.2873111949527,20.7565734897704,
-12.2047179265899));
#105597=CARTESIAN_POINT('Ctrl Pts',(-17.2843116651068,20.7537603968029,
-12.2049656971147));
#105598=CARTESIAN_POINT('Ctrl Pts',(-17.2787223597263,20.7484878034898,
-12.2054299294243));
#105599=CARTESIAN_POINT('Ctrl Pts',(-17.2761306053488,20.7460304829698,
-12.2056462248791));
#105600=CARTESIAN_POINT('Ctrl Pts',(-17.2702311954537,20.7404086574444,
-12.2061409118672));
#105601=CARTESIAN_POINT('Ctrl Pts',(-17.2669275897185,20.7372399866044,
-12.2064196239426));
#105602=CARTESIAN_POINT('Ctrl Pts',(-17.2568136745195,20.7274759935125,
-12.207278034215));
#105603=CARTESIAN_POINT('Ctrl Pts',(-17.2500374794555,20.7208457235827,
-12.2078603589001));
#105604=CARTESIAN_POINT('Ctrl Pts',(-17.1573428745015,20.6289204953568,
-12.2159230830404));
#105605=CARTESIAN_POINT('Ctrl Pts',(-17.0788605425881,20.5364632518845,
-12.2238920357722));
#105606=CARTESIAN_POINT('Ctrl Pts',(-16.9050472727718,20.292028949297,-12.2437081062179));
#105607=CARTESIAN_POINT('Ctrl Pts',(-16.8202527669139,20.1336528795698,
-12.2554516534286));
#105608=CARTESIAN_POINT('Ctrl Pts',(-16.7487232006562,19.9464089652028,
-12.2677649610291));
#105609=CARTESIAN_POINT('Ctrl Pts',(-16.7413640368456,19.9262288359775,
-12.2690742199382));
#105610=CARTESIAN_POINT('Ctrl Pts',(-16.7313506267608,19.8974152737031,
-12.2709190638132));
#105611=CARTESIAN_POINT('Ctrl Pts',(-16.7284427171872,19.8888719860025,
-12.271463033325));
#105612=CARTESIAN_POINT('Ctrl Pts',(-16.7235252790679,19.8741161470664,
-12.2723974326037));
#105613=CARTESIAN_POINT('Ctrl Pts',(-16.7214897159683,19.867912464607,-12.2727887183452));
#105614=CARTESIAN_POINT('Ctrl Pts',(-16.7176504287978,19.8560263161585,
-12.2735354783316));
#105615=CARTESIAN_POINT('Ctrl Pts',(-16.7158419482694,19.850345463094,-12.2738911061059));
#105616=CARTESIAN_POINT('Ctrl Pts',(-16.7112085858819,19.8355754444516,
-12.2748124537305));
#105617=CARTESIAN_POINT('Ctrl Pts',(-16.7084209400011,19.8264746680678,
-12.2753769482363));
#105618=CARTESIAN_POINT('Ctrl Pts',(-16.6991587323188,19.7954918679359,
-12.2772880897035));
#105619=CARTESIAN_POINT('Ctrl Pts',(-16.6929764876236,19.7735236082731,
-12.2786252095429));
#105620=CARTESIAN_POINT('Ctrl Pts',(-16.6417820048902,19.5796376772178,
-12.2902797451863));
#105621=CARTESIAN_POINT('Ctrl Pts',(-16.6182276133207,19.402790694168,-12.2998237830137));
#105622=CARTESIAN_POINT('Ctrl Pts',(-16.6164789542422,19.1396149196788,
-12.314149024606));
#105623=CARTESIAN_POINT('Ctrl Pts',(-16.6210856254121,19.054214320218,-12.3188318710045));
#105624=CARTESIAN_POINT('Ctrl Pts',(-16.6351115504586,18.9321503895753,
-12.325849763404));
#105625=CARTESIAN_POINT('Ctrl Pts',(-16.6403691389444,18.8950897931115,
-12.3280244807594));
#105626=CARTESIAN_POINT('Ctrl Pts',(-16.6478638698815,18.8507472641974,
-12.3307002934696));
#105627=CARTESIAN_POINT('Ctrl Pts',(-16.6491617299718,18.843310768482,-12.3311515531232));
#105628=CARTESIAN_POINT('Ctrl Pts',(-16.6512395090436,18.831770270929,-12.3318559762129));
#105629=CARTESIAN_POINT('Ctrl Pts',(-16.6519918644425,18.8276612817882,
-12.3321075998139));
#105630=CARTESIAN_POINT('Ctrl Pts',(-16.653408677252,18.820050577058,-12.3325752135234));
#105631=CARTESIAN_POINT('Ctrl Pts',(-16.654069818119,18.8165483026953,-12.3327910135327));
#105632=CARTESIAN_POINT('Ctrl Pts',(-16.6555831790833,18.8086411456773,
-12.3332796143443));
#105633=CARTESIAN_POINT('Ctrl Pts',(-16.6564405547861,18.8042373175098,
-12.3335527044166));
#105634=CARTESIAN_POINT('Ctrl Pts',(-16.6590085506938,18.7912669934161,
-12.3343598057923));
#105635=CARTESIAN_POINT('Ctrl Pts',(-16.6607581789969,18.7827084437987,
-12.3348959628262));
#105636=CARTESIAN_POINT('Ctrl Pts',(-16.6736571237646,18.721543140939,-12.3387522016628));
#105637=CARTESIAN_POINT('Ctrl Pts',(-16.6867534426695,18.6693716591661,
-12.3421709146376));
#105638=CARTESIAN_POINT('Ctrl Pts',(-16.7104391642818,18.5882347163738,
-12.3476350995392));
#105639=CARTESIAN_POINT('Ctrl Pts',(-16.7197005676377,18.558901282634,-12.3496416651875));
#105640=CARTESIAN_POINT('Ctrl Pts',(-16.7713011535742,18.4070729532009,
-12.3601590876147));
#105641=CARTESIAN_POINT('Ctrl Pts',(-16.82418860556,18.2884440129881,-12.3688059240255));
#105642=CARTESIAN_POINT('Ctrl Pts',(-16.9306717659915,18.0985923569696,
-12.3828985068889));
#105643=CARTESIAN_POINT('Ctrl Pts',(-16.9785032679527,18.0245438908122,
-12.388473936393));
#105644=CARTESIAN_POINT('Ctrl Pts',(-17.0429891587583,17.9371901485475,
-12.3951372929841));
#105645=CARTESIAN_POINT('Ctrl Pts',(-17.055402945988,17.9208755178247,-12.3963860190921));
#105646=CARTESIAN_POINT('Ctrl Pts',(-17.0735170210324,17.8977735459857,
-12.3981609332677));
#105647=CARTESIAN_POINT('Ctrl Pts',(-17.0790257002158,17.8908380729079,
-12.3986946660552));
#105648=CARTESIAN_POINT('Ctrl Pts',(-17.0886518177924,17.8788736556669,
-12.3996170229862));
#105649=CARTESIAN_POINT('Ctrl Pts',(-17.0927491582007,17.8738287642508,
-12.4000064453681));
#105650=CARTESIAN_POINT('Ctrl Pts',(-17.100672643188,17.8641641805943,-12.4007534761138));
#105651=CARTESIAN_POINT('Ctrl Pts',(-17.1044953118977,17.859541731485,-12.4011112196286));
#105652=CARTESIAN_POINT('Ctrl Pts',(-17.1145624057919,17.8474732077344,
-12.4020464554971));
#105653=CARTESIAN_POINT('Ctrl Pts',(-17.1208385912739,17.840053717704,-12.4026226469948));
#105654=CARTESIAN_POINT('Ctrl Pts',(-17.1428054609125,17.8144449636284,
-12.4046159558711));
#105655=CARTESIAN_POINT('Ctrl Pts',(-17.1587548347637,17.796479314563,-12.4060223845816));
#105656=CARTESIAN_POINT('Ctrl Pts',(-17.2751316001207,17.6698007100448,
-12.4160079827468));
#105657=CARTESIAN_POINT('Ctrl Pts',(-17.386410726083,17.5716092324639,-12.4240787171203));
#105658=CARTESIAN_POINT('Ctrl Pts',(-17.5447466168555,17.4589991622943,
-12.4346304835519));
#105659=CARTESIAN_POINT('Ctrl Pts',(-17.5833272620597,17.4334222395349,
-12.4371410213788));
#105660=CARTESIAN_POINT('Ctrl Pts',(-17.6834791700664,17.3716545246044,
-12.4435777414851));
#105661=CARTESIAN_POINT('Ctrl Pts',(-17.7460962079574,17.3372790125278,
-12.4475279674693));
#105662=CARTESIAN_POINT('Ctrl Pts',(-17.8405333843261,17.2914861123943,
-12.4535472390394));
#105663=CARTESIAN_POINT('Ctrl Pts',(-17.8710846401087,17.2775592965727,
-12.4555037594948));
#105664=CARTESIAN_POINT('Ctrl Pts',(-17.9086747925823,17.2614921765919,
-12.4579374025227));
#105665=CARTESIAN_POINT('Ctrl Pts',(-17.9154122191964,17.2586535929542,
-12.4583746100309));
#105666=CARTESIAN_POINT('Ctrl Pts',(-17.925974092016,17.2542679920748,-12.4590617844941));
#105667=CARTESIAN_POINT('Ctrl Pts',(-17.9297886608853,17.2526971275658,
-12.4593103307196));
#105668=CARTESIAN_POINT('Ctrl Pts',(-17.9369125936265,17.2497877702468,
-12.4597752262529));
#105669=CARTESIAN_POINT('Ctrl Pts',(-17.9402207598512,17.2484464947928,
-12.4599914043886));
#105670=CARTESIAN_POINT('Ctrl Pts',(-17.9477608880499,17.2454115800384,
-12.4604847862257));
#105671=CARTESIAN_POINT('Ctrl Pts',(-17.9519949205355,17.2437232445228,
-12.4607623038403));
#105672=CARTESIAN_POINT('Ctrl Pts',(-17.963017283664,17.2393692438376,-12.4614859101291));
#105673=CARTESIAN_POINT('Ctrl Pts',(-17.9698139289861,17.2367249855006,
-12.4619332341893));
#105674=CARTESIAN_POINT('Ctrl Pts',(-18.0131755332702,17.2201124589298,
-12.4647936639114));
#105675=CARTESIAN_POINT('Ctrl Pts',(-18.0501058423478,17.2071263895655,
-12.4672594017656));
#105676=CARTESIAN_POINT('Ctrl Pts',(-18.0991267188595,17.191401696334,-12.4705518240767));
#105677=CARTESIAN_POINT('Ctrl Pts',(-18.1109139992187,17.1877340223886,
-12.471344966723));
#105678=CARTESIAN_POINT('Ctrl Pts',(-18.1458487460221,17.1771981247549,
-12.4736987158397));
#105679=CARTESIAN_POINT('Ctrl Pts',(-18.1690820010302,17.1706226923207,
-12.4752680034453));
#105680=CARTESIAN_POINT('Ctrl Pts',(-18.3317803114042,17.1275679579354,
-12.486263746072));
#105681=CARTESIAN_POINT('Ctrl Pts',(-18.474555156648,17.1050172913893,-12.4959108700233));
#105682=CARTESIAN_POINT('Ctrl Pts',(-18.6802311390641,17.0937805087175,
-12.5092191237075));
#105683=CARTESIAN_POINT('Ctrl Pts',(-18.742071142451,17.0931129746865,-12.5131507151506));
#105684=CARTESIAN_POINT('Ctrl Pts',(-18.8410951749605,17.0963823391104,
-12.5193243378294));
#105685=CARTESIAN_POINT('Ctrl Pts',(-18.8782965770677,17.0985947351868,
-12.5216162848772));
#105686=CARTESIAN_POINT('Ctrl Pts',(-18.9265161335453,17.1027423009678,
-12.524553380184));
#105687=CARTESIAN_POINT('Ctrl Pts',(-18.9376025846519,17.1037840684572,
-12.5252263607198));
#105688=CARTESIAN_POINT('Ctrl Pts',(-18.9556144881182,17.1056200820621,
-12.5263161115541));
#105689=CARTESIAN_POINT('Ctrl Pts',(-18.9625450379386,17.1063611360517,
-12.5267345477325));
#105690=CARTESIAN_POINT('Ctrl Pts',(-18.9758627017549,17.1078516961695,
-12.527536971656));
#105691=CARTESIAN_POINT('Ctrl Pts',(-18.982250298083,17.1085961031914,-12.5279211153193));
#105692=CARTESIAN_POINT('Ctrl Pts',(-18.9968632870301,17.1103666193308,
-12.5287983086816));
#105693=CARTESIAN_POINT('Ctrl Pts',(-19.005086276883,17.1114119591885,-12.529290746441));
#105694=CARTESIAN_POINT('Ctrl Pts',(-19.0269054855044,17.1143160272117,
-12.5305944022915));
#105695=CARTESIAN_POINT('Ctrl Pts',(-19.0404902723101,17.1162587196999,
-12.5314029686364));
#105696=CARTESIAN_POINT('Ctrl Pts',(-19.1432879122264,17.1319807392357,
-12.5374998057136));
#105697=CARTESIAN_POINT('Ctrl Pts',(-19.2315620098317,17.151322211414,-12.5426055874753));
#105698=CARTESIAN_POINT('Ctrl Pts',(-19.4524107327221,17.2147454339367,
-12.5553255610993));
#105699=CARTESIAN_POINT('Ctrl Pts',(-19.5823414515173,17.2664020464035,
-12.5627450233497));
#105700=CARTESIAN_POINT('Ctrl Pts',(-19.7553604186876,17.3558533540198,
-12.5735037596431));
#105701=CARTESIAN_POINT('Ctrl Pts',(-19.8034593726833,17.3831592019586,
-12.5766018660388));
#105702=CARTESIAN_POINT('Ctrl Pts',(-19.8746319756805,17.4273355050485,
-12.581433751383));
#105703=CARTESIAN_POINT('Ctrl Pts',(-19.8985260758143,17.4428430009495,
-12.5831003971749));
#105704=CARTESIAN_POINT('Ctrl Pts',(-19.9278456879129,17.4627237955927,
-12.5852110176198));
#105705=CARTESIAN_POINT('Ctrl Pts',(-19.9335733773526,17.4666488533715,
-12.5856265097071));
#105706=CARTESIAN_POINT('Ctrl Pts',(-19.942606418798,17.4729045247935,-12.5862869921594));
#105707=CARTESIAN_POINT('Ctrl Pts',(-19.9459246375478,17.4752165950882,
-12.5865307376505));
#105708=CARTESIAN_POINT('Ctrl Pts',(-19.9521703955418,17.4795951575709,
-12.5869916929442));
#105709=CARTESIAN_POINT('Ctrl Pts',(-19.955099320414,17.4816595795131,-12.5872087621034));
#105710=CARTESIAN_POINT('Ctrl Pts',(-19.9617838702117,17.4863965628554,
-12.5877062306935));
#105711=CARTESIAN_POINT('Ctrl Pts',(-19.9655360125942,17.4890739574188,
-12.5879869595359));
#105712=CARTESIAN_POINT('Ctrl Pts',(-19.9754745481618,17.4962148412065,
-12.5887344477188));
#105713=CARTESIAN_POINT('Ctrl Pts',(-19.9816455446555,17.5006995043469,
-12.5892026121565));
#105714=CARTESIAN_POINT('Ctrl Pts',(-20.0247025244535,17.532347439808,-12.592496746876));
#105715=CARTESIAN_POINT('Ctrl Pts',(-20.0607197676149,17.560666277959,-12.5953947809447));
#105716=CARTESIAN_POINT('Ctrl Pts',(-20.1245701489341,17.6143106424667,
-12.6007562174839));
#105717=CARTESIAN_POINT('Ctrl Pts',(-20.1527028149936,17.6392543652428,
-12.6032035793863));
#105718=CARTESIAN_POINT('Ctrl Pts',(-20.275819313844,17.7544146700018,-12.6142536960959));
#105719=CARTESIAN_POINT('Ctrl Pts',(-20.362979256332,17.8525899411399,-12.6229968955414));
#105720=CARTESIAN_POINT('Ctrl Pts',(-20.4927972962823,18.0294209959865,
-12.6372013617079));
#105721=CARTESIAN_POINT('Ctrl Pts',(-20.5405828374066,18.1038601044472,
-12.6427967603634));
#105722=CARTESIAN_POINT('Ctrl Pts',(-20.5935715881277,18.1990196359036,
-12.6494812675744));
#105723=CARTESIAN_POINT('Ctrl Pts',(-20.6033012801272,18.2171068873108,
-12.6507323208643));
#105724=CARTESIAN_POINT('Ctrl Pts',(-20.6168513893215,18.2431992949443,
-12.652509930538));
#105725=CARTESIAN_POINT('Ctrl Pts',(-20.6208868700635,18.2510908885253,
-12.6530440631504));
#105726=CARTESIAN_POINT('Ctrl Pts',(-20.6277957964382,18.2648135838021,
-12.6539668888513));
#105727=CARTESIAN_POINT('Ctrl Pts',(-20.6306921431392,18.2706329607962,
-12.6543563824189));
#105728=CARTESIAN_POINT('Ctrl Pts',(-20.6362088781865,18.2818464365402,
-12.655103395696));
#105729=CARTESIAN_POINT('Ctrl Pts',(-20.6388332360891,18.2872385023335,
-12.6554610512908));
#105730=CARTESIAN_POINT('Ctrl Pts',(-20.6456466883697,18.3013900757899,
-12.6563957159273));
#105731=CARTESIAN_POINT('Ctrl Pts',(-20.6497985245005,18.3101674441554,
-12.656971427242));
#105732=CARTESIAN_POINT('Ctrl Pts',(-20.6639911334815,18.3407138870399,
-12.6589614020745));
#105733=CARTESIAN_POINT('Ctrl Pts',(-20.6737226592922,18.3626252198241,
-12.6603650251453));
#105734=CARTESIAN_POINT('Ctrl Pts',(-20.6971018560742,18.4177720291238,
-12.6638422012189));
#105735=CARTESIAN_POINT('Ctrl Pts',(-20.7102719365412,18.4511802539283,
-12.6658991156327));
#105736=CARTESIAN_POINT('Ctrl Pts',(-20.7225805288028,18.4848894846743,
-12.6679318969538));
#105737=CARTESIAN_POINT('',(-20.853822991173,19.2120774369757,-11.6890562790225));
#105738=CARTESIAN_POINT('Ctrl Pts',(-20.7242505411024,18.4842642021379,
-12.4443820858314));
#105739=CARTESIAN_POINT('Ctrl Pts',(-20.5136267642773,17.9235819449507,
-12.408272473254));
#105740=CARTESIAN_POINT('Ctrl Pts',(-19.5197099237742,16.8917269399042,
-12.329770925116));
#105741=CARTESIAN_POINT('Ctrl Pts',(-17.2597752565566,17.1878855805931,
-12.2088774414178));
#105742=CARTESIAN_POINT('Ctrl Pts',(-16.2349110453346,19.3555162442872,
-12.0817016347362));
#105743=CARTESIAN_POINT('Ctrl Pts',(-17.5028058390645,21.3905622235373,
-11.9545258280549));
#105744=CARTESIAN_POINT('Ctrl Pts',(-19.9002448589247,21.4259951415803,
-11.8273500213734));
#105745=CARTESIAN_POINT('Ctrl Pts',(-20.8239162970475,20.0366853799179,
-11.7388601716959));
#105746=CARTESIAN_POINT('Ctrl Pts',(-20.8542040955766,19.273466074897,-11.692762257579));
#105747=CARTESIAN_POINT('Ctrl Pts',(-20.853822991173,19.2120774369757,-11.6890562790225));
#105748=CARTESIAN_POINT('Ctrl Pts',(-20.8509997772511,19.2119711430765,
-11.6906773760522));
#105749=CARTESIAN_POINT('Ctrl Pts',(-20.8510795350122,19.038106790205,-11.6794937446562));
#105750=CARTESIAN_POINT('Ctrl Pts',(-20.829741896744,18.8648839271554,-11.6677631723301));
#105751=CARTESIAN_POINT('Ctrl Pts',(-20.7726123086137,18.637001790048,-11.6525929998784));
#105752=CARTESIAN_POINT('Ctrl Pts',(-20.7552164348725,18.5784659652781,
-11.648712755995));
#105753=CARTESIAN_POINT('Ctrl Pts',(-20.7311768486813,18.50876455386,-11.6441198123401));
#105754=CARTESIAN_POINT('Ctrl Pts',(-20.7269322965609,18.4968075654787,
-11.6433328539868));
#105755=CARTESIAN_POINT('Ctrl Pts',(-20.7225806143616,18.4848897189921,
-11.6425493859455));
#105756=CARTESIAN_POINT('Origin',(-18.734,19.211,0.));
#105757=CARTESIAN_POINT('',(-20.7225806140666,18.4848897181842,-10.844119113415));
#105758=CARTESIAN_POINT('',(-20.7225806135353,18.4848897167291,-11.0644159212905));
#105759=CARTESIAN_POINT('',(-20.7225806137986,18.4848897174502,0.));
#105760=CARTESIAN_POINT('Ctrl Pts',(-20.7225806135353,18.4848897167291,
-11.0644159212905));
#105761=CARTESIAN_POINT('Ctrl Pts',(-20.7579845105336,18.5818495103536,
-11.0708124284518));
#105762=CARTESIAN_POINT('Ctrl Pts',(-20.7862468955592,18.6812615260696,
-11.0775606980553));
#105763=CARTESIAN_POINT('Ctrl Pts',(-20.8362075141281,18.9228812641263,
-11.0938351530036));
#105764=CARTESIAN_POINT('Ctrl Pts',(-20.8509047690515,19.066044097594,-11.1033537530625));
#105765=CARTESIAN_POINT('Ctrl Pts',(-20.8510404641561,19.2715966101103,
-11.1164063739387));
#105766=CARTESIAN_POINT('Ctrl Pts',(-20.8483582574222,19.3335670541364,
-11.1202674161294));
#105767=CARTESIAN_POINT('Ctrl Pts',(-20.8418780039395,19.4077067100225,
-11.1248002039059));
#105768=CARTESIAN_POINT('Ctrl Pts',(-20.8406878629333,19.4200680935513,
-11.1255531154824));
#105769=CARTESIAN_POINT('Ctrl Pts',(-20.8385539134696,19.4403590526985,
-11.1267844866857));
#105770=CARTESIAN_POINT('Ctrl Pts',(-20.8376739011466,19.4482949011569,
-11.1272649420936));
#105771=CARTESIAN_POINT('Ctrl Pts',(-20.8360103028606,19.4625598420287,
-11.1281265864217));
#105772=CARTESIAN_POINT('Ctrl Pts',(-20.8352429787453,19.4688906999214,
-11.1285082828655));
#105773=CARTESIAN_POINT('Ctrl Pts',(-20.8335469912837,19.4823732454618,
-11.129319698516));
#105774=CARTESIAN_POINT('Ctrl Pts',(-20.8326103655088,19.4895238638156,
-11.1297491613722));
#105775=CARTESIAN_POINT('Ctrl Pts',(-20.8299874443797,19.5087836537127,
-11.1309035996037));
#105776=CARTESIAN_POINT('Ctrl Pts',(-20.8282327450459,19.5208833497365,
-11.1316264082981));
#105777=CARTESIAN_POINT('Ctrl Pts',(-20.8189028588071,19.5815155976498,
-11.1352369428666));
#105778=CARTESIAN_POINT('Ctrl Pts',(-20.8097446645727,19.6297915688479,
-11.1380741497991));
#105779=CARTESIAN_POINT('Ctrl Pts',(-20.7784289229906,19.7683456731649,
-11.1461497914733));
#105780=CARTESIAN_POINT('Ctrl Pts',(-20.7519966827993,19.8575409818251,
-11.1512603952119));
#105781=CARTESIAN_POINT('Ctrl Pts',(-20.66234994469,20.1001681817574,-11.1653489191763));
#105782=CARTESIAN_POINT('Ctrl Pts',(-20.5868669495829,20.2483141193899,
-11.1741493678622));
#105783=CARTESIAN_POINT('Ctrl Pts',(-20.4871421973997,20.3977505899914,
-11.1847107456619));
#105784=CARTESIAN_POINT('Ctrl Pts',(-20.4792655410229,20.4093040912681,
-11.1855394060308));
#105785=CARTESIAN_POINT('Ctrl Pts',(-20.4681194497217,20.4253101871166,
-11.1867057080819));
#105786=CARTESIAN_POINT('Ctrl Pts',(-20.4649459694673,20.4298295802376,
-11.1870370775382));
#105787=CARTESIAN_POINT('Ctrl Pts',(-20.4598136883828,20.4370780552825,
-11.1875719580491));
#105788=CARTESIAN_POINT('Ctrl Pts',(-20.4578659860817,20.4398150171287,
-11.1877747111508));
#105789=CARTESIAN_POINT('Ctrl Pts',(-20.453774817535,20.4455351639029,-11.1882001338125));
#105790=CARTESIAN_POINT('Ctrl Pts',(-20.4516300989897,20.4485174084696,
-11.1884228927116));
#105791=CARTESIAN_POINT('Ctrl Pts',(-20.4464076165461,20.4557395730299,
-11.1889646604425));
#105792=CARTESIAN_POINT('Ctrl Pts',(-20.443321864483,20.4599736635019,-11.1892842171977));
#105793=CARTESIAN_POINT('Ctrl Pts',(-20.4323912729261,20.4748556101276,
-11.1904141130635));
#105794=CARTESIAN_POINT('Ctrl Pts',(-20.4244625874357,20.4854411086334,
-11.1912299895));
#105795=CARTESIAN_POINT('Ctrl Pts',(-20.3764349025933,20.5483255775225,
-11.1961467361627));
#105796=CARTESIAN_POINT('Ctrl Pts',(-20.3340141770669,20.5987986407266,
-11.2003844694808));
#105797=CARTESIAN_POINT('Ctrl Pts',(-20.2240817826416,20.7178479439201,
-11.2109621072753));
#105798=CARTESIAN_POINT('Ctrl Pts',(-20.1541137643016,20.7839625451605,
-11.2173577785994));
#105799=CARTESIAN_POINT('Ctrl Pts',(-19.9712621247926,20.934565486735,-11.2329413186586));
#105800=CARTESIAN_POINT('Ctrl Pts',(-19.8539618969555,21.0129972743543,
-11.2419898570745));
#105801=CARTESIAN_POINT('Ctrl Pts',(-19.717114103807,21.0859346183671,-11.2514585061595));
#105802=CARTESIAN_POINT('Ctrl Pts',(-19.7044367168009,21.0925275067495,
-11.252326436666));
#105803=CARTESIAN_POINT('Ctrl Pts',(-19.6841535555004,21.1028162426984,
-11.253700687019));
#105804=CARTESIAN_POINT('Ctrl Pts',(-19.6765908815097,21.1065956606042,
-11.2542099345473));
#105805=CARTESIAN_POINT('Ctrl Pts',(-19.6632128769917,21.1131814103799,
-11.2551052974857));
#105806=CARTESIAN_POINT('Ctrl Pts',(-19.6574070058504,21.1160066119941,
-11.2554920689526));
#105807=CARTESIAN_POINT('Ctrl Pts',(-19.6453717560817,21.1217951503559,
-11.2562901406439));
#105808=CARTESIAN_POINT('Ctrl Pts',(-19.6391406299403,21.1247546933111,
-11.2567013054508));
#105809=CARTESIAN_POINT('Ctrl Pts',(-19.6231088252015,21.1322733622453,
-11.257754043659));
#105810=CARTESIAN_POINT('Ctrl Pts',(-19.6132874172106,21.1367880153378,
-11.2583940755956));
#105811=CARTESIAN_POINT('Ctrl Pts',(-19.5721500245015,21.1553175190691,
-11.2610549656036));
#105812=CARTESIAN_POINT('Ctrl Pts',(-19.5405292286959,21.1686457489669,
-11.2630522898664));
#105813=CARTESIAN_POINT('Ctrl Pts',(-19.4573061357852,21.2013654524187,
-11.2681969868866));
#105814=CARTESIAN_POINT('Ctrl Pts',(-19.4052450006245,21.2195211462679,
-11.2713049582114));
#105815=CARTESIAN_POINT('Ctrl Pts',(-19.2479504672115,21.2675752924697,
-11.2804500881202));
#105816=CARTESIAN_POINT('Ctrl Pts',(-19.141048083626,21.2913749077612,-11.2863385197153));
#105817=CARTESIAN_POINT('Ctrl Pts',(-18.9869092014435,21.3133494929698,
-11.2948153695867));
#105818=CARTESIAN_POINT('Ctrl Pts',(-18.9408313281924,21.3183815524446,
-11.2973493293416));
#105819=CARTESIAN_POINT('Ctrl Pts',(-18.8732956181031,21.3235206250554,
-11.3011064779075));
#105820=CARTESIAN_POINT('Ctrl Pts',(-18.8519413958002,21.3248203435619,
-11.3023007734537));
#105821=CARTESIAN_POINT('Ctrl Pts',(-18.7787711723302,21.3281616443893,
-11.3064252218375));
#105822=CARTESIAN_POINT('Ctrl Pts',(-18.726905702043,21.3286228685763,-11.3094038698376));
#105823=CARTESIAN_POINT('Ctrl Pts',(-18.6664284876887,21.3269390361204,
-11.3129946257956));
#105824=CARTESIAN_POINT('Ctrl Pts',(-18.6577782873495,21.3266450927753,
-11.3135110326991));
#105825=CARTESIAN_POINT('Ctrl Pts',(-18.6446646719969,21.3261189501094,
-11.3142984925047));
#105826=CARTESIAN_POINT('Ctrl Pts',(-18.6401996689471,21.3259256419538,
-11.3145674193035));
#105827=CARTESIAN_POINT('Ctrl Pts',(-18.6321761092844,21.32555281109,-11.3150521828745));
#105828=CARTESIAN_POINT('Ctrl Pts',(-18.628617367591,21.3253784420222,-11.3152677282955));
#105829=CARTESIAN_POINT('Ctrl Pts',(-18.6208738442635,21.3249794311378,
-11.3157379127352));
#105830=CARTESIAN_POINT('Ctrl Pts',(-18.6166893381185,21.3247513501573,
-11.3159927369557));
#105831=CARTESIAN_POINT('Ctrl Pts',(-18.6049073174612,21.3240740648805,
-11.3167122654164));
#105832=CARTESIAN_POINT('Ctrl Pts',(-18.5973115984563,21.323596317615,-11.3171785233143));
#105833=CARTESIAN_POINT('Ctrl Pts',(-18.5512927044935,21.3204526531747,
-11.3200171573825));
#105834=CARTESIAN_POINT('Ctrl Pts',(-18.5129481501408,21.3167796894321,
-11.322440642795));
#105835=CARTESIAN_POINT('Ctrl Pts',(-18.3856325083811,21.3010688941811,
-11.3306356250005));
#105836=CARTESIAN_POINT('Ctrl Pts',(-18.2973319041579,21.2844191284673,
-11.3365582415861));
#105837=CARTESIAN_POINT('Ctrl Pts',(-18.0441487550144,21.2197859751892,
-11.3538252853405));
#105838=CARTESIAN_POINT('Ctrl Pts',(-17.8836768076623,21.157301178375,-11.3650716755558));
#105839=CARTESIAN_POINT('Ctrl Pts',(-17.7119976962816,21.0651146703995,
-11.3770690601322));
#105840=CARTESIAN_POINT('Ctrl Pts',(-17.6916893340496,21.0537746642382,
-11.3784891042215));
#105841=CARTESIAN_POINT('Ctrl Pts',(-17.6632763498872,21.0372890885449,
-11.3804777712047));
#105842=CARTESIAN_POINT('Ctrl Pts',(-17.6550140828128,21.0324198761118,
-11.381056296067));
#105843=CARTESIAN_POINT('Ctrl Pts',(-17.6416584027079,21.0244261862462,
-11.3819919316247));
#105844=CARTESIAN_POINT('Ctrl Pts',(-17.6365446974493,21.0213360346021,
-11.3823502864271));
#105845=CARTESIAN_POINT('Ctrl Pts',(-17.6258801442078,21.0148297772442,
-11.3830978964969));
#105846=CARTESIAN_POINT('Ctrl Pts',(-17.6203318449393,21.0114095983811,
-11.3834869973548));
#105847=CARTESIAN_POINT('Ctrl Pts',(-17.6071923222302,21.0032259266913,
-11.3844088800682));
#105848=CARTESIAN_POINT('Ctrl Pts',(-17.5996153382607,20.9984397214894,
-11.3849408172334));
#105849=CARTESIAN_POINT('Ctrl Pts',(-17.574294126043,20.9822190376323,-11.386719781641));
#105850=CARTESIAN_POINT('Ctrl Pts',(-17.5566902158126,20.9705670811004,
-11.387958712242));
#105851=CARTESIAN_POINT('Ctrl Pts',(-17.4624601024923,20.9061491620252,
-11.3946072690356));
#105852=CARTESIAN_POINT('Ctrl Pts',(-17.3891969459869,20.8486361132048,
-11.3998312982591));
#105853=CARTESIAN_POINT('Ctrl Pts',(-17.2047827469816,20.6831179258877,
-11.4134775863346));
#105854=CARTESIAN_POINT('Ctrl Pts',(-17.1013074763857,20.5674458252306,
-11.4216609279055));
#105855=CARTESIAN_POINT('Ctrl Pts',(-16.9802032397533,20.3979122248355,
-11.433375191727));
#105856=CARTESIAN_POINT('Ctrl Pts',(-16.9507093259367,20.3531195403558,
-11.4364511156338));
#105857=CARTESIAN_POINT('Ctrl Pts',(-16.9184242281447,20.2997837226892,
-11.4401507752034));
#105858=CARTESIAN_POINT('Ctrl Pts',(-16.9139450443887,20.2922794878011,
-11.440672140623));
#105859=CARTESIAN_POINT('Ctrl Pts',(-16.9072365356623,20.2808805455965,
-11.4414656846782));
#105860=CARTESIAN_POINT('Ctrl Pts',(-16.9049728563827,20.2770060241592,
-11.4417356876353));
#105861=CARTESIAN_POINT('Ctrl Pts',(-16.9009333090442,20.2700411750234,
-11.4422215935871));
#105862=CARTESIAN_POINT('Ctrl Pts',(-16.8991529127134,20.2669535358476,
-11.4424371990941));
#105863=CARTESIAN_POINT('Ctrl Pts',(-16.8953030730426,20.2602378451347,
-11.4429065810143));
#105864=CARTESIAN_POINT('Ctrl Pts',(-16.8932365938309,20.2566082089763,
-11.4431605375263));
#105865=CARTESIAN_POINT('Ctrl Pts',(-16.8874667558539,20.2464037482004,
-11.4438752201855));
#105866=CARTESIAN_POINT('Ctrl Pts',(-16.8837878339844,20.2398152799768,
-11.4443374673691));
#105867=CARTESIAN_POINT('Ctrl Pts',(-16.862096123084,20.2004756093816,-11.4471017330519));
#105868=CARTESIAN_POINT('Ctrl Pts',(-16.844919248195,20.1672738219225,-11.449451863414));
#105869=CARTESIAN_POINT('Ctrl Pts',(-16.7914740506213,20.0569023890397,
-11.457278254883));
#105870=CARTESIAN_POINT('Ctrl Pts',(-16.7589884595079,19.9779976928646,
-11.4628922166034));
#105871=CARTESIAN_POINT('Ctrl Pts',(-16.673653546085,19.7290072475013,-11.4802802430761));
#105872=CARTESIAN_POINT('Ctrl Pts',(-16.6374025011106,19.5540195074303,
-11.4919745855397));
#105873=CARTESIAN_POINT('Ctrl Pts',(-16.6216992387344,19.3538082222448,
-11.5043334514449));
#105874=CARTESIAN_POINT('Ctrl Pts',(-16.6202838466278,19.3310532429137,
-11.5057249444752));
#105875=CARTESIAN_POINT('Ctrl Pts',(-16.6187990464069,19.2987749728946,
-11.5076808587237));
#105876=CARTESIAN_POINT('Ctrl Pts',(-16.6184259253278,19.2892678678961,
-11.5082547466318));
#105877=CARTESIAN_POINT('Ctrl Pts',(-16.6179232947684,19.2738005683485,
-11.5091849231686));
#105878=CARTESIAN_POINT('Ctrl Pts',(-16.61775484906,19.2678418513155,-11.5095424274324));
#105879=CARTESIAN_POINT('Ctrl Pts',(-16.617454632156,19.2553547260921,-11.5102898801202));
#105880=CARTESIAN_POINT('Ctrl Pts',(-16.6173278921667,19.2488262509701,
-11.5106796670301));
#105881=CARTESIAN_POINT('Ctrl Pts',(-16.6170978946007,19.2332705124533,
-11.5116061146544));
#105882=CARTESIAN_POINT('Ctrl Pts',(-16.617022171013,19.2242429223034,-11.5121419078479));
#105883=CARTESIAN_POINT('Ctrl Pts',(-16.6169613931839,19.1937172004032,
-11.5139475471835));
#105884=CARTESIAN_POINT('Ctrl Pts',(-16.6172460522855,19.1722194270122,
-11.515208956021));
#105885=CARTESIAN_POINT('Ctrl Pts',(-16.6229706616906,18.9712254259447,
-11.5269162695944));
#105886=CARTESIAN_POINT('Ctrl Pts',(-16.6508996755496,18.7931044056527,
-11.53656416354));
#105887=CARTESIAN_POINT('Ctrl Pts',(-16.734548283313,18.50504787237,-11.5528890786301));
#105888=CARTESIAN_POINT('Ctrl Pts',(-16.7779045786298,18.3925515737823,
-11.5594929098358));
#105889=CARTESIAN_POINT('Ctrl Pts',(-16.8347306148411,18.2758235145013,
-11.5671871224211));
#105890=CARTESIAN_POINT('Ctrl Pts',(-16.8389463840805,18.2673098805152,
-11.5677534037208));
#105891=CARTESIAN_POINT('Ctrl Pts',(-16.8452798834752,18.2547331377544,
-11.5685979463252));
#105892=CARTESIAN_POINT('Ctrl Pts',(-16.8473537985084,18.2506479292017,
-11.568873533089));
#105893=CARTESIAN_POINT('Ctrl Pts',(-16.8510681791836,18.2433897908696,
-11.5693654680895));
#105894=CARTESIAN_POINT('Ctrl Pts',(-16.8527034300416,18.2402142490287,
-11.5695814871177));
#105895=CARTESIAN_POINT('Ctrl Pts',(-16.8562374571197,18.2333938819136,
-11.5700471661826));
#105896=CARTESIAN_POINT('Ctrl Pts',(-16.8581387844127,18.2297504961754,
-11.5702969816558));
#105897=CARTESIAN_POINT('Ctrl Pts',(-16.8634187448824,18.2197042925756,
-11.5709886828184));
#105898=CARTESIAN_POINT('Ctrl Pts',(-16.8668195948237,18.2133133043919,
-11.5714319390947));
#105899=CARTESIAN_POINT('Ctrl Pts',(-16.8856710911908,18.178320955691,-11.573876105825));
#105900=CARTESIAN_POINT('Ctrl Pts',(-16.9017452797992,18.1500626147046,
-11.5759132922613));
#105901=CARTESIAN_POINT('Ctrl Pts',(-17.002156459529,17.9826322821542,-11.5883186817831));
#105902=CARTESIAN_POINT('Ctrl Pts',(-17.1016589033143,17.8531959753851,
-11.599277255974));
#105903=CARTESIAN_POINT('Ctrl Pts',(-17.2963410340352,17.6526477544578,
-11.6175341145785));
#105904=CARTESIAN_POINT('Ctrl Pts',(-17.3844807291122,17.5757230941183,
-11.6249726280474));
#105905=CARTESIAN_POINT('Ctrl Pts',(-17.4900556557493,17.4979628239627,
-11.6329791293076));
#105906=CARTESIAN_POINT('Ctrl Pts',(-17.5016671086332,17.4895908218166,
-11.6338486392411));
#105907=CARTESIAN_POINT('Ctrl Pts',(-17.5202763420332,17.4764581345465,
-11.6352249096113));
#105908=CARTESIAN_POINT('Ctrl Pts',(-17.5272191397605,17.4716206395595,
-11.6357346111356));
#105909=CARTESIAN_POINT('Ctrl Pts',(-17.5395114379058,17.4631648305526,
-11.6366305022658));
#105910=CARTESIAN_POINT('Ctrl Pts',(-17.5448488054406,17.4595291488458,
-11.6370173503646));
#105911=CARTESIAN_POINT('Ctrl Pts',(-17.5559191274432,17.4520622522175,
-11.6378153218571));
#105912=CARTESIAN_POINT('Ctrl Pts',(-17.5616543368674,17.448234504898,-11.6382263111067));
#105913=CARTESIAN_POINT('Ctrl Pts',(-17.5764165323491,17.438485950845,-11.6392780656892));
#105914=CARTESIAN_POINT('Ctrl Pts',(-17.5854703612653,17.4326060013278,
-11.639917295209));
#105915=CARTESIAN_POINT('Ctrl Pts',(-17.6233835937971,17.4083938015694,
-11.6425703968292));
#105916=CARTESIAN_POINT('Ctrl Pts',(-17.6526409352452,17.3906921479872,
-11.6445609105989));
#105917=CARTESIAN_POINT('Ctrl Pts',(-17.7299177863768,17.3464581417023,
-11.64968411544));
#105918=CARTESIAN_POINT('Ctrl Pts',(-17.7785631999672,17.3210691568222,
-11.6527778353638));
#105919=CARTESIAN_POINT('Ctrl Pts',(-17.9986788056892,17.2168604124533,
-11.6663221766345));
#105920=CARTESIAN_POINT('Ctrl Pts',(-18.1792199646723,17.1592945482625,
-11.6761688900735));
#105921=CARTESIAN_POINT('Ctrl Pts',(-18.4061017136453,17.119130997804,-11.6892631781547));
#105922=CARTESIAN_POINT('Ctrl Pts',(-18.4474294347507,17.1130700683978,
-11.6916799805745));
#105923=CARTESIAN_POINT('Ctrl Pts',(-18.4962811643947,17.1073760113794,
-11.694602067743));
#105924=CARTESIAN_POINT('Ctrl Pts',(-18.5036605627018,17.1065552109255,
-11.695045217215));
#105925=CARTESIAN_POINT('Ctrl Pts',(-18.5156165850949,17.1052889972477,
-11.6957662516826));
#105926=CARTESIAN_POINT('Ctrl Pts',(-18.5201906832431,17.1048196377873,
-11.6960428244561));
#105927=CARTESIAN_POINT('Ctrl Pts',(-18.5283222704429,17.1040119977157,
-11.69653584019));
#105928=CARTESIAN_POINT('Ctrl Pts',(-18.5318791236986,17.1036678189359,
-11.6967519483542));
#105929=CARTESIAN_POINT('Ctrl Pts',(-18.5395176016138,17.1029481987413,
-11.6972170467616));
#105930=CARTESIAN_POINT('Ctrl Pts',(-18.5435993894904,17.1025756103358,
-11.6974661883741));
#105931=CARTESIAN_POINT('Ctrl Pts',(-18.554844328683,17.1015820845437,-11.6981541704597));
#105932=CARTESIAN_POINT('Ctrl Pts',(-18.5620095234353,17.100985789345,-11.6985943578276));
#105933=CARTESIAN_POINT('Ctrl Pts',(-18.6008731439588,17.0979507859534,
-11.7009912097525));
#105934=CARTESIAN_POINT('Ctrl Pts',(-18.6326186018115,17.0961900083692,
-11.7029825472233));
#105935=CARTESIAN_POINT('Ctrl Pts',(-18.8276392870077,17.0897739414869,
-11.7153728631945));
#105936=CARTESIAN_POINT('Ctrl Pts',(-18.9909572686806,17.1033138040003,
-11.7263739028625));
#105937=CARTESIAN_POINT('Ctrl Pts',(-19.2657918897069,17.158544528777,-11.7446861638805));
#105938=CARTESIAN_POINT('Ctrl Pts',(-19.3783966820372,17.1910651417365,
-11.7521391043154));
#105939=CARTESIAN_POINT('Ctrl Pts',(-19.5011180995793,17.2378240377561,
-11.7601580957281));
#105940=CARTESIAN_POINT('Ctrl Pts',(-19.5144314680354,17.2430517547101,
-11.7610268712044));
#105941=CARTESIAN_POINT('Ctrl Pts',(-19.5355324265156,17.251585211936,-11.7624022022785));
#105942=CARTESIAN_POINT('Ctrl Pts',(-19.5433547676538,17.2548033315233,
-11.7629116927266));
#105943=CARTESIAN_POINT('Ctrl Pts',(-19.5571145917463,17.2605608017561,
-11.7638073382533));
#105944=CARTESIAN_POINT('Ctrl Pts',(-19.5630600972131,17.2630805833315,
-11.7641941506921));
#105945=CARTESIAN_POINT('Ctrl Pts',(-19.5744693055324,17.2679776511708,
-11.7649361022921));
#105946=CARTESIAN_POINT('Ctrl Pts',(-19.5799346755131,17.270350874714,-11.7652913752427));
#105947=CARTESIAN_POINT('Ctrl Pts',(-19.5943386932351,17.2766779319188,
-11.7662273577707));
#105948=CARTESIAN_POINT('Ctrl Pts',(-19.6032601719841,17.2806706787676,
-11.7668067320043));
#105949=CARTESIAN_POINT('Ctrl Pts',(-19.6362975564567,17.2957318233745,
-11.7689512222639));
#105950=CARTESIAN_POINT('Ctrl Pts',(-19.6602329958321,17.3071918166191,
-11.7705028524968));
#105951=CARTESIAN_POINT('Ctrl Pts',(-19.719048608807,17.3367238841889,-11.774315361069));
#105952=CARTESIAN_POINT('Ctrl Pts',(-19.7536537925293,17.3553227311087,
-11.7765581797086));
#105953=CARTESIAN_POINT('Ctrl Pts',(-19.881612670487,17.4287562809325,-11.784882087309));
#105954=CARTESIAN_POINT('Ctrl Pts',(-19.9712357075821,17.4897628056551,
-11.7907658645788));
#105955=CARTESIAN_POINT('Ctrl Pts',(-20.162193736129,17.6424009371761,-11.8040415330628));
#105956=CARTESIAN_POINT('Ctrl Pts',(-20.2601157999815,17.7375005398172,
-11.8113988535014));
#105957=CARTESIAN_POINT('Ctrl Pts',(-20.3583117961853,17.8532283653158,
-11.8202986991472));
#105958=CARTESIAN_POINT('Ctrl Pts',(-20.3682779988764,17.8652407297263,
-11.8212220846294));
#105959=CARTESIAN_POINT('Ctrl Pts',(-20.381750003524,17.8818490267196,-11.8224999396963));
#105960=CARTESIAN_POINT('Ctrl Pts',(-20.3853714371822,17.886351081017,-11.8228464484126));
#105961=CARTESIAN_POINT('Ctrl Pts',(-20.3910999480515,17.8935325881788,
-11.823399473813));
#105962=CARTESIAN_POINT('Ctrl Pts',(-20.3932190925738,17.8962024408672,
-11.8236051336071));
#105963=CARTESIAN_POINT('Ctrl Pts',(-20.3975851129308,17.9017304366302,
-11.8240311140067));
#105964=CARTESIAN_POINT('Ctrl Pts',(-20.3998310708248,17.9045892452111,
-11.8242514995298));
#105965=CARTESIAN_POINT('Ctrl Pts',(-20.4051695365946,17.9114205585473,
-11.8247783135232));
#105966=CARTESIAN_POINT('Ctrl Pts',(-20.408255250054,17.9153983246562,-11.8250852187671));
#105967=CARTESIAN_POINT('Ctrl Pts',(-20.418634169762,17.9288766958081,-11.8261255400785));
#105968=CARTESIAN_POINT('Ctrl Pts',(-20.4258607732686,17.9384279738483,
-11.826863410319));
#105969=CARTESIAN_POINT('Ctrl Pts',(-20.5082141624011,18.0492144273899,
-11.8354246480051));
#105970=CARTESIAN_POINT('Ctrl Pts',(-20.5742271637865,18.1568942444952,
-11.8437557121081));
#105971=CARTESIAN_POINT('Ctrl Pts',(-20.6639654874019,18.3376911509954,
-11.8570944299295));
#105972=CARTESIAN_POINT('Ctrl Pts',(-20.6939974412518,18.4073544815339,
-11.8620973608283));
#105973=CARTESIAN_POINT('Ctrl Pts',(-20.721016234076,18.4806160848838,-11.8671696308045));
#105974=CARTESIAN_POINT('Ctrl Pts',(-20.7218001501807,18.4827522806762,
-11.8673173710366));
#105975=CARTESIAN_POINT('Ctrl Pts',(-20.7225806137507,18.4848897173191,
-11.8674650369494));
#105976=CARTESIAN_POINT('Ctrl Pts',(-20.7225806143616,18.4848897189921,
-11.6425493859455));
#105977=CARTESIAN_POINT('Ctrl Pts',(-20.7142679983043,18.4621241590236,
-11.6410527994022));
#105978=CARTESIAN_POINT('Ctrl Pts',(-20.7055644761456,18.4395014220629,
-11.6395689721133));
#105979=CARTESIAN_POINT('Ctrl Pts',(-20.6923109675864,18.4067423615176,
-11.6374245029276));
#105980=CARTESIAN_POINT('Ctrl Pts',(-20.6880673194941,18.3964859650925,
-11.63675370293));
#105981=CARTESIAN_POINT('Ctrl Pts',(-20.6810308679606,18.3798512349006,
-11.6356666001178));
#105982=CARTESIAN_POINT('Ctrl Pts',(-20.6782869568271,18.3734525674138,
-11.6352486465248));
#105983=CARTESIAN_POINT('Ctrl Pts',(-20.6729468957414,18.3611674735963,
-11.6344465570414));
#105984=CARTESIAN_POINT('Ctrl Pts',(-20.6703553845417,18.3552791263467,
-11.6340622683996));
#105985=CARTESIAN_POINT('Ctrl Pts',(-20.6643565558064,18.3418155784917,
-11.6331839240812));
#105986=CARTESIAN_POINT('Ctrl Pts',(-20.6609314031985,18.3342484037618,
-11.6326904859046));
#105987=CARTESIAN_POINT('Ctrl Pts',(-20.6517054394834,18.3141807586619,
-11.6313824212375));
#105988=CARTESIAN_POINT('Ctrl Pts',(-20.6458268972398,18.3017163079416,
-11.630570475544));
#105989=CARTESIAN_POINT('Ctrl Pts',(-20.5995489628504,18.2060249935389,
-11.6243392030782));
#105990=CARTESIAN_POINT('Ctrl Pts',(-20.5538524598522,18.1254642945199,
-11.619112129004));
#105991=CARTESIAN_POINT('Ctrl Pts',(-20.4258214013433,17.9306935849389,
-11.6062233157348));
#105992=CARTESIAN_POINT('Ctrl Pts',(-20.3371158370147,17.8212296950832,
-11.5987519188402));
#105993=CARTESIAN_POINT('Ctrl Pts',(-20.2010309774874,17.6838122192984,
-11.5880489838806));
#105994=CARTESIAN_POINT('Ctrl Pts',(-20.162450153694,17.6476664452851,-11.5850813872512));
#105995=CARTESIAN_POINT('Ctrl Pts',(-20.108701657067,17.6009622883346,-11.5809700625467));
#105996=CARTESIAN_POINT('Ctrl Pts',(-20.0946874260822,17.5891011865518,
-11.5799000500308));
#105997=CARTESIAN_POINT('Ctrl Pts',(-20.0737585435042,17.5718499606658,
-11.5783019343463));
#105998=CARTESIAN_POINT('Ctrl Pts',(-20.0669614688815,17.5663178048296,
-11.5777828900162));
#105999=CARTESIAN_POINT('Ctrl Pts',(-20.0546537165162,17.5564269053892,
-11.5768425879283));
#106000=CARTESIAN_POINT('Ctrl Pts',(-20.049155276356,17.5520530568212,-11.5764223531706));
#106001=CARTESIAN_POINT('Ctrl Pts',(-20.0404396658009,17.5451906044537,
-11.5757558051433));
#106002=CARTESIAN_POINT('Ctrl Pts',(-20.0372368644139,17.5426837178577,
-11.5755107717217));
#106003=CARTESIAN_POINT('Ctrl Pts',(-20.034017555783,17.5401788381769,-11.5752643616912));
#106004=CARTESIAN_POINT('Ctrl Pts',(-20.0340082213093,17.5401715753351,
-11.5752636472176));
#106005=CARTESIAN_POINT('Ctrl Pts',(-20.0339895166574,17.5401570221227,
-11.5752622155356));
#106006=CARTESIAN_POINT('Ctrl Pts',(-20.0339801462261,17.5401497315562,
-11.5752614983078));
#106007=CARTESIAN_POINT('Ctrl Pts',(-20.0339613686576,17.5401351221179,
-11.5752600610408));
#106008=CARTESIAN_POINT('Ctrl Pts',(-20.0339519622102,17.5401278037839,
-11.5752593410543));
#106009=CARTESIAN_POINT('Ctrl Pts',(-20.0339331125487,17.5401131387666,
-11.5752578982653));
#106010=CARTESIAN_POINT('Ctrl Pts',(-20.0339236691864,17.5401057919688,
-11.5752571754514));
#106011=CARTESIAN_POINT('Ctrl Pts',(-20.0339040666131,17.5400905417203,
-11.575255675029));
#106012=CARTESIAN_POINT('Ctrl Pts',(-20.0338939075657,17.540082638417,-11.5752548974329));
#106013=CARTESIAN_POINT('Ctrl Pts',(-20.0338734124997,17.5400666944345,
-11.5752533286926));
#106014=CARTESIAN_POINT('Ctrl Pts',(-20.0338630762897,17.5400586536116,
-11.5752525375338));
#106015=CARTESIAN_POINT('Ctrl Pts',(-20.0338422231017,17.540042431652,-11.5752509413773));
#106016=CARTESIAN_POINT('Ctrl Pts',(-20.0338317061711,17.5400342505576,
-11.5752501363832));
#106017=CARTESIAN_POINT('Ctrl Pts',(-20.0338104872993,17.5400177447709,
-11.5752485122314));
#106018=CARTESIAN_POINT('Ctrl Pts',(-20.0337997858628,17.5400094204769,
-11.5752476931123));
#106019=CARTESIAN_POINT('Ctrl Pts',(-20.0337781941368,17.5399926253195,
-11.5752460404161));
#106020=CARTESIAN_POINT('Ctrl Pts',(-20.0337673039442,17.5399841545371,
-11.5752452068464));
#106021=CARTESIAN_POINT('Ctrl Pts',(-20.03374533129,17.5399670637635,-11.5752435249875));
#106022=CARTESIAN_POINT('Ctrl Pts',(-20.0337342481511,17.5399584432516,
-11.5752426766464));
#106023=CARTESIAN_POINT('Ctrl Pts',(-20.0337118851474,17.5399410495704,
-11.5752409649035));
#106024=CARTESIAN_POINT('Ctrl Pts',(-20.0337006054112,17.5399322765076,
-11.5752401015114));
#106025=CARTESIAN_POINT('Ctrl Pts',(-20.0336778445948,17.5399145741522,
-11.5752383593127));
#106026=CARTESIAN_POINT('Ctrl Pts',(-20.0336663637293,17.5399056450331,
-11.5752374805226));
#106027=CARTESIAN_POINT('Ctrl Pts',(-20.0336431964986,17.5398876273529,
-11.5752357072096));
#106028=CARTESIAN_POINT('Ctrl Pts',(-20.0336315099244,17.5398785386362,
-11.5752348126707));
#106029=CARTESIAN_POINT('Ctrl Pts',(-20.0336079267838,17.5398601982874,
-11.5752330075162));
#106030=CARTESIAN_POINT('Ctrl Pts',(-20.0335960301635,17.5398509466207,
-11.5752320968964));
#106031=CARTESIAN_POINT('Ctrl Pts',(-20.0335720219904,17.5398322765518,
-11.5752302592018));
#106032=CARTESIAN_POINT('Ctrl Pts',(-20.0335599107319,17.5398228583858,
-11.5752293321494));
#106033=CARTESIAN_POINT('Ctrl Pts',(-20.0335354687951,17.5398038518512,
-11.575227461246));
#106034=CARTESIAN_POINT('Ctrl Pts',(-20.0335231377892,17.5397942632356,
-11.5752265173698));
#106035=CARTESIAN_POINT('Ctrl Pts',(-20.0334982514618,17.5397749120179,
-11.5752246124438));
#106036=CARTESIAN_POINT('Ctrl Pts',(-20.0334856960872,17.5397651493828,
-11.5752236513898));
#106037=CARTESIAN_POINT('Ctrl Pts',(-20.0334603558312,17.5397454461138,
-11.5752217117107));
#106038=CARTESIAN_POINT('Ctrl Pts',(-20.0334475709584,17.5397355054951,
-11.5752207330862));
#106039=CARTESIAN_POINT('Ctrl Pts',(-20.0307420610612,17.5376319409334,
-11.5750136380816));
#106040=CARTESIAN_POINT('Ctrl Pts',(-20.0280443381108,17.5355448724492,
-11.5748070551759));
#106041=CARTESIAN_POINT('Ctrl Pts',(-20.0217183146218,17.5306751951837,
-11.5743224423692));
#106042=CARTESIAN_POINT('Ctrl Pts',(-20.0180860470383,17.5278978253271,
-11.5740440482796));
#106043=CARTESIAN_POINT('Ctrl Pts',(-20.0069159694157,17.5194139637821,
-11.5731875677778));
#106044=CARTESIAN_POINT('Ctrl Pts',(-19.9993490269805,17.5137462725279,
-11.5726068716553));
#106045=CARTESIAN_POINT('Ctrl Pts',(-19.8929714721592,17.4351755328555,
-11.5644394761263));
#106046=CARTESIAN_POINT('Ctrl Pts',(-19.7880493079973,17.3709618075451,
-11.5563504883798));
#106047=CARTESIAN_POINT('Ctrl Pts',(-19.5840730471582,17.2693209845488,
-11.5412923247994));
#106048=CARTESIAN_POINT('Ctrl Pts',(-19.4866077199321,17.2295040114444,
-11.5343486951377));
#106049=CARTESIAN_POINT('Ctrl Pts',(-19.3341667211761,17.1801074084072,
-11.5240486173121));
#106050=CARTESIAN_POINT('Ctrl Pts',(-19.2811053798119,17.1651746564991,
-11.5205596053547));
#106051=CARTESIAN_POINT('Ctrl Pts',(-19.1941608463262,17.1443317532563,
-11.5150022114063));
#106052=CARTESIAN_POINT('Ctrl Pts',(-19.1606128272286,17.1371467364979,
-11.5128953937016));
#106053=CARTESIAN_POINT('Ctrl Pts',(-19.1162828425483,17.1287738719271,
-11.5101589172838));
#106054=CARTESIAN_POINT('Ctrl Pts',(-19.1056469286479,17.1268492407342,
-11.5095059183646));
#106055=CARTESIAN_POINT('Ctrl Pts',(-19.0881996248776,17.1238298564816,
-11.5084404254008));
#106056=CARTESIAN_POINT('Ctrl Pts',(-19.0813968951305,17.1226868095844,
-11.5080264019505));
#106057=CARTESIAN_POINT('Ctrl Pts',(-19.0682159988403,17.1205382434269,
-11.5072268874871));
#106058=CARTESIAN_POINT('Ctrl Pts',(-19.0618385882497,17.1195286157694,
-11.5068412701392));
#106059=CARTESIAN_POINT('Ctrl Pts',(-19.047099958625,17.1172643677929,-11.5059528464782));
#106060=CARTESIAN_POINT('Ctrl Pts',(-19.0387356075384,17.116030622103,-11.505450706246));
#106061=CARTESIAN_POINT('Ctrl Pts',(-19.0162147777684,17.1128465209799,
-11.5041040841106));
#106062=CARTESIAN_POINT('Ctrl Pts',(-19.0020454172619,17.1109893163341,
-11.5032625436985));
#106063=CARTESIAN_POINT('Ctrl Pts',(-18.8718534913555,17.09526400384,-11.4955800345721));
#106064=CARTESIAN_POINT('Ctrl Pts',(-18.7548809745676,17.0908793336759,
-11.4890558161052));
#106065=CARTESIAN_POINT('Ctrl Pts',(-18.4754784123043,17.1035452086983,
-11.4737444116413));
#106066=CARTESIAN_POINT('Ctrl Pts',(-18.3142400771303,17.1296569650721,
-11.4651405278943));
#106067=CARTESIAN_POINT('Ctrl Pts',(-18.1264120002332,17.1828045289622,
-11.4539312087114));
#106068=CARTESIAN_POINT('Ctrl Pts',(-18.0954257233085,17.1923463199269,
-11.4520402013928));
#106069=CARTESIAN_POINT('Ctrl Pts',(-18.0578102079587,17.2048821845487,
-11.4496794072417));
#106070=CARTESIAN_POINT('Ctrl Pts',(-18.0509595891235,17.2072043222906,
-11.449246778347));
#106071=CARTESIAN_POINT('Ctrl Pts',(-18.0402370168989,17.2109003019963,
-11.4485652284902));
#106072=CARTESIAN_POINT('Ctrl Pts',(-18.0363568587799,17.2122504094998,
-11.4483176903531));
#106073=CARTESIAN_POINT('Ctrl Pts',(-18.0291103843932,17.21479550397,-11.4478536548803));
#106074=CARTESIAN_POINT('Ctrl Pts',(-18.0257431542934,17.2159877193328,
-11.4476373224178));
#106075=CARTESIAN_POINT('Ctrl Pts',(-18.0180621558906,17.2187291820401,
-11.4471422359591));
#106076=CARTESIAN_POINT('Ctrl Pts',(-18.0137504064273,17.2202839150778,
-11.4468631593991));
#106077=CARTESIAN_POINT('Ctrl Pts',(-18.0005076293773,17.2251076584017,
-11.446002534179));
#106078=CARTESIAN_POINT('Ctrl Pts',(-17.9915936980599,17.228422807237,-11.445418339707));
#106079=CARTESIAN_POINT('Ctrl Pts',(-17.9106479665844,17.2591494902491,
-11.4400706938159));
#106080=CARTESIAN_POINT('Ctrl Pts',(-17.8401483310086,17.2904127108057,
-11.4351061750814));
#106081=CARTESIAN_POINT('Ctrl Pts',(-17.6517735869652,17.3865686132769,
-11.4212671672486));
#106082=CARTESIAN_POINT('Ctrl Pts',(-17.5381140560914,17.4589656360344,
-11.4122838432954));
#106083=CARTESIAN_POINT('Ctrl Pts',(-17.3615866073959,17.5966380928363,
-11.3977800034907));
#106084=CARTESIAN_POINT('Ctrl Pts',(-17.2946313903948,17.6560387676602,
-11.3921155164201));
#106085=CARTESIAN_POINT('Ctrl Pts',(-17.2170661150255,17.7341697178937,
-11.3853579009784));
#106086=CARTESIAN_POINT('Ctrl Pts',(-17.2027212171555,17.7490487592684,
-11.3840988333214));
#106087=CARTESIAN_POINT('Ctrl Pts',(-17.1825230597481,17.770622527984,-11.3823119452264));
#106088=CARTESIAN_POINT('Ctrl Pts',(-17.1764908649224,17.7771474078774,
-11.3817764395737));
#106089=CARTESIAN_POINT('Ctrl Pts',(-17.1661147309155,17.7885137656125,
-11.3808520030361));
#106090=CARTESIAN_POINT('Ctrl Pts',(-17.1617517269921,17.7933376024162,
-11.3804622639691));
#106091=CARTESIAN_POINT('Ctrl Pts',(-17.1534123993448,17.8026436049007,
-11.3797153062182));
#106092=CARTESIAN_POINT('Ctrl Pts',(-17.1494327430641,17.8071226875738,
-11.3793579491379));
#106093=CARTESIAN_POINT('Ctrl Pts',(-17.1390723605854,17.8188834247486,
-11.3784252275528));
#106094=CARTESIAN_POINT('Ctrl Pts',(-17.1327224291063,17.8261921145004,
-11.3778511501465));
#106095=CARTESIAN_POINT('Ctrl Pts',(-17.1109326916153,17.8516221034012,
-11.3758725496567));
#106096=CARTESIAN_POINT('Ctrl Pts',(-17.0957482120688,17.8699605150712,
-11.3744785031832));
#106097=CARTESIAN_POINT('Ctrl Pts',(-16.9809519754435,18.0134613512361,
-11.3638086918584));
#106098=CARTESIAN_POINT('Ctrl Pts',(-16.8955049454504,18.1492942495825,
-11.355139250804));
#106099=CARTESIAN_POINT('Ctrl Pts',(-16.7687398322938,18.4128784968633,
-11.3392522400741));
#106100=CARTESIAN_POINT('Ctrl Pts',(-16.722658037229,18.5373987086006,-11.3320561440501));
#106101=CARTESIAN_POINT('Ctrl Pts',(-16.6854511075074,18.6768856932822,
-11.3235369086322));
#106102=CARTESIAN_POINT('Ctrl Pts',(-16.6824807208633,18.688410973857,-11.3228296072729));
#106103=CARTESIAN_POINT('Ctrl Pts',(-16.6783955606457,18.7048334219099,
-11.3218161639325));
#106104=CARTESIAN_POINT('Ctrl Pts',(-16.6772007270811,18.7097106966971,
-11.3215144828439));
#106105=CARTESIAN_POINT('Ctrl Pts',(-16.6751713061913,18.7181241428242,
-11.3209927954166));
#106106=CARTESIAN_POINT('Ctrl Pts',(-16.6743284401425,18.7216583336757,
-11.3207732643332));
#106107=CARTESIAN_POINT('Ctrl Pts',(-16.6727116556253,18.7285157988948,
-11.3203465234846));
#106108=CARTESIAN_POINT('Ctrl Pts',(-16.6719366718143,18.7318387816814,
-11.3201393821978));
#106109=CARTESIAN_POINT('Ctrl Pts',(-16.6698670219458,18.7408110594636,
-11.3195791655846));
#106110=CARTESIAN_POINT('Ctrl Pts',(-16.6685875272649,18.7464637726204,
-11.3192252337057));
#106111=CARTESIAN_POINT('Ctrl Pts',(-16.6639224608173,18.7674740157194,
-11.3179062564002));
#106112=CARTESIAN_POINT('Ctrl Pts',(-16.6606849336319,18.782863434113,-11.3169332733319));
#106113=CARTESIAN_POINT('Ctrl Pts',(-16.6315545776624,18.9294197676727,
-11.3076114803182));
#106114=CARTESIAN_POINT('Ctrl Pts',(-16.6179731617444,19.0627150742554,
-11.2987286172781));
#106115=CARTESIAN_POINT('Ctrl Pts',(-16.6159381294442,19.3575225289747,
-11.279257179858));
#106116=CARTESIAN_POINT('Ctrl Pts',(-16.6332267342542,19.5182877290594,
-11.2687827793791));
#106117=CARTESIAN_POINT('Ctrl Pts',(-16.6726949506265,19.6937614786819,
-11.2577663860324));
#106118=CARTESIAN_POINT('Ctrl Pts',(-16.6770300595005,19.7119110207862,
-11.2566312272291));
#106119=CARTESIAN_POINT('Ctrl Pts',(-16.6836951122388,19.738268029812,-11.2549885646297));
#106120=CARTESIAN_POINT('Ctrl Pts',(-16.6858355071368,19.7465221018191,
-11.2544749779631));
#106121=CARTESIAN_POINT('Ctrl Pts',(-16.6896811727935,19.7609918824613,
-11.2535760407691));
#106122=CARTESIAN_POINT('Ctrl Pts',(-16.6913650566072,19.7672131133834,
-11.253190003525));
#106123=CARTESIAN_POINT('Ctrl Pts',(-16.694694150111,19.7792936626221,-11.25244124102));
#106124=CARTESIAN_POINT('Ctrl Pts',(-16.6963362652449,19.7851537613059,
-11.2520784196587));
#106125=CARTESIAN_POINT('Ctrl Pts',(-16.7003292378898,19.7991702841125,
-11.2512115022822));
#106126=CARTESIAN_POINT('Ctrl Pts',(-16.702703938274,19.807319850902,-11.2507081862378));
#106127=CARTESIAN_POINT('Ctrl Pts',(-16.7114937949828,19.836823283509,-11.2488885306869));
#106128=CARTESIAN_POINT('Ctrl Pts',(-16.7181973228101,19.8580902207719,
-11.2475816003458));
#106129=CARTESIAN_POINT('Ctrl Pts',(-16.7832110064602,20.0535224277731,
-11.2356051056296));
#106130=CARTESIAN_POINT('Ctrl Pts',(-16.863615029258,20.2195077983969,-11.2257712892612));
#106131=CARTESIAN_POINT('Ctrl Pts',(-17.0091283207147,20.4410954386816,
-11.2113256851837));
#106132=CARTESIAN_POINT('Ctrl Pts',(-17.0577018893979,20.5065074936038,
-11.2068523316914));
#106133=CARTESIAN_POINT('Ctrl Pts',(-17.1332465148671,20.5968571775584,
-11.200118114807));
#106134=CARTESIAN_POINT('Ctrl Pts',(-17.1572902942947,20.6241517904327,
-11.1980031086553));
#106135=CARTESIAN_POINT('Ctrl Pts',(-17.1871153249824,20.6563002642737,
-11.1953935088133));
#106136=CARTESIAN_POINT('Ctrl Pts',(-17.1922362116198,20.661761685721,-11.1949459226384));
#106137=CARTESIAN_POINT('Ctrl Pts',(-17.2002499741399,20.6702180081735,
-11.1942460064957));
#106138=CARTESIAN_POINT('Ctrl Pts',(-17.2031229576615,20.6732317934441,
-11.193995184822));
#106139=CARTESIAN_POINT('Ctrl Pts',(-17.2084725451051,20.6788105112329,
-11.1935282921086));
#106140=CARTESIAN_POINT('Ctrl Pts',(-17.2109467443891,20.6813776700208,
-11.1933124062761));
#106141=CARTESIAN_POINT('Ctrl Pts',(-17.2165615029321,20.6871740067452,
-11.192822617295));
#106142=CARTESIAN_POINT('Ctrl Pts',(-17.2197058742373,20.6903994019153,
-11.1925484186943));
#106143=CARTESIAN_POINT('Ctrl Pts',(-17.2278442018562,20.6986943071637,
-11.1918390299488));
#106144=CARTESIAN_POINT('Ctrl Pts',(-17.2328534221425,20.7037486688498,
-11.1914026814653));
#106145=CARTESIAN_POINT('Ctrl Pts',(-17.2636240960976,20.7344851254862,
-11.1887245785999));
#106146=CARTESIAN_POINT('Ctrl Pts',(-17.2900168422225,20.7595233291875,
-11.1864373663102));
#106147=CARTESIAN_POINT('Ctrl Pts',(-17.3284016498339,20.7941033287077,
-11.183141132263));
#106148=CARTESIAN_POINT('Ctrl Pts',(-17.3398741119615,20.8042155719893,
-11.1821596154963));
#106149=CARTESIAN_POINT('Ctrl Pts',(-17.3623619963444,20.8236083293833,
-11.1802443075245));
#106150=CARTESIAN_POINT('Ctrl Pts',(-17.3733646504341,20.8329025458702,
-11.1793111067676));
#106151=CARTESIAN_POINT('Ctrl Pts',(-17.5037665382605,20.9407954958032,
-11.1683040397763));
#106152=CARTESIAN_POINT('Ctrl Pts',(-17.6335443859336,21.0261226182628,
-11.15791299429));
#106153=CARTESIAN_POINT('Ctrl Pts',(-17.8260805709793,21.1244078526214,
-11.1439515806298));
#106154=CARTESIAN_POINT('Ctrl Pts',(-17.8818712216058,21.1498978700305,
-11.1400533877699));
#106155=CARTESIAN_POINT('Ctrl Pts',(-17.9730226558238,21.1868478140952,
-11.1339258497592));
#106156=CARTESIAN_POINT('Ctrl Pts',(-18.0077121643375,21.1998608182901,
-11.1316475071957));
#106157=CARTESIAN_POINT('Ctrl Pts',(-18.0532298482721,21.2155858608301,
-11.1287250877809));
#106158=CARTESIAN_POINT('Ctrl Pts',(-18.0637611517557,21.2191315610793,
-11.1280535217017));
#106159=CARTESIAN_POINT('Ctrl Pts',(-18.080938105988,21.2247645521812,-11.1269654885831));
#106160=CARTESIAN_POINT('Ctrl Pts',(-18.0875668985806,21.2269022189148,
-11.1265473654658));
#106161=CARTESIAN_POINT('Ctrl Pts',(-18.1003377952121,21.2309511345486,
-11.1257451589221));
#106162=CARTESIAN_POINT('Ctrl Pts',(-18.1064782878332,21.2328671761296,
-11.12536092163));
#106163=CARTESIAN_POINT('Ctrl Pts',(-18.1205619511819,21.237191415267,-11.124482983632));
#106164=CARTESIAN_POINT('Ctrl Pts',(-18.1285107748232,21.2395809553057,
-11.1239898984634));
#106165=CARTESIAN_POINT('Ctrl Pts',(-18.1496741058157,21.2458075064624,
-11.1226833900505));
#106166=CARTESIAN_POINT('Ctrl Pts',(-18.1629124549513,21.2495625740202,
-11.1218726373307));
#106167=CARTESIAN_POINT('Ctrl Pts',(-18.2646755391493,21.2773586389636,
-11.1156882871355));
#106168=CARTESIAN_POINT('Ctrl Pts',(-18.3546475436367,21.2957537435224,
-11.1105035040751));
#106169=CARTESIAN_POINT('Ctrl Pts',(-18.5850410149184,21.3274426100362,
-11.0976385322787));
#106170=CARTESIAN_POINT('Ctrl Pts',(-18.7261028645048,21.3326629126159,
-11.0901532712794));
#106171=CARTESIAN_POINT('Ctrl Pts',(-18.9197796953218,21.3205047949299,
-11.0794171883434));
#106172=CARTESIAN_POINT('Ctrl Pts',(-18.9727768894575,21.3151647740702,
-11.0764282988209));
#106173=CARTESIAN_POINT('Ctrl Pts',(-19.0530270227582,21.3040079881616,
-11.0717509325949));
#106174=CARTESIAN_POINT('Ctrl Pts',(-19.0804620802739,21.299641792904,-11.0701245936126));
#106175=CARTESIAN_POINT('Ctrl Pts',(-19.1145806000935,21.2935212695761,
-11.068059056357));
#106176=CARTESIAN_POINT('Ctrl Pts',(-19.1213533549372,21.2922721606862,
-11.0676469070562));
#106177=CARTESIAN_POINT('Ctrl Pts',(-19.132081071184,21.2902394561277,-11.0669905363685));
#106178=CARTESIAN_POINT('Ctrl Pts',(-19.1360401643707,21.2894775583973,
-11.0667475336628));
#106179=CARTESIAN_POINT('Ctrl Pts',(-19.1435166158106,21.2880166108967,
-11.0662871495129));
#106180=CARTESIAN_POINT('Ctrl Pts',(-19.1470343830802,21.2873199315696,
-11.0660699038531));
#106181=CARTESIAN_POINT('Ctrl Pts',(-19.1550907644023,21.2857031146373,
-11.0655709405759));
#106182=CARTESIAN_POINT('Ctrl Pts',(-19.1596281368579,21.2847770212648,
-11.0652888863698));
#106183=CARTESIAN_POINT('Ctrl Pts',(-19.1717032312351,21.2822711543069,
-11.0645355729004));
#106184=CARTESIAN_POINT('Ctrl Pts',(-19.1792353518084,21.2806651397423,
-11.0640628742583));
#106185=CARTESIAN_POINT('Ctrl Pts',(-19.2329514076814,21.2689048963913,
-11.0606725719468));
#106186=CARTESIAN_POINT('Ctrl Pts',(-19.2787888660389,21.2572476416358,
-11.057678209601));
#106187=CARTESIAN_POINT('Ctrl Pts',(-19.327919673285,21.2429851071738,-11.0543855819364));
#106188=CARTESIAN_POINT('Ctrl Pts',(-19.3316428036375,21.2418931860235,
-11.0541355428846));
#106189=CARTESIAN_POINT('Ctrl Pts',(-19.3401240257215,21.2393804681468,
-11.0535647930362));
#106190=CARTESIAN_POINT('Ctrl Pts',(-19.34488015232,21.2379531560931,-11.0532438880699));
#106191=CARTESIAN_POINT('Ctrl Pts',(-19.3733564021484,21.2292981137232,
-11.0513176746354));
#106192=CARTESIAN_POINT('Ctrl Pts',(-19.396952521248,21.2216709771324,-11.0497013216415));
#106193=CARTESIAN_POINT('Ctrl Pts',(-19.457529509479,21.2009080112977,-11.0455074332608));
#106194=CARTESIAN_POINT('Ctrl Pts',(-19.4942888383445,21.187155261532,-11.042919375839));
#106195=CARTESIAN_POINT('Ctrl Pts',(-19.6319038481043,21.1312611157895,
-11.0331075129289));
#106196=CARTESIAN_POINT('Ctrl Pts',(-19.7298346063784,21.0823500415907,
-11.0258811690573));
#106197=CARTESIAN_POINT('Ctrl Pts',(-19.8707065449846,20.9977880625475,
-11.0153210767918));
#106198=CARTESIAN_POINT('Ctrl Pts',(-19.9167399310098,20.9676560340767,
-11.0118389064452));
#106199=CARTESIAN_POINT('Ctrl Pts',(-19.989459172803,20.9159001970269,-11.0062911348919));
#106200=CARTESIAN_POINT('Ctrl Pts',(-20.0168825279939,20.8953619121748,
-11.0041872637018));
#106201=CARTESIAN_POINT('Ctrl Pts',(-20.0522837146794,20.8674823423999,
-11.0014539967142));
#106202=CARTESIAN_POINT('Ctrl Pts',(-20.060719583527,20.8607335713784,-11.0008013291272));
#106203=CARTESIAN_POINT('Ctrl Pts',(-20.0744558832739,20.8495708989396,
-10.9997362382166));
#106204=CARTESIAN_POINT('Ctrl Pts',(-20.0797869803167,20.8451952059703,
-10.9993222877143));
#106205=CARTESIAN_POINT('Ctrl Pts',(-20.0900678090611,20.8366724125768,
-10.9985228183528));
#106206=CARTESIAN_POINT('Ctrl Pts',(-20.0950201305242,20.8325285694427,
-10.9981371736606));
#106207=CARTESIAN_POINT('Ctrl Pts',(-20.106414970519,20.8229049847666,-10.9972485500964));
#106208=CARTESIAN_POINT('Ctrl Pts',(-20.1128437930544,20.8174091411412,
-10.9967462382674));
#106209=CARTESIAN_POINT('Ctrl Pts',(-20.1300532723777,20.8025177510998,
-10.9953988519906));
#106210=CARTESIAN_POINT('Ctrl Pts',(-20.1407720696844,20.7930511528646,
-10.9945567243212));
#106211=CARTESIAN_POINT('Ctrl Pts',(-20.2387839193093,20.7047055148721,
-10.986826653984));
#106212=CARTESIAN_POINT('Ctrl Pts',(-20.319460569841,20.618782274522,-10.9802601807293));
#106213=CARTESIAN_POINT('Ctrl Pts',(-20.4942609397657,20.3984081969231,
-10.964865660767));
#106214=CARTESIAN_POINT('Ctrl Pts',(-20.5807193123279,20.2588894181197,
-10.9562205640924));
#106215=CARTESIAN_POINT('Ctrl Pts',(-20.6634192031584,20.0827747350609,
-10.9450300389358));
#106216=CARTESIAN_POINT('Ctrl Pts',(-20.6759748549493,20.0544352876828,
-10.9432201481326));
#106217=CARTESIAN_POINT('Ctrl Pts',(-20.6906487518604,20.0192484431265,
-10.9409496676435));
#106218=CARTESIAN_POINT('Ctrl Pts',(-20.6933610171813,20.0126509745681,
-10.9405229627674));
#106219=CARTESIAN_POINT('Ctrl Pts',(-20.6975744486875,20.0022528560292,
-10.9398486931349));
#106220=CARTESIAN_POINT('Ctrl Pts',(-20.6990980704846,19.998461281868,-10.9396024628172));
#106221=CARTESIAN_POINT('Ctrl Pts',(-20.7019342809556,19.9913438027277,
-10.939139518495));
#106222=CARTESIAN_POINT('Ctrl Pts',(-20.7032494244098,19.988018975572,-10.9389229611091));
#106223=CARTESIAN_POINT('Ctrl Pts',(-20.7062437528034,19.9803925544831,
-10.9384255506059));
#106224=CARTESIAN_POINT('Ctrl Pts',(-20.7079172856637,19.9760887999387,
-10.9381443632281));
#106225=CARTESIAN_POINT('Ctrl Pts',(-20.7130574322784,19.9627409745949,
-10.9372708464959));
#106226=CARTESIAN_POINT('Ctrl Pts',(-20.7164760114298,19.9536787118702,
-10.9366757574526));
#106227=CARTESIAN_POINT('Ctrl Pts',(-20.7565245175941,19.8452677016758,
-10.9295353227033));
#106228=CARTESIAN_POINT('Ctrl Pts',(-20.7857089216245,19.743340227512,-10.9226145524593));
#106229=CARTESIAN_POINT('Ctrl Pts',(-20.8362075146981,19.4991187304815,
-10.9061648543539));
#106230=CARTESIAN_POINT('Ctrl Pts',(-20.8509047690848,19.3559558994674,
-10.8966462544734));
#106231=CARTESIAN_POINT('Ctrl Pts',(-20.8510404641427,19.1504033897853,
-10.8835936337831));
#106232=CARTESIAN_POINT('Ctrl Pts',(-20.8483582574264,19.0884329461174,
-10.8797325916156));
#106233=CARTESIAN_POINT('Ctrl Pts',(-20.8418780039874,19.0142932904846,
-10.8751998038545));
#106234=CARTESIAN_POINT('Ctrl Pts',(-20.8406878629741,19.001931906853,-10.8744468922717));
#106235=CARTESIAN_POINT('Ctrl Pts',(-20.8385539134922,18.9816409475059,
-10.8732155210563));
#106236=CARTESIAN_POINT('Ctrl Pts',(-20.837673901159,18.9737050989499,-10.8727350656425));
#106237=CARTESIAN_POINT('Ctrl Pts',(-20.8360103028502,18.9594401578817,
-10.8718734213025));
#106238=CARTESIAN_POINT('Ctrl Pts',(-20.8352429787225,18.9531092998899,
-10.8714917248528));
#106239=CARTESIAN_POINT('Ctrl Pts',(-20.8335469912293,18.9396267541141,
-10.8706803091881));
#106240=CARTESIAN_POINT('Ctrl Pts',(-20.8326103654351,18.9324761356255,
-10.8702508463239));
#106241=CARTESIAN_POINT('Ctrl Pts',(-20.8299874442421,18.9132163453064,
-10.8690964080671));
#106242=CARTESIAN_POINT('Ctrl Pts',(-20.82823274486,18.9011166489953,-10.8683735993557));
#106243=CARTESIAN_POINT('Ctrl Pts',(-20.8189028582193,18.8404843987702,
-10.8647630646501));
#106244=CARTESIAN_POINT('Ctrl Pts',(-20.8097446634955,18.7922084255718,
-10.8619258576018));
#106245=CARTESIAN_POINT('Ctrl Pts',(-20.7790242557178,18.6562883324648,
-10.8540037395737));
#106246=CARTESIAN_POINT('Ctrl Pts',(-20.75352795488,18.5696444497169,-10.8490364708034));
#106247=CARTESIAN_POINT('Ctrl Pts',(-20.7225806140666,18.4848897181842,
-10.844119113415));
#106248=CARTESIAN_POINT('Origin',(-18.734,19.211,0.));
#106249=CARTESIAN_POINT('',(-20.7225806138021,18.4848897174598,-10.0464612475213));
#106250=CARTESIAN_POINT('',(-20.7219730443074,18.4851210911025,-10.2662522663146));
#106251=CARTESIAN_POINT('',(-20.7225806137986,18.4848897174502,0.));
#106252=CARTESIAN_POINT('',(-20.853822977789,19.2099225630314,-10.3109437209775));
#106253=CARTESIAN_POINT('Ctrl Pts',(-20.7219730443073,18.4851210911022,
-10.2662522663145));
#106254=CARTESIAN_POINT('Ctrl Pts',(-20.7875398406205,18.6593673202803,
-10.2774434393124));
#106255=CARTESIAN_POINT('Ctrl Pts',(-20.8444161789688,18.9018894991261,
-10.2923405908667));
#106256=CARTESIAN_POINT('Ctrl Pts',(-20.8542040821902,19.1485339254976,
-10.307237742421));
#106257=CARTESIAN_POINT('Ctrl Pts',(-20.853822977789,19.2099225630314,-10.3109437209775));
#106258=CARTESIAN_POINT('Ctrl Pts',(-20.8509997772509,19.210028856431,-10.3093226316228));
#106259=CARTESIAN_POINT('Ctrl Pts',(-20.8510795347034,19.3838924485192,
-10.3205062140852));
#106260=CARTESIAN_POINT('Ctrl Pts',(-20.8297420835379,19.5571145591513,
-10.3322367335455));
#106261=CARTESIAN_POINT('Ctrl Pts',(-20.7726128044767,19.7849965017717,
-10.3474068945114));
#106262=CARTESIAN_POINT('Ctrl Pts',(-20.7552168309962,19.8435328169872,
-10.3512871713045));
#106263=CARTESIAN_POINT('Ctrl Pts',(-20.7232747138574,19.9361472779942,
-10.3573899605202));
#106264=CARTESIAN_POINT('Ctrl Pts',(-20.7103236571686,19.9707351732621,
-10.3596609811954));
#106265=CARTESIAN_POINT('Ctrl Pts',(-20.6923110115516,20.015257531746,-10.3625754978198));
#106266=CARTESIAN_POINT('Ctrl Pts',(-20.6880673552092,20.0255139495368,
-10.3632462992183));
#106267=CARTESIAN_POINT('Ctrl Pts',(-20.6810308933608,20.0421487056393,
-10.3643334037274));
#106268=CARTESIAN_POINT('Ctrl Pts',(-20.6782869804511,20.0485473777868,
-10.364751357626));
#106269=CARTESIAN_POINT('Ctrl Pts',(-20.6729469184083,20.0608324746743,
-10.3655534473118));
#106270=CARTESIAN_POINT('Ctrl Pts',(-20.6703554080878,20.0667208203588,
-10.3659377358523));
#106271=CARTESIAN_POINT('Ctrl Pts',(-20.6643565850482,20.080184356458,-10.3668160794057));
#106272=CARTESIAN_POINT('Ctrl Pts',(-20.6609314373623,20.087751521046,-10.3673095169224));
#106273=CARTESIAN_POINT('Ctrl Pts',(-20.6517054951808,20.1078191216519,
-10.3686175786929));
#106274=CARTESIAN_POINT('Ctrl Pts',(-20.6458269701031,20.1202835382805,
-10.3694295221689));
#106275=CARTESIAN_POINT('Ctrl Pts',(-20.5995496897935,20.2159735242317,
-10.3756607081486));
#106276=CARTESIAN_POINT('Ctrl Pts',(-20.5538539910314,20.2965330155285,
-10.38088770432));
#106277=CARTESIAN_POINT('Ctrl Pts',(-20.4258237932771,20.4913033240151,
-10.3937764819646));
#106278=CARTESIAN_POINT('Ctrl Pts',(-20.3371180113939,20.6007678609914,
-10.4012479119931));
#106279=CARTESIAN_POINT('Ctrl Pts',(-20.2010324356082,20.7381864016567,
-10.4119509113538));
#106280=CARTESIAN_POINT('Ctrl Pts',(-20.1624511839615,20.7743326344711,
-10.4149185414929));
#106281=CARTESIAN_POINT('Ctrl Pts',(-20.1087021231141,20.8210373153859,
-10.4190299095633));
#106282=CARTESIAN_POINT('Ctrl Pts',(-20.0946877849398,20.8328985140195,
-10.420099930273));
#106283=CARTESIAN_POINT('Ctrl Pts',(-20.073758755537,20.850149866293,-10.4216980571669));
#106284=CARTESIAN_POINT('Ctrl Pts',(-20.0669616433089,20.8556820540654,
-10.4222171043653));
#106285=CARTESIAN_POINT('Ctrl Pts',(-20.0546538281695,20.8655730056279,
-10.4231574112431));
#106286=CARTESIAN_POINT('Ctrl Pts',(-20.0491553630238,20.8699468746082,
-10.4235776479075));
#106287=CARTESIAN_POINT('Ctrl Pts',(-20.0404397216919,20.8768093517305,
-10.4242441982853));
#106288=CARTESIAN_POINT('Ctrl Pts',(-20.0372369146868,20.8793162428884,
-10.4244892321355));
#106289=CARTESIAN_POINT('Ctrl Pts',(-20.0340175995839,20.8818211277429,
-10.4247356426605));
#106290=CARTESIAN_POINT('Ctrl Pts',(-20.0340082656108,20.8818283901956,
-10.4247363570957));
#106291=CARTESIAN_POINT('Ctrl Pts',(-20.0339895612393,20.8818429431906,
-10.4247377887563));
#106292=CARTESIAN_POINT('Ctrl Pts',(-20.0339801910055,20.8818502336039,
-10.4247385059689));
#106293=CARTESIAN_POINT('Ctrl Pts',(-20.0339614143614,20.8818648423237,
-10.4247399431651));
#106294=CARTESIAN_POINT('Ctrl Pts',(-20.0339520076384,20.8818721608726,
-10.4247406631727));
#106295=CARTESIAN_POINT('Ctrl Pts',(-20.0339331575991,20.8818868261847,
-10.4247421059906));
#106296=CARTESIAN_POINT('Ctrl Pts',(-20.0339237143765,20.8818941728742,
-10.4247428287939));
#106297=CARTESIAN_POINT('Ctrl Pts',(-20.0339041119862,20.8819094229811,
-10.4247443292022));
#106298=CARTESIAN_POINT('Ctrl Pts',(-20.0338939533132,20.8819173259936,
-10.4247451067697));
#106299=CARTESIAN_POINT('Ctrl Pts',(-20.0338734585654,20.8819332697294,
-10.4247466754856));
#106300=CARTESIAN_POINT('Ctrl Pts',(-20.0338631227878,20.8819413102164,
-10.4247474666113));
#106301=CARTESIAN_POINT('Ctrl Pts',(-20.0338422707524,20.8819575312804,
-10.4247490626796));
#106302=CARTESIAN_POINT('Ctrl Pts',(-20.0338317538745,20.8819657123344,
-10.4247498676696));
#106303=CARTESIAN_POINT('Ctrl Pts',(-20.0338105355873,20.8819822176672,
-10.4247514917767));
#106304=CARTESIAN_POINT('Ctrl Pts',(-20.0337998343062,20.8819905418408,
-10.4247523108839));
#106305=CARTESIAN_POINT('Ctrl Pts',(-20.0337782426903,20.8820073369137,
-10.4247539635717));
#106306=CARTESIAN_POINT('Ctrl Pts',(-20.0337673529512,20.8820158073437,
-10.4247547971066));
#106307=CARTESIAN_POINT('Ctrl Pts',(-20.0337453811954,20.8820328974195,
-10.4247564788967));
#106308=CARTESIAN_POINT('Ctrl Pts',(-20.0337342982742,20.8820415177628,
-10.4247573272212));
#106309=CARTESIAN_POINT('Ctrl Pts',(-20.033711935954,20.8820589109134,-10.4247590389118));
#106310=CARTESIAN_POINT('Ctrl Pts',(-20.0337006564343,20.8820676838083,
-10.4247599022873));
#106311=CARTESIAN_POINT('Ctrl Pts',(-20.0336778958689,20.8820853859696,
-10.4247616444667));
#106312=CARTESIAN_POINT('Ctrl Pts',(-20.0336664154454,20.8820943147455,
-10.424762523223));
#106313=CARTESIAN_POINT('Ctrl Pts',(-20.0336432487705,20.8821123319946,
-10.4247642964935));
#106314=CARTESIAN_POINT('Ctrl Pts',(-20.0336315626091,20.8821214203909,
-10.4247651910008));
#106315=CARTESIAN_POINT('Ctrl Pts',(-20.0336079805509,20.8821397598991,
-10.4247669960724));
#106316=CARTESIAN_POINT('Ctrl Pts',(-20.0335960840755,20.8821490114537,
-10.4247679066811));
#106317=CARTESIAN_POINT('Ctrl Pts',(-20.0335720764689,20.8821676810834,
-10.4247697443324));
#106318=CARTESIAN_POINT('Ctrl Pts',(-20.0335599654901,20.8821770990325,
-10.4247706713633));
#106319=CARTESIAN_POINT('Ctrl Pts',(-20.033535524038,20.8821961051915,-10.4247725422296));
#106320=CARTESIAN_POINT('Ctrl Pts',(-20.0335231934309,20.8822056934977,
-10.4247734860753));
#106321=CARTESIAN_POINT('Ctrl Pts',(-20.03349830783,20.8822250441517,-10.4247753909457));
#106322=CARTESIAN_POINT('Ctrl Pts',(-20.0334857528043,20.8822348065163,
-10.424776351973));
#106323=CARTESIAN_POINT('Ctrl Pts',(-20.0334604130318,20.8822545094107,
-10.424778291615));
#106324=CARTESIAN_POINT('Ctrl Pts',(-20.0334476286159,20.8822644496747,
-10.4247792702046));
#106325=CARTESIAN_POINT('Ctrl Pts',(-20.0307421269511,20.8843680079866,
-10.4249863645778));
#106326=CARTESIAN_POINT('Ctrl Pts',(-20.0280444118049,20.886455070613,-10.4251929468845));
#106327=CARTESIAN_POINT('Ctrl Pts',(-20.0217184109835,20.8913247309189,
-10.425677557951));
#106328=CARTESIAN_POINT('Ctrl Pts',(-20.0180861583096,20.8941020897305,
-10.4259559508954));
#106329=CARTESIAN_POINT('Ctrl Pts',(-20.0069161709817,20.9025858840143,
-10.4268124244656));
#106330=CARTESIAN_POINT('Ctrl Pts',(-19.9993493046154,20.908253519964,-10.4273931147414));
#106331=CARTESIAN_POINT('Ctrl Pts',(-19.892968007856,20.9868270576636,-10.4355607974486));
#106332=CARTESIAN_POINT('Ctrl Pts',(-19.7880415525439,21.0510429530457,
-10.4436501165375));
#106333=CARTESIAN_POINT('Ctrl Pts',(-19.5840560713799,21.1526867069838,
-10.4587089149894));
#106334=CARTESIAN_POINT('Ctrl Pts',(-19.4865858912594,21.1925045339,-10.4656528495737));
#106335=CARTESIAN_POINT('Ctrl Pts',(-19.3341454061733,21.2418987269036,
-10.4759527980815));
#106336=CARTESIAN_POINT('Ctrl Pts',(-19.2810897401927,21.2568293634489,
-10.4794414138498));
#106337=CARTESIAN_POINT('Ctrl Pts',(-19.1941536233652,21.2776698097161,
-10.4849982506522));
#106338=CARTESIAN_POINT('Ctrl Pts',(-19.160608252104,21.2848541595246,-10.4871048977934));
#106339=CARTESIAN_POINT('Ctrl Pts',(-19.1162812482732,21.2932264191434,
-10.4898411884362));
#106340=CARTESIAN_POINT('Ctrl Pts',(-19.105645641529,21.2951509871593,-10.4904941681811));
#106341=CARTESIAN_POINT('Ctrl Pts',(-19.0881987131235,21.2981702980181,
-10.4915596378732));
#106342=CARTESIAN_POINT('Ctrl Pts',(-19.0813960508335,21.2993133306391,
-10.4919736570974));
#106343=CARTESIAN_POINT('Ctrl Pts',(-19.0682151944386,21.3014618852634,
-10.4927731689362));
#106344=CARTESIAN_POINT('Ctrl Pts',(-19.0618377561312,21.3024715147506,
-10.4931587878568));
#106345=CARTESIAN_POINT('Ctrl Pts',(-19.0470989310319,21.3047357865575,
-10.4940472230526));
#106346=CARTESIAN_POINT('Ctrl Pts',(-19.0387344119298,21.3059695524934,
-10.4945493731913));
#106347=CARTESIAN_POINT('Ctrl Pts',(-19.0162128344487,21.3091537443846,
-10.495896039452));
#106348=CARTESIAN_POINT('Ctrl Pts',(-19.0020428929694,21.3110110098388,
-10.4967376137776));
#106349=CARTESIAN_POINT('Ctrl Pts',(-18.8718062099437,21.3267415330394,
-10.5044227567239));
#106350=CARTESIAN_POINT('Ctrl Pts',(-18.7547888765673,21.3311240240564,
-10.5109493149571));
#106351=CARTESIAN_POINT('Ctrl Pts',(-18.4752044442039,21.3184318620377,
-10.5262705031869));
#106352=CARTESIAN_POINT('Ctrl Pts',(-18.3138324572534,21.2922716019514,
-10.5348814326682));
#106353=CARTESIAN_POINT('Ctrl Pts',(-18.1260421499104,21.2390820367457,
-10.5460913458496));
#106354=CARTESIAN_POINT('Ctrl Pts',(-18.0952131956695,21.2295838249247,
-10.5479730782015));
#106355=CARTESIAN_POINT('Ctrl Pts',(-18.0577634108762,21.2171020008226,
-10.5503235524921));
#106356=CARTESIAN_POINT('Ctrl Pts',(-18.0509234635446,21.2147833226423,
-10.5507555186146));
#106357=CARTESIAN_POINT('Ctrl Pts',(-18.0402138753413,21.2110916658093,
-10.5514362541201));
#106358=CARTESIAN_POINT('Ctrl Pts',(-18.0363360622653,21.2097423264981,
-10.5516836461284));
#106359=CARTESIAN_POINT('Ctrl Pts',(-18.029091600221,21.2071978636018,-10.5521475582669));
#106360=CARTESIAN_POINT('Ctrl Pts',(-18.0257240426883,21.2060054963237,
-10.5523639144416));
#106361=CARTESIAN_POINT('Ctrl Pts',(-18.018039211939,21.2032625813299,-10.5528592541087));
#106362=CARTESIAN_POINT('Ctrl Pts',(-18.0137239648623,21.2017065266633,
-10.5531385614447));
#106363=CARTESIAN_POINT('Ctrl Pts',(-18.0004598318507,21.1968747782628,
-10.5540005907713));
#106364=CARTESIAN_POINT('Ctrl Pts',(-17.9915281239089,21.1935527278337,
-10.5545859708601));
#106365=CARTESIAN_POINT('Ctrl Pts',(-17.9095482572567,21.1624295455935,
-10.5600022070352));
#106366=CARTESIAN_POINT('Ctrl Pts',(-17.8380772855782,21.1306660400094,
-10.5650397657947));
#106367=CARTESIAN_POINT('Ctrl Pts',(-17.7326832185344,21.0766571319327,
-10.5727922014047));
#106368=CARTESIAN_POINT('Ctrl Pts',(-17.6973643998133,21.0572660540737,
-10.5754488612951));
#106369=CARTESIAN_POINT('Ctrl Pts',(-17.5683033805438,20.9815363820442,
-10.5853336319267));
#106370=CARTESIAN_POINT('Ctrl Pts',(-17.4784083661181,20.9189639352676,
-10.5925644778513));
#106371=CARTESIAN_POINT('Ctrl Pts',(-17.3511186208319,20.8148580617091,
-10.6031340236403));
#106372=CARTESIAN_POINT('Ctrl Pts',(-17.3098649644141,20.7783422763041,
-10.606621114317));
#106373=CARTESIAN_POINT('Ctrl Pts',(-17.2453100661104,20.7165454227837,
-10.6121758063741));
#106374=CARTESIAN_POINT('Ctrl Pts',(-17.2211193680305,20.6922350079567,
-10.6142817968916));
#106375=CARTESIAN_POINT('Ctrl Pts',(-17.1900944257434,20.6595031463752,
-10.6170173723597));
#106376=CARTESIAN_POINT('Ctrl Pts',(-17.1827201608207,20.6516028788732,
-10.6176702783));
#106377=CARTESIAN_POINT('Ctrl Pts',(-17.1707387261679,20.6385681305599,
-10.6187356584339));
#106378=CARTESIAN_POINT('Ctrl Pts',(-17.1660956511109,20.6334670583672,
-10.6191496614082));
#106379=CARTESIAN_POINT('Ctrl Pts',(-17.1571546290361,20.6235471204119,
-10.6199491631924));
#106380=CARTESIAN_POINT('Ctrl Pts',(-17.1528536400138,20.6187311110586,
-10.6203347881965));
#106381=CARTESIAN_POINT('Ctrl Pts',(-17.1429714138387,20.6075631147828,
-10.6212232678859));
#106382=CARTESIAN_POINT('Ctrl Pts',(-17.1374060401068,20.6011971895926,
-10.6217254562207));
#106383=CARTESIAN_POINT('Ctrl Pts',(-17.122536281731,20.5839814157623,-10.6230722925617));
#106384=CARTESIAN_POINT('Ctrl Pts',(-17.1133032857624,20.5730702840548,
-10.623913997595));
#106385=CARTESIAN_POINT('Ctrl Pts',(-17.0294702174267,20.4719407523271,
-10.6316094095525));
#106386=CARTESIAN_POINT('Ctrl Pts',(-16.9623585410229,20.375768297469,-10.6381450905014));
#106387=CARTESIAN_POINT('Ctrl Pts',(-16.8213881891425,20.1331408326455,
-10.653505649878));
#106388=CARTESIAN_POINT('Ctrl Pts',(-16.7559079457202,19.9827300584193,
-10.6621451756692));
#106389=CARTESIAN_POINT('Ctrl Pts',(-16.6992067310605,19.7960675561764,
-10.6733578986754));
#106390=CARTESIAN_POINT('Ctrl Pts',(-16.6907003679106,19.7656296645746,
-10.6752023921982));
#106391=CARTESIAN_POINT('Ctrl Pts',(-16.6811025206306,19.7280613539657,
-10.6775114153712));
#106392=CARTESIAN_POINT('Ctrl Pts',(-16.6793614997114,19.7210991416788,
-10.6779406829497));
#106393=CARTESIAN_POINT('Ctrl Pts',(-16.676682518661,19.7101498341389,-10.6786181023438));
#106394=CARTESIAN_POINT('Ctrl Pts',(-16.6757206536851,19.7061685650602,
-10.6788648988796));
#106395=CARTESIAN_POINT('Ctrl Pts',(-16.673941116773,19.6987080799527,-10.6793283120801));
#106396=CARTESIAN_POINT('Ctrl Pts',(-16.6731206996699,19.6952295761467,
-10.6795447685404));
#106397=CARTESIAN_POINT('Ctrl Pts',(-16.6712638688833,19.6872665622819,
-10.680041156689));
#106398=CARTESIAN_POINT('Ctrl Pts',(-16.6702332725829,19.6827807529395,
-10.6803214175055));
#106399=CARTESIAN_POINT('Ctrl Pts',(-16.6670963897893,19.6689200708493,
-10.6811892618614));
#106400=CARTESIAN_POINT('Ctrl Pts',(-16.665039328775,19.6595343444159,-10.681779554686));
#106401=CARTESIAN_POINT('Ctrl Pts',(-16.6454505617271,19.5671540590612,
-10.6876132465499));
#106402=CARTESIAN_POINT('Ctrl Pts',(-16.6328601615305,19.4831994431482,
-10.6930995615428));
#106403=CARTESIAN_POINT('Ctrl Pts',(-16.6128800721526,19.2587712569526,
-10.7078847396533));
#106404=CARTESIAN_POINT('Ctrl Pts',(-16.6143840936352,19.1179080203136,
-10.7172628525592));
#106405=CARTESIAN_POINT('Ctrl Pts',(-16.6383730535925,18.9010557252902,
-10.7313035421089));
#106406=CARTESIAN_POINT('Ctrl Pts',(-16.6511502936989,18.8244030254141,
-10.7361948925371));
#106407=CARTESIAN_POINT('Ctrl Pts',(-16.6722967670111,18.7299222408223,
-10.7421282458664));
#106408=CARTESIAN_POINT('Ctrl Pts',(-16.676734845176,18.7112839287012,-10.7432941974425));
#106409=CARTESIAN_POINT('Ctrl Pts',(-16.6835354278751,18.6843518106475,
-10.7449728587424));
#106410=CARTESIAN_POINT('Ctrl Pts',(-16.6856964500663,18.6760085536682,
-10.7454920330164));
#106411=CARTESIAN_POINT('Ctrl Pts',(-16.6895661344616,18.6614357258711,
-10.7463974226501));
#106412=CARTESIAN_POINT('Ctrl Pts',(-16.6912524588262,18.6552003900487,
-10.7467843554042));
#106413=CARTESIAN_POINT('Ctrl Pts',(-16.6945759071338,18.6431311043774,
-10.7475324564266));
#106414=CARTESIAN_POINT('Ctrl Pts',(-16.6962095898083,18.6372962798761,
-10.7478937320647));
#106415=CARTESIAN_POINT('Ctrl Pts',(-16.7001643481948,18.6234015927053,
-10.748753162296));
#106416=CARTESIAN_POINT('Ctrl Pts',(-16.7025083271118,18.6153483124574,
-10.7492505675291));
#106417=CARTESIAN_POINT('Ctrl Pts',(-16.7110762478855,18.5865501865974,
-10.7510268739553));
#106418=CARTESIAN_POINT('Ctrl Pts',(-16.717570724429,18.5658867509804,-10.7522969489057));
#106419=CARTESIAN_POINT('Ctrl Pts',(-16.7840604168619,18.3651594669723,
-10.7646007442742));
#106420=CARTESIAN_POINT('Ctrl Pts',(-16.8676918564502,18.1938421500789,
-10.774730972425));
#106421=CARTESIAN_POINT('Ctrl Pts',(-17.0160143725509,17.9715616423399,
-10.7893122345329));
#106422=CARTESIAN_POINT('Ctrl Pts',(-17.0624802662086,17.9095769409566,
-10.7935774807497));
#106423=CARTESIAN_POINT('Ctrl Pts',(-17.1349116915486,17.8232497857898,
-10.8000284415128));
#106424=CARTESIAN_POINT('Ctrl Pts',(-17.1582626137448,17.7967915867878,
-10.8020820436337));
#106425=CARTESIAN_POINT('Ctrl Pts',(-17.1873099291548,17.7654918230145,
-10.8046235111111));
#106426=CARTESIAN_POINT('Ctrl Pts',(-17.1923861853274,17.7600792896601,
-10.805067188069));
#106427=CARTESIAN_POINT('Ctrl Pts',(-17.2003450934466,17.7516820617921,
-10.8057623063219));
#106428=CARTESIAN_POINT('Ctrl Pts',(-17.2032082997816,17.7486789042641,
-10.8060122725733));
#106429=CARTESIAN_POINT('Ctrl Pts',(-17.2085492138833,17.7431098057744,
-10.8064784057865));
#106430=CARTESIAN_POINT('Ctrl Pts',(-17.211024584124,17.7405417023292,-10.8066943927894));
#106431=CARTESIAN_POINT('Ctrl Pts',(-17.2166544045894,17.7347304403955,
-10.8071854928628));
#106432=CARTESIAN_POINT('Ctrl Pts',(-17.2198127531469,17.7314911459828,
-10.8074609081608));
#106433=CARTESIAN_POINT('Ctrl Pts',(-17.2280108528771,17.7231366819758,
-10.8081754993753));
#106434=CARTESIAN_POINT('Ctrl Pts',(-17.2330662422571,17.7180370346621,
-10.8086158615613));
#106435=CARTESIAN_POINT('Ctrl Pts',(-17.2646308497667,17.6865184476744,
-10.8113629830092));
#106436=CARTESIAN_POINT('Ctrl Pts',(-17.2918091070731,17.660782358504,-10.8137178686075));
#106437=CARTESIAN_POINT('Ctrl Pts',(-17.3347064814091,17.6222659328121,
-10.8173994796434));
#106438=CARTESIAN_POINT('Ctrl Pts',(-17.34995242055,17.6089667484124,-10.818701426894));
#106439=CARTESIAN_POINT('Ctrl Pts',(-17.4908527415713,17.4895705784112,
-10.8306580504794));
#106440=CARTESIAN_POINT('Ctrl Pts',(-17.6282823331921,17.3982315275648,
-10.8417216792679));
#106441=CARTESIAN_POINT('Ctrl Pts',(-17.8288125085212,17.2963249868643,
-10.8562402978281));
#106442=CARTESIAN_POINT('Ctrl Pts',(-17.883867081296,17.2712526234096,-10.8600828493431));
#106443=CARTESIAN_POINT('Ctrl Pts',(-17.9739239914241,17.2348120659962,
-10.8661334627554));
#106444=CARTESIAN_POINT('Ctrl Pts',(-18.0082775023838,17.2219395660662,
-10.8683890108845));
#106445=CARTESIAN_POINT('Ctrl Pts',(-18.0534161745131,17.2063510872536,
-10.8712868175459));
#106446=CARTESIAN_POINT('Ctrl Pts',(-18.063910773973,17.202818722488,-10.8719559951208));
#106447=CARTESIAN_POINT('Ctrl Pts',(-18.081042755503,17.197201542884,-10.8730411277717));
#106448=CARTESIAN_POINT('Ctrl Pts',(-18.0876634498147,17.1950668526175,
-10.873458722423));
#106449=CARTESIAN_POINT('Ctrl Pts',(-18.1004290327026,17.1910202372432,
-10.8742605655831));
#106450=CARTESIAN_POINT('Ctrl Pts',(-18.1065723439577,17.1891036252087,
-10.8746449644778));
#106451=CARTESIAN_POINT('Ctrl Pts',(-18.1206770056599,17.1847736776067,
-10.8755241764001));
#106452=CARTESIAN_POINT('Ctrl Pts',(-18.1286440655654,17.1823791875746,
-10.8760183677387));
#106453=CARTESIAN_POINT('Ctrl Pts',(-18.1498877211188,17.1761307266099,
-10.8773297547881));
#106454=CARTESIAN_POINT('Ctrl Pts',(-18.1631884413225,17.1723596952557,
-10.8781442477075));
#106455=CARTESIAN_POINT('Ctrl Pts',(-18.267370450886,17.1439214784324,-10.8844747697419));
#106456=CARTESIAN_POINT('Ctrl Pts',(-18.3597747944633,17.1252110771481,
-10.889791163526));
#106457=CARTESIAN_POINT('Ctrl Pts',(-18.5915301539621,17.0941887716848,
-10.9027105473566));
#106458=CARTESIAN_POINT('Ctrl Pts',(-18.7314188597847,17.0894019203521,
-10.91013447599));
#106459=CARTESIAN_POINT('Ctrl Pts',(-18.9229156420533,17.1017982659259,
-10.9207593955267));
#106460=CARTESIAN_POINT('Ctrl Pts',(-18.9749293575128,17.1071051883609,
-10.9236957143393));
#106461=CARTESIAN_POINT('Ctrl Pts',(-19.0538614279364,17.1181239019138,
-10.9282984953181));
#106462=CARTESIAN_POINT('Ctrl Pts',(-19.0809554862358,17.1224446562798,
-10.9299051564242));
#106463=CARTESIAN_POINT('Ctrl Pts',(-19.1147074886045,17.128502016166,-10.9319486657742));
#106464=CARTESIAN_POINT('Ctrl Pts',(-19.1214525000138,17.1297463869473,
-10.9323591511823));
#106465=CARTESIAN_POINT('Ctrl Pts',(-19.132146355281,17.1317730560228,-10.9330134750114));
#106466=CARTESIAN_POINT('Ctrl Pts',(-19.1360992870879,17.1325338907055,
-10.933256107702));
#106467=CARTESIAN_POINT('Ctrl Pts',(-19.1435709721854,17.1339941045857,
-10.933716211663));
#106468=CARTESIAN_POINT('Ctrl Pts',(-19.1470901266373,17.1346911555874,
-10.9339335495849));
#106469=CARTESIAN_POINT('Ctrl Pts',(-19.1551585924222,17.136310628741,-10.9344332767563));
#106470=CARTESIAN_POINT('Ctrl Pts',(-19.1597066499969,17.1372390700979,
-10.9347160062497));
#106471=CARTESIAN_POINT('Ctrl Pts',(-19.1718288435444,17.1397552552654,
-10.9354722935461));
#106472=CARTESIAN_POINT('Ctrl Pts',(-19.1793973068715,17.1413695683372,
-10.9359473083792));
#106473=CARTESIAN_POINT('Ctrl Pts',(-19.2336956577122,17.1532627493143,
-10.9393747037463));
#106474=CARTESIAN_POINT('Ctrl Pts',(-19.2800703965404,17.1650809667022,
-10.9424056394983));
#106475=CARTESIAN_POINT('Ctrl Pts',(-19.3291631537236,17.1793797921044,
-10.9456979453872));
#106476=CARTESIAN_POINT('Ctrl Pts',(-19.3323233142932,17.1803082311534,
-10.9459102512275));
#106477=CARTESIAN_POINT('Ctrl Pts',(-19.3402000557516,17.1826423602956,
-10.9464403451065));
#106478=CARTESIAN_POINT('Ctrl Pts',(-19.3449139104348,17.1840571257254,
-10.9467584040841));
#106479=CARTESIAN_POINT('Ctrl Pts',(-19.3733511147444,17.1927001714496,
-10.9486819706202));
#106480=CARTESIAN_POINT('Ctrl Pts',(-19.3969503378651,17.200328262934,-10.9502985344721));
#106481=CARTESIAN_POINT('Ctrl Pts',(-19.4575300997938,17.2210922093458,
-10.9544926160063));
#106482=CARTESIAN_POINT('Ctrl Pts',(-19.4942891401823,17.2348448606408,
-10.9570806533823));
#106483=CARTESIAN_POINT('Ctrl Pts',(-19.6319038650052,17.2907388922522,
-10.9668924960268));
#106484=CARTESIAN_POINT('Ctrl Pts',(-19.7298346206829,17.3396499661639,
-10.9741188397263));
#106485=CARTESIAN_POINT('Ctrl Pts',(-19.8707065542806,17.4242119434513,
-10.9846789316369));
#106486=CARTESIAN_POINT('Ctrl Pts',(-19.9167399378574,17.4543439706201,
-10.9881611018028));
#106487=CARTESIAN_POINT('Ctrl Pts',(-19.9894591761601,17.5060998054725,
-10.9937088730945));
#106488=CARTESIAN_POINT('Ctrl Pts',(-20.0168825302285,17.5266380895548,
-10.9958127441997));
#106489=CARTESIAN_POINT('Ctrl Pts',(-20.0522837156195,17.5545176583499,
-10.998546011088));
#106490=CARTESIAN_POINT('Ctrl Pts',(-20.0607195842579,17.5612664292112,
-10.999198678659));
#106491=CARTESIAN_POINT('Ctrl Pts',(-20.0744558836948,17.5724291014053,
-11.0002637695457));
#106492=CARTESIAN_POINT('Ctrl Pts',(-20.0797869806361,17.5768047942932,
-11.0006777200402));
#106493=CARTESIAN_POINT('Ctrl Pts',(-20.0900678092054,17.5853275875439,
-11.0014771893881));
#106494=CARTESIAN_POINT('Ctrl Pts',(-20.0950201305943,17.5894714306165,
-11.0018628340745));
#106495=CARTESIAN_POINT('Ctrl Pts',(-20.1064149704466,17.5990950151723,
-11.0027514576276));
#106496=CARTESIAN_POINT('Ctrl Pts',(-20.1128437929147,17.6045908587393,
-11.0032537694513));
#106497=CARTESIAN_POINT('Ctrl Pts',(-20.1300532721182,17.6194822486732,
-11.0046011557186));
#106498=CARTESIAN_POINT('Ctrl Pts',(-20.1407720693722,17.6289488468585,
-11.0054432833836));
#106499=CARTESIAN_POINT('Ctrl Pts',(-20.2387839238738,17.7172944892056,
-11.0131733541038));
#106500=CARTESIAN_POINT('Ctrl Pts',(-20.3194605785722,17.8032177347584,
-11.0197398277044));
#106501=CARTESIAN_POINT('Ctrl Pts',(-20.4942609474718,18.0235918151934,
-11.0351343477121));
#106502=CARTESIAN_POINT('Ctrl Pts',(-20.5807193165826,18.1631105901631,
-11.043779444138));
#106503=CARTESIAN_POINT('Ctrl Pts',(-20.6634192044316,18.3392252677977,
-11.0549699689516));
#106504=CARTESIAN_POINT('Ctrl Pts',(-20.6759748557222,18.3675647141389,
-11.0567798596891));
#106505=CARTESIAN_POINT('Ctrl Pts',(-20.690648752115,18.4027515574913,-11.0590503401007));
#106506=CARTESIAN_POINT('Ctrl Pts',(-20.6933610173737,18.4093490259035,
-11.0594770449673));
#106507=CARTESIAN_POINT('Ctrl Pts',(-20.6975744487915,18.4197471442292,
-11.0601513145861));
#106508=CARTESIAN_POINT('Ctrl Pts',(-20.6990980705593,18.4235387183188,
-11.0603975448992));
#106509=CARTESIAN_POINT('Ctrl Pts',(-20.70193428098,18.4306561973342,-11.0608604892132));
#106510=CARTESIAN_POINT('Ctrl Pts',(-20.703249424413,18.4339810244365,-11.0610770465957));
#106511=CARTESIAN_POINT('Ctrl Pts',(-20.7062437527631,18.4416074454138,
-11.0615744570916));
#106512=CARTESIAN_POINT('Ctrl Pts',(-20.7079172856,18.4459111998975,-11.0618556444654));
#106513=CARTESIAN_POINT('Ctrl Pts',(-20.7130574321558,18.4592590250836,
-11.0627291611873));
#106514=CARTESIAN_POINT('Ctrl Pts',(-20.7164760112716,18.4683212877087,
-11.0633242502241));
#106515=CARTESIAN_POINT('Ctrl Pts',(-20.7207530739769,18.4798992648316,
-11.06408682766));
#106516=CARTESIAN_POINT('Ctrl Pts',(-20.7216692101372,18.4823936783584,
-11.064251255848));
#106517=CARTESIAN_POINT('Ctrl Pts',(-20.7225806135353,18.4848897167291,
-11.0644159212905));
#106518=CARTESIAN_POINT('',(-20.8509993992227,19.2094051048361,-10.0879365117025));
#106519=CARTESIAN_POINT('Ctrl Pts',(-20.7225806140666,18.4848897181842,
-10.844119113415));
#106520=CARTESIAN_POINT('Ctrl Pts',(-20.7216543340203,18.4823529374921,
-10.8439719327555));
#106521=CARTESIAN_POINT('Ctrl Pts',(-20.7207231706843,18.4798178494646,
-10.8438247920179));
#106522=CARTESIAN_POINT('Ctrl Pts',(-20.6623499375528,18.3218318044859,
-10.8346510877151));
#106523=CARTESIAN_POINT('Ctrl Pts',(-20.5868669459257,18.1736858755523,
-10.8258506394662));
#106524=CARTESIAN_POINT('Ctrl Pts',(-20.4871421987,18.0242494119213,-10.8152892621795));
#106525=CARTESIAN_POINT('Ctrl Pts',(-20.4792655419488,18.0126959100725,
-10.8144606017706));
#106526=CARTESIAN_POINT('Ctrl Pts',(-20.4681194501686,17.9966898135209,
-10.813294299669));
#106527=CARTESIAN_POINT('Ctrl Pts',(-20.4649459698207,17.9921704202635,
-10.8129629302029));
#106528=CARTESIAN_POINT('Ctrl Pts',(-20.4598136886024,17.9849219450265,
-10.812428049678));
#106529=CARTESIAN_POINT('Ctrl Pts',(-20.4578659862623,17.9821849831245,
-10.8122252965722));
#106530=CARTESIAN_POINT('Ctrl Pts',(-20.4537748176495,17.9764648362565,
-10.8117998739036));
#106531=CARTESIAN_POINT('Ctrl Pts',(-20.4516300990772,17.9734825916516,
-10.8115771150017));
#106532=CARTESIAN_POINT('Ctrl Pts',(-20.4464076165922,17.9662604270335,
-10.8110353472665));
#106533=CARTESIAN_POINT('Ctrl Pts',(-20.443321864516,17.9620263365432,-10.81071579051));
#106534=CARTESIAN_POINT('Ctrl Pts',(-20.4323912730453,17.9471443900344,
-10.8095858946531));
#106535=CARTESIAN_POINT('Ctrl Pts',(-20.424462587658,17.9365588916631,-10.8087700182273));
#106536=CARTESIAN_POINT('Ctrl Pts',(-20.3764349043982,17.873674424813,-10.8038532717267));
#106537=CARTESIAN_POINT('Ctrl Pts',(-20.3340141805246,17.8232013633744,
-10.799615538571));
#106538=CARTESIAN_POINT('Ctrl Pts',(-20.2240817870232,17.7041520603046,
-10.7890379008404));
#106539=CARTESIAN_POINT('Ctrl Pts',(-20.1541137676121,17.6380374577248,
-10.7826422294064));
#106540=CARTESIAN_POINT('Ctrl Pts',(-19.9712621264858,17.4874345144272,
-10.7670586891983));
#106541=CARTESIAN_POINT('Ctrl Pts',(-19.8539618981669,17.4090027263477,
-10.7580101507407));
#106542=CARTESIAN_POINT('Ctrl Pts',(-19.7171141043647,17.3360653819244,
-10.7485415016082));
#106543=CARTESIAN_POINT('Ctrl Pts',(-19.7044367172556,17.3294724934841,
-10.7476735710945));
#106544=CARTESIAN_POINT('Ctrl Pts',(-19.684153555759,17.3191837574311,-10.7462993207281));
#106545=CARTESIAN_POINT('Ctrl Pts',(-19.6765908816755,17.3154043394778,
-10.7457900731935));
#106546=CARTESIAN_POINT('Ctrl Pts',(-19.663212876976,17.3088185896121,-10.744894710243));
#106547=CARTESIAN_POINT('Ctrl Pts',(-19.6574070057459,17.3059933879549,
-10.7445079387702));
#106548=CARTESIAN_POINT('Ctrl Pts',(-19.6453717557756,17.3002048494976,
-10.7437098670655));
#106549=CARTESIAN_POINT('Ctrl Pts',(-19.6391406295207,17.29724530649,-10.7432987022512));
#106550=CARTESIAN_POINT('Ctrl Pts',(-19.6231088244508,17.289726637406,-10.7422459640215));
#106551=CARTESIAN_POINT('Ctrl Pts',(-19.6132874162419,17.2852119842185,
-10.7416059320709));
#106552=CARTESIAN_POINT('Ctrl Pts',(-19.5721500222677,17.2666824799479,
-10.7389450419825));
#106553=CARTESIAN_POINT('Ctrl Pts',(-19.5405292253946,17.2533542496531,
-10.7369477176546));
#106554=CARTESIAN_POINT('Ctrl Pts',(-19.45730612924,17.2206345451399,-10.7318030204427));
#106555=CARTESIAN_POINT('Ctrl Pts',(-19.4052449918637,17.2024788507419,
-10.7286950489945));
#106556=CARTESIAN_POINT('Ctrl Pts',(-19.2479504540769,17.15442470414,-10.7195499188603));
#106557=CARTESIAN_POINT('Ctrl Pts',(-19.1410480683381,17.1306250891409,
-10.7136614871618));
#106558=CARTESIAN_POINT('Ctrl Pts',(-18.986908990109,17.1086504772908,-10.705184626503));
#106559=CARTESIAN_POINT('Ctrl Pts',(-18.9408309213161,17.103618403317,-10.7026506559916));
#106560=CARTESIAN_POINT('Ctrl Pts',(-18.8732954417683,17.0984793676563,
-10.6988935198717));
#106561=CARTESIAN_POINT('Ctrl Pts',(-18.8519416472176,17.0971796748016,
-10.6976992482264));
#106562=CARTESIAN_POINT('Ctrl Pts',(-18.7787716411238,17.0938383603343,
-10.6935748127765));
#106563=CARTESIAN_POINT('Ctrl Pts',(-18.7269059588419,17.0933771253771,
-10.6905961530558));
#106564=CARTESIAN_POINT('Ctrl Pts',(-18.6664285235738,17.0950609626963,
-10.6870053840491));
#106565=CARTESIAN_POINT('Ctrl Pts',(-18.6577783141055,17.0953549062234,
-10.6864889766077));
#106566=CARTESIAN_POINT('Ctrl Pts',(-18.6446646876146,17.0958810492267,
-10.6857015161395));
#106567=CARTESIAN_POINT('Ctrl Pts',(-18.6401996825508,17.0960743574386,
-10.6854325892211));
#106568=CARTESIAN_POINT('Ctrl Pts',(-18.6321761206969,17.0964471883601,
-10.6849478255204));
#106569=CARTESIAN_POINT('Ctrl Pts',(-18.6286173788257,17.0966215574175,
-10.6847322800897));
#106570=CARTESIAN_POINT('Ctrl Pts',(-18.6208738567738,17.0970205681956,
-10.6842620957299));
#106571=CARTESIAN_POINT('Ctrl Pts',(-18.6166893520786,17.0972486490708,
-10.6840072715993));
#106572=CARTESIAN_POINT('Ctrl Pts',(-18.6049073397474,17.0979259337829,
-10.6832877436521));
#106573=CARTESIAN_POINT('Ctrl Pts',(-18.5973116276153,17.0984036805232,
-10.6828214861814));
#106574=CARTESIAN_POINT('Ctrl Pts',(-18.5512928651302,17.1015473351933,
-10.6799828602673));
#106575=CARTESIAN_POINT('Ctrl Pts',(-18.5129484348214,17.1052202829683,
-10.677559382916));
#106576=CARTESIAN_POINT('Ctrl Pts',(-18.3856334166693,17.1209309761825,
-10.6693644419136));
#106577=CARTESIAN_POINT('Ctrl Pts',(-18.2973333024692,17.1375805989713,
-10.6634418599992));
#106578=CARTESIAN_POINT('Ctrl Pts',(-18.0441499013831,17.202213570861,-10.6461748034108));
#106579=CARTESIAN_POINT('Ctrl Pts',(-17.8836772629773,17.2646985604323,
-10.6349283640233));
#106580=CARTESIAN_POINT('Ctrl Pts',(-17.7119975759407,17.3568853964835,
-10.6229309391828));
#106581=CARTESIAN_POINT('Ctrl Pts',(-17.6916892526373,17.3682253823639,
-10.6215108978118));
#106582=CARTESIAN_POINT('Ctrl Pts',(-17.6632763130112,17.3847109331125,
-10.619522233943));
#106583=CARTESIAN_POINT('Ctrl Pts',(-17.6550140522053,17.3895801420575,
-10.618943709519));
#106584=CARTESIAN_POINT('Ctrl Pts',(-17.6416583794255,17.3975738277824,
-10.6180080744736));
#106585=CARTESIAN_POINT('Ctrl Pts',(-17.6365446752666,17.4006639788495,
-10.6176497197478));
#106586=CARTESIAN_POINT('Ctrl Pts',(-17.6258801221134,17.4071702363243,
-10.6169021096835));
#106587=CARTESIAN_POINT('Ctrl Pts',(-17.6203318218453,17.4105904158996,
-10.616513008755));
#106588=CARTESIAN_POINT('Ctrl Pts',(-17.6071922927949,17.4187740917833,
-10.6155911255955));
#106589=CARTESIAN_POINT('Ctrl Pts',(-17.5996153035212,17.4235603005258,
-10.6150591880569));
#106590=CARTESIAN_POINT('Ctrl Pts',(-17.5742940552263,17.4397810082951,
-10.6132802211099));
#106591=CARTESIAN_POINT('Ctrl Pts',(-17.5566901147835,17.4514329860545,
-10.6120412883748));
#106592=CARTESIAN_POINT('Ctrl Pts',(-17.4624597246945,17.5158511046683,
-10.6053927119669));
#106593=CARTESIAN_POINT('Ctrl Pts',(-17.3891963448101,17.5733643631854,
-10.6001686665427));
#106594=CARTESIAN_POINT('Ctrl Pts',(-17.2047797618198,17.7388848584874,
-10.5865221978904));
#106595=CARTESIAN_POINT('Ctrl Pts',(-17.1013027708117,17.8545594954077,
-10.5783387053207));
#106596=CARTESIAN_POINT('Ctrl Pts',(-16.9801993074224,18.024093718978,-10.5666244076512));
#106597=CARTESIAN_POINT('Ctrl Pts',(-16.950707137834,18.0688840146192,-10.5635486459546));
#106598=CARTESIAN_POINT('Ctrl Pts',(-16.9184237280195,18.1222171132852,
-10.5598491744357));
#106599=CARTESIAN_POINT('Ctrl Pts',(-16.9139446751054,18.1297211358079,
-10.5593278237063));
#106600=CARTESIAN_POINT('Ctrl Pts',(-16.9072363226249,18.1411198183784,
-10.5585342976682));
#106601=CARTESIAN_POINT('Ctrl Pts',(-16.9049726711123,18.144994293949,-10.5582642978902));
#106602=CARTESIAN_POINT('Ctrl Pts',(-16.900933153481,18.1519590942489,-10.5577783953199));
#106603=CARTESIAN_POINT('Ctrl Pts',(-16.8991527593703,18.1550467306166,
-10.5575627899971));
#106604=CARTESIAN_POINT('Ctrl Pts',(-16.8953029020148,18.1617624544132,
-10.5570934057404));
#106605=CARTESIAN_POINT('Ctrl Pts',(-16.8932364031233,18.1653921265951,
-10.5568394466927));
#106606=CARTESIAN_POINT('Ctrl Pts',(-16.8874664541485,18.1755967884846,
-10.5561247499005));
#106607=CARTESIAN_POINT('Ctrl Pts',(-16.8837874425121,18.1821854226602,
-10.5556624910248));
#106608=CARTESIAN_POINT('Ctrl Pts',(-16.8620940873218,18.2215281189502,
-10.5528980123702));
#106609=CARTESIAN_POINT('Ctrl Pts',(-16.8449158083539,18.2547328461959,
-10.5505476722786));
#106610=CARTESIAN_POINT('Ctrl Pts',(-16.7914642396141,18.365118866017,-10.5427202437643));
#106611=CARTESIAN_POINT('Ctrl Pts',(-16.758974926751,18.4440357485269,-10.5371054176708));
#106612=CARTESIAN_POINT('Ctrl Pts',(-16.6736475831275,18.6930227718753,
-10.5197177477906));
#106613=CARTESIAN_POINT('Ctrl Pts',(-16.6374020638314,18.8679926917734,
-10.508024687605));
#106614=CARTESIAN_POINT('Ctrl Pts',(-16.6216995381932,19.0681871115291,
-10.4956668419621));
#106615=CARTESIAN_POINT('Ctrl Pts',(-16.6202840116311,19.0909435700787,
-10.4942752570022));
#106616=CARTESIAN_POINT('Ctrl Pts',(-16.6187991059411,19.1232235659733,
-10.4923192372809));
#106617=CARTESIAN_POINT('Ctrl Pts',(-16.6184259692592,19.1327309149415,
-10.4917453344423));
#106618=CARTESIAN_POINT('Ctrl Pts',(-16.6179233222142,19.1481985026732,
-10.4908151403365));
#106619=CARTESIAN_POINT('Ctrl Pts',(-16.6177548727037,19.1541572637932,
-10.4904576333428));
#106620=CARTESIAN_POINT('Ctrl Pts',(-16.6174546507248,19.1666443936419,
-10.489710180215));
#106621=CARTESIAN_POINT('Ctrl Pts',(-16.6173279087249,19.1731728292861,
-10.4893203955717));
#106622=CARTESIAN_POINT('Ctrl Pts',(-16.6170979078866,19.1887283122697,
-10.4883939629391));
#106623=CARTESIAN_POINT('Ctrl Pts',(-16.6170221806385,19.1977556863427,
-10.4878581823956));
#106624=CARTESIAN_POINT('Ctrl Pts',(-16.6169613826195,19.2282799081068,
-10.4860526310735));
#106625=CARTESIAN_POINT('Ctrl Pts',(-16.6172459888386,19.249776397744,-10.4847912964629));
#106626=CARTESIAN_POINT('Ctrl Pts',(-16.622968798079,19.4507254041479,-10.4730865891205));
#106627=CARTESIAN_POINT('Ctrl Pts',(-16.6508849994117,19.6288036369092,
-10.4634407893317));
#106628=CARTESIAN_POINT('Ctrl Pts',(-16.7345162291315,19.9168694929822,
-10.4471157906244));
#106629=CARTESIAN_POINT('Ctrl Pts',(-16.7778863883128,20.0294119810515,
-10.440509532291));
#106630=CARTESIAN_POINT('Ctrl Pts',(-16.8347330806377,20.1461814779287,
-10.4328125536686));
#106631=CARTESIAN_POINT('Ctrl Pts',(-16.8389481968708,20.1546937445466,
-10.4322463615213));
#106632=CARTESIAN_POINT('Ctrl Pts',(-16.8452808961623,20.1672688609738,
-10.4314019266966));
#106633=CARTESIAN_POINT('Ctrl Pts',(-16.8473546806142,20.1713538023063,
-10.4311263575692));
#106634=CARTESIAN_POINT('Ctrl Pts',(-16.8510689186138,20.1786116479274,
-10.4306344418552));
#106635=CARTESIAN_POINT('Ctrl Pts',(-16.8527041589658,20.1817871634565,
-10.4304184243771));
#106636=CARTESIAN_POINT('Ctrl Pts',(-16.8562382689555,20.18860767827,-10.429952734729));
#106637=CARTESIAN_POINT('Ctrl Pts',(-16.8581396908201,20.192251237435,-10.4297029070488));
#106638=CARTESIAN_POINT('Ctrl Pts',(-16.8634201712418,20.2022984055287,
-10.4290111384764));
#106639=CARTESIAN_POINT('Ctrl Pts',(-16.8668214536686,20.2086901809639,
-10.4285678265664));
#106640=CARTESIAN_POINT('Ctrl Pts',(-16.8856796893083,20.2436948471861,
-10.4261227917617));
#106641=CARTESIAN_POINT('Ctrl Pts',(-16.9017607057491,20.2719644283098,
-10.4240847631223));
#106642=CARTESIAN_POINT('Ctrl Pts',(-17.0021764420717,20.439394421619,-10.4116790900861));
#106643=CARTESIAN_POINT('Ctrl Pts',(-17.1016737565232,20.5688205528447,
-10.4007212871873));
#106644=CARTESIAN_POINT('Ctrl Pts',(-17.2963388132869,20.7693490770264,
-10.3824661528239));
#106645=CARTESIAN_POINT('Ctrl Pts',(-17.3844667800199,20.8462643261838,
-10.3750285790364));
#106646=CARTESIAN_POINT('Ctrl Pts',(-17.4911520102363,20.9248449959051,
-10.3669377150156));
#106647=CARTESIAN_POINT('Ctrl Pts',(-17.503904462694,20.9340208314554,-10.365983920476));
#106648=CARTESIAN_POINT('Ctrl Pts',(-17.5233533538149,20.947688998477,-10.3645490071438));
#106649=CARTESIAN_POINT('Ctrl Pts',(-17.5299750473181,20.9522862761405,
-10.3640638718326));
#106650=CARTESIAN_POINT('Ctrl Pts',(-17.5418881103604,20.9604567742544,
-10.3631970851697));
#106651=CARTESIAN_POINT('Ctrl Pts',(-17.5471696634533,20.9640440713344,
-10.3628149011501));
#106652=CARTESIAN_POINT('Ctrl Pts',(-17.5584111989841,20.971605373997,-10.362005840726));
#106653=CARTESIAN_POINT('Ctrl Pts',(-17.5643752968711,20.9755731403905,
-10.3615792031245));
#106654=CARTESIAN_POINT('Ctrl Pts',(-17.5803902667297,20.9861106333292,
-10.3604404477912));
#106655=CARTESIAN_POINT('Ctrl Pts',(-17.5904771796444,20.9926253100861,
-10.3597303948442));
#106656=CARTESIAN_POINT('Ctrl Pts',(-17.6398585863886,21.0239263469489,
-10.3562883066337));
#106657=CARTESIAN_POINT('Ctrl Pts',(-17.6799080450982,21.0475015638419,
-10.3536011745934));
#106658=CARTESIAN_POINT('Ctrl Pts',(-17.869069707589,21.1506234581316,-10.3413281212276));
#106659=CARTESIAN_POINT('Ctrl Pts',(-18.0265804656648,21.2134492192743,
-10.3323387424235));
#106660=CARTESIAN_POINT('Ctrl Pts',(-18.2858254415672,21.2823964472521,
-10.3176550200653));
#106661=CARTESIAN_POINT('Ctrl Pts',(-18.3834250818174,21.301128155566,-10.3121334802109));
#106662=CARTESIAN_POINT('Ctrl Pts',(-18.4915899250137,21.3140977985747,
-10.3056794510721));
#106663=CARTESIAN_POINT('Ctrl Pts',(-18.5012236736348,21.3151858683672,
-10.3051017122815));
#106664=CARTESIAN_POINT('Ctrl Pts',(-18.5154581592575,21.3166946131921,
-10.3042433288564));
#106665=CARTESIAN_POINT('Ctrl Pts',(-18.5200535020191,21.3171664785234,
-10.3039654875614));
#106666=CARTESIAN_POINT('Ctrl Pts',(-18.5282085021999,21.3179768971809,
-10.3034710749827));
#106667=CARTESIAN_POINT('Ctrl Pts',(-18.5317675116668,21.3183214767269,
-10.3032548456809));
#106668=CARTESIAN_POINT('Ctrl Pts',(-18.5393945371849,21.3190404175898,
-10.3027904648566));
#106669=CARTESIAN_POINT('Ctrl Pts',(-18.5434627074604,21.3194120156766,
-10.3025421670823));
#106670=CARTESIAN_POINT('Ctrl Pts',(-18.5546322905618,21.3203996858653,
-10.3018588348985));
#106671=CARTESIAN_POINT('Ctrl Pts',(-18.5617357031844,21.3209916631655,
-10.3014224829616));
#106672=CARTESIAN_POINT('Ctrl Pts',(-18.5996701014527,21.3239601697813,
-10.2990832227456));
#106673=CARTESIAN_POINT('Ctrl Pts',(-18.6305456747066,21.3256967087688,
-10.2971475420398));
#106674=CARTESIAN_POINT('Ctrl Pts',(-18.7241033582773,21.3289049998071,
-10.2912081873798));
#106675=CARTESIAN_POINT('Ctrl Pts',(-18.7868208341602,21.3282690883687,
-10.2871270836676));
#106676=CARTESIAN_POINT('Ctrl Pts',(-18.9713807215036,21.3181924241045,
-10.2749807343996));
#106677=CARTESIAN_POINT('Ctrl Pts',(-19.0925523315125,21.3009887310576,
-10.2668443026107));
#106678=CARTESIAN_POINT('Ctrl Pts',(-19.3061139796514,21.2515374903664,
-10.2526438938305));
#106679=CARTESIAN_POINT('Ctrl Pts',(-19.3990545859024,21.2231666539092,
-10.2465102883386));
#106680=CARTESIAN_POINT('Ctrl Pts',(-19.5027250957551,21.1835476434987,
-10.2397370251966));
#106681=CARTESIAN_POINT('Ctrl Pts',(-19.5156692473789,21.1784541115143,
-10.238892417675));
#106682=CARTESIAN_POINT('Ctrl Pts',(-19.5362964385011,21.1701015915325,
-10.237548035836));
#106683=CARTESIAN_POINT('Ctrl Pts',(-19.5440118748617,21.166924177179,-10.2370455285622));
#106684=CARTESIAN_POINT('Ctrl Pts',(-19.5576477703087,21.1612140427079,
-10.2361579762615));
#106685=CARTESIAN_POINT('Ctrl Pts',(-19.5635758012032,21.1586997852309,
-10.2357723112204));
#106686=CARTESIAN_POINT('Ctrl Pts',(-19.5696170997966,21.1561049023048,
-10.2353794495631));
#106687=CARTESIAN_POINT('Ctrl Pts',(-19.5697418750956,21.1560512940934,
-10.2353713355829));
#106688=CARTESIAN_POINT('Ctrl Pts',(-19.5699732862728,21.1559518446766,
-10.2353562873453));
#106689=CARTESIAN_POINT('Ctrl Pts',(-19.5700799230437,21.1559060069206,
-10.2353493530096));
#106690=CARTESIAN_POINT('Ctrl Pts',(-19.5702777089093,21.155820969505,-10.2353364915663));
#106691=CARTESIAN_POINT('Ctrl Pts',(-19.5703688582651,21.155781772531,-10.2353305644271));
#106692=CARTESIAN_POINT('Ctrl Pts',(-19.5705379316014,21.155709051809,-10.2353195702246));
#106693=CARTESIAN_POINT('Ctrl Pts',(-19.5706158554099,21.1556755301778,
-10.2353145031619));
#106694=CARTESIAN_POINT('Ctrl Pts',(-19.5707604075466,21.155613335762,-10.2353051035888));
#106695=CARTESIAN_POINT('Ctrl Pts',(-19.5708270352755,21.1555846647273,
-10.2353007711095));
#106696=CARTESIAN_POINT('Ctrl Pts',(-19.5709506415334,21.1555314673423,
-10.2352927336312));
#106697=CARTESIAN_POINT('Ctrl Pts',(-19.5710076192507,21.1555069424313,
-10.2352890286793));
#106698=CARTESIAN_POINT('Ctrl Pts',(-19.5711339322195,21.1554525669773,
-10.2352808152665));
#106699=CARTESIAN_POINT('Ctrl Pts',(-19.5712032692351,21.1554227142473,
-10.2352763066982));
#106700=CARTESIAN_POINT('Ctrl Pts',(-19.5713395177064,21.1553640444614,
-10.2352674473265));
#106701=CARTESIAN_POINT('Ctrl Pts',(-19.5714064289843,21.1553352277843,
-10.235263096533));
#106702=CARTESIAN_POINT('Ctrl Pts',(-19.5715379181781,21.1552785912924,
-10.2352545467108));
#106703=CARTESIAN_POINT('Ctrl Pts',(-19.5716024959016,21.1552507718407,
-10.2352503476932));
#106704=CARTESIAN_POINT('Ctrl Pts',(-19.571729405952,21.1551960927359,-10.2352420956988));
#106705=CARTESIAN_POINT('Ctrl Pts',(-19.5717917376581,21.1551692336106,
-10.235238042761));
#106706=CARTESIAN_POINT('Ctrl Pts',(-19.5719142399558,21.1551164396126,
-10.235230077442));
#106707=CARTESIAN_POINT('Ctrl Pts',(-19.5719744099628,21.1550905052337,
-10.2352261650975));
#106708=CARTESIAN_POINT('Ctrl Pts',(-19.5720926696469,21.1550395266262,
-10.2352184757084));
#106709=CARTESIAN_POINT('Ctrl Pts',(-19.5721507587247,21.1550144828807,
-10.2352146987017));
#106710=CARTESIAN_POINT('Ctrl Pts',(-19.572264934109,21.154965252769,-10.2352072749419));
#106711=CARTESIAN_POINT('Ctrl Pts',(-19.5723210198019,21.1549410668763,
-10.2352036282276));
#106712=CARTESIAN_POINT('Ctrl Pts',(-19.5724312628441,21.1548935209943,
-10.23519646021));
#106713=CARTESIAN_POINT('Ctrl Pts',(-19.5724854195906,21.1548701614593,
-10.2351929389449));
#106714=CARTESIAN_POINT('Ctrl Pts',(-19.5725918762277,21.154824238034,-10.2351860171745));
#106715=CARTESIAN_POINT('Ctrl Pts',(-19.5726441754442,21.1548016746152,
-10.2351826167121));
#106716=CARTESIAN_POINT('Ctrl Pts',(-19.5727469857355,21.154757314313,-10.2351759320767));
#106717=CARTESIAN_POINT('Ctrl Pts',(-19.572797495968,21.154735517961,-10.2351726479576));
#106718=CARTESIAN_POINT('Ctrl Pts',(-19.5728967944376,21.1546926637473,
-10.2351661917052));
#106719=CARTESIAN_POINT('Ctrl Pts',(-19.5729455814446,21.1546716065727,
-10.2351630196512));
#106720=CARTESIAN_POINT('Ctrl Pts',(-19.5730414964587,21.1546302039879,
-10.2351567834308));
#106721=CARTESIAN_POINT('Ctrl Pts',(-19.5730886237369,21.1546098590378,
-10.2351537193111));
#106722=CARTESIAN_POINT('Ctrl Pts',(-19.5731812801373,21.154569855067,-10.2351476950012));
#106723=CARTESIAN_POINT('Ctrl Pts',(-19.5732268080293,21.1545501967129,
-10.2351447348902));
#106724=CARTESIAN_POINT('Ctrl Pts',(-19.5733163139483,21.1545115454851,
-10.2351389154559));
#106725=CARTESIAN_POINT('Ctrl Pts',(-19.5733603059771,21.1544925466917,
-10.2351360552213));
#106726=CARTESIAN_POINT('Ctrl Pts',(-19.5734468003774,21.1544551889559,
-10.2351304316238));
#106727=CARTESIAN_POINT('Ctrl Pts',(-19.573489302699,21.1544368301536,-10.2351276682632));
#106728=CARTESIAN_POINT('Ctrl Pts',(-19.5735728760549,21.1544007275378,
-10.2351222346163));
#106729=CARTESIAN_POINT('Ctrl Pts',(-19.5736139471291,21.1543829838166,
-10.2351195643269));
#106730=CARTESIAN_POINT('Ctrl Pts',(-19.573694709497,21.1543480894354,-10.2351143134719));
#106731=CARTESIAN_POINT('Ctrl Pts',(-19.5737344009397,21.1543309388131,
-10.2351117328961));
#106732=CARTESIAN_POINT('Ctrl Pts',(-19.5738124537,21.1542972094759,-10.2351066582384));
#106733=CARTESIAN_POINT('Ctrl Pts',(-19.5738508149958,21.1542806308656,
-10.2351041641574));
#106734=CARTESIAN_POINT('Ctrl Pts',(-19.5806180562704,21.1513557927854,
-10.2346641894215));
#106735=CARTESIAN_POINT('Ctrl Pts',(-19.5873318495993,21.1484125766935,
-10.2342279027148));
#106736=CARTESIAN_POINT('Ctrl Pts',(-19.6058483423217,21.1401803287857,
-10.2330251381579));
#106737=CARTESIAN_POINT('Ctrl Pts',(-19.6176181930145,21.1348178638103,
-10.2322611822493));
#106738=CARTESIAN_POINT('Ctrl Pts',(-19.6437523370135,21.1226204396081,
-10.2305657146303));
#106739=CARTESIAN_POINT('Ctrl Pts',(-19.6580903071511,21.1157307274413,
-10.2296361073986));
#106740=CARTESIAN_POINT('Ctrl Pts',(-19.702145179987,21.0939468272331,-10.2267802678017));
#106741=CARTESIAN_POINT('Ctrl Pts',(-19.7315907130382,21.0785135283598,
-10.2248722292976));
#106742=CARTESIAN_POINT('Ctrl Pts',(-19.8455660918575,21.0153102069606,
-10.2174706515384));
#106743=CARTESIAN_POINT('Ctrl Pts',(-19.9271357089285,20.962440507687,-10.212144414821));
#106744=CARTESIAN_POINT('Ctrl Pts',(-20.1322479364308,20.8084942117171,
-10.198190740769));
#106745=CARTESIAN_POINT('Ctrl Pts',(-20.2484750443433,20.6987617478178,
-10.1896972785582));
#106746=CARTESIAN_POINT('Ctrl Pts',(-20.3605847917494,20.5660346882025,
-10.1794909032523));
#106747=CARTESIAN_POINT('Ctrl Pts',(-20.3697800014617,20.5549199575445,
-10.1786364442597));
#106748=CARTESIAN_POINT('Ctrl Pts',(-20.3823824722885,20.5393657337455,
-10.1774396334951));
#106749=CARTESIAN_POINT('Ctrl Pts',(-20.3858870313162,20.5350051101431,
-10.1771039938543));
#106750=CARTESIAN_POINT('Ctrl Pts',(-20.3914768025684,20.5279931762741,
-10.1765640059058));
#106751=CARTESIAN_POINT('Ctrl Pts',(-20.3935730619795,20.5253506491755,
-10.1763604430214));
#106752=CARTESIAN_POINT('Ctrl Pts',(-20.3979316711108,20.5198291716477,
-10.1759349485047));
#106753=CARTESIAN_POINT('Ctrl Pts',(-20.4001928675041,20.5169493612755,
-10.1757129347041));
#106754=CARTESIAN_POINT('Ctrl Pts',(-20.405633105068,20.5099836654563,-10.1751757362406));
#106755=CARTESIAN_POINT('Ctrl Pts',(-20.4088046410741,20.5058919700169,
-10.1748600254042));
#106756=CARTESIAN_POINT('Ctrl Pts',(-20.4197880307085,20.4916141102361,
-10.173757939017));
#106757=CARTESIAN_POINT('Ctrl Pts',(-20.4275220388204,20.4813687926063,
-10.1729663755848));
#106758=CARTESIAN_POINT('Ctrl Pts',(-20.4722134396685,20.4210322383863,
-10.1683034958164));
#106759=CARTESIAN_POINT('Ctrl Pts',(-20.5070370476685,20.369405002454,-10.164309539088));
#106760=CARTESIAN_POINT('Ctrl Pts',(-20.6118061721582,20.1982660253265,
-10.1512361186923));
#106761=CARTESIAN_POINT('Ctrl Pts',(-20.6723278871939,20.0734026319898,
-10.1419706979438));
#106762=CARTESIAN_POINT('Ctrl Pts',(-20.7344247313902,19.9050267018588,
-10.130313183837));
#106763=CARTESIAN_POINT('Ctrl Pts',(-20.7474992329999,19.8661284610667,
-10.1276721286586));
#106764=CARTESIAN_POINT('Ctrl Pts',(-20.7623061626206,19.8174325798067,
-10.1244342720389));
#106765=CARTESIAN_POINT('Ctrl Pts',(-20.7651107253494,19.8079720170767,
-10.1238083728947));
#106766=CARTESIAN_POINT('Ctrl Pts',(-20.783378684374,19.744729851012,-10.119645452622));
#106767=CARTESIAN_POINT('Ctrl Pts',(-20.7967715207409,19.6903695042325,
-10.116169605456));
#106768=CARTESIAN_POINT('Ctrl Pts',(-20.8104072878551,19.6237546954499,
-10.112030509052));
#106769=CARTESIAN_POINT('Ctrl Pts',(-20.8127188525531,19.6119508761455,
-10.1113015747757));
#106770=CARTESIAN_POINT('Ctrl Pts',(-20.8163752070018,19.5923978742264,
-10.110101367228));
#106771=CARTESIAN_POINT('Ctrl Pts',(-20.8177776139856,19.5846598710808,
-10.1096282667333));
#106772=CARTESIAN_POINT('Ctrl Pts',(-20.8202374445089,19.5706426942465,
-10.1087745941513));
#106773=CARTESIAN_POINT('Ctrl Pts',(-20.8213097124377,19.5643662521112,
-10.108393554067));
#106774=CARTESIAN_POINT('Ctrl Pts',(-20.8233364562906,19.5521716664567,
-10.107655532389));
#106775=CARTESIAN_POINT('Ctrl Pts',(-20.8242941435062,19.5462541250107,
-10.1072984522392));
#106776=CARTESIAN_POINT('Ctrl Pts',(-20.8263396723343,19.5332652342932,
-10.106516937583));
#106777=CARTESIAN_POINT('Ctrl Pts',(-20.8274168308279,19.5261922587443,
-10.1060928441082));
#106778=CARTESIAN_POINT('Ctrl Pts',(-20.8299772003143,19.508787698909,-10.1050528142087));
#106779=CARTESIAN_POINT('Ctrl Pts',(-20.8314199105171,19.4984502785485,
-10.104438153699));
#106780=CARTESIAN_POINT('Ctrl Pts',(-20.8449846038358,19.3957107033154,
-10.0983586071851));
#106781=CARTESIAN_POINT('Ctrl Pts',(-20.8510696179301,19.3026105798559,
-10.0930912443828));
#106782=CARTESIAN_POINT('Ctrl Pts',(-20.8509993992227,19.2094051048361,
-10.0879365117025));
#106783=CARTESIAN_POINT('Ctrl Pts',(-20.8509994011045,19.2094076046327,
-10.0879366499539));
#106784=CARTESIAN_POINT('Ctrl Pts',(-20.8508903570022,19.0644396499636,
-10.0799191880673));
#106785=CARTESIAN_POINT('Ctrl Pts',(-20.8358914557206,18.9198677623656,
-10.0722246121862));
#106786=CARTESIAN_POINT('Ctrl Pts',(-20.7926402107778,18.7128956226968,
-10.0604947085716));
#106787=CARTESIAN_POINT('Ctrl Pts',(-20.775987532445,18.6485120637171,-10.056735705653));
#106788=CARTESIAN_POINT('Ctrl Pts',(-20.7524080825635,18.5723339612825,
-10.0520405686672));
#106789=CARTESIAN_POINT('Ctrl Pts',(-20.7483605188363,18.5596804342305,
-10.0512523078793));
#106790=CARTESIAN_POINT('Ctrl Pts',(-20.7425481579392,18.5420823325455,
-10.0501432138957));
#106791=CARTESIAN_POINT('Ctrl Pts',(-20.7408835587576,18.5371046603246,
-10.0498280660244));
#106792=CARTESIAN_POINT('Ctrl Pts',(-20.7380219448138,18.5286521768047,
-10.0492903910603));
#106793=CARTESIAN_POINT('Ctrl Pts',(-20.7368343465263,18.5251741567682,
-10.0490684186571));
#106794=CARTESIAN_POINT('Ctrl Pts',(-20.7345445654253,18.5185249368981,
-10.0486426263969));
#106795=CARTESIAN_POINT('Ctrl Pts',(-20.7334438884132,18.5153532448196,
-10.0484389005606));
#106796=CARTESIAN_POINT('Ctrl Pts',(-20.7305162333362,18.5069813137827,
-10.0478995311231));
#106797=CARTESIAN_POINT('Ctrl Pts',(-20.7286764970099,18.5017856098278,
-10.0475631397474));
#106798=CARTESIAN_POINT('Ctrl Pts',(-20.7254160069984,18.4926905187973,
-10.0469714583051));
#106799=CARTESIAN_POINT('Ctrl Pts',(-20.7240040333705,18.4887880020968,
-10.0467166641269));
#106800=CARTESIAN_POINT('Ctrl Pts',(-20.7225806138021,18.4848897174598,
-10.0464612475213));
#106801=CARTESIAN_POINT('Origin',(-18.734,19.211,0.));
#106802=CARTESIAN_POINT('',(-20.7225807588464,18.4848901146894,-9.24346988827878));
#106803=CARTESIAN_POINT('',(-20.7225806137986,18.4848897174502,-9.46634970542581));
#106804=CARTESIAN_POINT('',(-20.7225806137986,18.4848897174502,0.));
#106805=CARTESIAN_POINT('',(-20.8516085051224,19.2128934567755,-9.51094371951089));
#106806=CARTESIAN_POINT('Ctrl Pts',(-20.7225806137986,18.4848897174502,
-9.46634970542581));
#106807=CARTESIAN_POINT('Ctrl Pts',(-20.7472616943129,18.5524831938379,
-9.47066129020357));
#106808=CARTESIAN_POINT('Ctrl Pts',(-20.768494307004,18.6213418962955,-9.47497287498133));
#106809=CARTESIAN_POINT('Ctrl Pts',(-20.7861614183071,18.6910745118658,
-9.4792844597591));
#106810=CARTESIAN_POINT('Ctrl Pts',(-20.8038310812988,18.7608171990267,
-9.48359666726579));
#106811=CARTESIAN_POINT('Ctrl Pts',(-20.8179341108459,18.8314335643017,
-9.48790887477247));
#106812=CARTESIAN_POINT('Ctrl Pts',(-20.8284043874146,18.902521050996,-9.49222108227916));
#106813=CARTESIAN_POINT('Ctrl Pts',(-20.8388856923757,18.9736834144808,
-9.49653783185468));
#106814=CARTESIAN_POINT('Ctrl Pts',(-20.8457265542653,19.0453173949163,
-9.50085458143021));
#106815=CARTESIAN_POINT('Ctrl Pts',(-20.8489127423905,19.1170154689625,
-9.50517133100573));
#106816=CARTESIAN_POINT('Ctrl Pts',(-20.8503329346207,19.1489737349782,
-9.50709545286107));
#106817=CARTESIAN_POINT('Ctrl Pts',(-20.8510277144022,19.1809447313957,
-9.5090195747164));
#106818=CARTESIAN_POINT('Ctrl Pts',(-20.8509991540684,19.2128925310398,
-9.51094369657173));
#106819=CARTESIAN_POINT('Ctrl Pts',(-20.8516474640139,19.2128935159625,
-9.51094372097751));
#106820=CARTESIAN_POINT('Ctrl Pts',(-20.8529701716602,19.3558822341492,
-9.51955279572482));
#106821=CARTESIAN_POINT('Ctrl Pts',(-20.77452049264,20.2015184074521,-9.57055380603263));
#106822=CARTESIAN_POINT('Ctrl Pts',(-19.6371491634786,21.5456631571965,
-9.66394675190087));
#106823=CARTESIAN_POINT('Ctrl Pts',(-17.2597752658646,21.2341144066337,
-9.79112255858231));
#106824=CARTESIAN_POINT('Ctrl Pts',(-16.2349110611132,19.0664837566253,
-9.91829836526376));
#106825=CARTESIAN_POINT('Ctrl Pts',(-17.5028058468379,17.031437790224,-10.0454741719452));
#106826=CARTESIAN_POINT('Ctrl Pts',(-19.6892758366696,16.9991228861485,
-10.1614588056287));
#106827=CARTESIAN_POINT('Ctrl Pts',(-20.5391741505579,17.9993261502973,
-10.2350515037519));
#106828=CARTESIAN_POINT('Ctrl Pts',(-20.7219730443073,18.4851210911022,
-10.2662522663145));
#106829=CARTESIAN_POINT('Ctrl Pts',(-20.7225806138021,18.4848897174598,
-10.0464612475213));
#106830=CARTESIAN_POINT('Ctrl Pts',(-20.7192292584429,18.4757114418486,
-10.0458598845578));
#106831=CARTESIAN_POINT('Ctrl Pts',(-20.7158144538027,18.4665566261871,
-10.0452550715018));
#106832=CARTESIAN_POINT('Ctrl Pts',(-20.6531107477152,18.3019423801365,
-10.0342938815402));
#106833=CARTESIAN_POINT('Ctrl Pts',(-20.5757664518257,18.1539936132858,
-10.0231064405996));
#106834=CARTESIAN_POINT('Ctrl Pts',(-20.4366046550753,17.9503358154075,
-10.0069020249956));
#106835=CARTESIAN_POINT('Ctrl Pts',(-20.3875635364868,17.8866637597059,
-10.0016903281187));
#106836=CARTESIAN_POINT('Ctrl Pts',(-20.3092873850567,17.7961835956228,
-9.99410986078368));
#106837=CARTESIAN_POINT('Ctrl Pts',(-20.2827305771936,17.7671614645455,
-9.99164823551441));
#106838=CARTESIAN_POINT('Ctrl Pts',(-20.2369236068718,17.7198212613663,
-9.98758111794582));
#106839=CARTESIAN_POINT('Ctrl Pts',(-20.2181103780658,17.7010960676583,
-9.98595788160913));
#106840=CARTESIAN_POINT('Ctrl Pts',(-20.1918823896307,17.6759547994022,
-9.98375726203708));
#106841=CARTESIAN_POINT('Ctrl Pts',(-20.1847684802612,17.6692297020659,
-9.98316646069937));
#106842=CARTESIAN_POINT('Ctrl Pts',(-20.1732499953931,17.6584910783321,
-9.98221949472933));
#106843=CARTESIAN_POINT('Ctrl Pts',(-20.1688747389153,17.6544464397751,
-9.98186199598629));
#106844=CARTESIAN_POINT('Ctrl Pts',(-20.1597234017734,17.6460580012073,
-9.98111879015933));
#106845=CARTESIAN_POINT('Ctrl Pts',(-20.1549444041178,17.6417174633672,
-9.98073322400363));
#106846=CARTESIAN_POINT('Ctrl Pts',(-20.1438651652245,17.6317468206085,
-9.97984517530119));
#106847=CARTESIAN_POINT('Ctrl Pts',(-20.1375508973816,17.6261324123611,
-9.97934335703039));
#106848=CARTESIAN_POINT('Ctrl Pts',(-20.1204817236984,17.611137165082,-9.97799816822268));
#106849=CARTESIAN_POINT('Ctrl Pts',(-20.1096651777285,17.6018269221928,
-9.97715772927185));
#106850=CARTESIAN_POINT('Ctrl Pts',(-20.0094118528506,17.517284481492,-9.96947482119003));
#106851=CARTESIAN_POINT('Ctrl Pts',(-19.9139779331128,17.4494651585837,
-9.96294926674155));
#106852=CARTESIAN_POINT('Ctrl Pts',(-19.6733869540662,17.3068623850346,
-9.9476384555831));
#106853=CARTESIAN_POINT('Ctrl Pts',(-19.524263822558,17.2402998388123,-9.93903632368726));
#106854=CARTESIAN_POINT('Ctrl Pts',(-19.3380437823101,17.1817455077592,
-9.92782714614726));
#106855=CARTESIAN_POINT('Ctrl Pts',(-19.3068600295617,17.1727228324961,
-9.92593382656331));
#106856=CARTESIAN_POINT('Ctrl Pts',(-19.2684875435943,17.1625702525105,
-9.9235704599097));
#106857=CARTESIAN_POINT('Ctrl Pts',(-19.2614825854748,17.1607552625992,
-9.92313766635831));
#106858=CARTESIAN_POINT('Ctrl Pts',(-19.250485711119,17.1579660514445,-9.92245591419394));
#106859=CARTESIAN_POINT('Ctrl Pts',(-19.2464999533063,17.156967458653,-9.92220833976146));
#106860=CARTESIAN_POINT('Ctrl Pts',(-19.2390438849293,17.1551224662386,
-9.92174427360243));
#106861=CARTESIAN_POINT('Ctrl Pts',(-19.2355743308113,17.1542732438305,
-9.92152794697672));
#106862=CARTESIAN_POINT('Ctrl Pts',(-19.2276487042941,17.1523545820157,
-9.92103292316839));
#106863=CARTESIAN_POINT('Ctrl Pts',(-19.223191313764,17.1512908317278,-9.92075390373884));
#106864=CARTESIAN_POINT('Ctrl Pts',(-19.2094772777523,17.1480650231234,
-9.91989362591211));
#106865=CARTESIAN_POINT('Ctrl Pts',(-19.2002096443159,17.1459508673444,
-9.91930972473851));
#106866=CARTESIAN_POINT('Ctrl Pts',(-19.1166677079326,17.1274840974736,
-9.91402529553097));
#106867=CARTESIAN_POINT('Ctrl Pts',(-19.0415842745261,17.1150843416033,
-9.90912895176016));
#106868=CARTESIAN_POINT('Ctrl Pts',(-18.8155315308582,17.0901606878071,
-9.8942539240383));
#106869=CARTESIAN_POINT('Ctrl Pts',(-18.663693402277,17.0897572228357,-9.88412220250481));
#106870=CARTESIAN_POINT('Ctrl Pts',(-18.4580374486812,17.1113333495289,
-9.87082768138821));
#106871=CARTESIAN_POINT('Ctrl Pts',(-18.4032094151102,17.1192701430802,
-9.867320486863));
#106872=CARTESIAN_POINT('Ctrl Pts',(-18.3148993658855,17.1356135548935,
-9.86173753465641));
#106873=CARTESIAN_POINT('Ctrl Pts',(-18.2812033465313,17.142703684837,-9.85962289906963));
#106874=CARTESIAN_POINT('Ctrl Pts',(-18.2371603710423,17.1530990030193,
-9.85687790975412));
#106875=CARTESIAN_POINT('Ctrl Pts',(-18.2266461872596,17.1556659040956,
-9.85622403382406));
#106876=CARTESIAN_POINT('Ctrl Pts',(-18.2094605105504,17.1600014749622,
-9.85515747661951));
#106877=CARTESIAN_POINT('Ctrl Pts',(-18.2027772598948,17.1617223155832,
-9.85474326003886));
#106878=CARTESIAN_POINT('Ctrl Pts',(-18.1898588556673,17.1651160618714,
-9.85394362566391));
#106879=CARTESIAN_POINT('Ctrl Pts',(-18.1836227126032,17.1667848654824,
-9.85355808020826));
#106880=CARTESIAN_POINT('Ctrl Pts',(-18.1692444773468,17.1707030729017,
-9.85267018338997));
#106881=CARTESIAN_POINT('Ctrl Pts',(-18.1611079849665,17.1729727446965,
-9.85216849557217));
#106882=CARTESIAN_POINT('Ctrl Pts',(-18.1392696098283,17.1792056687413,
-9.85082388737276));
#106883=CARTESIAN_POINT('Ctrl Pts',(-18.1255936861256,17.1832588395962,
-9.84998389456965));
#106884=CARTESIAN_POINT('Ctrl Pts',(-18.0001577331489,17.2218179266526,
-9.84229581169312));
#106885=CARTESIAN_POINT('Ctrl Pts',(-17.8913895626666,17.2653939960854,
-9.83576520565507));
#106886=CARTESIAN_POINT('Ctrl Pts',(-17.6409649188848,17.3906861326746,
-9.82043611232572));
#106887=CARTESIAN_POINT('Ctrl Pts',(-17.5040963052504,17.4802217977321,
-9.81182142397062));
#106888=CARTESIAN_POINT('Ctrl Pts',(-17.3541557404107,17.6051501542586,
-9.80061117768796));
#106889=CARTESIAN_POINT('Ctrl Pts',(-17.3299143814775,17.6263021644634,
-9.79873437698213));
#106890=CARTESIAN_POINT('Ctrl Pts',(-17.3008379550254,17.6528640532562,
-9.79638939059324));
#106891=CARTESIAN_POINT('Ctrl Pts',(-17.2955350581716,17.6577583306483,
-9.79595777837437));
#106892=CARTESIAN_POINT('Ctrl Pts',(-17.2872553878152,17.6654787692485,
-9.79527747772444));
#106893=CARTESIAN_POINT('Ctrl Pts',(-17.2842615769759,17.6682866916569,
-9.79503016376186));
#106894=CARTESIAN_POINT('Ctrl Pts',(-17.2786772207057,17.6735549205963,
-9.79456631734594));
#106895=CARTESIAN_POINT('Ctrl Pts',(-17.2760847308732,17.6760130842573,
-9.79434994835765));
#106896=CARTESIAN_POINT('Ctrl Pts',(-17.2701762540741,17.6816438929165,
-9.79385447278043));
#106897=CARTESIAN_POINT('Ctrl Pts',(-17.2668643645917,17.6848207550195,
-9.7935750416618));
#106898=CARTESIAN_POINT('Ctrl Pts',(-17.2582424576261,17.6931451420628,
-9.79284320079083));
#106899=CARTESIAN_POINT('Ctrl Pts',(-17.2529490907731,17.6983097163529,
-9.79238950999087));
#106900=CARTESIAN_POINT('Ctrl Pts',(-17.2183372667072,17.7324352258961,
-9.78939468194003));
#106901=CARTESIAN_POINT('Ctrl Pts',(-17.1898448105618,17.7622172187049,
-9.78679518565037));
#106902=CARTESIAN_POINT('Ctrl Pts',(-17.147220574699,17.8094569786565,-9.78271912947184));
#106903=CARTESIAN_POINT('Ctrl Pts',(-17.1324652284145,17.826341882549,-9.78127101771809));
#106904=CARTESIAN_POINT('Ctrl Pts',(-17.0165750514617,17.9632887680826,
-9.76961529082282));
#106905=CARTESIAN_POINT('Ctrl Pts',(-16.9288089313468,18.0940295422687,
-9.7590752129637));
#106906=CARTESIAN_POINT('Ctrl Pts',(-16.8280505717015,18.2875352114421,
-9.7449863694245));
#106907=CARTESIAN_POINT('Ctrl Pts',(-16.8021637192357,18.3429907133462,
-9.74109728006499));
#106908=CARTESIAN_POINT('Ctrl Pts',(-16.7645366432666,18.4336514308909,
-9.73498231498705));
#106909=CARTESIAN_POINT('Ctrl Pts',(-16.7512570201627,18.4681761595308,
-9.73270769071316));
#106910=CARTESIAN_POINT('Ctrl Pts',(-16.7351741821253,18.5134989736038,
-9.72978928421131));
#106911=CARTESIAN_POINT('Ctrl Pts',(-16.7315426414751,18.5239942746394,
-9.72911810615832));
#106912=CARTESIAN_POINT('Ctrl Pts',(-16.7257686508755,18.5411161758072,
-9.72803054424939));
#106913=CARTESIAN_POINT('Ctrl Pts',(-16.7235760491618,18.5477255249743,
-9.72761250700058));
#106914=CARTESIAN_POINT('Ctrl Pts',(-16.7194207240301,18.5604612060101,
-9.72681035980897));
#106915=CARTESIAN_POINT('Ctrl Pts',(-16.7174532386901,18.5665858920584,
-9.72642609656468));
#106916=CARTESIAN_POINT('Ctrl Pts',(-16.7130102760682,18.5806362340416,
-9.72554795302985));
#106917=CARTESIAN_POINT('Ctrl Pts',(-16.7105534385819,18.588567708297,-9.72505468926941));
#106918=CARTESIAN_POINT('Ctrl Pts',(-16.7041462558614,18.6096910925134,
-9.72374739360048));
#106919=CARTESIAN_POINT('Ctrl Pts',(-16.7002778116199,18.6229075764203,
-9.72293603741057));
#106920=CARTESIAN_POINT('Ctrl Pts',(-16.6715227363951,18.7248271891946,
-9.71672789116723));
#106921=CARTESIAN_POINT('Ctrl Pts',(-16.6523196348054,18.815037454539,-9.71152165510277));
#106922=CARTESIAN_POINT('Ctrl Pts',(-16.6187969411326,19.0454611850514,
-9.69864331870203));
#106923=CARTESIAN_POINT('Ctrl Pts',(-16.6124727143517,19.1863666960421,
-9.69116392748577));
#106924=CARTESIAN_POINT('Ctrl Pts',(-16.6230746347889,19.3798061231709,
-9.6804441511693));
#106925=CARTESIAN_POINT('Ctrl Pts',(-16.6279653658204,19.4326275173585,
-9.6774669403305));
#106926=CARTESIAN_POINT('Ctrl Pts',(-16.638421692189,19.5126753421487,-9.67280613148938));
#106927=CARTESIAN_POINT('Ctrl Pts',(-16.6425486019467,19.5400704172097,
-9.67118414829697));
#106928=CARTESIAN_POINT('Ctrl Pts',(-16.6483699305577,19.5741577611718,
-9.66912348596524));
#106929=CARTESIAN_POINT('Ctrl Pts',(-16.6495612934932,19.5809346184253,
-9.66871170314222));
#106930=CARTESIAN_POINT('Ctrl Pts',(-16.6515028342518,19.5916715102366,
-9.66805578327073));
#106931=CARTESIAN_POINT('Ctrl Pts',(-16.6522313320841,19.5956354855115,
-9.66781286204611));
#106932=CARTESIAN_POINT('Ctrl Pts',(-16.6536294726477,19.6031228528446,
-9.66735253984719));
#106933=CARTESIAN_POINT('Ctrl Pts',(-16.6542967508952,19.6066466324067,
-9.66713527412185));
#106934=CARTESIAN_POINT('Ctrl Pts',(-16.655846612084,19.6147189173539,-9.66663614374831));
#106935=CARTESIAN_POINT('Ctrl Pts',(-16.6567351748868,19.6192662285108,
-9.66635394171129));
#106936=CARTESIAN_POINT('Ctrl Pts',(-16.6591420175153,19.6313722058962,
-9.66559997756064));
#106937=CARTESIAN_POINT('Ctrl Pts',(-16.6606866560881,19.6389254757344,
-9.66512677221462));
#106938=CARTESIAN_POINT('Ctrl Pts',(-16.6720299713919,19.6928907500064,
-9.66172678035979));
#106939=CARTESIAN_POINT('Ctrl Pts',(-16.6833441228806,19.7389666757993,
-9.65872275899436));
#106940=CARTESIAN_POINT('Ctrl Pts',(-16.7061569268642,19.8200100078691,
-9.6533034696357));
#106941=CARTESIAN_POINT('Ctrl Pts',(-16.7170387987474,19.8551335458005,
-9.65090847010828));
#106942=CARTESIAN_POINT('Ctrl Pts',(-16.7290822194177,19.8907016370013,
-9.6484462209914));
#106943=CARTESIAN_POINT('Ctrl Pts',(-16.7293356236529,19.8914486464457,
-9.64839449140688));
#106944=CARTESIAN_POINT('Ctrl Pts',(-16.7712938712655,20.014910343315,-9.63984213495151));
#106945=CARTESIAN_POINT('Ctrl Pts',(-16.8241832259323,20.133545787856,-9.63119483620107));
#106946=CARTESIAN_POINT('Ctrl Pts',(-16.9306698863168,20.3234047045237,
-9.61710172206642));
#106947=CARTESIAN_POINT('Ctrl Pts',(-16.9785020373741,20.3974543903341,
-9.61152620200881));
#106948=CARTESIAN_POINT('Ctrl Pts',(-17.0429888147084,20.4848093974725,
-9.60486274947755));
#106949=CARTESIAN_POINT('Ctrl Pts',(-17.0554027018575,20.5011241672537,
-9.60361401279766));
#106950=CARTESIAN_POINT('Ctrl Pts',(-17.0735168984427,20.5242262992094,
-9.60183908637065));
#106951=CARTESIAN_POINT('Ctrl Pts',(-17.0790255955911,20.5311617961332,
-9.60130535176057));
#106952=CARTESIAN_POINT('Ctrl Pts',(-17.0886517344082,20.5431262413686,
-9.60038299268831));
#106953=CARTESIAN_POINT('Ctrl Pts',(-17.0927490778357,20.5481711371344,
-9.59999356997746));
#106954=CARTESIAN_POINT('Ctrl Pts',(-17.1006725612993,20.5578357200678,
-9.59924653930038));
#106955=CARTESIAN_POINT('Ctrl Pts',(-17.1044952253837,20.5624581641716,
-9.59888879617962));
#106956=CARTESIAN_POINT('Ctrl Pts',(-17.1145622903182,20.5745266548548,
-9.59795356289297));
#106957=CARTESIAN_POINT('Ctrl Pts',(-17.1208384511196,20.5819461171163,
-9.59737737356893));
#106958=CARTESIAN_POINT('Ctrl Pts',(-17.142805149784,20.6075546780837,-9.59538407980322));
#106959=CARTESIAN_POINT('Ctrl Pts',(-17.158754372078,20.6255201664292,-9.59397766381086));
#106960=CARTESIAN_POINT('Ctrl Pts',(-17.2751770633516,20.7522488723551,
-9.58398811811653));
#106961=CARTESIAN_POINT('Ctrl Pts',(-17.3865124199935,20.8504805127702,
-9.57591395001439));
#106962=CARTESIAN_POINT('Ctrl Pts',(-17.5448576694999,20.9630743684982,
-9.56536229977445));
#106963=CARTESIAN_POINT('Ctrl Pts',(-17.5833811467825,20.9886108206187,
-9.56285552616156));
#106964=CARTESIAN_POINT('Ctrl Pts',(-17.6834747591274,21.0503430218408,
-9.55642254511744));
#106965=CARTESIAN_POINT('Ctrl Pts',(-17.7460932155647,21.0847194742361,
-9.55247223031956));
#106966=CARTESIAN_POINT('Ctrl Pts',(-17.8405323244734,21.1305134029403,
-9.54645283652381));
#106967=CARTESIAN_POINT('Ctrl Pts',(-17.8710840248494,21.1444404374242,
-9.5444962879679));
#106968=CARTESIAN_POINT('Ctrl Pts',(-17.9086746611854,21.1605077679038,
-9.54206261370465));
#106969=CARTESIAN_POINT('Ctrl Pts',(-17.9154121177493,21.163346364633,-9.54162540426563));
#106970=CARTESIAN_POINT('Ctrl Pts',(-17.9259740272493,21.1677319811952,
-9.5409382274285));
#106971=CARTESIAN_POINT('Ctrl Pts',(-17.9297886027342,21.1693028485686,
-9.54068968077592));
#106972=CARTESIAN_POINT('Ctrl Pts',(-17.936912541271,21.172212208473,-9.54022478487092));
#106973=CARTESIAN_POINT('Ctrl Pts',(-17.9402207066579,21.173553483691,-9.54000860679316));
#106974=CARTESIAN_POINT('Ctrl Pts',(-17.9477608243921,21.1765883944744,
-9.53951522564785));
#106975=CARTESIAN_POINT('Ctrl Pts',(-17.9519948472268,21.1782767263126,
-9.53923770867076));
#106976=CARTESIAN_POINT('Ctrl Pts',(-17.9630171687524,21.182630711101,-9.53851410512816));
#106977=CARTESIAN_POINT('Ctrl Pts',(-17.9698137820198,21.1852749574866,
-9.53806678319188));
#106978=CARTESIAN_POINT('Ctrl Pts',(-18.0131748559959,21.2018872853939,
-9.53520638856773));
#106979=CARTESIAN_POINT('Ctrl Pts',(-18.0501046568233,21.2148731954422,
-9.53274068511487));
#106980=CARTESIAN_POINT('Ctrl Pts',(-18.0991255561503,21.230597941644,-9.52944826186314));
#106981=CARTESIAN_POINT('Ctrl Pts',(-18.1109133790197,21.234265790091,-9.52865508276562));
#106982=CARTESIAN_POINT('Ctrl Pts',(-18.1458487131312,21.2448018662563,
-9.52630129409243));
#106983=CARTESIAN_POINT('Ctrl Pts',(-18.1690820104827,21.2513773108174,
-9.52473200362552));
#106984=CARTESIAN_POINT('Ctrl Pts',(-18.3317803462426,21.294432047482,-9.51373625927888));
#106985=CARTESIAN_POINT('Ctrl Pts',(-18.4745551729318,21.3169827093222,
-9.50408913664737));
#106986=CARTESIAN_POINT('Ctrl Pts',(-18.68023113681,21.3282194912357,-9.49078088416227));
#106987=CARTESIAN_POINT('Ctrl Pts',(-18.7420711405565,21.3288870253313,
-9.48684929269609));
#106988=CARTESIAN_POINT('Ctrl Pts',(-18.8410951737027,21.3256176609582,
-9.48067566997719));
#106989=CARTESIAN_POINT('Ctrl Pts',(-18.8782965760856,21.3234052648851,
-9.47838372291228));
#106990=CARTESIAN_POINT('Ctrl Pts',(-18.9265161329777,21.3192576990847,
-9.47544662757999));
#106991=CARTESIAN_POINT('Ctrl Pts',(-18.9376025842254,21.3182159315848,
-9.47477364703566));
#106992=CARTESIAN_POINT('Ctrl Pts',(-18.9556144879361,21.3163799179574,
-9.47368389618655));
#106993=CARTESIAN_POINT('Ctrl Pts',(-18.9625450378592,21.3156388639573,
-9.47326546000194));
#106994=CARTESIAN_POINT('Ctrl Pts',(-18.9758627018832,21.3141483038161,
-9.4724630360659));
#106995=CARTESIAN_POINT('Ctrl Pts',(-18.9822502983172,21.3134038967813,
-9.47207889239622));
#106996=CARTESIAN_POINT('Ctrl Pts',(-18.9968632875222,21.3116333806082,
-9.4712016990185));
#106997=CARTESIAN_POINT('Ctrl Pts',(-19.0050862775266,21.310588040729,-9.47070926125003));
#106998=CARTESIAN_POINT('Ctrl Pts',(-19.0269054865848,21.3076839726392,
-9.46940560537363));
#106999=CARTESIAN_POINT('Ctrl Pts',(-19.0404902736747,21.3057412801023,
-9.46859703901192));
#107000=CARTESIAN_POINT('Ctrl Pts',(-19.1432879196679,21.2900192595542,
-9.46250020157523));
#107001=CARTESIAN_POINT('Ctrl Pts',(-19.2315620229315,21.2706777856789,
-9.4573944194948));
#107002=CARTESIAN_POINT('Ctrl Pts',(-19.4524107508922,21.2072545595245,
-9.44467444557782));
#107003=CARTESIAN_POINT('Ctrl Pts',(-19.5823414692185,21.1555979458743,
-9.43725498332676));
#107004=CARTESIAN_POINT('Ctrl Pts',(-19.7553604313235,21.0661466388808,
-9.42649624725405));
#107005=CARTESIAN_POINT('Ctrl Pts',(-19.8034593809973,21.0388407930322,
-9.42339814111303));
#107006=CARTESIAN_POINT('Ctrl Pts',(-19.8746319785227,20.9946644931094,
-9.41856625612374));
#107007=CARTESIAN_POINT('Ctrl Pts',(-19.8985260773497,20.9791569980145,
-9.41689961041943));
#107008=CARTESIAN_POINT('Ctrl Pts',(-19.9278456881352,20.9592762042554,
-9.41478899006835));
#107009=CARTESIAN_POINT('Ctrl Pts',(-19.9335733775351,20.9553511465029,
-9.41437349798387));
#107010=CARTESIAN_POINT('Ctrl Pts',(-19.9426064189659,20.9490954750897,
-9.4137130155325));
#107011=CARTESIAN_POINT('Ctrl Pts',(-19.9459246377392,20.9467834047782,
-9.41346927003957));
#107012=CARTESIAN_POINT('Ctrl Pts',(-19.9521703958111,20.9424048422397,
-9.41300831474008));
#107013=CARTESIAN_POINT('Ctrl Pts',(-19.9550993207377,20.9403404202584,
-9.41279124557676));
#107014=CARTESIAN_POINT('Ctrl Pts',(-19.961783870699,20.935603436798,-9.4122937769743));
#107015=CARTESIAN_POINT('Ctrl Pts',(-19.965536013193,20.9329260421533,-9.41201304812349));
#107016=CARTESIAN_POINT('Ctrl Pts',(-19.9754745491542,20.9257851580766,
-9.4112655599105));
#107017=CARTESIAN_POINT('Ctrl Pts',(-19.9816455459255,20.9213004947281,
-9.41079739545133));
#107018=CARTESIAN_POINT('Ctrl Pts',(-20.0247025304064,20.889652555765,-9.40750326036925));
#107019=CARTESIAN_POINT('Ctrl Pts',(-20.0607197777586,20.8613337140389,
-9.40460522594295));
#107020=CARTESIAN_POINT('Ctrl Pts',(-20.1245701421479,20.8076893628077,
-9.39924379076558));
#107021=CARTESIAN_POINT('Ctrl Pts',(-20.1527027882546,20.782745658247,-9.3967964306359));
#107022=CARTESIAN_POINT('Ctrl Pts',(-20.2758192823856,20.6675853647251,
-9.38574631474252));
#107023=CARTESIAN_POINT('Ctrl Pts',(-20.3629792372826,20.5694100832347,
-9.37700311419997));
#107024=CARTESIAN_POINT('Ctrl Pts',(-20.492797290268,20.3925790132671,-9.3627986467188));
#107025=CARTESIAN_POINT('Ctrl Pts',(-20.5405828338921,20.3181399016093,
-9.35720324779837));
#107026=CARTESIAN_POINT('Ctrl Pts',(-20.5935715870133,20.2229803661569,
-9.3505187402978));
#107027=CARTESIAN_POINT('Ctrl Pts',(-20.6033012793282,20.2048931142049,
-9.34926768696914));
#107028=CARTESIAN_POINT('Ctrl Pts',(-20.6168513889154,20.1788007058475,
-9.34749007724529));
#107029=CARTESIAN_POINT('Ctrl Pts',(-20.6208868697482,20.1709091120963,
-9.34695594462113));
#107030=CARTESIAN_POINT('Ctrl Pts',(-20.6277957962641,20.1571864165471,
-9.34603311890173));
#107031=CARTESIAN_POINT('Ctrl Pts',(-20.6306921430164,20.1513670394523,
-9.34564362532734));
#107032=CARTESIAN_POINT('Ctrl Pts',(-20.636208878151,20.140153563533,-9.34489661203854));
#107033=CARTESIAN_POINT('Ctrl Pts',(-20.6388332360916,20.1347614976619,
-9.34453895643853));
#107034=CARTESIAN_POINT('Ctrl Pts',(-20.6456466884508,20.1206099240407,
-9.34360429179119));
#107035=CARTESIAN_POINT('Ctrl Pts',(-20.6497985246213,20.1118325555888,
-9.34302858047085));
#107036=CARTESIAN_POINT('Ctrl Pts',(-20.6639911336504,20.0812861125865,
-9.34103860563081));
#107037=CARTESIAN_POINT('Ctrl Pts',(-20.6737226594694,20.0593747797715,
-9.33963498255815));
#107038=CARTESIAN_POINT('Ctrl Pts',(-20.742914465457,19.8961652662946,-9.32934412035894));
#107039=CARTESIAN_POINT('Ctrl Pts',(-20.7872440914993,19.7489445395367,
-9.32100728448304));
#107040=CARTESIAN_POINT('Ctrl Pts',(-20.8390879899929,19.4702807547455,
-9.30561476859398));
#107041=CARTESIAN_POINT('Ctrl Pts',(-20.8510398088518,19.3404434101152,
-9.29857236344691));
#107042=CARTESIAN_POINT('Ctrl Pts',(-20.8509988956986,19.2070755044686,
-9.29078137624927));
#107043=CARTESIAN_POINT('Ctrl Pts',(-20.8509902910738,19.2038004665512,
-9.29058970680201));
#107044=CARTESIAN_POINT('Ctrl Pts',(-20.8508966094021,19.1848667378393,
-9.28947952790844));
#107045=CARTESIAN_POINT('Ctrl Pts',(-20.850645400934,19.1692098497994,-9.28855320314594));
#107046=CARTESIAN_POINT('Ctrl Pts',(-20.8500635583701,19.1477742975099,
-9.28727189919378));
#107047=CARTESIAN_POINT('Ctrl Pts',(-20.8498828690298,19.14199162895,-9.28692493644138));
#107048=CARTESIAN_POINT('Ctrl Pts',(-20.8495580047971,19.1328018054636,
-9.28637136546238));
#107049=CARTESIAN_POINT('Ctrl Pts',(-20.8494292952819,19.1293940837142,
-9.28616561716021));
#107050=CARTESIAN_POINT('Ctrl Pts',(-20.8491463961677,19.1223550151953,
-9.2857396080172));
#107051=CARTESIAN_POINT('Ctrl Pts',(-20.8489910887203,19.1187237603298,
-9.28551928295103));
#107052=CARTESIAN_POINT('Ctrl Pts',(-20.8485986099401,19.1100692907856,
-9.28499286777946));
#107053=CARTESIAN_POINT('Ctrl Pts',(-20.8483528901894,19.1050465018352,
-9.28468630279956));
#107054=CARTESIAN_POINT('Ctrl Pts',(-20.847463120908,19.088096318964,-9.28364831690258));
#107055=CARTESIAN_POINT('Ctrl Pts',(-20.8467360342108,19.0761737677434,
-9.28291246841416));
#107056=CARTESIAN_POINT('Ctrl Pts',(-20.8368853576822,18.9344026989202,
-9.27409923509962));
#107057=CARTESIAN_POINT('Ctrl Pts',(-20.8159060912923,18.8056692574441,
-9.26548169761633));
#107058=CARTESIAN_POINT('Ctrl Pts',(-20.7661530760357,18.6137727633789,
-9.25238175885633));
#107059=CARTESIAN_POINT('Ctrl Pts',(-20.745904045056,18.5487650723614,-9.24789386380929));
#107060=CARTESIAN_POINT('Ctrl Pts',(-20.7225807588464,18.4848901146894,
-9.24346988827878));
#107061=CARTESIAN_POINT('Origin',(-18.734,19.211,0.));
#107062=CARTESIAN_POINT('',(-20.7225806137986,18.4848897174502,-8.44448866019381));
#107063=CARTESIAN_POINT('',(-20.7225805936643,18.484889662309,-8.66553669489169));
#107064=CARTESIAN_POINT('',(-20.7225806137986,18.4848897174502,0.));
#107065=CARTESIAN_POINT('',(-20.8509999986719,19.2110749873286,-8.71094372102529));
#107066=CARTESIAN_POINT('Ctrl Pts',(-20.7225805936643,18.484889662309,-8.66553669489169));
#107067=CARTESIAN_POINT('Ctrl Pts',(-20.7775649874159,18.6354740744751,
-8.67608256008694));
#107068=CARTESIAN_POINT('Ctrl Pts',(-20.8152928026166,18.7918910934345,
-8.68676276296178));
#107069=CARTESIAN_POINT('Ctrl Pts',(-20.8382408983242,18.9774167511052,
-8.69860361758393));
#107070=CARTESIAN_POINT('Ctrl Pts',(-20.8409993784059,19.0037691959386,
-8.70026806086961));
#107071=CARTESIAN_POINT('Ctrl Pts',(-20.8463154926722,19.0657772647298,
-8.70414334614212));
#107072=CARTESIAN_POINT('Ctrl Pts',(-20.8484662881568,19.1014603085863,
-8.70634148136337));
#107073=CARTESIAN_POINT('Ctrl Pts',(-20.8501018463908,19.1483376863317,
-8.70918910543019));
#107074=CARTESIAN_POINT('Ctrl Pts',(-20.8504028279016,19.1594959479233,
-8.70986396462703));
#107075=CARTESIAN_POINT('Ctrl Pts',(-20.8507477575,19.1775925090626,-8.71095377752203));
#107076=CARTESIAN_POINT('Ctrl Pts',(-20.8508458709025,19.1845294511023,
-8.71137042056006));
#107077=CARTESIAN_POINT('Ctrl Pts',(-20.8509497984104,19.1957925998922,
-8.71204512860756));
#107078=CARTESIAN_POINT('Ctrl Pts',(-20.8509764542535,19.2001185215261,
-8.71230384414341));
#107079=CARTESIAN_POINT('Ctrl Pts',(-20.8509965706163,19.2066147860699,
-8.7126917300085));
#107080=CARTESIAN_POINT('Ctrl Pts',(-20.850999953759,19.2087850666355,-8.71282121002485));
#107081=CARTESIAN_POINT('Ctrl Pts',(-20.8509999995292,19.2109553535338,
-8.71295058578666));
#107082=CARTESIAN_POINT('Ctrl Pts',(-20.8509999986719,19.2110749873286,
-8.71094372102529));
#107083=CARTESIAN_POINT('Ctrl Pts',(-20.8509972790728,19.2878531769888,
-8.71553605185449));
#107084=CARTESIAN_POINT('Ctrl Pts',(-20.8468134450972,19.3645459476709,
-8.7201283826837));
#107085=CARTESIAN_POINT('Ctrl Pts',(-20.8385019469854,19.440696658954,-8.72472071351291));
#107086=CARTESIAN_POINT('Ctrl Pts',(-20.8301661890788,19.5170696407114,
-8.72932644854457));
#107087=CARTESIAN_POINT('Ctrl Pts',(-20.8176787337246,19.5928969954346,
-8.73393218357623));
#107088=CARTESIAN_POINT('Ctrl Pts',(-20.8011445449252,19.6677301505114,
-8.7385379186079));
#107089=CARTESIAN_POINT('Ctrl Pts',(-20.7845848825973,19.742678597879,-8.74315074950159));
#107090=CARTESIAN_POINT('Ctrl Pts',(-20.7639661648764,19.8166294002047,
-8.74776358039528));
#107091=CARTESIAN_POINT('Ctrl Pts',(-20.7394430352779,19.8891498597325,
-8.75237641128897));
#107092=CARTESIAN_POINT('Ctrl Pts',(-20.7148521353619,19.9618707314692,
-8.75700198986289));
#107093=CARTESIAN_POINT('Ctrl Pts',(-20.6863354068359,20.0331529809764,
-8.76162756843682));
#107094=CARTESIAN_POINT('Ctrl Pts',(-20.6540955877885,20.1025839465552,
-8.76625314701075));
#107095=CARTESIAN_POINT('Ctrl Pts',(-20.6367568977556,20.1399241682573,
-8.76874079971745));
#107096=CARTESIAN_POINT('Ctrl Pts',(-20.6183421527917,20.1767293760292,
-8.77122845242414));
#107097=CARTESIAN_POINT('Ctrl Pts',(-20.5988881380091,20.2129387370059,
-8.77371610513084));
#107098=CARTESIAN_POINT('Ctrl Pts',(-20.5645713376049,20.2768118977537,
-8.77810431406173));
#107099=CARTESIAN_POINT('Ctrl Pts',(-20.5269022333032,20.3390446523177,
-8.78249252299262));
#107100=CARTESIAN_POINT('Ctrl Pts',(-20.4860618340585,20.399262735945,-8.78688073192352));
#107101=CARTESIAN_POINT('Ctrl Pts',(-20.4452820487377,20.459391445952,-8.79126242802478));
#107102=CARTESIAN_POINT('Ctrl Pts',(-20.4013405804888,20.5175110248669,
-8.79564412412605));
#107103=CARTESIAN_POINT('Ctrl Pts',(-20.3544642120284,20.5732719029384,
-8.80002582022731));
#107104=CARTESIAN_POINT('Ctrl Pts',(-20.3076429270315,20.6289672575405,
-8.80440236748695));
#107105=CARTESIAN_POINT('Ctrl Pts',(-20.2578939016355,20.6823090498171,
-8.80877891474658));
#107106=CARTESIAN_POINT('Ctrl Pts',(-20.2054860875607,20.732978217359,-8.81315546200621));
#107107=CARTESIAN_POINT('Ctrl Pts',(-20.1531115097599,20.7836152512513,
-8.81752923372318));
#107108=CARTESIAN_POINT('Ctrl Pts',(-20.0980818347941,20.8315826889225,
-8.82190300544015));
#107109=CARTESIAN_POINT('Ctrl Pts',(-20.0407040448455,20.8765970518659,
-8.82627677715712));
#107110=CARTESIAN_POINT('Ctrl Pts',(-19.9833437151512,20.9215977167874,
-8.83064921792067));
#107111=CARTESIAN_POINT('Ctrl Pts',(-19.9236370683482,20.9636467934742,
-8.83502165868421));
#107112=CARTESIAN_POINT('Ctrl Pts',(-19.8619241653176,21.0025010681807,
-8.83939409944776));
#107113=CARTESIAN_POINT('Ctrl Pts',(-19.8002096842813,21.0413563363953,
-8.8437666520151));
#107114=CARTESIAN_POINT('Ctrl Pts',(-19.7364892544409,21.0770163851234,
-8.84813920458243));
#107115=CARTESIAN_POINT('Ctrl Pts',(-19.6711304798876,21.1092822402545,
-8.85251175714977));
#107116=CARTESIAN_POINT('Ctrl Pts',(-19.6057038735327,21.1415815821071,
-8.85688884771709));
#107117=CARTESIAN_POINT('Ctrl Pts',(-19.5386359610959,21.1704794832197,
-8.86126593828441));
#107118=CARTESIAN_POINT('Ctrl Pts',(-19.4703166749626,21.1958241116462,
-8.86564302885173));
#107119=CARTESIAN_POINT('Ctrl Pts',(-19.4019600771315,21.2211825817149,
-8.87002250991067));
#107120=CARTESIAN_POINT('Ctrl Pts',(-19.3323512055658,21.2429837711606,
-8.87440199096961));
#107121=CARTESIAN_POINT('Ctrl Pts',(-19.2618949953294,21.2611258190429,
-8.87878147202854));
#107122=CARTESIAN_POINT('Ctrl Pts',(-19.1913139019334,21.2793000235832,
-8.88316871568826));
#107123=CARTESIAN_POINT('Ctrl Pts',(-19.1198829437791,21.2938020386136,
-8.88755595934798));
#107124=CARTESIAN_POINT('Ctrl Pts',(-19.0480164983111,21.3045812950035,
-8.89194320300769));
#107125=CARTESIAN_POINT('Ctrl Pts',(-18.9991542404263,21.311910150662,-8.89492610594255));
#107126=CARTESIAN_POINT('Ctrl Pts',(-18.9500908178376,21.3175191746182,
-8.89790900887741));
#107127=CARTESIAN_POINT('Ctrl Pts',(-18.9009566611241,21.3214062341896,
-8.90089191181226));
#107128=CARTESIAN_POINT('Ctrl Pts',(-18.8286744078927,21.3271245662635,
-8.90528012074316));
#107129=CARTESIAN_POINT('Ctrl Pts',(-18.7559569381438,21.3291362205188,
-8.90966832967406));
#107130=CARTESIAN_POINT('Ctrl Pts',(-18.6832169260197,21.3273908144284,
-8.91405653860496));
#107131=CARTESIAN_POINT('Ctrl Pts',(-18.6105848721342,21.3256479988102,
-8.91843823470623));
#107132=CARTESIAN_POINT('Ctrl Pts',(-18.5379308205422,21.3201592036426,
-8.92281993080749));
#107133=CARTESIAN_POINT('Ctrl Pts',(-18.4656714572674,21.3109259018249,
-8.92720162690876));
#107134=CARTESIAN_POINT('Ctrl Pts',(-18.393497004495,21.3017034498716,-8.9315781741684));
#107135=CARTESIAN_POINT('Ctrl Pts',(-18.3217167948299,21.2887452929197,
-8.93595472142804));
#107136=CARTESIAN_POINT('Ctrl Pts',(-18.2507446877308,21.2721048743729,
-8.94033126868768));
#107137=CARTESIAN_POINT('Ctrl Pts',(-18.1798175901105,21.2554750089376,
-8.94470504040465));
#107138=CARTESIAN_POINT('Ctrl Pts',(-18.1096980467019,21.2351676251632,
-8.94907881212163));
#107139=CARTESIAN_POINT('Ctrl Pts',(-18.0407905817005,21.2112874049448,
-8.9534525838386));
#107140=CARTESIAN_POINT('Ctrl Pts',(-17.9719040854722,21.1874144515577,
-8.95782502460215));
#107141=CARTESIAN_POINT('Ctrl Pts',(-17.9042293909009,21.1599709780648,
-8.96219746536571));
#107142=CARTESIAN_POINT('Ctrl Pts',(-17.8381550707622,21.1291112748636,
-8.96656990612926));
#107143=CARTESIAN_POINT('Ctrl Pts',(-17.772079061096,21.0982507825765,-8.9709424586966));
#107144=CARTESIAN_POINT('Ctrl Pts',(-17.7076039433216,21.0639740930875,
-8.97531501126394));
#107145=CARTESIAN_POINT('Ctrl Pts',(-17.6450960003,21.0264826023505,-8.97968756383129));
#107146=CARTESIAN_POINT('Ctrl Pts',(-17.5825231841774,20.9889522015303,
-8.98406465439861));
#107147=CARTESIAN_POINT('Ctrl Pts',(-17.5219220335752,20.9482005866783,
-8.98844174496594));
#107148=CARTESIAN_POINT('Ctrl Pts',(-17.4636312781367,20.9044734454698,
-8.99281883553327));
#107149=CARTESIAN_POINT('Ctrl Pts',(-17.4053086879533,20.8607224232466,
-8.99719831659221));
#107150=CARTESIAN_POINT('Ctrl Pts',(-17.3492993758006,20.8139929484573,
-9.00157779765115));
#107151=CARTESIAN_POINT('Ctrl Pts',(-17.2959081742797,20.7645703720129,
-9.0059572787101));
#107152=CARTESIAN_POINT('Ctrl Pts',(-17.2424223372125,20.7150601943836,
-9.01034452236982));
#107153=CARTESIAN_POINT('Ctrl Pts',(-17.1915642147119,20.6628477284534,
-9.01473176602953));
#107154=CARTESIAN_POINT('Ctrl Pts',(-17.1436006220655,20.6082540279654,
-9.01911900968925));
#107155=CARTESIAN_POINT('Ctrl Pts',(-17.1109900008267,20.57113557227,-9.02210191262407));
#107156=CARTESIAN_POINT('Ctrl Pts',(-17.0797165992414,20.5329170566123,
-9.02508481555889));
#107157=CARTESIAN_POINT('Ctrl Pts',(-17.0498528101568,20.4937069980877,
-9.0280677184937));
#107158=CARTESIAN_POINT('Ctrl Pts',(-17.0059195850955,20.4360242867296,
-9.0324559274246));
#107159=CARTESIAN_POINT('Ctrl Pts',(-16.9648675150388,20.3759692727541,
-9.0368441363555));
#107160=CARTESIAN_POINT('Ctrl Pts',(-16.9269623364049,20.3138616787018,
-9.0412323452864));
#107161=CARTESIAN_POINT('Ctrl Pts',(-16.889113415341,20.2518462626167,-9.04561404138767));
#107162=CARTESIAN_POINT('Ctrl Pts',(-16.8544023633226,20.1877847222597,
-9.04999573748894));
#107163=CARTESIAN_POINT('Ctrl Pts',(-16.8230534861161,20.1220282218872,
-9.05437743359021));
#107164=CARTESIAN_POINT('Ctrl Pts',(-16.7917414463352,20.0563489906357,
-9.05875398084985));
#107165=CARTESIAN_POINT('Ctrl Pts',(-16.7637839395866,19.9889791891847,
-9.06313052810949));
#107166=CARTESIAN_POINT('Ctrl Pts',(-16.7393600427009,19.9202957357448,
-9.06750707536913));
#107167=CARTESIAN_POINT('Ctrl Pts',(-16.7149516350957,19.851655840353,-9.07188084708611));
#107168=CARTESIAN_POINT('Ctrl Pts',(-16.694072552212,19.7817043993275,-9.07625461880308));
#107169=CARTESIAN_POINT('Ctrl Pts',(-16.6768537344171,19.7108382158241,
-9.08062839052006));
#107170=CARTESIAN_POINT('Ctrl Pts',(-16.6596401563662,19.6399935971384,
-9.08500083128361));
#107171=CARTESIAN_POINT('Ctrl Pts',(-16.6460847459306,19.5682352570613,
-9.08937327204717));
#107172=CARTESIAN_POINT('Ctrl Pts',(-16.6362680963764,19.4959734382704,
-9.09374571281072));
#107173=CARTESIAN_POINT('Ctrl Pts',(-16.6264511958094,19.4237097717368,
-9.09811826537807));
#107174=CARTESIAN_POINT('Ctrl Pts',(-16.620373308882,19.3509430791855,-9.10249081794542));
#107175=CARTESIAN_POINT('Ctrl Pts',(-16.6180633554341,19.2780903583472,
-9.10686337051276));
#107176=CARTESIAN_POINT('Ctrl Pts',(-16.6157510046294,19.2051620282073,
-9.11124046108009));
#107177=CARTESIAN_POINT('Ctrl Pts',(-16.6172144102078,19.1321479746869,
-9.11561755164742));
#107178=CARTESIAN_POINT('Ctrl Pts',(-16.6224303356468,19.0594660018898,
-9.11999464221475));
#107179=CARTESIAN_POINT('Ctrl Pts',(-16.6276491096962,18.9867443347699,
-9.12437412327369));
#107180=CARTESIAN_POINT('Ctrl Pts',(-16.6366244245267,18.9143555885064,
-9.12875360433264));
#107181=CARTESIAN_POINT('Ctrl Pts',(-16.6492813452852,18.8427105341121,
-9.13313308539158));
#107182=CARTESIAN_POINT('Ctrl Pts',(-16.6619607003507,18.7709384893398,
-9.1375203290513));
#107183=CARTESIAN_POINT('Ctrl Pts',(-16.6783345842871,18.6999132392689,
-9.14190757271103));
#107184=CARTESIAN_POINT('Ctrl Pts',(-16.6982774637592,18.6300329136335,
-9.14629481637075));
#107185=CARTESIAN_POINT('Ctrl Pts',(-16.7118367001087,18.582521025854,-9.14927771930555));
#107186=CARTESIAN_POINT('Ctrl Pts',(-16.7270447244344,18.5355380865901,
-9.15226062224035));
#107187=CARTESIAN_POINT('Ctrl Pts',(-16.7438494759072,18.4892037050155,
-9.15524352517515));
#107188=CARTESIAN_POINT('Ctrl Pts',(-16.7685712862063,18.4210402577036,
-9.15963173410604));
#107189=CARTESIAN_POINT('Ctrl Pts',(-16.79684734214,18.3540153233854,-9.16401994303694));
#107190=CARTESIAN_POINT('Ctrl Pts',(-16.8285526457322,18.2885254040822,
-9.16840815196783));
#107191=CARTESIAN_POINT('Ctrl Pts',(-16.860210893397,18.2231326826776,-9.1727898480691));
#107192=CARTESIAN_POINT('Ctrl Pts',(-16.8952880767682,18.1592708843012,
-9.17717154417036));
#107193=CARTESIAN_POINT('Ctrl Pts',(-16.9336103347363,18.097318693157,-9.18155324027162));
#107194=CARTESIAN_POINT('Ctrl Pts',(-16.9718875610014,18.0354393007677,
-9.18592978753126));
#107195=CARTESIAN_POINT('Ctrl Pts',(-17.0134020343725,17.9754654662074,
-9.1903063347909));
#107196=CARTESIAN_POINT('Ctrl Pts',(-17.0579337571748,17.9177517834298,
-9.19468288205053));
#107197=CARTESIAN_POINT('Ctrl Pts',(-17.1024372386058,17.8600747018311,
-9.1990566537675));
#107198=CARTESIAN_POINT('Ctrl Pts',(-17.1499538788908,17.8046553090193,
-9.20343042548448));
#107199=CARTESIAN_POINT('Ctrl Pts',(-17.2002209049087,17.7518184871439,
-9.20780419720145));
#107200=CARTESIAN_POINT('Ctrl Pts',(-17.2504726345018,17.6989977436909,
-9.212176637965));
#107201=CARTESIAN_POINT('Ctrl Pts',(-17.3034727559329,17.6487583602256,
-9.21654907872854));
#107202=CARTESIAN_POINT('Ctrl Pts',(-17.358919943639,17.6013901595112,-9.22092151949209));
#107203=CARTESIAN_POINT('Ctrl Pts',(-17.4143685491359,17.5540207475868,
-9.22529407205944));
#107204=CARTESIAN_POINT('Ctrl Pts',(-17.4722639770751,17.5095229759788,
-9.22966662462678));
#107205=CARTESIAN_POINT('Ctrl Pts',(-17.5322712521174,17.4681468746585,
-9.23403917719411));
#107206=CARTESIAN_POINT('Ctrl Pts',(-17.5923408049732,17.4267278316597,
-9.23841626776144));
#107207=CARTESIAN_POINT('Ctrl Pts',(-17.6545261829432,17.3884372018126,
-9.24279335832876));
#107208=CARTESIAN_POINT('Ctrl Pts',(-17.7184635014061,17.3534815963163,
-9.24717044889609));
#107209=CARTESIAN_POINT('Ctrl Pts',(-17.7824357384117,17.3185069002664,
-9.25154992995503));
#107210=CARTESIAN_POINT('Ctrl Pts',(-17.8481613859391,17.2868710642732,
-9.25592941101397));
#107211=CARTESIAN_POINT('Ctrl Pts',(-17.9152544897581,17.2587334225422,
-9.26030889207291));
#107212=CARTESIAN_POINT('Ctrl Pts',(-17.9824665156532,17.2305459070301,
-9.26469613573263));
#107213=CARTESIAN_POINT('Ctrl Pts',(-18.0510503837927,17.2058691314343,
-9.26908337939234));
#107214=CARTESIAN_POINT('Ctrl Pts',(-18.1206033812623,17.1848130421599,
-9.27347062305206));
#107215=CARTESIAN_POINT('Ctrl Pts',(-18.167892717431,17.1704969304132,-9.2764535259869));
#107216=CARTESIAN_POINT('Ctrl Pts',(-18.2156297492657,17.1578534982273,
-9.27943642892174));
#107217=CARTESIAN_POINT('Ctrl Pts',(-18.2636857248405,17.1469037128609,
-9.28241933185657));
#107218=CARTESIAN_POINT('Ctrl Pts',(-18.3343818439592,17.1307952618032,
-9.28680754078747));
#107219=CARTESIAN_POINT('Ctrl Pts',(-18.4060444995741,17.1182916243426,
-9.29119574971837));
#107220=CARTESIAN_POINT('Ctrl Pts',(-18.4782726371995,17.1095023159863,
-9.29558395864926));
#107221=CARTESIAN_POINT('Ctrl Pts',(-18.5503935762931,17.1007260524208,
-9.29996565475053));
#107222=CARTESIAN_POINT('Ctrl Pts',(-18.6230778564464,17.0956532323251,
-9.3043473508518));
#107223=CARTESIAN_POINT('Ctrl Pts',(-18.6959129564509,17.0943426405973,
-9.30872904695306));
#107224=CARTESIAN_POINT('Ctrl Pts',(-18.7686624694164,17.0930335889191,
-9.3131055942127));
#107225=CARTESIAN_POINT('Ctrl Pts',(-18.8415619702681,17.0954779920626,
-9.31748214147234));
#107226=CARTESIAN_POINT('Ctrl Pts',(-18.9141942210378,17.1016828017805,
-9.32185868873198));
#107227=CARTESIAN_POINT('Ctrl Pts',(-18.9867804094896,17.1078836764983,
-9.32623246044896));
#107228=CARTESIAN_POINT('Ctrl Pts',(-19.0590992046971,17.1178401850896,
-9.33060623216593));
#107229=CARTESIAN_POINT('Ctrl Pts',(-19.13073519808,17.1315072294897,-9.33498000388291));
#107230=CARTESIAN_POINT('Ctrl Pts',(-19.2023493923895,17.1451701149624,
-9.33935244464646));
#107231=CARTESIAN_POINT('Ctrl Pts',(-19.2732807238328,17.1625412042304,
-9.34372488541001));
#107232=CARTESIAN_POINT('Ctrl Pts',(-19.3431223955196,17.1835240057459,
-9.34809732617357));
#107233=CARTESIAN_POINT('Ctrl Pts',(-19.4129658530657,17.204507343794,-9.35246987874091));
#107234=CARTESIAN_POINT('Ctrl Pts',(-19.4817191341329,17.2291024367364,
-9.35684243130826));
#107235=CARTESIAN_POINT('Ctrl Pts',(-19.5489906872857,17.2571629598051,
-9.36121498387561));
#107236=CARTESIAN_POINT('Ctrl Pts',(-19.6163320573938,17.285252605143,-9.36559207444294));
#107237=CARTESIAN_POINT('Ctrl Pts',(-19.6821881831278,17.3168146752694,
-9.36996916501026));
#107238=CARTESIAN_POINT('Ctrl Pts',(-19.7461883733225,17.3516550355271,
-9.37434625557759));
#107239=CARTESIAN_POINT('Ctrl Pts',(-19.8102235163965,17.3865144233986,
-9.37872573663653));
#107240=CARTESIAN_POINT('Ctrl Pts',(-19.8724002944083,17.424655413658,-9.38310521769548));
#107241=CARTESIAN_POINT('Ctrl Pts',(-19.9323758228016,17.4658397244595,
-9.38748469875442));
#107242=CARTESIAN_POINT('Ctrl Pts',(-19.9924576574163,17.5070970341754,
-9.39187194241414));
#107243=CARTESIAN_POINT('Ctrl Pts',(-20.050330067536,17.5514081430505,-9.39625918607386));
#107244=CARTESIAN_POINT('Ctrl Pts',(-20.1056826247707,17.598493945158,-9.40064642973358));
#107245=CARTESIAN_POINT('Ctrl Pts',(-20.1433170299306,17.630507753414,-9.40362933266839));
#107246=CARTESIAN_POINT('Ctrl Pts',(-20.1797873054598,17.663803392597,-9.4066122356032));
#107247=CARTESIAN_POINT('Ctrl Pts',(-20.2150061302365,17.6982839518925,
-9.40959513853801));
#107248=CARTESIAN_POINT('Ctrl Pts',(-20.2660736595565,17.7482809913723,
-9.41392036756108));
#107249=CARTESIAN_POINT('Ctrl Pts',(-20.3147200093818,17.8009782881339,
-9.41824559658415));
#107250=CARTESIAN_POINT('Ctrl Pts',(-20.3606400168152,17.8561083970681,
-9.42257082560722));
#107251=CARTESIAN_POINT('Ctrl Pts',(-20.4064831242367,17.9111461822795,
-9.42688881137877));
#107252=CARTESIAN_POINT('Ctrl Pts',(-20.4496086380981,17.9686083126782,
-9.43120679715031));
#107253=CARTESIAN_POINT('Ctrl Pts',(-20.489747535905,18.0281899602372,-9.43552478292186));
#107254=CARTESIAN_POINT('Ctrl Pts',(-20.5298476914497,18.087714099296,-9.43983860095224));
#107255=CARTESIAN_POINT('Ctrl Pts',(-20.5669666687477,18.1493532900628,
-9.44415241898263));
#107256=CARTESIAN_POINT('Ctrl Pts',(-20.6008760498721,18.2127701595255,
-9.44846623701301));
#107257=CARTESIAN_POINT('Ctrl Pts',(-20.6347648510145,18.276148540582,-9.45277743693906));
#107258=CARTESIAN_POINT('Ctrl Pts',(-20.6654476851552,18.3413020229497,
-9.45708863686511));
#107259=CARTESIAN_POINT('Ctrl Pts',(-20.692740781525,18.4078664178416,-9.46139983679116));
#107260=CARTESIAN_POINT('Ctrl Pts',(-20.7031862293494,18.433341538157,-9.46304979300271));
#107261=CARTESIAN_POINT('Ctrl Pts',(-20.7131356639248,18.4590230623861,
-9.46469974921426));
#107262=CARTESIAN_POINT('Ctrl Pts',(-20.7225806137986,18.4848897174502,
-9.46634970542581));
#107263=CARTESIAN_POINT('',(-20.8509991049198,19.2129467328109,-8.4890562790225));
#107264=CARTESIAN_POINT('Ctrl Pts',(-20.7225807588464,18.4848901146894,
-9.24346988827878));
#107265=CARTESIAN_POINT('Ctrl Pts',(-20.6903083395894,18.39650636827,-9.23734843558896));
#107266=CARTESIAN_POINT('Ctrl Pts',(-20.6521496472009,18.3102912124771,
-9.23135300036806));
#107267=CARTESIAN_POINT('Ctrl Pts',(-20.5973016866332,18.2058341370534,
-9.2240858578963));
#107268=CARTESIAN_POINT('Ctrl Pts',(-20.5859225848332,18.1850202735708,
-9.22263722284196));
#107269=CARTESIAN_POINT('Ctrl Pts',(-20.5694165868721,18.1559983874074,
-9.2206157129183));
#107270=CARTESIAN_POINT('Ctrl Pts',(-20.5645798963423,18.1476281469331,
-9.22003249182282));
#107271=CARTESIAN_POINT('Ctrl Pts',(-20.5566541761581,18.1341264602102,
-9.21909131991471));
#107272=CARTESIAN_POINT('Ctrl Pts',(-20.5536004477713,18.1289745482744,
-9.21873209594647));
#107273=CARTESIAN_POINT('Ctrl Pts',(-20.5471836479079,18.1182528241218,
-9.217984278638));
#107274=CARTESIAN_POINT('Ctrl Pts',(-20.5438166747774,18.1126854109202,
-9.21759583267081));
#107275=CARTESIAN_POINT('Ctrl Pts',(-20.5357844895098,18.0995411280695,
-9.21667837924833));
#107276=CARTESIAN_POINT('Ctrl Pts',(-20.5310970461766,18.0919779354556,
-9.21615019438572));
#107277=CARTESIAN_POINT('Ctrl Pts',(-20.5153276832105,18.0668887096903,
-9.2143969132788));
#107278=CARTESIAN_POINT('Ctrl Pts',(-20.5040357536673,18.0494956154335,
-9.21317959276562));
#107279=CARTESIAN_POINT('Ctrl Pts',(-20.4423940085405,17.9575352427292,
-9.20672866183974));
#107280=CARTESIAN_POINT('Ctrl Pts',(-20.3875818629946,17.8860646473677,
-9.20166799572178));
#107281=CARTESIAN_POINT('Ctrl Pts',(-20.239237271279,17.7162386259572,-9.18923109939529));
#107282=CARTESIAN_POINT('Ctrl Pts',(-20.1405044242798,17.6229842972969,
-9.18201885997539));
#107283=CARTESIAN_POINT('Ctrl Pts',(-19.9740224059233,17.4935257233293,
-9.17034301708339));
#107284=CARTESIAN_POINT('Ctrl Pts',(-19.9120806441693,17.4504611918285,
-9.16608238927342));
#107285=CARTESIAN_POINT('Ctrl Pts',(-19.8399125093472,17.4058028978743,
-9.16105250608856));
#107286=CARTESIAN_POINT('Ctrl Pts',(-19.8318095060137,17.400863724253,-9.16048684628342));
#107287=CARTESIAN_POINT('Ctrl Pts',(-19.8197475229313,17.3936221394976,
-9.15964305507023));
#107288=CARTESIAN_POINT('Ctrl Pts',(-19.8158137093209,17.3912777495406,
-9.1593675912986));
#107289=CARTESIAN_POINT('Ctrl Pts',(-19.8087982558611,17.3871276178277,
-9.15887579078604));
#107290=CARTESIAN_POINT('Ctrl Pts',(-19.8057196225779,17.3853168928855,
-9.15865978255638));
#107291=CARTESIAN_POINT('Ctrl Pts',(-19.7990875252467,17.3814387235023,
-9.15819402960866));
#107292=CARTESIAN_POINT('Ctrl Pts',(-19.7955326690794,17.3793738665576,
-9.157944128941));
#107293=CARTESIAN_POINT('Ctrl Pts',(-19.7856957203983,17.3736982789767,
-9.15725195721474));
#107294=CARTESIAN_POINT('Ctrl Pts',(-19.7794011390049,17.3701094661957,
-9.15680831255862));
#107295=CARTESIAN_POINT('Ctrl Pts',(-19.7446856398884,17.3505521283599,
-9.15435807751532));
#107296=CARTESIAN_POINT('Ctrl Pts',(-19.7159188643973,17.3352103479093,
-9.15231500282216));
#107297=CARTESIAN_POINT('Ctrl Pts',(-19.5415662171688,17.2473348280452,
-9.13990762731865));
#107298=CARTESIAN_POINT('Ctrl Pts',(-19.3883729642573,17.1911138485735,
-9.12895444031794));
#107299=CARTESIAN_POINT('Ctrl Pts',(-19.1167166811949,17.1256085732853,
-9.11070156650593));
#107300=CARTESIAN_POINT('Ctrl Pts',(-19.0010936888834,17.1076697300265,
-9.10326200789545));
#107301=CARTESIAN_POINT('Ctrl Pts',(-18.8703108408879,17.0983446725026,
-9.09525614356276));
#107302=CARTESIAN_POINT('Ctrl Pts',(-18.8560477444649,17.0974727250556,
-9.09438818313206));
#107303=CARTESIAN_POINT('Ctrl Pts',(-18.8333331565297,17.0963148221154,
-9.09301389449998));
#107304=CARTESIAN_POINT('Ctrl Pts',(-18.8248870837847,17.0959349847366,
-9.0925046383631));
#107305=CARTESIAN_POINT('Ctrl Pts',(-18.8099870560799,17.0953543169118,
-9.09160926540666));
#107306=CARTESIAN_POINT('Ctrl Pts',(-18.8035340756784,17.0951323995075,
-9.09122249248421));
#107307=CARTESIAN_POINT('Ctrl Pts',(-18.7901850998829,17.0947344641633,
-9.09042442269024));
#107308=CARTESIAN_POINT('Ctrl Pts',(-18.7832890495817,17.0945626220126,
-9.09001326121201));
#107309=CARTESIAN_POINT('Ctrl Pts',(-18.7655855987095,17.0942080452139,
-9.08896054167088));
#107310=CARTESIAN_POINT('Ctrl Pts',(-18.7547773312555,17.0940743662193,
-9.0883205249654));
#107311=CARTESIAN_POINT('Ctrl Pts',(-18.7096624307513,17.0938619304368,
-9.085659783059));
#107312=CARTESIAN_POINT('Ctrl Pts',(-18.6753563294909,17.0945343046956,
-9.08366258832262));
#107313=CARTESIAN_POINT('Ctrl Pts',(-18.5860257293788,17.0984590033235,
-9.07851830035413));
#107314=CARTESIAN_POINT('Ctrl Pts',(-18.5310841793984,17.1030266456553,
-9.0754106003379));
#107315=CARTESIAN_POINT('Ctrl Pts',(-18.3678444459834,17.123040178458,-9.06626594373675));
#107316=CARTESIAN_POINT('Ctrl Pts',(-18.2604997145706,17.1447365925,-9.06037771571652));
#107317=CARTESIAN_POINT('Ctrl Pts',(-18.1111197350522,17.1871868071586,
-9.05192281864917));
#107318=CARTESIAN_POINT('Ctrl Pts',(-18.0673492586714,17.201180054876,-9.04941075452979));
#107319=CARTESIAN_POINT('Ctrl Pts',(-18.003068890374,17.2240612375143,-9.045626788143));
#107320=CARTESIAN_POINT('Ctrl Pts',(-17.9821876135874,17.2318678619025,
-9.04438233540202));
#107321=CARTESIAN_POINT('Ctrl Pts',(-17.9135808826573,17.2587594368671,
-9.04023136472835));
#107322=CARTESIAN_POINT('Ctrl Pts',(-17.866430766497,17.2792511943401,-9.03727797782522));
#107323=CARTESIAN_POINT('Ctrl Pts',(-17.8129718908838,17.3048367666467,
-9.03376035406435));
#107324=CARTESIAN_POINT('Ctrl Pts',(-17.8058857238463,17.3082769681307,
-9.03329057397738));
#107325=CARTESIAN_POINT('Ctrl Pts',(-17.7946183282661,17.3138249951052,
-9.03253773336924));
#107326=CARTESIAN_POINT('Ctrl Pts',(-17.7904245305458,17.3159073223538,
-9.03225621795564));
#107327=CARTESIAN_POINT('Ctrl Pts',(-17.7830248264716,17.319612115509,-9.03175713356468));
#107328=CARTESIAN_POINT('Ctrl Pts',(-17.7798160995386,17.3212288513649,
-9.03153992450984));
#107329=CARTESIAN_POINT('Ctrl Pts',(-17.773041017024,17.324664171307,-9.03107959958146));
#107330=CARTESIAN_POINT('Ctrl Pts',(-17.769475755008,17.3264846761617,-9.03083636882649));
#107331=CARTESIAN_POINT('Ctrl Pts',(-17.759905226379,17.3314058816175,-9.03018081430051));
#107332=CARTESIAN_POINT('Ctrl Pts',(-17.7539096684074,17.3345252154846,
-9.02976734263338));
#107333=CARTESIAN_POINT('Ctrl Pts',(-17.724704962782,17.3498978165027,-9.02774000926112));
#107334=CARTESIAN_POINT('Ctrl Pts',(-17.7017112284554,17.3625526636707,
-9.02610270299731));
#107335=CARTESIAN_POINT('Ctrl Pts',(-17.6365230815829,17.4000252945157,
-9.02135462931007));
#107336=CARTESIAN_POINT('Ctrl Pts',(-17.5949477248333,17.4258825662844,
-9.01819628861483));
#107337=CARTESIAN_POINT('Ctrl Pts',(-17.4740574198348,17.5070121729297,
-9.00869584960283));
#107338=CARTESIAN_POINT('Ctrl Pts',(-17.3975893964271,17.5663005383351,
-9.00226695202653));
#107339=CARTESIAN_POINT('Ctrl Pts',(-17.2201677022836,17.7244313396584,
-8.98663144364373));
#107340=CARTESIAN_POINT('Ctrl Pts',(-17.1245173602814,17.8285552124252,
-8.97756391735156));
#107341=CARTESIAN_POINT('Ctrl Pts',(-17.0313565068578,17.9528672074506,
-8.96807857658354));
#107342=CARTESIAN_POINT('Ctrl Pts',(-17.0229070615236,17.9643829938517,
-8.96721102492995));
#107343=CARTESIAN_POINT('Ctrl Pts',(-17.0096436064228,17.9828487581173,
-8.96583725915923));
#107344=CARTESIAN_POINT('Ctrl Pts',(-17.0047536795196,17.9897434293522,
-8.96532812057188));
#107345=CARTESIAN_POINT('Ctrl Pts',(-16.9962016695629,18.0019558950485,
-8.96443288433582));
#107346=CARTESIAN_POINT('Ctrl Pts',(-16.9925223996357,18.0072614678221,
-8.96404613121473));
#107347=CARTESIAN_POINT('Ctrl Pts',(-16.9849620336064,18.0182708662349,
-8.96324803527219));
#107348=CARTESIAN_POINT('Ctrl Pts',(-16.9810844276534,18.0239770042768,
-8.96283682817445));
#107349=CARTESIAN_POINT('Ctrl Pts',(-16.9712013946726,18.0386745400552,
-8.96178385308575));
#107350=CARTESIAN_POINT('Ctrl Pts',(-16.9652367856299,18.0476932455129,
-8.96114362792164));
#107351=CARTESIAN_POINT('Ctrl Pts',(-16.9406198414327,18.0855420216681,
-8.95848085909162));
#107352=CARTESIAN_POINT('Ctrl Pts',(-16.9226006072697,18.1147789952353,
-8.95648189167311));
#107353=CARTESIAN_POINT('Ctrl Pts',(-16.8775016624623,18.1921048423589,
-8.95133200470345));
#107354=CARTESIAN_POINT('Ctrl Pts',(-16.8515762352676,18.2408377264412,
-8.94822059091668));
#107355=CARTESIAN_POINT('Ctrl Pts',(-16.7800137119302,18.389053436859,-8.93906945594282));
#107356=CARTESIAN_POINT('Ctrl Pts',(-16.7401520658335,18.4911181633063,
-8.93317844158517));
#107357=CARTESIAN_POINT('Ctrl Pts',(-16.6935664703212,18.6445100468694,
-8.92445019024973));
#107358=CARTESIAN_POINT('Ctrl Pts',(-16.6805367772416,18.6937299550284,
-8.92166567303186));
#107359=CARTESIAN_POINT('Ctrl Pts',(-16.6658192487566,18.7587115674047,
-8.917958809007));
#107360=CARTESIAN_POINT('Ctrl Pts',(-16.6625156761329,18.7740914001609,
-8.91707922224968));
#107361=CARTESIAN_POINT('Ctrl Pts',(-16.6488821027157,18.8411966359645,
-8.91322628594086));
#107362=CARTESIAN_POINT('Ctrl Pts',(-16.6403167641891,18.8932568753744,
-8.91019833674597));
#107363=CARTESIAN_POINT('Ctrl Pts',(-16.6326149766072,18.9542013648139,
-8.90655274116614));
#107364=CARTESIAN_POINT('Ctrl Pts',(-16.6315783129375,18.9628315098977,
-8.90603415520237));
#107365=CARTESIAN_POINT('Ctrl Pts',(-16.6300882631837,18.9759160808096,
-8.90524402113409));
#107366=CARTESIAN_POINT('Ctrl Pts',(-16.6295957989255,18.9803660843912,
-8.90497462085352));
#107367=CARTESIAN_POINT('Ctrl Pts',(-16.6287367224929,18.9883607592236,
-8.90448935550362));
#107368=CARTESIAN_POINT('Ctrl Pts',(-16.6283649411118,18.9919048206068,
-8.90427378448645));
#107369=CARTESIAN_POINT('Ctrl Pts',(-16.6275760431054,18.99961262089,-8.90380395693945));
#107370=CARTESIAN_POINT('Ctrl Pts',(-16.6271623281248,19.0037766087173,
-8.90354951746798));
#107371=CARTESIAN_POINT('Ctrl Pts',(-16.6260337072066,19.0154888838935,
-8.90283213906703));
#107372=CARTESIAN_POINT('Ctrl Pts',(-16.6253470121312,19.0230397360276,
-8.90236766099264));
#107373=CARTESIAN_POINT('Ctrl Pts',(-16.6214621588587,19.0684612666666,
-8.89956235031418));
#107374=CARTESIAN_POINT('Ctrl Pts',(-16.6192439489004,19.1064062636917,
-8.89717176310606));
#107375=CARTESIAN_POINT('Ctrl Pts',(-16.6152879466501,19.2320690459693,
-8.88914355983114));
#107376=CARTESIAN_POINT('Ctrl Pts',(-16.6179805449662,19.3198319840568,
-8.88336095675132));
#107377=CARTESIAN_POINT('Ctrl Pts',(-16.6422709203489,19.5808395850592,
-8.86604060451694));
#107378=CARTESIAN_POINT('Ctrl Pts',(-16.6798383616897,19.7518834242279,
-8.85459345794534));
#107379=CARTESIAN_POINT('Ctrl Pts',(-16.7456645980709,19.9381474156945,
-8.84243278823315));
#107380=CARTESIAN_POINT('Ctrl Pts',(-16.753705457454,19.9597687396893,-8.84102462834996));
#107381=CARTESIAN_POINT('Ctrl Pts',(-16.7655760968599,19.990158328726,-8.83904959752108));
#107382=CARTESIAN_POINT('Ctrl Pts',(-16.7691141662067,19.9990380882435,
-8.83847300682397));
#107383=CARTESIAN_POINT('Ctrl Pts',(-16.7749591998491,20.0134236865229,
-8.8375396492632));
#107384=CARTESIAN_POINT('Ctrl Pts',(-16.7772294943446,20.0189441928006,
-8.83718165019393));
#107385=CARTESIAN_POINT('Ctrl Pts',(-16.7820294167997,20.0304768979414,
-8.83643411163075));
#107386=CARTESIAN_POINT('Ctrl Pts',(-16.7845635463761,20.036487164461,-8.83604472949029));
#107387=CARTESIAN_POINT('Ctrl Pts',(-16.790656012413,20.0507523135977,-8.83512096642121));
#107388=CARTESIAN_POINT('Ctrl Pts',(-16.794239246073,20.058996476174,-8.83458743957967));
#107389=CARTESIAN_POINT('Ctrl Pts',(-16.806477042741,20.0866692351083,-8.83279751320582));
#107390=CARTESIAN_POINT('Ctrl Pts',(-16.815372026829,20.105990563738,-8.83154934939907));
#107391=CARTESIAN_POINT('Ctrl Pts',(-16.8912560756496,20.2644900374526,
-8.82131541919827));
#107392=CARTESIAN_POINT('Ctrl Pts',(-16.9730020083597,20.3960906972459,
-8.81289814565379));
#107393=CARTESIAN_POINT('Ctrl Pts',(-17.1527684397966,20.6252498445392,
-8.79708144219461));
#107394=CARTESIAN_POINT('Ctrl Pts',(-17.2474050757665,20.7244136970755,
-8.78969581197635));
#107395=CARTESIAN_POINT('Ctrl Pts',(-17.3627251487734,20.823928150583,-8.78076356911416));
#107396=CARTESIAN_POINT('Ctrl Pts',(-17.3746370788697,20.8339800840723,
-8.77984146474872));
#107397=CARTESIAN_POINT('Ctrl Pts',(-17.3911125734593,20.8475743811132,
-8.77856511293135));
#107398=CARTESIAN_POINT('Ctrl Pts',(-17.3955815886669,20.8512312336081,
-8.77821880218579));
#107399=CARTESIAN_POINT('Ctrl Pts',(-17.402711805465,20.857017119495,-8.7776660146463));
#107400=CARTESIAN_POINT('Ctrl Pts',(-17.4053633214568,20.8591581206392,
-8.77746039342052));
#107401=CARTESIAN_POINT('Ctrl Pts',(-17.410854403414,20.8635701046648,-8.77703442534781));
#107402=CARTESIAN_POINT('Ctrl Pts',(-17.4136946459747,20.8658401711196,
-8.77681401328082));
#107403=CARTESIAN_POINT('Ctrl Pts',(-17.4204832662322,20.8712373803497,
-8.77628702455514));
#107404=CARTESIAN_POINT('Ctrl Pts',(-17.4244369713162,20.8743577611866,
-8.77597997029093));
#107405=CARTESIAN_POINT('Ctrl Pts',(-17.4378411345816,20.884859309836,-8.77493862502507));
#107406=CARTESIAN_POINT('Ctrl Pts',(-17.4473429581101,20.8921741238841,
-8.77419986816113));
#107407=CARTESIAN_POINT('Ctrl Pts',(-17.5586199792945,20.9763428973501,
-8.76554655148382));
#107408=CARTESIAN_POINT('Ctrl Pts',(-17.667067384525,21.043921653715,-8.75711299323475));
#107409=CARTESIAN_POINT('Ctrl Pts',(-17.9283045479755,21.1756341474197,
-8.73777924048841));
#107410=CARTESIAN_POINT('Ctrl Pts',(-18.0838999539409,21.2324653363557,
-8.72698402934422));
#107411=CARTESIAN_POINT('Ctrl Pts',(-18.2675081867491,21.276098454808,-8.71536087180296));
#107412=CARTESIAN_POINT('Ctrl Pts',(-18.2905648925023,21.2811718808147,
-8.71391924262907));
#107413=CARTESIAN_POINT('Ctrl Pts',(-18.323158379011,21.2877742407969,-8.71190578414224));
#107414=CARTESIAN_POINT('Ctrl Pts',(-18.3326274726973,21.2896250705507,
-8.71132371824018));
#107415=CARTESIAN_POINT('Ctrl Pts',(-18.3479909601404,21.2925191198023,
-8.71038390884797));
#107416=CARTESIAN_POINT('Ctrl Pts',(-18.3538776263852,21.2936021720859,
-8.71002489936757));
#107417=CARTESIAN_POINT('Ctrl Pts',(-18.3661753534045,21.2958108778802,
-8.70927713734061));
#107418=CARTESIAN_POINT('Ctrl Pts',(-18.3725871795826,21.2969319600285,
-8.70888853388355));
#107419=CARTESIAN_POINT('Ctrl Pts',(-18.3877912319547,21.2995181196459,
-8.70797000841313));
#107420=CARTESIAN_POINT('Ctrl Pts',(-18.3965877860205,21.3009572839462,
-8.70744091433629));
#107421=CARTESIAN_POINT('Ctrl Pts',(-18.4253807082772,21.3054814378798,
-8.70571651322996));
#107422=CARTESIAN_POINT('Ctrl Pts',(-18.4454126279572,21.3083353883952,
-8.70452851777621));
#107423=CARTESIAN_POINT('Ctrl Pts',(-18.4930782464337,21.3144304510945,
-8.70172751204178));
#107424=CARTESIAN_POINT('Ctrl Pts',(-18.520741291133,21.317414911011,-8.7001224606839));
#107425=CARTESIAN_POINT('Ctrl Pts',(-18.7171632174364,21.3346967664227,
-8.68885184275668));
#107426=CARTESIAN_POINT('Ctrl Pts',(-18.8870366382803,21.3292431036846,
-8.67982469425932));
#107427=CARTESIAN_POINT('Ctrl Pts',(-19.1572083200178,21.2878703031383,
-8.66488782810029));
#107428=CARTESIAN_POINT('Ctrl Pts',(-19.2586531281362,21.2645892464582,
-8.65912345852071));
#107429=CARTESIAN_POINT('Ctrl Pts',(-19.3672203720451,21.231102674287,-8.65239239498147));
#107430=CARTESIAN_POINT('Ctrl Pts',(-19.3764579479185,21.2281838367725,
-8.65181508283472));
#107431=CARTESIAN_POINT('Ctrl Pts',(-19.3900688511936,21.223780164267,-8.65095721441388));
#107432=CARTESIAN_POINT('Ctrl Pts',(-19.3944580257278,21.2223442078616,
-8.65067945663196));
#107433=CARTESIAN_POINT('Ctrl Pts',(-19.402237097736,21.2197710088452,-8.65018513623201));
#107434=CARTESIAN_POINT('Ctrl Pts',(-19.4056288494964,21.2186395276747,
-8.64996891512292));
#107435=CARTESIAN_POINT('Ctrl Pts',(-19.4128905138738,21.2161965903029,
-8.64950448804922));
#107436=CARTESIAN_POINT('Ctrl Pts',(-19.4167594426001,21.2148825410882,
-8.64925613549996));
#107437=CARTESIAN_POINT('Ctrl Pts',(-19.427371073762,21.2112440904193,-8.64857250172216));
#107438=CARTESIAN_POINT('Ctrl Pts',(-19.4341057996568,21.2088968274504,
-8.64813590107006));
#107439=CARTESIAN_POINT('Ctrl Pts',(-19.469522545189,21.1963519181368,-8.64582597643536));
#107440=CARTESIAN_POINT('Ctrl Pts',(-19.4979924242387,21.1855710942037,
-8.64392094984173));
#107441=CARTESIAN_POINT('Ctrl Pts',(-19.6765791192122,21.113504567797,-8.63170751631969));
#107442=CARTESIAN_POINT('Ctrl Pts',(-19.819466720913,21.0357575906665,-8.62079152232837));
#107443=CARTESIAN_POINT('Ctrl Pts',(-20.0499071872592,20.8736437336749,
-8.60236926501126));
#107444=CARTESIAN_POINT('Ctrl Pts',(-20.1417396485142,20.7966460337832,
-8.59474165427677));
#107445=CARTESIAN_POINT('Ctrl Pts',(-20.237728804307,20.7012132347215,-8.58647646815566));
#107446=CARTESIAN_POINT('Ctrl Pts',(-20.2487462297809,20.690013077051,-8.58552266149275));
#107447=CARTESIAN_POINT('Ctrl Pts',(-20.2652268072771,20.6728818162581,
-8.58408773358543));
#107448=CARTESIAN_POINT('Ctrl Pts',(-20.270782249834,20.6670406242377,-8.58360259570072));
#107449=CARTESIAN_POINT('Ctrl Pts',(-20.2806777383336,20.6565164254353,
-8.5827358061962));
#107450=CARTESIAN_POINT('Ctrl Pts',(-20.285030195311,20.6518452717336,-8.58235362189488));
#107451=CARTESIAN_POINT('Ctrl Pts',(-20.2942209544187,20.6418916398686,
-8.58154456269921));
#107452=CARTESIAN_POINT('Ctrl Pts',(-20.2990537199674,20.6366041411294,
-8.58111792659856));
#107453=CARTESIAN_POINT('Ctrl Pts',(-20.3088371056724,20.6257904914001,
-8.58025171602067));
#107454=CARTESIAN_POINT('Ctrl Pts',(-20.3137857015481,20.6202626381434,
-8.57981222978447));
#107455=CARTESIAN_POINT('Ctrl Pts',(-20.335574356308,20.5956645210763,-8.57787103507855));
#107456=CARTESIAN_POINT('Ctrl Pts',(-20.3520993621153,20.5763171027709,
-8.57638243280682));
#107457=CARTESIAN_POINT('Ctrl Pts',(-20.4222714019905,20.4910958303987,
-8.56998131244689));
#107458=CARTESIAN_POINT('Ctrl Pts',(-20.4722775266332,20.4223212234805,
-8.56521408864848));
#107459=CARTESIAN_POINT('Ctrl Pts',(-20.5551898596844,20.2925375571772,
-8.5567264422167));
#107460=CARTESIAN_POINT('Ctrl Pts',(-20.5894925766467,20.2325692067203,
-8.55298131127313));
#107461=CARTESIAN_POINT('Ctrl Pts',(-20.6801422932605,20.054410133297,-8.54212544850229));
#107462=CARTESIAN_POINT('Ctrl Pts',(-20.7285327012151,19.932554217635,-8.53503491361746));
#107463=CARTESIAN_POINT('Ctrl Pts',(-20.769799326511,19.7919117142914,-8.52644208282981));
#107464=CARTESIAN_POINT('Ctrl Pts',(-20.7740668387401,19.7767425016399,
-8.52550998776409));
#107465=CARTESIAN_POINT('Ctrl Pts',(-20.7796729208635,19.7559265525559,
-8.52422191267096));
#107466=CARTESIAN_POINT('Ctrl Pts',(-20.7811583219922,19.7503194319977,
-8.52387405870588));
#107467=CARTESIAN_POINT('Ctrl Pts',(-20.7834811070228,19.7414034703812,
-8.52331941663725));
#107468=CARTESIAN_POINT('Ctrl Pts',(-20.7843335776056,19.7380985387925,
-8.52311349442651));
#107469=CARTESIAN_POINT('Ctrl Pts',(-20.7860768721652,19.7312717633836,
-8.52268742707242));
#107470=CARTESIAN_POINT('Ctrl Pts',(-20.7869666217107,19.7277496941576,
-8.52246721905637));
#107471=CARTESIAN_POINT('Ctrl Pts',(-20.7890638354669,19.7193569746191,
-8.52194157923698));
#107472=CARTESIAN_POINT('Ctrl Pts',(-20.7902630516338,19.7144843024198,
-8.52163567625239));
#107473=CARTESIAN_POINT('Ctrl Pts',(-20.7927674041357,19.7041503872006,
-8.52098545266681));
#107474=CARTESIAN_POINT('Ctrl Pts',(-20.7940681571072,19.6986881331292,
-8.52064089399558));
#107475=CARTESIAN_POINT('Ctrl Pts',(-20.7975804762354,19.683674039106,-8.51969155133116));
#107476=CARTESIAN_POINT('Ctrl Pts',(-20.7997474098406,19.6741120380835,
-8.51908444441543));
#107477=CARTESIAN_POINT('Ctrl Pts',(-20.8343835382445,19.5161922354477,
-8.50902056227148));
#107478=CARTESIAN_POINT('Ctrl Pts',(-20.8508585305448,19.3647964103147,
-8.49886440074919));
#107479=CARTESIAN_POINT('Ctrl Pts',(-20.8509990928577,19.2129598060055,
-8.48885791885903));
#107480=CARTESIAN_POINT('Ctrl Pts',(-20.8509991049198,19.2129467328109,
-8.4890562790225));
#107481=CARTESIAN_POINT('Ctrl Pts',(-20.8510652694519,19.1409952794406,
-8.48473008583438));
#107482=CARTESIAN_POINT('Ctrl Pts',(-20.8474590099797,19.0689489014342,
-8.48040389264625));
#107483=CARTESIAN_POINT('Ctrl Pts',(-20.8401779985051,18.9972168420736,
-8.47607769945812));
#107484=CARTESIAN_POINT('Ctrl Pts',(-20.8329019842487,18.9255340149865,
-8.47175447549083));
#107485=CARTESIAN_POINT('Ctrl Pts',(-20.8219562717615,18.8541655692599,
-8.46743125152355));
#107486=CARTESIAN_POINT('Ctrl Pts',(-20.8073905458164,18.7835182524142,
-8.46310802755626));
#107487=CARTESIAN_POINT('Ctrl Pts',(-20.7928276075188,18.712884456337,-8.45878563098502));
#107488=CARTESIAN_POINT('Ctrl Pts',(-20.7746461242502,18.6429720006697,
-8.45446323441377));
#107489=CARTESIAN_POINT('Ctrl Pts',(-20.7529470567908,18.5741783751506,
-8.45014083784253));
#107490=CARTESIAN_POINT('Ctrl Pts',(-20.7434888020108,18.5441924027759,
-8.44825677862629));
#107491=CARTESIAN_POINT('Ctrl Pts',(-20.7333628777044,18.5144188420078,
-8.44637271941005));
#107492=CARTESIAN_POINT('Ctrl Pts',(-20.7225806137986,18.4848897174502,
-8.44448866019381));
#107493=CARTESIAN_POINT('Origin',(-18.734,19.211,0.));
#107494=CARTESIAN_POINT('',(-20.7249099383763,18.4840591618169,-7.64456003119576));
#107495=CARTESIAN_POINT('',(-20.72258060468,18.4848896924774,-7.86510589144174));
#107496=CARTESIAN_POINT('',(-20.7225806137986,18.4848897174502,0.));
#107497=CARTESIAN_POINT('Ctrl Pts',(-20.72258060468,18.4848896924774,-7.86510589144174));
#107498=CARTESIAN_POINT('Ctrl Pts',(-20.7375769998214,18.525959954405,-7.86752226702014));
#107499=CARTESIAN_POINT('Ctrl Pts',(-20.7513004634184,18.5674931846836,
-7.86996742714882));
#107500=CARTESIAN_POINT('Ctrl Pts',(-20.774507307338,18.6457943285263,-7.87462970750348));
#107501=CARTESIAN_POINT('Ctrl Pts',(-20.7843050079669,18.6824392235647,
-7.87683265697601));
#107502=CARTESIAN_POINT('Ctrl Pts',(-20.7948724777023,18.7266952903225,
-7.87953976353451));
#107503=CARTESIAN_POINT('Ctrl Pts',(-20.7965927836893,18.7340750311575,
-7.8799927178299));
#107504=CARTESIAN_POINT('Ctrl Pts',(-20.7992012895929,18.7455430893457,
-7.88069921951285));
#107505=CARTESIAN_POINT('Ctrl Pts',(-20.8001170723227,18.749625157845,-7.88095121241774));
#107506=CARTESIAN_POINT('Ctrl Pts',(-20.8017905253459,18.7571894193622,
-7.88141916099004));
#107507=CARTESIAN_POINT('Ctrl Pts',(-20.8025515052419,18.7606708210759,
-7.88163492431416));
#107508=CARTESIAN_POINT('Ctrl Pts',(-20.8042489792987,18.7685316732664,
-7.88212299081495));
#107509=CARTESIAN_POINT('Ctrl Pts',(-20.8051803635868,18.77291215825,-7.88239558046764));
#107510=CARTESIAN_POINT('Ctrl Pts',(-20.8078797703266,18.7858090387155,
-7.88319986520688));
#107511=CARTESIAN_POINT('Ctrl Pts',(-20.8096091888307,18.7943332931264,
-7.88373368416764));
#107512=CARTESIAN_POINT('Ctrl Pts',(-20.8214936949608,18.8548223153753,
-7.88753628113026));
#107513=CARTESIAN_POINT('Ctrl Pts',(-20.8297477735186,18.9071369988817,
-7.89090069994371));
#107514=CARTESIAN_POINT('Ctrl Pts',(-20.8378088389374,18.9745650814762,
-7.89528838354835));
#107515=CARTESIAN_POINT('Ctrl Pts',(-20.8394281152034,18.9894474376463,
-7.8962600198513));
#107516=CARTESIAN_POINT('Ctrl Pts',(-20.8475637141893,19.0723916912477,
-7.90168909965173));
#107517=CARTESIAN_POINT('Ctrl Pts',(-20.8509374102031,19.1407195013328,
-7.90621171713557));
#107518=CARTESIAN_POINT('Ctrl Pts',(-20.8511442880123,19.3698585923934,
-7.92135267539541));
#107519=CARTESIAN_POINT('Ctrl Pts',(-20.832975226392,19.5301508319367,-7.9318506755467));
#107520=CARTESIAN_POINT('Ctrl Pts',(-20.7914795966215,19.7100311498939,
-7.94322217798434));
#107521=CARTESIAN_POINT('Ctrl Pts',(-20.7857446856256,19.7331093721006,
-7.94467445754255));
#107522=CARTESIAN_POINT('Ctrl Pts',(-20.777130402795,19.7654373703139,-7.94670015645179));
#107523=CARTESIAN_POINT('Ctrl Pts',(-20.7745746989045,19.7747708253192,
-7.94728397926491));
#107524=CARTESIAN_POINT('Ctrl Pts',(-20.7703333351987,19.7898535533649,
-7.94822586104407));
#107525=CARTESIAN_POINT('Ctrl Pts',(-20.7686871311676,19.7956136909892,
-7.9485851969033));
#107526=CARTESIAN_POINT('Ctrl Pts',(-20.7652024820852,19.8076136017481,
-7.94933304408305));
#107527=CARTESIAN_POINT('Ctrl Pts',(-20.7633596814752,19.813852052895,-7.94972140892112));
#107528=CARTESIAN_POINT('Ctrl Pts',(-20.7589304678799,19.8285958452658,
-7.95063830833244));
#107529=CARTESIAN_POINT('Ctrl Pts',(-20.7563191641273,19.8370936271149,
-7.9511660230735));
#107530=CARTESIAN_POINT('Ctrl Pts',(-20.7474528182278,19.8653124503228,
-7.95291610515229));
#107531=CARTESIAN_POINT('Ctrl Pts',(-20.7409620989911,19.8849586128504,
-7.95413073624497));
#107532=CARTESIAN_POINT('Ctrl Pts',(-20.704833847573,19.9891582238327,-7.96055729785824));
#107533=CARTESIAN_POINT('Ctrl Pts',(-20.6701375233483,20.0718660872074,
-7.96559780859476));
#107534=CARTESIAN_POINT('Ctrl Pts',(-20.5703572156766,20.2729144430854,
-7.97797943898009));
#107535=CARTESIAN_POINT('Ctrl Pts',(-20.4990149366166,20.3876861426273,
-7.98515788350393));
#107536=CARTESIAN_POINT('Ctrl Pts',(-20.370854188125,20.5557113840558,-7.99685014611318));
#107537=CARTESIAN_POINT('Ctrl Pts',(-20.3212057374879,20.6139667239307,
-8.00116972646293));
#107538=CARTESIAN_POINT('Ctrl Pts',(-20.2619779463709,20.6762858434198,
-8.00626509881932));
#107539=CARTESIAN_POINT('Ctrl Pts',(-20.2553888181487,20.683126103271,-8.00683122863796));
#107540=CARTESIAN_POINT('Ctrl Pts',(-20.2455537544683,20.6931994579397,
-8.0076755881059));
#107541=CARTESIAN_POINT('Ctrl Pts',(-20.2423428874341,20.6964668353033,
-8.00795114489806));
#107542=CARTESIAN_POINT('Ctrl Pts',(-20.2366096474223,20.7022632248489,
-8.00844304711825));
#107543=CARTESIAN_POINT('Ctrl Pts',(-20.2340914542446,20.7047963003654,
-8.00865906350769));
#107544=CARTESIAN_POINT('Ctrl Pts',(-20.2286618069518,20.7102304609905,
-8.00912476054446));
#107545=CARTESIAN_POINT('Ctrl Pts',(-20.225748354315,20.7131294015686,-8.00937459675336));
#107546=CARTESIAN_POINT('Ctrl Pts',(-20.2176786507927,20.7211122788836,
-8.01006641244211));
#107547=CARTESIAN_POINT('Ctrl Pts',(-20.212504785718,20.7261782168353,-8.01050976324142));
#107548=CARTESIAN_POINT('Ctrl Pts',(-20.1839451609985,20.753856521646,-8.01295540519318));
#107549=CARTESIAN_POINT('Ctrl Pts',(-20.1600679338781,20.7759527773244,
-8.01499402291496));
#107550=CARTESIAN_POINT('Ctrl Pts',(-20.0137580453866,20.9052203256788,
-8.0273998941035));
#107551=CARTESIAN_POINT('Ctrl Pts',(-19.8798138343924,20.9985328676181,
-8.03835715738868));
#107552=CARTESIAN_POINT('Ctrl Pts',(-19.6336216446591,21.1308996988453,
-8.05661524271468));
#107553=CARTESIAN_POINT('Ctrl Pts',(-19.526323430212,21.1776126576731,-8.06405608414213));
#107554=CARTESIAN_POINT('Ctrl Pts',(-19.4021738965136,21.2198396724125,
-8.07206314263055));
#107555=CARTESIAN_POINT('Ctrl Pts',(-19.3885991768308,21.2243040304063,
-8.07293111877289));
#107556=CARTESIAN_POINT('Ctrl Pts',(-19.366922360117,21.2311905268723,-8.07430542749688));
#107557=CARTESIAN_POINT('Ctrl Pts',(-19.3588493389351,21.233702100081,-8.07481468814729));
#107558=CARTESIAN_POINT('Ctrl Pts',(-19.3445847674101,21.2380463564072,
-8.07571006634878));
#107559=CARTESIAN_POINT('Ctrl Pts',(-19.3383995131545,21.2398991890058,
-8.07609684002707));
#107560=CARTESIAN_POINT('Ctrl Pts',(-19.3255888911096,21.2436729119852,
-8.07689490880411));
#107561=CARTESIAN_POINT('Ctrl Pts',(-19.3189624102432,21.2455897777038,
-8.07730606852224));
#107562=CARTESIAN_POINT('Ctrl Pts',(-19.3019291031211,21.250426968723,-8.07835877822346));
#107563=CARTESIAN_POINT('Ctrl Pts',(-19.2915089853879,21.2533000672519,
-8.07899878690564));
#107564=CARTESIAN_POINT('Ctrl Pts',(-19.2479272749469,21.2649582753908,
-8.08165945088431));
#107565=CARTESIAN_POINT('Ctrl Pts',(-19.2145755250427,21.2730167803175,
-8.08365657747511));
#107566=CARTESIAN_POINT('Ctrl Pts',(-19.127178851698,21.2918978704387,-8.0888006502615));
#107567=CARTESIAN_POINT('Ctrl Pts',(-19.0728802726973,21.3014273158352,
-8.09190820756228));
#107568=CARTESIAN_POINT('Ctrl Pts',(-18.9099124879943,21.3235104553182,
-8.10105261517301));
#107569=CARTESIAN_POINT('Ctrl Pts',(-18.800578682725,21.3297764841732,-8.10694073608899));
#107570=CARTESIAN_POINT('Ctrl Pts',(-18.6455302129237,21.3266448901245,
-8.11538394594907));
#107571=CARTESIAN_POINT('Ctrl Pts',(-18.5998530274913,21.3242402979392,
-8.11788435240091));
#107572=CARTESIAN_POINT('Ctrl Pts',(-18.5315822066191,21.3184238939376,
-8.121683725345));
#107573=CARTESIAN_POINT('Ctrl Pts',(-18.5089067037586,21.3161226539018,
-8.12295602795445));
#107574=CARTESIAN_POINT('Ctrl Pts',(-18.4852456492105,21.3133347363886,
-8.12429840239874));
#107575=CARTESIAN_POINT('Ctrl Pts',(-18.4842180238449,21.3132128900864,
-8.12435673239391));
#107576=CARTESIAN_POINT('Ctrl Pts',(-18.4649310487697,21.3109116774326,
-8.12545205327248));
#107577=CARTESIAN_POINT('Ctrl Pts',(-18.4467012450516,21.3084953023214,
-8.12649667173703));
#107578=CARTESIAN_POINT('Ctrl Pts',(-18.3954025259099,21.3010143246308,
-8.12946827570211));
#107579=CARTESIAN_POINT('Ctrl Pts',(-18.3624204620127,21.2954031501119,
-8.13141652591858));
#107580=CARTESIAN_POINT('Ctrl Pts',(-18.3227886349005,21.287690199803,-8.13381814793919));
#107581=CARTESIAN_POINT('Ctrl Pts',(-18.3159965927483,21.2863337373251,
-8.13423189616548));
#107582=CARTESIAN_POINT('Ctrl Pts',(-18.304855544583,21.2840518098103,-8.13491430553586));
#107583=CARTESIAN_POINT('Ctrl Pts',(-18.3005025208339,21.2831459177625,
-8.13518187439928));
#107584=CARTESIAN_POINT('Ctrl Pts',(-18.2926676551979,21.2814896637643,
-8.13566520646445));
#107585=CARTESIAN_POINT('Ctrl Pts',(-18.2891848291454,21.2807442232738,
-8.13588068607341));
#107586=CARTESIAN_POINT('Ctrl Pts',(-18.2815902696258,21.2790986804165,
-8.13635192841704));
#107587=CARTESIAN_POINT('Ctrl Pts',(-18.2774793851383,21.2781951150224,
-8.13660788297164));
#107588=CARTESIAN_POINT('Ctrl Pts',(-18.2658602580979,21.2756049018854,
-8.13733374098581));
#107589=CARTESIAN_POINT('Ctrl Pts',(-18.2583585692817,21.2738895860056,
-8.13780524118772));
#107590=CARTESIAN_POINT('Ctrl Pts',(-18.2118556405573,21.2629892140187,
-8.14074514235477));
#107591=CARTESIAN_POINT('Ctrl Pts',(-18.1731150447937,21.2527399571674,
-8.14326888438847));
#107592=CARTESIAN_POINT('Ctrl Pts',(-17.9685915573466,21.1923712004236,
-8.15690935316512));
#107593=CARTESIAN_POINT('Ctrl Pts',(-17.8091349993931,21.1231483572091,
-8.16860034017371));
#107594=CARTESIAN_POINT('Ctrl Pts',(-17.5748943676725,20.9852296621986,
-8.18622209495736));
#107595=CARTESIAN_POINT('Ctrl Pts',(-17.4934949350718,20.929304034047,-8.19245943349971));
#107596=CARTESIAN_POINT('Ctrl Pts',(-17.4053697450291,20.8592187500021,
-8.19933147006765));
#107597=CARTESIAN_POINT('Ctrl Pts',(-17.3945430211814,20.8504323465081,
-8.20017811802275));
#107598=CARTESIAN_POINT('Ctrl Pts',(-17.3773696158958,20.8362116120886,
-8.20152511587853));
#107599=CARTESIAN_POINT('Ctrl Pts',(-17.3709670679166,20.8308456754649,
-8.20202821552975));
#107600=CARTESIAN_POINT('Ctrl Pts',(-17.3596847241826,20.8212757540045,
-8.20291645183421));
#107601=CARTESIAN_POINT('Ctrl Pts',(-17.3547920679314,20.8170871591606,
-8.20330221166024));
#107602=CARTESIAN_POINT('Ctrl Pts',(-17.344666695465,20.8083384559043,-8.20410177236088));
#107603=CARTESIAN_POINT('Ctrl Pts',(-17.3394371310998,20.8037748052531,
-8.20451542011653));
#107604=CARTESIAN_POINT('Ctrl Pts',(-17.3259758392404,20.7919105034922,
-8.20558203771492));
#107605=CARTESIAN_POINT('Ctrl Pts',(-17.3177783470846,20.7845711912914,
-8.20623338557506));
#107606=CARTESIAN_POINT('Ctrl Pts',(-17.2829809838188,20.7529245069529,
-8.20900657420588));
#107607=CARTESIAN_POINT('Ctrl Pts',(-17.2569458891753,20.7280032138624,
-8.21110227037802));
#107608=CARTESIAN_POINT('Ctrl Pts',(-17.1900041520504,20.6605671555438,
-8.21656087570482));
#107609=CARTESIAN_POINT('Ctrl Pts',(-17.1502155649188,20.6169856848495,
-8.21987777033214));
#107610=CARTESIAN_POINT('Ctrl Pts',(-17.0040346104367,20.4427773459455,
-8.23248460572176));
#107611=CARTESIAN_POINT('Ctrl Pts',(-16.9115655999521,20.3013123221957,
-8.24134744939338));
#107612=CARTESIAN_POINT('Ctrl Pts',(-16.8126538433843,20.1015551754427,
-8.25387130412168));
#107613=CARTESIAN_POINT('Ctrl Pts',(-16.7903660746532,20.0518006054982,
-8.25699617925251));
#107614=CARTESIAN_POINT('Ctrl Pts',(-16.7667528499304,19.9931153814201,
-8.26074974563898));
#107615=CARTESIAN_POINT('Ctrl Pts',(-16.7635317152814,19.9849641801932,
-8.26127259550564));
#107616=CARTESIAN_POINT('Ctrl Pts',(-16.758736153102,19.9726048321004,-8.26206796025164));
#107617=CARTESIAN_POINT('Ctrl Pts',(-16.7571243087456,19.9684111734145,
-8.26233828450779));
#107618=CARTESIAN_POINT('Ctrl Pts',(-16.7542575786825,19.9608810917377,
-8.2628245328397));
#107619=CARTESIAN_POINT('Ctrl Pts',(-16.7529977601694,19.9575466040421,
-8.26304015759751));
#107620=CARTESIAN_POINT('Ctrl Pts',(-16.7502814963103,19.9503019062624,
-8.26350930585135));
#107621=CARTESIAN_POINT('Ctrl Pts',(-16.7488282072439,19.9463906193554,
-8.26376300794614));
#107622=CARTESIAN_POINT('Ctrl Pts',(-16.7447856904949,19.9354115466325,
-8.26447627188808));
#107623=CARTESIAN_POINT('Ctrl Pts',(-16.7422226112388,19.9283342928819,
-8.26493734528075));
#107624=CARTESIAN_POINT('Ctrl Pts',(-16.7272663571117,19.8863384269095,
-8.26768033005309));
#107625=CARTESIAN_POINT('Ctrl Pts',(-16.7157547264623,19.8511152498446,
-8.27000951277372));
#107626=CARTESIAN_POINT('Ctrl Pts',(-16.6811834284812,19.7351081467683,
-8.2777327908292));
#107627=CARTESIAN_POINT('Ctrl Pts',(-16.6620070545219,19.6532540281286,
-8.28326092204806));
#107628=CARTESIAN_POINT('Ctrl Pts',(-16.6172146324318,19.3933020309549,
-8.30068485188907));
#107629=CARTESIAN_POINT('Ctrl Pts',(-16.6093739541459,19.212914346402,-8.31250730874657));
#107630=CARTESIAN_POINT('Ctrl Pts',(-16.6263355366115,19.0111193713292,
-8.32496771542771));
#107631=CARTESIAN_POINT('Ctrl Pts',(-16.628594135158,18.9885860554209,-8.32634975246745));
#107632=CARTESIAN_POINT('Ctrl Pts',(-16.6323116477244,18.9566673223458,
-8.32829481314576));
#107633=CARTESIAN_POINT('Ctrl Pts',(-16.6334727635477,18.9472494084905,
-8.32886716127869));
#107634=CARTESIAN_POINT('Ctrl Pts',(-16.6354657538434,18.931932808445,-8.32979552680643));
#107635=CARTESIAN_POINT('Ctrl Pts',(-16.6362592617004,18.926029342388,-8.33015275042749));
#107636=CARTESIAN_POINT('Ctrl Pts',(-16.637975400756,18.9136574886664,-8.33090016173763));
#107637=CARTESIAN_POINT('Ctrl Pts',(-16.6389030839445,18.9071898561725,
-8.33129018551736));
#107638=CARTESIAN_POINT('Ctrl Pts',(-16.6411871212474,18.8917741236501,
-8.3322181930552));
#107639=CARTESIAN_POINT('Ctrl Pts',(-16.6425709488715,18.8828301757122,
-8.33275530147617));
#107640=CARTESIAN_POINT('Ctrl Pts',(-16.6474566566296,18.8525396779709,
-8.33457010559597));
#107641=CARTESIAN_POINT('Ctrl Pts',(-16.6512284129043,18.8312375831703,
-8.33583924520943));
#107642=CARTESIAN_POINT('Ctrl Pts',(-16.6737782541512,18.7143464355662,
-8.34276958649708));
#107643=CARTESIAN_POINT('Ctrl Pts',(-16.6988112710497,18.6200782894915,
-8.34822624713029));
#107644=CARTESIAN_POINT('Ctrl Pts',(-16.7737993194569,18.4001273663881,
-8.36099710371439));
#107645=CARTESIAN_POINT('Ctrl Pts',(-16.8294586823472,18.2768584786398,
-8.36817945517728));
#107646=CARTESIAN_POINT('Ctrl Pts',(-16.9041964086709,18.1462230184113,
-8.37655369570066));
#107647=CARTESIAN_POINT('Ctrl Pts',(-16.9120732801524,18.1328004758076,
-8.37742396767121));
#107648=CARTESIAN_POINT('Ctrl Pts',(-16.9472976337008,18.0742649059864,
-8.38126790410149));
#107649=CARTESIAN_POINT('Ctrl Pts',(-16.9761757042415,18.0301000143669,
-8.38429629711212));
#107650=CARTESIAN_POINT('Ctrl Pts',(-17.0116955329246,17.9799712101822,
-8.38794237774091));
#107651=CARTESIAN_POINT('Ctrl Pts',(-17.0167645801836,17.9729099121094,
-8.38846097419108));
#107652=CARTESIAN_POINT('Ctrl Pts',(-17.0245101761043,17.9622591991466,
-8.38925112112448));
#107653=CARTESIAN_POINT('Ctrl Pts',(-17.0271549333267,17.9586466300419,
-8.38952052367901));
#107654=CARTESIAN_POINT('Ctrl Pts',(-17.0319252814881,17.9521738198729,
-8.39000579143878));
#107655=CARTESIAN_POINT('Ctrl Pts',(-17.034046650294,17.9493105343655,-8.39022136257886));
#107656=CARTESIAN_POINT('Ctrl Pts',(-17.0386747861549,17.9430966404029,
-8.39069118841527));
#107657=CARTESIAN_POINT('Ctrl Pts',(-17.0411842283435,17.9397481474907,
-8.39094562604249));
#107658=CARTESIAN_POINT('Ctrl Pts',(-17.0482684602618,17.930353420368,-8.391662994154));
#107659=CARTESIAN_POINT('Ctrl Pts',(-17.0528657740952,17.9243243623628,
-8.39212746371394));
#107660=CARTESIAN_POINT('Ctrl Pts',(-17.0807007083364,17.8882246263595,
-8.39493261631368));
#107661=CARTESIAN_POINT('Ctrl Pts',(-17.1047106885366,17.8587614259561,
-8.39732304757671));
#107662=CARTESIAN_POINT('Ctrl Pts',(-17.1867203120694,17.7634819342764,
-8.40535046610004));
#107663=CARTESIAN_POINT('Ctrl Pts',(-17.2480149309345,17.7006260651215,
-8.41113241175424));
#107664=CARTESIAN_POINT('Ctrl Pts',(-17.4423290221763,17.5246716669501,
-8.42845312280769));
#107665=CARTESIAN_POINT('Ctrl Pts',(-17.5856342033998,17.4239923843037,
-8.43990132062418));
#107666=CARTESIAN_POINT('Ctrl Pts',(-17.7600534528488,17.331199728219,-8.45206277306558));
#107667=CARTESIAN_POINT('Ctrl Pts',(-17.7805913041882,17.3207003244761,
-8.45347080372527));
#107668=CARTESIAN_POINT('Ctrl Pts',(-17.8098777285528,17.3063272237661,
-8.45544568632157));
#107669=CARTESIAN_POINT('Ctrl Pts',(-17.8184866945323,17.3021742485732,
-8.45602225603627));
#107670=CARTESIAN_POINT('Ctrl Pts',(-17.8325171624734,17.2955226907508,
-8.45695558888772));
#107671=CARTESIAN_POINT('Ctrl Pts',(-17.8379215538362,17.2929885172246,
-8.45731358410124));
#107672=CARTESIAN_POINT('Ctrl Pts',(-17.8492538994521,17.2877330184803,
-8.45806112192241));
#107673=CARTESIAN_POINT('Ctrl Pts',(-17.8551838658238,17.2850161609144,
-8.45845050714453));
#107674=CARTESIAN_POINT('Ctrl Pts',(-17.8693159695207,17.2786202922171,
-8.45937429077242));
#107675=CARTESIAN_POINT('Ctrl Pts',(-17.877529212119,17.2749660124574,-8.45990783498824));
#107676=CARTESIAN_POINT('Ctrl Pts',(-17.9052540260613,17.2628414989501,
-8.46169788147031));
#107677=CARTESIAN_POINT('Ctrl Pts',(-17.9248703083587,17.2546128641837,
-8.46294614647993));
#107678=CARTESIAN_POINT('Ctrl Pts',(-18.0885207382021,17.1888473888761,
-8.47321745326249));
#107679=CARTESIAN_POINT('Ctrl Pts',(-18.2383561212894,17.1470016270937,
-8.48166671119933));
#107680=CARTESIAN_POINT('Ctrl Pts',(-18.5257346406427,17.0998780267568,
-8.49748117395406));
#107681=CARTESIAN_POINT('Ctrl Pts',(-18.6618271134729,17.0908605546421,
-8.50483302257926));
#107682=CARTESIAN_POINT('Ctrl Pts',(-18.8134283353893,17.0954329492276,
-8.51372669283649));
#107683=CARTESIAN_POINT('Ctrl Pts',(-18.8290293538823,17.0960763142369,
-8.51465042055911));
#107684=CARTESIAN_POINT('Ctrl Pts',(-18.8503921865413,17.0971941306936,
-8.51592867720537));
#107685=CARTESIAN_POINT('Ctrl Pts',(-18.8561617258545,17.0975197173487,
-8.51627523879971));
#107686=CARTESIAN_POINT('Ctrl Pts',(-18.865332399465,17.0980749135176,-8.51682832773566));
#107687=CARTESIAN_POINT('Ctrl Pts',(-18.8687344859943,17.0982891257582,
-8.51703399783409));
#107688=CARTESIAN_POINT('Ctrl Pts',(-18.8757637449014,17.0987487703053,
-8.51745998154834));
#107689=CARTESIAN_POINT('Ctrl Pts',(-18.8793907968412,17.0989953285727,
-8.51768036000098));
#107690=CARTESIAN_POINT('Ctrl Pts',(-18.888038373376,17.0996055513629,-8.51820712741096));
#107691=CARTESIAN_POINT('Ctrl Pts',(-18.8930582554253,17.0999777811714,
-8.51851399292017));
#107692=CARTESIAN_POINT('Ctrl Pts',(-18.9100140911606,17.1012958970198,
-8.51955404132159));
#107693=CARTESIAN_POINT('Ctrl Pts',(-18.9219430788029,17.1023251207571,
-8.52029167527382));
#107694=CARTESIAN_POINT('Ctrl Pts',(-19.058975194832,17.1153201314184,-8.52882833096445));
#107695=CARTESIAN_POINT('Ctrl Pts',(-19.1827700137946,17.138300833222,-8.53713204906159));
#107696=CARTESIAN_POINT('Ctrl Pts',(-19.4646935637701,17.2170865602461,
-8.55647671210745));
#107697=CARTESIAN_POINT('Ctrl Pts',(-19.619747527816,17.2809545129042,-8.56741235140886));
#107698=CARTESIAN_POINT('Ctrl Pts',(-19.7862055411517,17.3738543308215,
-8.57915174424997));
#107699=CARTESIAN_POINT('Ctrl Pts',(-19.8065247159106,17.3856420860227,
-8.58058612436764));
#107700=CARTESIAN_POINT('Ctrl Pts',(-19.834737149007,17.4026427321543,-8.58258038378754));
#107701=CARTESIAN_POINT('Ctrl Pts',(-19.8427974910587,17.4075737032734,
-8.58315046283729));
#107702=CARTESIAN_POINT('Ctrl Pts',(-19.8563859001443,17.4160120486852,
-8.58411214211518));
#107703=CARTESIAN_POINT('Ctrl Pts',(-19.8619311463022,17.4194913662208,
-8.58450476711414));
#107704=CARTESIAN_POINT('Ctrl Pts',(-19.8728926162624,17.426440116179,-8.58528127060543));
#107705=CARTESIAN_POINT('Ctrl Pts',(-19.8783093421466,17.4299086207597,
-8.5856651778542));
#107706=CARTESIAN_POINT('Ctrl Pts',(-19.8891596012715,17.43692632237,-8.58643460602489));
#107707=CARTESIAN_POINT('Ctrl Pts',(-19.8945927894194,17.4404759259902,
-8.58682010627732));
#107708=CARTESIAN_POINT('Ctrl Pts',(-19.9138389949438,17.4531764930154,
-8.58818652430193));
#107709=CARTESIAN_POINT('Ctrl Pts',(-19.9275610394943,17.4624647261385,
-8.58916229315734));
#107710=CARTESIAN_POINT('Ctrl Pts',(-20.0449882486269,17.5439758706704,
-8.59752966848056));
#107711=CARTESIAN_POINT('Ctrl Pts',(-20.1421484798553,17.6251930698747,
-8.60454806203147));
#107712=CARTESIAN_POINT('Ctrl Pts',(-20.3274770907587,17.8106575464539,
-8.6188567048415));
#107713=CARTESIAN_POINT('Ctrl Pts',(-20.4139881948288,17.9157154158987,
-8.62609796880144));
#107714=CARTESIAN_POINT('Ctrl Pts',(-20.5158511784127,18.0669441804967,
-8.63641321351391));
#107715=CARTESIAN_POINT('Ctrl Pts',(-20.5405818680822,18.1064102163149,
-8.6390983240072));
#107716=CARTESIAN_POINT('Ctrl Pts',(-20.5678430828171,18.1532820306659,
-8.64231814207972));
#107717=CARTESIAN_POINT('Ctrl Pts',(-20.5716607533356,18.1599287813493,
-8.64277544070319));
#107718=CARTESIAN_POINT('Ctrl Pts',(-20.5777215519317,18.1706148857748,
-8.64351201608973));
#107719=CARTESIAN_POINT('Ctrl Pts',(-20.5799877389192,18.1746411751752,
-8.64378985066426));
#107720=CARTESIAN_POINT('Ctrl Pts',(-20.5839887627887,18.1818044752853,
-8.64428476126932));
#107721=CARTESIAN_POINT('Ctrl Pts',(-20.5857288325681,18.1849385101275,
-8.64450149778334));
#107722=CARTESIAN_POINT('Ctrl Pts',(-20.5894120814875,18.1916122852367,
-8.64496348701184));
#107723=CARTESIAN_POINT('Ctrl Pts',(-20.5913530655499,18.1951531146861,
-8.64520886806589));
#107724=CARTESIAN_POINT('Ctrl Pts',(-20.596590458459,18.2047725900186,-8.64587618405547));
#107725=CARTESIAN_POINT('Ctrl Pts',(-20.5998672000462,18.2108618069068,
-8.64629933750692));
#107726=CARTESIAN_POINT('Ctrl Pts',(-20.6163198486875,18.2417982766792,
-8.64845248001302));
#107727=CARTESIAN_POINT('Ctrl Pts',(-20.6290288278897,18.2668890126877,
-8.65020948010647));
#107728=CARTESIAN_POINT('Ctrl Pts',(-20.6647759863615,18.3410944524601,
-8.6554208437193));
#107729=CARTESIAN_POINT('Ctrl Pts',(-20.6864298666476,18.3908485600598,
-8.65893358048579));
#107730=CARTESIAN_POINT('Ctrl Pts',(-20.7117862945679,18.4558239130744,
-8.6634990956526));
#107731=CARTESIAN_POINT('Ctrl Pts',(-20.7172641108656,18.4703295411108,
-8.66451700717518));
#107732=CARTESIAN_POINT('Ctrl Pts',(-20.7225805936643,18.484889662309,-8.66553669489169));
#107733=CARTESIAN_POINT('',(-20.8507520319894,19.2105366956018,-7.68905625085211));
#107734=CARTESIAN_POINT('Ctrl Pts',(-20.7225806137986,18.4848897174502,
-8.44448866019381));
#107735=CARTESIAN_POINT('Ctrl Pts',(-20.6978226921706,18.417085798169,-8.44016253807091));
#107736=CARTESIAN_POINT('Ctrl Pts',(-20.6696011102778,18.350572196178,-8.435836415948));
#107737=CARTESIAN_POINT('Ctrl Pts',(-20.6380875635549,18.2857219064975,
-8.4315102938251));
#107738=CARTESIAN_POINT('Ctrl Pts',(-20.6065603427493,18.2208434775462,
-8.42718229454911));
#107739=CARTESIAN_POINT('Ctrl Pts',(-20.5717385521847,18.1576302317059,
-8.42285429527312));
#107740=CARTESIAN_POINT('Ctrl Pts',(-20.5338394211753,18.0964296531922,
-8.41852629599714));
#107741=CARTESIAN_POINT('Ctrl Pts',(-20.4958706676413,18.035116646275,-8.41419034597851));
#107742=CARTESIAN_POINT('Ctrl Pts',(-20.4548135633609,17.9758240998444,
-8.40985439595988));
#107743=CARTESIAN_POINT('Ctrl Pts',(-20.4109278137949,17.9188691601385,
-8.40551844594126));
#107744=CARTESIAN_POINT('Ctrl Pts',(-20.3707284188952,17.8666983726878,
-8.40154671095239));
#107745=CARTESIAN_POINT('Ctrl Pts',(-20.3281563085948,17.8164887934209,
-8.39757497596352));
#107746=CARTESIAN_POINT('Ctrl Pts',(-20.2834377820475,17.7684565657965,
-8.39360324097465));
#107747=CARTESIAN_POINT('Ctrl Pts',(-20.2340300954518,17.7153877052549,
-8.38921503204375));
#107748=CARTESIAN_POINT('Ctrl Pts',(-20.1817963672772,17.6647565409338,
-8.38482682311285));
#107749=CARTESIAN_POINT('Ctrl Pts',(-20.1270066890244,17.6168791249302,
-8.38043861418195));
#107750=CARTESIAN_POINT('Ctrl Pts',(-20.0722983277384,17.5690727669502,
-8.37605691808068));
#107751=CARTESIAN_POINT('Ctrl Pts',(-20.01504190713,17.5240123587826,-8.37167522197942));
#107752=CARTESIAN_POINT('Ctrl Pts',(-19.9555455237307,17.4819784462149,
-8.36729352587816));
#107753=CARTESIAN_POINT('Ctrl Pts',(-19.8961190533169,17.4399939268396,
-8.36291697861851));
#107754=CARTESIAN_POINT('Ctrl Pts',(-19.8344582408824,17.4010291152647,
-8.35854043135888));
#107755=CARTESIAN_POINT('Ctrl Pts',(-19.7709042257785,17.3653243441594,
-8.35416388409923));
#107756=CARTESIAN_POINT('Ctrl Pts',(-19.7073905157073,17.329642216501,-8.34979011238226));
#107757=CARTESIAN_POINT('Ctrl Pts',(-19.6419864047148,17.2972162628699,
-8.34541634066529));
#107758=CARTESIAN_POINT('Ctrl Pts',(-19.5750607832524,17.2682427431933,
-8.34104256894831));
#107759=CARTESIAN_POINT('Ctrl Pts',(-19.5081555274812,17.2392780402561,
-8.33667012818476));
#107760=CARTESIAN_POINT('Ctrl Pts',(-19.4397301228482,17.2137638770621,
-8.3322976874212));
#107761=CARTESIAN_POINT('Ctrl Pts',(-19.3701752330593,17.1918491703585,
-8.32792524665765));
#107762=CARTESIAN_POINT('Ctrl Pts',(-19.3006185647443,17.1699339032935,
-8.32355269409031));
#107763=CARTESIAN_POINT('Ctrl Pts',(-19.2299328146155,17.1516184185037,
-8.31918014152297));
#107764=CARTESIAN_POINT('Ctrl Pts',(-19.1585240564104,17.1370018501626,
-8.31480758895562));
#107765=CARTESIAN_POINT('Ctrl Pts',(-19.0870411875025,17.1223701121955,
-8.3104304983883));
#107766=CARTESIAN_POINT('Ctrl Pts',(-19.0148342859542,17.1114450521883,
-8.30605340782097));
#107767=CARTESIAN_POINT('Ctrl Pts',(-18.9423190546115,17.1042745381788,
-8.30167631725364));
#107768=CARTESIAN_POINT('Ctrl Pts',(-18.8697642200095,17.0971001080854,
-8.2972968361947));
#107769=CARTESIAN_POINT('Ctrl Pts',(-18.7969012025321,17.0936843291133,
-8.29291735513576));
#107770=CARTESIAN_POINT('Ctrl Pts',(-18.7241475303643,17.0940229267084,
-8.28853787407682));
#107771=CARTESIAN_POINT('Ctrl Pts',(-18.6512649028008,17.0943621244655,
-8.2841506304171));
#107772=CARTESIAN_POINT('Ctrl Pts',(-18.5784924896208,17.0984689605669,
-8.27976338675737));
#107773=CARTESIAN_POINT('Ctrl Pts',(-18.506243930902,17.1062871518924,-8.27537614309765));
#107774=CARTESIAN_POINT('Ctrl Pts',(-18.457121872828,17.1116027686346,-8.27239324016284));
#107775=CARTESIAN_POINT('Ctrl Pts',(-18.4082418439356,17.1186329436866,
-8.26941033722803));
#107776=CARTESIAN_POINT('Ctrl Pts',(-18.3597305432932,17.1273466282089,
-8.26642743429323));
#107777=CARTESIAN_POINT('Ctrl Pts',(-18.2883645862437,17.1401655060193,
-8.26203922536233));
#107778=CARTESIAN_POINT('Ctrl Pts',(-18.2175186632352,17.1566801162964,
-8.25765101643143));
#107779=CARTESIAN_POINT('Ctrl Pts',(-18.1476047194718,17.1768344278367,
-8.25326280750054));
#107780=CARTESIAN_POINT('Ctrl Pts',(-18.0777945395928,17.1969588270371,
-8.24888111139927));
#107781=CARTESIAN_POINT('Ctrl Pts',(-18.0089140527666,17.2207120714409,
-8.24449941529801));
#107782=CARTESIAN_POINT('Ctrl Pts',(-17.9413659204122,17.2479869547362,
-8.24011771919674));
#107783=CARTESIAN_POINT('Ctrl Pts',(-17.8738971624889,17.275229787873,-8.2357411719371));
#107784=CARTESIAN_POINT('Ctrl Pts',(-17.8077580939885,17.3059858596158,
-8.23136462467746));
#107785=CARTESIAN_POINT('Ctrl Pts',(-17.743335448913,17.3400984132725,-8.22698807741782));
#107786=CARTESIAN_POINT('Ctrl Pts',(-17.6789536597427,17.3741893332434,
-8.22261430570085));
#107787=CARTESIAN_POINT('Ctrl Pts',(-17.6162865594643,17.4116322864694,
-8.21824053398388));
#107788=CARTESIAN_POINT('Ctrl Pts',(-17.5556988450224,17.4522233262354,
-8.21386676226691));
#107789=CARTESIAN_POINT('Ctrl Pts',(-17.4951295676255,17.4928020140117,
-8.20949432150335));
#107790=CARTESIAN_POINT('Ctrl Pts',(-17.4366388203457,17.5365266181305,
-8.2051218807398));
#107791=CARTESIAN_POINT('Ctrl Pts',(-17.3805632774557,17.5831492580496,
-8.20074943997625));
#107792=CARTESIAN_POINT('Ctrl Pts',(-17.3244863007078,17.6297730901148,
-8.1963768874089));
#107793=CARTESIAN_POINT('Ctrl Pts',(-17.2708250206044,17.6792947951746,
-8.19200433484156));
#107794=CARTESIAN_POINT('Ctrl Pts',(-17.2198825933093,17.7314265889263,
-8.18763178227421));
#107795=CARTESIAN_POINT('Ctrl Pts',(-17.1688872960418,17.7836124870198,
-8.18325469170688));
#107796=CARTESIAN_POINT('Ctrl Pts',(-17.1206168232081,17.8384135364602,
-8.17887760113955));
#107797=CARTESIAN_POINT('Ctrl Pts',(-17.0753364363188,17.8955061070015,
-8.17450051057222));
#107798=CARTESIAN_POINT('Ctrl Pts',(-17.0300313201297,17.9526298579144,
-8.17012102951329));
#107799=CARTESIAN_POINT('Ctrl Pts',(-16.9877198211689,18.0120472284182,
-8.16574154845435));
#107800=CARTESIAN_POINT('Ctrl Pts',(-16.9486243453002,18.0734048296493,
-8.16136206739541));
#107801=CARTESIAN_POINT('Ctrl Pts',(-16.909459572963,18.1348711868168,-8.15697482373569));
#107802=CARTESIAN_POINT('Ctrl Pts',(-16.873522445187,18.1982842223064,-8.15258758007597));
#107803=CARTESIAN_POINT('Ctrl Pts',(-16.840989532304,18.2632656652873,-8.14820033641625));
#107804=CARTESIAN_POINT('Ctrl Pts',(-16.8188702864075,18.3074467849174,
-8.14521743348143));
#107805=CARTESIAN_POINT('Ctrl Pts',(-16.7983237185205,18.3523524542016,
-8.14223453054661));
#107806=CARTESIAN_POINT('Ctrl Pts',(-16.779392301285,18.3978593331261,-8.13925162761179));
#107807=CARTESIAN_POINT('Ctrl Pts',(-16.7515419099037,18.4648054245267,
-8.13486341868089));
#107808=CARTESIAN_POINT('Ctrl Pts',(-16.7270805292277,18.5333146794851,
-8.13047520975));
#107809=CARTESIAN_POINT('Ctrl Pts',(-16.7061840240079,18.6030103886487,
-8.1260870008191));
#107810=CARTESIAN_POINT('Ctrl Pts',(-16.6853185326665,18.6726026578242,
-8.12170530471783));
#107811=CARTESIAN_POINT('Ctrl Pts',(-16.6680075510804,18.7433774273515,
-8.11732360861657));
#107812=CARTESIAN_POINT('Ctrl Pts',(-16.654378888696,18.8149380939565,-8.1129419125153));
#107813=CARTESIAN_POINT('Ctrl Pts',(-16.6407662410746,18.8864146710833,
-8.10856536525566));
#107814=CARTESIAN_POINT('Ctrl Pts',(-16.6308274068038,18.9586748392569,
-8.10418881799602));
#107815=CARTESIAN_POINT('Ctrl Pts',(-16.6246399100932,19.0313085669594,
-8.09981227073638));
#107816=CARTESIAN_POINT('Ctrl Pts',(-16.618456337403,19.1038962314074,-8.09543849901941));
#107817=CARTESIAN_POINT('Ctrl Pts',(-16.6160194227851,19.1768565058774,
-8.09106472730244));
#107818=CARTESIAN_POINT('Ctrl Pts',(-16.6173550828665,19.2497723454648,
-8.08669095558546));
#107819=CARTESIAN_POINT('Ctrl Pts',(-16.618690336502,19.3226659965173,-8.08231851482191));
#107820=CARTESIAN_POINT('Ctrl Pts',(-16.6237958768595,19.3955147575249,
-8.07794607405836));
#107821=CARTESIAN_POINT('Ctrl Pts',(-16.6326455110292,19.4679013656683,
-8.07357363329481));
#107822=CARTESIAN_POINT('Ctrl Pts',(-16.641495371485,19.5402898247453,-8.06920108072745));
#107823=CARTESIAN_POINT('Ctrl Pts',(-16.6540894553073,19.6122156289261,
-8.0648285281601));
#107824=CARTESIAN_POINT('Ctrl Pts',(-16.670349874122,19.6832680996675,-8.06045597559275));
#107825=CARTESIAN_POINT('Ctrl Pts',(-16.6866271686126,19.754394311343,-8.05607888502542));
#107826=CARTESIAN_POINT('Ctrl Pts',(-16.7065782873149,19.8246449087061,
-8.0517017944581));
#107827=CARTESIAN_POINT('Ctrl Pts',(-16.7300746894323,19.8936216738912,
-8.04732470389077));
#107828=CARTESIAN_POINT('Ctrl Pts',(-16.7535839238069,19.9626361098477,
-8.04294522283183));
#107829=CARTESIAN_POINT('Ctrl Pts',(-16.7806421175113,20.0303748802481,
-8.03856574177288));
#107830=CARTESIAN_POINT('Ctrl Pts',(-16.8110725105125,20.096459694268,-8.03418626071394));
#107831=CARTESIAN_POINT('Ctrl Pts',(-16.841556841181,20.1626616431772,-8.02979901705422));
#107832=CARTESIAN_POINT('Ctrl Pts',(-16.8754250830337,20.2272033538502,
-8.0254117733945));
#107833=CARTESIAN_POINT('Ctrl Pts',(-16.9124547443363,20.2897316077547,
-8.02102452973478));
#107834=CARTESIAN_POINT('Ctrl Pts',(-16.9376313458523,20.3322447952014,
-8.01804162679997));
#107835=CARTESIAN_POINT('Ctrl Pts',(-16.9642684397432,20.3738277943096,
-8.01505872386516));
#107836=CARTESIAN_POINT('Ctrl Pts',(-16.992285306212,20.4143781306983,-8.01207582093036));
#107837=CARTESIAN_POINT('Ctrl Pts',(-17.033501486001,20.4740325519721,-8.00768761199946));
#107838=CARTESIAN_POINT('Ctrl Pts',(-17.0778664461833,20.5316834623514,
-8.00329940306856));
#107839=CARTESIAN_POINT('Ctrl Pts',(-17.1251586260628,20.5869790817843,
-7.99891119413766));
#107840=CARTESIAN_POINT('Ctrl Pts',(-17.1723806165062,20.6421926333496,
-7.99452949803641));
#107841=CARTESIAN_POINT('Ctrl Pts',(-17.2225208913246,20.6950574697366,
-7.99014780193515));
#107842=CARTESIAN_POINT('Ctrl Pts',(-17.2753151507576,20.7452514495971,
-7.9857661058339));
#107843=CARTESIAN_POINT('Ctrl Pts',(-17.3280473727344,20.7953864475367,
-7.98138955857426));
#107844=CARTESIAN_POINT('Ctrl Pts',(-17.3834270362631,20.8428564928137,
-7.97701301131462));
#107845=CARTESIAN_POINT('Ctrl Pts',(-17.4411513321099,20.8873744575526,
-7.97263646405498));
#107846=CARTESIAN_POINT('Ctrl Pts',(-17.4988390200472,20.9318641896452,
-7.96826269233801));
#107847=CARTESIAN_POINT('Ctrl Pts',(-17.5588680089998,20.9734052619584,
-7.96388892062104));
#107848=CARTESIAN_POINT('Ctrl Pts',(-17.6209016583803,21.0117501442131,
-7.95951514890407));
#107849=CARTESIAN_POINT('Ctrl Pts',(-17.6829164307129,21.0500833579914,
-7.95514270814051));
#107850=CARTESIAN_POINT('Ctrl Pts',(-17.7469342423152,21.0852220591674,
-7.95077026737696));
#107851=CARTESIAN_POINT('Ctrl Pts',(-17.8125900634642,21.1169624153831,
-7.9463978266134));
#107852=CARTESIAN_POINT('Ctrl Pts',(-17.8782475634396,21.1487035832032,
-7.94202527404607));
#107853=CARTESIAN_POINT('Ctrl Pts',(-17.9455427209574,21.1770460253878,
-7.93765272147873));
#107854=CARTESIAN_POINT('Ctrl Pts',(-18.0140880608545,21.2018329412273,
-7.9332801689114));
#107855=CARTESIAN_POINT('Ctrl Pts',(-18.082704539691,21.2266455818631,-7.92890307834407));
#107856=CARTESIAN_POINT('Ctrl Pts',(-18.152573336826,21.2478951643122,-7.92452598777674));
#107857=CARTESIAN_POINT('Ctrl Pts',(-18.2232900373585,21.2654742232646,
-7.92014889720942));
#107858=CARTESIAN_POINT('Ctrl Pts',(-18.2940453589056,21.2830628827936,
-7.91576941615048));
#107859=CARTESIAN_POINT('Ctrl Pts',(-18.3656490319724,21.2969769355905,
-7.91138993509155));
#107860=CARTESIAN_POINT('Ctrl Pts',(-18.4376872969879,21.307160247222,-7.90701045403262));
#107861=CARTESIAN_POINT('Ctrl Pts',(-18.5098532493447,21.317361608705,-7.9026232103729));
#107862=CARTESIAN_POINT('Ctrl Pts',(-18.5824548510264,21.3238189809293,
-7.89823596671317));
#107863=CARTESIAN_POINT('Ctrl Pts',(-18.6550746705894,21.3265282537412,
-7.89384872305345));
#107864=CARTESIAN_POINT('Ctrl Pts',(-18.7044491502636,21.3283702981885,
-7.89086582011861));
#107865=CARTESIAN_POINT('Ctrl Pts',(-18.7538320255725,21.328480806371,-7.88788291718377));
#107866=CARTESIAN_POINT('Ctrl Pts',(-18.8030934396838,21.3268721834252,
-7.88490001424892));
#107867=CARTESIAN_POINT('Ctrl Pts',(-18.8755629038515,21.3245057056244,
-7.88051180531802));
#107868=CARTESIAN_POINT('Ctrl Pts',(-18.9480521075247,21.3184071393707,
-7.87612359638712));
#107869=CARTESIAN_POINT('Ctrl Pts',(-19.020145332748,21.3085723702763,-7.87173538745622));
#107870=CARTESIAN_POINT('Ctrl Pts',(-19.092131559672,21.2987521976099,-7.86735369135494));
#107871=CARTESIAN_POINT('Ctrl Pts',(-19.1637225008059,21.2852068946333,
-7.86297199525365));
#107872=CARTESIAN_POINT('Ctrl Pts',(-19.2345042258083,21.267984326617,-7.85859029915237));
#107873=CARTESIAN_POINT('Ctrl Pts',(-19.3052027766504,21.2507819964888,
-7.85421375189273));
#107874=CARTESIAN_POINT('Ctrl Pts',(-19.3750935339405,21.2299110986508,
-7.84983720463309));
#107875=CARTESIAN_POINT('Ctrl Pts',(-19.4437711636792,21.2054708308746,
-7.84546065737346));
#107876=CARTESIAN_POINT('Ctrl Pts',(-19.5124052390632,21.181046062761,-7.84108688565648));
#107877=CARTESIAN_POINT('Ctrl Pts',(-19.5798272600416,21.1530565773996,
-7.83671311393951));
#107878=CARTESIAN_POINT('Ctrl Pts',(-19.645646875657,21.1216514528047,-7.83233934222254));
#107879=CARTESIAN_POINT('Ctrl Pts',(-19.7114464621423,21.0902558848947,
-7.82796690145899));
#107880=CARTESIAN_POINT('Ctrl Pts',(-19.7756441762378,21.0554469488639,
-7.82359446069543));
#107881=CARTESIAN_POINT('Ctrl Pts',(-19.8378710435217,21.0174212463527,
-7.81922201993188));
#107882=CARTESIAN_POINT('Ctrl Pts',(-19.9000995019534,20.97939457152,-7.81484946736454));
#107883=CARTESIAN_POINT('Ctrl Pts',(-19.9603566029528,20.9381512201346,
-7.81047691479719));
#107884=CARTESIAN_POINT('Ctrl Pts',(-20.0183007689806,20.8939321242391,
-7.80610436222985));
#107885=CARTESIAN_POINT('Ctrl Pts',(-20.0763050716495,20.8496671360979,
-7.80172727166252));
#107886=CARTESIAN_POINT('Ctrl Pts',(-20.1319912623925,20.8024205306336,
-7.79735018109519));
#107887=CARTESIAN_POINT('Ctrl Pts',(-20.185050077775,20.752474187844,-7.79297309052786));
#107888=CARTESIAN_POINT('Ctrl Pts',(-20.2381378705458,20.7025005675028,
-7.78859360946892));
#107889=CARTESIAN_POINT('Ctrl Pts',(-20.2885950971614,20.6498246228585,
-7.78421412840997));
#107890=CARTESIAN_POINT('Ctrl Pts',(-20.3361505972387,20.5947638757272,
-7.77983464735103));
#107891=CARTESIAN_POINT('Ctrl Pts',(-20.3837903891206,20.5396055337913,
-7.77544740369131));
#107892=CARTESIAN_POINT('Ctrl Pts',(-20.4285178872519,20.4820543293407,
-7.77106016003158));
#107893=CARTESIAN_POINT('Ctrl Pts',(-20.4701036879207,20.4224590314114,
-7.76667291637186));
#107894=CARTESIAN_POINT('Ctrl Pts',(-20.4983780251769,20.3819399714091,
-7.76369001343707));
#107895=CARTESIAN_POINT('Ctrl Pts',(-20.5252009588541,20.3404766042677,
-7.76070711050228));
#107896=CARTESIAN_POINT('Ctrl Pts',(-20.5505126306682,20.2981848336979,
-7.75772420756748));
#107897=CARTESIAN_POINT('Ctrl Pts',(-20.5890325091506,20.2338242543132,
-7.75318475796428));
#107898=CARTESIAN_POINT('Ctrl Pts',(-20.6241921153259,20.1673074236142,
-7.74864530836107));
#107899=CARTESIAN_POINT('Ctrl Pts',(-20.6557527999571,20.09900629269,-7.74410585875786));
#107900=CARTESIAN_POINT('Ctrl Pts',(-20.6876473131869,20.0299827163852,
-7.73951839377991));
#107901=CARTESIAN_POINT('Ctrl Pts',(-20.7158660149377,19.9591372097163,
-7.73493092880197));
#107902=CARTESIAN_POINT('Ctrl Pts',(-20.7402081049558,19.8868831552935,
-7.73034346382402));
#107903=CARTESIAN_POINT('Ctrl Pts',(-20.7642010194565,19.8156655503632,
-7.7258218038142));
#107904=CARTESIAN_POINT('Ctrl Pts',(-20.7844276391864,19.7430799630087,
-7.72130014380437));
#107905=CARTESIAN_POINT('Ctrl Pts',(-20.800742748614,19.6695448844458,-7.71677848379455));
#107906=CARTESIAN_POINT('Ctrl Pts',(-20.8174140154883,19.5944045413925,
-7.71215811633254));
#107907=CARTESIAN_POINT('Ctrl Pts',(-20.8300007712015,19.5182731789951,
-7.70753774887053));
#107908=CARTESIAN_POINT('Ctrl Pts',(-20.8384015048747,19.441615060829,-7.70291738140852));
#107909=CARTESIAN_POINT('Ctrl Pts',(-20.8468022385479,19.3649569426629,
-7.69829701394651));
#107910=CARTESIAN_POINT('Ctrl Pts',(-20.8510168371563,19.2877725479369,
-7.69367664648451));
#107911=CARTESIAN_POINT('Ctrl Pts',(-20.850999949394,19.2105371115439,-7.6890562790225));
#107912=CARTESIAN_POINT('Ctrl Pts',(-20.8476071281599,19.2105314192558,
-7.68905589350251));
#107913=CARTESIAN_POINT('Ctrl Pts',(-20.8480884203062,18.9629933058656,
-7.67422393940026));
#107914=CARTESIAN_POINT('Ctrl Pts',(-20.8073981352126,18.7156059215239,
-7.65939198529801));
#107915=CARTESIAN_POINT('Ctrl Pts',(-20.7249099383763,18.4840591618169,
-7.64456003119576));
#107916=CARTESIAN_POINT('Origin',(-18.734,19.211,0.));
#107917=CARTESIAN_POINT('',(-20.7225806151895,18.4848897212595,-6.84500607926505));
#107918=CARTESIAN_POINT('',(-20.7225806056755,18.4848896952038,-7.06814847058112));
#107919=CARTESIAN_POINT('',(-20.7225806137986,18.4848897174502,0.));
#107920=CARTESIAN_POINT('',(-20.8510002458083,19.2120354932906,-7.10922378494469));
#107921=CARTESIAN_POINT('Ctrl Pts',(-20.7225806056755,18.4848896952038,
-7.06814847058112));
#107922=CARTESIAN_POINT('Ctrl Pts',(-20.7469467821702,18.5516207492762,
-7.07223678875001));
#107923=CARTESIAN_POINT('Ctrl Pts',(-20.7679438661329,18.6195503552378,
-7.07621988970315));
#107924=CARTESIAN_POINT('Ctrl Pts',(-20.829084658028,18.8595719529904,-7.0898896347857));
#107925=CARTESIAN_POINT('Ctrl Pts',(-20.8510858772448,19.0354726805544,
-7.09915343889004));
#107926=CARTESIAN_POINT('Ctrl Pts',(-20.8509997481128,19.212032710241,-7.10922276175899));
#107927=CARTESIAN_POINT('Ctrl Pts',(-20.8509997467294,19.212035542177,-7.10922292326604));
#107928=CARTESIAN_POINT('Ctrl Pts',(-20.8509866388109,19.238832577368,-7.11075117535696));
#107929=CARTESIAN_POINT('Ctrl Pts',(-20.8504647358669,19.2656259780468,
-7.11229812416721));
#107930=CARTESIAN_POINT('Ctrl Pts',(-20.8488772351525,19.306881542247,-7.1147189423379));
#107931=CARTESIAN_POINT('Ctrl Pts',(-20.8481713907108,19.3213553130007,
-7.1155756299352));
#107932=CARTESIAN_POINT('Ctrl Pts',(-20.847039981172,19.34051107497,-7.11672056384823));
#107933=CARTESIAN_POINT('Ctrl Pts',(-20.8467473097919,19.3452009113002,
-7.11700175783987));
#107934=CARTESIAN_POINT('Ctrl Pts',(-20.8462061821906,19.3534311774479,
-7.11749684192021));
#107935=CARTESIAN_POINT('Ctrl Pts',(-20.8459644307084,19.3569720500464,
-7.11771036402102));
#107936=CARTESIAN_POINT('Ctrl Pts',(-20.8454718256778,19.3639296117368,
-7.11813097919925));
#107937=CARTESIAN_POINT('Ctrl Pts',(-20.8452215797129,19.3673463399483,
-7.11833803869449));
#107938=CARTESIAN_POINT('Ctrl Pts',(-20.8446669325148,19.374674968951,-7.11878326863147));
#107939=CARTESIAN_POINT('Ctrl Pts',(-20.8443599503591,19.3785866188367,
-7.11902158000591));
#107940=CARTESIAN_POINT('Ctrl Pts',(-20.8435234723322,19.3888783451667,
-7.11965031160079));
#107941=CARTESIAN_POINT('Ctrl Pts',(-20.8429759114186,19.3952568550261,
-7.12004172511595));
#107942=CARTESIAN_POINT('Ctrl Pts',(-20.8405832027644,19.4217202366947,
-7.12167260083017));
#107943=CARTESIAN_POINT('Ctrl Pts',(-20.8384800652699,19.4417799699492,
-7.12292549519722));
#107944=CARTESIAN_POINT('Ctrl Pts',(-20.835585736007,19.4660383587798,-7.12445837341481));
#107945=CARTESIAN_POINT('Ctrl Pts',(-20.8350679509523,19.4702694257601,
-7.12472638862714));
#107946=CARTESIAN_POINT('Ctrl Pts',(-20.8313092230471,19.500232926735,-7.1266289285973));
#107947=CARTESIAN_POINT('Ctrl Pts',(-20.8276085458607,19.5259044409515,
-7.12828252494956));
#107948=CARTESIAN_POINT('Ctrl Pts',(-20.7949769851179,19.7261438788488,
-7.1413336803723));
#107949=CARTESIAN_POINT('Ctrl Pts',(-20.7447340062298,19.8965335727698,
-7.15327774337597));
#107950=CARTESIAN_POINT('Ctrl Pts',(-20.6502651860484,20.1127161683493,
-7.16848804445987));
#107951=CARTESIAN_POINT('Ctrl Pts',(-20.6244119201432,20.1657293204335,
-7.17223080315733));
#107952=CARTESIAN_POINT('Ctrl Pts',(-20.5792508989512,20.2492848789387,
-7.17814298236814));
#107953=CARTESIAN_POINT('Ctrl Pts',(-20.5613178022045,20.2805308643735,
-7.18035723787088));
#107954=CARTESIAN_POINT('Ctrl Pts',(-20.5368774061374,20.3207040517759,
-7.18321038315292));
#107955=CARTESIAN_POINT('Ctrl Pts',(-20.5310863590702,20.330057929371,-7.18387517373648));
#107956=CARTESIAN_POINT('Ctrl Pts',(-20.5215233221819,20.345238749928,-7.18495497962293));
#107957=CARTESIAN_POINT('Ctrl Pts',(-20.5177951807465,20.3510929453834,
-7.18537160435052));
#107958=CARTESIAN_POINT('Ctrl Pts',(-20.5105519342274,20.3623443046225,
-7.18617279265389));
#107959=CARTESIAN_POINT('Ctrl Pts',(-20.5070408606974,20.3677439606527,
-7.18655750017841));
#107960=CARTESIAN_POINT('Ctrl Pts',(-20.498919027194,20.3801106120571,-7.18743910752061));
#107961=CARTESIAN_POINT('Ctrl Pts',(-20.4942915398638,20.3870665344756,
-7.18793537409213));
#107962=CARTESIAN_POINT('Ctrl Pts',(-20.4818301475165,20.4055598561801,
-7.18925592976821));
#107963=CARTESIAN_POINT('Ctrl Pts',(-20.4739231320461,20.4170476702888,
-7.19007745492741));
#107964=CARTESIAN_POINT('Ctrl Pts',(-20.4095513678279,20.5086202508339,
-7.19663791284082));
#107965=CARTESIAN_POINT('Ctrl Pts',(-20.3476984772763,20.5847799811123,
-7.20215962191543));
#107966=CARTESIAN_POINT('Ctrl Pts',(-20.1873374477826,20.7563905983615,
-7.21511375898675));
#107967=CARTESIAN_POINT('Ctrl Pts',(-20.0844177080016,20.8470902846918,
-7.22239522681411));
#107968=CARTESIAN_POINT('Ctrl Pts',(-19.9318268842307,20.9572926963362,
-7.23282452956406));
#107969=CARTESIAN_POINT('Ctrl Pts',(-19.889107549375,20.9858389406645,-7.23571235750914));
#107970=CARTESIAN_POINT('Ctrl Pts',(-19.8300638695438,21.0222585378053,
-7.23972036859023));
#107971=CARTESIAN_POINT('Ctrl Pts',(-19.8146125671854,21.031519138202,-7.24077074177687));
#107972=CARTESIAN_POINT('Ctrl Pts',(-19.791573920485,21.0449305179197,-7.24234197176213));
#107973=CARTESIAN_POINT('Ctrl Pts',(-19.7840758999984,21.0492340277016,
-7.24285411880012));
#107974=CARTESIAN_POINT('Ctrl Pts',(-19.770452897438,21.0569424418053,-7.24378643146881));
#107975=CARTESIAN_POINT('Ctrl Pts',(-19.7643369253056,21.0603631131528,
-7.24420564019099));
#107976=CARTESIAN_POINT('Ctrl Pts',(-19.7546742301547,21.0657046622724,
-7.24486915771922));
#107977=CARTESIAN_POINT('Ctrl Pts',(-19.751138744273,21.0676459120229,-7.24511218495754));
#107978=CARTESIAN_POINT('Ctrl Pts',(-19.747588675693,21.0695819854432,-7.24535648936914));
#107979=CARTESIAN_POINT('Ctrl Pts',(-19.7475795859075,21.0695869425827,
-7.24535711490102));
#107980=CARTESIAN_POINT('Ctrl Pts',(-19.7475613507176,21.0695968870199,
-7.24535836979594));
#107981=CARTESIAN_POINT('Ctrl Pts',(-19.7475522053045,21.0696018743214,
-7.2453589991596));
#107982=CARTESIAN_POINT('Ctrl Pts',(-19.7475338597622,21.0696118785872,
-7.24536026165599));
#107983=CARTESIAN_POINT('Ctrl Pts',(-19.7475246581378,21.0696168963658,
-7.24536089489164));
#107984=CARTESIAN_POINT('Ctrl Pts',(-19.7475061984414,21.0696269625269,
-7.24536216525126));
#107985=CARTESIAN_POINT('Ctrl Pts',(-19.7474969416186,21.0696320102271,
-7.24536280228928));
#107986=CARTESIAN_POINT('Ctrl Pts',(-19.74747837093,21.0696421365528,-7.24536408029467));
#107987=CARTESIAN_POINT('Ctrl Pts',(-19.7474690572325,21.0696472150854,
-7.24536472125048));
#107988=CARTESIAN_POINT('Ctrl Pts',(-19.7474503730712,21.0696574029218,
-7.24536600707248));
#107989=CARTESIAN_POINT('Ctrl Pts',(-19.7474410022956,21.0696625123943,
-7.24536665196016));
#107990=CARTESIAN_POINT('Ctrl Pts',(-19.7474222031634,21.0696727625515,
-7.24536794570202));
#107991=CARTESIAN_POINT('Ctrl Pts',(-19.7474127753466,21.0696779029406,
-7.24536859451908));
#107992=CARTESIAN_POINT('Ctrl Pts',(-19.7473938621929,21.0696882148942,
-7.24536989611561));
#107993=CARTESIAN_POINT('Ctrl Pts',(-19.7473843762638,21.0696933867804,
-7.24537054893585));
#107994=CARTESIAN_POINT('Ctrl Pts',(-19.7473653458116,21.0697037623103,
-7.2453718586127));
#107995=CARTESIAN_POINT('Ctrl Pts',(-19.7473558022532,21.0697089654268,
-7.24537251540296));
#107996=CARTESIAN_POINT('Ctrl Pts',(-19.7473366566343,21.0697194033637,
-7.24537383301358));
#107997=CARTESIAN_POINT('Ctrl Pts',(-19.7473270539974,21.0697246384972,
-7.24537449387365));
#107998=CARTESIAN_POINT('Ctrl Pts',(-19.7473077898938,21.0697351406431,
-7.24537581964653));
#107999=CARTESIAN_POINT('Ctrl Pts',(-19.747298128484,21.0697404076234,-7.24537648455546));
#108000=CARTESIAN_POINT('Ctrl Pts',(-19.7472787461405,21.0697509738377,
-7.24537781847392));
#108001=CARTESIAN_POINT('Ctrl Pts',(-19.7472690253539,21.0697562729904,
-7.24537848747334));
#108002=CARTESIAN_POINT('Ctrl Pts',(-19.7472495617317,21.0697668831173,
-7.24537982699377));
#108003=CARTESIAN_POINT('Ctrl Pts',(-19.747239762086,21.0697722250598,-7.24538050142478));
#108004=CARTESIAN_POINT('Ctrl Pts',(-19.747220120423,21.0697829318393,-7.24538185320671));
#108005=CARTESIAN_POINT('Ctrl Pts',(-19.7472102800833,21.0697882957617,
-7.24538253044237));
#108006=CARTESIAN_POINT('Ctrl Pts',(-19.7471905368017,21.0697990575273,
-7.24538388922641));
#108007=CARTESIAN_POINT('Ctrl Pts',(-19.7471806358372,21.0698044542912,
-7.24538457063869));
#108008=CARTESIAN_POINT('Ctrl Pts',(-19.7471607708919,21.0698152819621,
-7.24538593780454));
#108009=CARTESIAN_POINT('Ctrl Pts',(-19.7471508087519,21.0698207118643,
-7.24538662343144));
#108010=CARTESIAN_POINT('Ctrl Pts',(-19.7471307895991,21.0698316231706,
-7.24538800121905));
#108011=CARTESIAN_POINT('Ctrl Pts',(-19.7471207816009,21.0698370778576,
-7.24538869000625));
#108012=CARTESIAN_POINT('Ctrl Pts',(-19.7441075652915,21.07147934817,-7.24559607133871));
#108013=CARTESIAN_POINT('Ctrl Pts',(-19.7411004588033,21.0731088485091,
-7.24580323311674));
#108014=CARTESIAN_POINT('Ctrl Pts',(-19.734048189569,21.0769082749406,-7.2462895287151));
#108015=CARTESIAN_POINT('Ctrl Pts',(-19.7299999213996,21.0790723293297,
-7.24656903072244));
#108016=CARTESIAN_POINT('Ctrl Pts',(-19.7175117266943,21.0856959230251,
-7.24743224548494));
#108017=CARTESIAN_POINT('Ctrl Pts',(-19.7090487868861,21.0901114857038,
-7.24801862673343));
#108018=CARTESIAN_POINT('Ctrl Pts',(-19.5959279689524,21.148162679678,-7.25587224861653));
#108019=CARTESIAN_POINT('Ctrl Pts',(-19.4870191423013,21.193038039962,-7.26360090159983));
#108020=CARTESIAN_POINT('Ctrl Pts',(-19.2704614072204,21.2618342266719,
-7.27860966937119));
#108021=CARTESIAN_POINT('Ctrl Pts',(-19.1635296367042,21.2868659915252,
-7.28586175390677));
#108022=CARTESIAN_POINT('Ctrl Pts',(-18.9798958472266,21.3150480880672,
-7.29780669591059));
#108023=CARTESIAN_POINT('Ctrl Pts',(-18.9040832937476,21.3225295485691,
-7.302598333006));
#108024=CARTESIAN_POINT('Ctrl Pts',(-18.8090892881317,21.3267527863396,
-7.30842436700041));
#108025=CARTESIAN_POINT('Ctrl Pts',(-18.790143078176,21.3273402953087,-7.30957773020232));
#108026=CARTESIAN_POINT('Ctrl Pts',(-18.7626111758836,21.3278240449663,
-7.31124168769252));
#108027=CARTESIAN_POINT('Ctrl Pts',(-18.7540303813472,21.3279226305993,
-7.31175858917514));
#108028=CARTESIAN_POINT('Ctrl Pts',(-18.738995838723,21.3280039413551,-7.31266134982074));
#108029=CARTESIAN_POINT('Ctrl Pts',(-18.732542372347,21.3280093346203,-7.31304791387815));
#108030=CARTESIAN_POINT('Ctrl Pts',(-18.7200192406795,21.327962536269,-7.31379626560532));
#108031=CARTESIAN_POINT('Ctrl Pts',(-18.7139496327782,21.3279137501448,
-7.31415815610573));
#108032=CARTESIAN_POINT('Ctrl Pts',(-18.699453270723,21.3277348791519,-7.31502057352149));
#108033=CARTESIAN_POINT('Ctrl Pts',(-18.6910268771331,21.3275805770049,
-7.31552033889434));
#108034=CARTESIAN_POINT('Ctrl Pts',(-18.6606992749911,21.3268440386015,
-7.31731370092195));
#108035=CARTESIAN_POINT('Ctrl Pts',(-18.6388060191357,21.3259721394975,
-7.31859824488434));
#108036=CARTESIAN_POINT('Ctrl Pts',(-18.4297009203736,21.3143908780171,
-7.3307809302873));
#108037=CARTESIAN_POINT('Ctrl Pts',(-18.2446857031687,21.2791944941734,
-7.34080119373469));
#108038=CARTESIAN_POINT('Ctrl Pts',(-17.9918550085426,21.1952207225491,
-7.35533055634334));
#108039=CARTESIAN_POINT('Ctrl Pts',(-17.9184496379319,21.1661948069355,
-7.35967215678778));
#108040=CARTESIAN_POINT('Ctrl Pts',(-17.8144380101076,21.118188605362,-7.36622721649198));
#108041=CARTESIAN_POINT('Ctrl Pts',(-17.7824203921183,21.102417071965,-7.36830359405264));
#108042=CARTESIAN_POINT('Ctrl Pts',(-17.7442251037883,21.0823872097441,
-7.37087033802637));
#108043=CARTESIAN_POINT('Ctrl Pts',(-17.7376497520927,21.0788947009194,
-7.37131548093427));
#108044=CARTESIAN_POINT('Ctrl Pts',(-17.7274341054552,21.0733993562359,
-7.3720123985891));
#108045=CARTESIAN_POINT('Ctrl Pts',(-17.7237809778512,21.0714203258339,
-7.37226268586176));
#108046=CARTESIAN_POINT('Ctrl Pts',(-17.7170029557306,21.0677225778187,
-7.37272910290817));
#108047=CARTESIAN_POINT('Ctrl Pts',(-17.7138765700374,21.0660067132131,
-7.37294505074972));
#108048=CARTESIAN_POINT('Ctrl Pts',(-17.7068004432007,21.0620998005357,
-7.37343565337955));
#108049=CARTESIAN_POINT('Ctrl Pts',(-17.7028533888527,21.0599040176485,
-7.37371060783005));
#108050=CARTESIAN_POINT('Ctrl Pts',(-17.6926708524161,21.0541966306698,
-7.37442322724189));
#108051=CARTESIAN_POINT('Ctrl Pts',(-17.6864461541182,21.050666042944,-7.37486206785098));
#108052=CARTESIAN_POINT('Ctrl Pts',(-17.6481280501512,21.0286748589315,
-7.37758278292947));
#108053=CARTESIAN_POINT('Ctrl Pts',(-17.6165076871889,21.009407721105,-7.37991175355753));
#108054=CARTESIAN_POINT('Ctrl Pts',(-17.442243393115,20.8968533354313,-7.39315500204117));
#108055=CARTESIAN_POINT('Ctrl Pts',(-17.3107668824149,20.7874349907261,
-7.40465479597926));
#108056=CARTESIAN_POINT('Ctrl Pts',(-17.1285733358706,20.5942356621574,
-7.42191011089756));
#108057=CARTESIAN_POINT('Ctrl Pts',(-17.0680484040015,20.5207118646229,
-7.42795239755897));
#108058=CARTESIAN_POINT('Ctrl Pts',(-17.0002336088481,20.4259894318504,
-7.43510796054048));
#108059=CARTESIAN_POINT('Ctrl Pts',(-16.9880630700075,20.4084345525163,
-7.43640986189084));
#108060=CARTESIAN_POINT('Ctrl Pts',(-16.9711422664415,20.3832212629625,
-7.43824622619549));
#108061=CARTESIAN_POINT('Ctrl Pts',(-16.9661722933924,20.3757125318183,
-7.43878896937054));
#108062=CARTESIAN_POINT('Ctrl Pts',(-16.9576834984331,20.3627079779575,
-7.43972192179025));
#108063=CARTESIAN_POINT('Ctrl Pts',(-16.9541419315327,20.357227219107,-7.44011298005118));
#108064=CARTESIAN_POINT('Ctrl Pts',(-16.9474110858534,20.3467044699221,
-7.44085975392969));
#108065=CARTESIAN_POINT('Ctrl Pts',(-16.9442176736913,20.3416652098244,
-7.44121562091924));
#108066=CARTESIAN_POINT('Ctrl Pts',(-16.9359727271505,20.3285320813027,
-7.44213855489813));
#108067=CARTESIAN_POINT('Ctrl Pts',(-16.9309544943303,20.3204173856874,
-7.44270438797607));
#108068=CARTESIAN_POINT('Ctrl Pts',(-16.9140481035296,20.2926613110696,
-7.44462502750829));
#108069=CARTESIAN_POINT('Ctrl Pts',(-16.9024244075849,20.2728601637084,
-7.44597017547181));
#108070=CARTESIAN_POINT('Ctrl Pts',(-16.8045469022421,20.099733511415,-7.45752710287622));
#108071=CARTESIAN_POINT('Ctrl Pts',(-16.7373941875307,19.9364022466313,
-7.46698362266903));
#108072=CARTESIAN_POINT('Ctrl Pts',(-16.6684626516087,19.6829753194227,
-7.48127480216599));
#108073=CARTESIAN_POINT('Ctrl Pts',(-16.6508703309531,19.5980060005061,
-7.48602197005629));
#108074=CARTESIAN_POINT('Ctrl Pts',(-16.6331668456332,19.4748441830829,
-7.49312667492237));
#108075=CARTESIAN_POINT('Ctrl Pts',(-16.6287970218653,19.4373486677181,
-7.49531931382054));
#108076=CARTESIAN_POINT('Ctrl Pts',(-16.6247572804446,19.3922219998179,
-7.49801499248867));
#108077=CARTESIAN_POINT('Ctrl Pts',(-16.6241229869961,19.3846814592724,
-7.49846733096744));
#108078=CARTESIAN_POINT('Ctrl Pts',(-16.6232010055168,19.3729694050171,
-7.49917307734983));
#108079=CARTESIAN_POINT('Ctrl Pts',(-16.6228852191966,19.3688000787462,
-7.49942493610065));
#108080=CARTESIAN_POINT('Ctrl Pts',(-16.6223231612413,19.3610754137424,
-7.49989276282739));
#108081=CARTESIAN_POINT('Ctrl Pts',(-16.6220735147062,19.357520378419,-7.5001085392746));
#108082=CARTESIAN_POINT('Ctrl Pts',(-16.6215302107451,19.34949358185,-7.50059679894941));
#108083=CARTESIAN_POINT('Ctrl Pts',(-16.6212417766759,19.3450215342786,
-7.50086956966399));
#108084=CARTESIAN_POINT('Ctrl Pts',(-16.6204344445541,19.3318533619991,
-7.50167487299511));
#108085=CARTESIAN_POINT('Ctrl Pts',(-16.6199550301464,19.3231550342996,
-7.50220953737669));
#108086=CARTESIAN_POINT('Ctrl Pts',(-16.6169292109334,19.2613111660761,
-7.50602903476624));
#108087=CARTESIAN_POINT('Ctrl Pts',(-16.6163337223535,19.2080936523045,
-7.50941043539998));
#108088=CARTESIAN_POINT('Ctrl Pts',(-16.6182284982312,19.136597479866,-7.51403235991408));
#108089=CARTESIAN_POINT('Ctrl Pts',(-16.6189517616592,19.1182869752344,
-7.51522308339859));
#108090=CARTESIAN_POINT('Ctrl Pts',(-16.6224277275562,19.0520911377894,
-7.5195484362301));
#108091=CARTESIAN_POINT('Ctrl Pts',(-16.6265698190564,19.0042941889997,
-7.5227104157986));
#108092=CARTESIAN_POINT('Ctrl Pts',(-16.6454711166344,18.8480959323211,
-7.53310371964198));
#108093=CARTESIAN_POINT('Ctrl Pts',(-16.6670072456871,18.7406844904373,
-7.54033607612409));
#108094=CARTESIAN_POINT('Ctrl Pts',(-16.7117292009486,18.5823942610658,
-7.55090879469441));
#108095=CARTESIAN_POINT('Ctrl Pts',(-16.7287734952871,18.5299773533292,
-7.55439753703905));
#108096=CARTESIAN_POINT('Ctrl Pts',(-16.7597165677077,18.4461010208939,
-7.55995455183979));
#108097=CARTESIAN_POINT('Ctrl Pts',(-16.7723691943367,18.4142125014765,
-7.56206125347214));
#108098=CARTESIAN_POINT('Ctrl Pts',(-16.7900208471462,18.3726976268708,
-7.56479760346392));
#108099=CARTESIAN_POINT('Ctrl Pts',(-16.7943261005433,18.3627836443009,
-7.56545058933261));
#108100=CARTESIAN_POINT('Ctrl Pts',(-16.8015031399717,18.3465970455908,
-7.56651606645575));
#108101=CARTESIAN_POINT('Ctrl Pts',(-16.8043299557075,18.3403048159528,
-7.56693008702831));
#108102=CARTESIAN_POINT('Ctrl Pts',(-16.8098622357212,18.3281497556809,
-7.56772959970173));
#108103=CARTESIAN_POINT('Ctrl Pts',(-16.8125638640162,18.3222852726665,
-7.5681152181177));
#108104=CARTESIAN_POINT('Ctrl Pts',(-16.8188649922172,18.3087703254852,
-7.56900364962267));
#108105=CARTESIAN_POINT('Ctrl Pts',(-16.8224835929839,18.3011288484176,
-7.56950579659309));
#108106=CARTESIAN_POINT('Ctrl Pts',(-16.8323412323096,18.2806306405874,
-7.57085244874572));
#108107=CARTESIAN_POINT('Ctrl Pts',(-16.8386648996876,18.2678149247873,
-7.57169401222917));
#108108=CARTESIAN_POINT('Ctrl Pts',(-16.8978944681167,18.1507802428592,
-7.57937831199596));
#108109=CARTESIAN_POINT('Ctrl Pts',(-16.9592192411624,18.0510396631901,
-7.58590412118604));
#108110=CARTESIAN_POINT('Ctrl Pts',(-17.1249845837826,17.8256123045543,
-7.60122216395494));
#108111=CARTESIAN_POINT('Ctrl Pts',(-17.236311721042,17.7059592805319,-7.60983082559518));
#108112=CARTESIAN_POINT('Ctrl Pts',(-17.3848200802793,17.579299529788,-7.62104054326569));
#108113=CARTESIAN_POINT('Ctrl Pts',(-17.4098779647989,17.5589002877034,
-7.62292525659317));
#108114=CARTESIAN_POINT('Ctrl Pts',(-17.4410979515934,17.534651137863,-7.62527904786693));
#108115=CARTESIAN_POINT('Ctrl Pts',(-17.4468272626404,17.5302479197882,
-7.62571122740489));
#108116=CARTESIAN_POINT('Ctrl Pts',(-17.4558478258553,17.5233884082339,
-7.62639222513861));
#108117=CARTESIAN_POINT('Ctrl Pts',(-17.4591239364024,17.5209121659685,
-7.62663966420562));
#108118=CARTESIAN_POINT('Ctrl Pts',(-17.4652633386587,17.5162997179251,
-7.62710361602306));
#108119=CARTESIAN_POINT('Ctrl Pts',(-17.4681248394151,17.5141612218448,
-7.62731996452228));
#108120=CARTESIAN_POINT('Ctrl Pts',(-17.4746722116452,17.5092939286056,
-7.62781522246919));
#108121=CARTESIAN_POINT('Ctrl Pts',(-17.4783615335456,17.506569868669,-7.62809445534763));
#108122=CARTESIAN_POINT('Ctrl Pts',(-17.4897393120993,17.4982259236788,
-7.62895603151567));
#108123=CARTESIAN_POINT('Ctrl Pts',(-17.4974567391075,17.4926460050014,
-7.62954102893509));
#108124=CARTESIAN_POINT('Ctrl Pts',(-17.6026931037089,17.417633166598,-7.637523314598));
#108125=CARTESIAN_POINT('Ctrl Pts',(-17.7058820850413,17.356549460309,-7.64539832406016));
#108126=CARTESIAN_POINT('Ctrl Pts',(-17.9117679230947,17.2571600545062,
-7.66050172347273));
#108127=CARTESIAN_POINT('Ctrl Pts',(-18.0133882175354,17.2174408067252,
-7.66770223878746));
#108128=CARTESIAN_POINT('Ctrl Pts',(-18.189357192284,17.1638859145967,-7.6795201694923));
#108129=CARTESIAN_POINT('Ctrl Pts',(-18.2622094568914,17.145878286301,-7.68423782880869));
#108130=CARTESIAN_POINT('Ctrl Pts',(-18.354336922749,17.1282377886458,-7.68998408675162));
#108131=CARTESIAN_POINT('Ctrl Pts',(-18.3728492830438,17.1249480647135,
-7.69112801922012));
#108132=CARTESIAN_POINT('Ctrl Pts',(-18.3998438808234,17.1205211447916,
-7.69278094959314));
#108133=CARTESIAN_POINT('Ctrl Pts',(-18.4082926746177,17.119188130447,-7.6932961380045));
#108134=CARTESIAN_POINT('Ctrl Pts',(-18.4231256089149,17.1169398998958,
-7.69419692106731));
#108135=CARTESIAN_POINT('Ctrl Pts',(-18.4295062413988,17.1160025913426,
-7.69458321121145));
#108136=CARTESIAN_POINT('Ctrl Pts',(-18.4419084710015,17.1142385734645,
-7.69533176838538));
#108137=CARTESIAN_POINT('Ctrl Pts',(-18.4479295348826,17.1134086119331,
-7.69569413478422));
#108138=CARTESIAN_POINT('Ctrl Pts',(-18.4623385252913,17.1114856292067,
-7.69655885604421));
#108139=CARTESIAN_POINT('Ctrl Pts',(-18.4707296339782,17.1104169220098,
-7.69706043993987));
#108140=CARTESIAN_POINT('Ctrl Pts',(-18.5010717403946,17.1067371647947,
-7.6988671635793));
#108141=CARTESIAN_POINT('Ctrl Pts',(-18.5230573802345,17.1044196148271,
-7.70016307062361));
#108142=CARTESIAN_POINT('Ctrl Pts',(-18.7299483776857,17.085882405688,-7.71224409602855));
#108143=CARTESIAN_POINT('Ctrl Pts',(-18.9161909189968,17.0937013233405,
-7.72217233217738));
#108144=CARTESIAN_POINT('Ctrl Pts',(-19.2068116659795,17.1445758292433,
-7.73825630792358));
#108145=CARTESIAN_POINT('Ctrl Pts',(-19.3129451810829,17.1717658806178,
-7.74428770586997));
#108146=CARTESIAN_POINT('Ctrl Pts',(-19.4276538344826,17.2108318754326,
-7.7514399859801));
#108147=CARTESIAN_POINT('Ctrl Pts',(-19.438788686742,17.214728209541,-7.75214113270838));
#108148=CARTESIAN_POINT('Ctrl Pts',(-19.4545988887945,17.2204093145448,
-7.75314726774578));
#108149=CARTESIAN_POINT('Ctrl Pts',(-19.4593016035648,17.2221179979071,
-7.75344788229311));
#108150=CARTESIAN_POINT('Ctrl Pts',(-19.4674057351831,17.2250951165373,
-7.75396831740386));
#108151=CARTESIAN_POINT('Ctrl Pts',(-19.4708100630542,17.2263556718151,
-7.7541876688923));
#108152=CARTESIAN_POINT('Ctrl Pts',(-19.4774126379573,17.2288198046164,
-7.75461453976269));
#108153=CARTESIAN_POINT('Ctrl Pts',(-19.4806112190219,17.2300223715317,
-7.75482199283272));
#108154=CARTESIAN_POINT('Ctrl Pts',(-19.4892507942977,17.2332944796223,
-7.75538408958011));
#108155=CARTESIAN_POINT('Ctrl Pts',(-19.4946861394802,17.235378709625,-7.75573959985214));
#108156=CARTESIAN_POINT('Ctrl Pts',(-19.514929688888,17.2432371974404,-7.75707052048708));
#108157=CARTESIAN_POINT('Ctrl Pts',(-19.5296808860076,17.2491555823059,
-7.75805405065918));
#108158=CARTESIAN_POINT('Ctrl Pts',(-19.6585622906279,17.3025572023171,
-7.76675921292675));
#108159=CARTESIAN_POINT('Ctrl Pts',(-19.7683864980642,17.3597819736637,
-7.77493889589455));
#108160=CARTESIAN_POINT('Ctrl Pts',(-20.0135027475799,17.5161539252156,
-7.7941521040843));
#108161=CARTESIAN_POINT('Ctrl Pts',(-20.1433088144144,17.6224472075079,
-7.80506970155752));
#108162=CARTESIAN_POINT('Ctrl Pts',(-20.2740376721806,17.7582693134469,
-7.81664817056723));
#108163=CARTESIAN_POINT('Ctrl Pts',(-20.2885731903803,17.7738344816468,
-7.81794610161462));
#108164=CARTESIAN_POINT('Ctrl Pts',(-20.3089101469849,17.7962816847784,
-7.81977788786208));
#108165=CARTESIAN_POINT('Ctrl Pts',(-20.3149060267143,17.8029850778136,
-7.82031996724489));
#108166=CARTESIAN_POINT('Ctrl Pts',(-20.3251770012896,17.8146163474709,
-7.82125213696267));
#108167=CARTESIAN_POINT('Ctrl Pts',(-20.329472334899,17.8195261107251,-7.82164307255232));
#108168=CARTESIAN_POINT('Ctrl Pts',(-20.3376537913389,17.8289655808528,
-7.82238985596887));
#108169=CARTESIAN_POINT('Ctrl Pts',(-20.3415435812567,17.8334920132112,
-7.82274585399512));
#108170=CARTESIAN_POINT('Ctrl Pts',(-20.3516099216603,17.845306620592,-7.82366965506387));
#108171=CARTESIAN_POINT('Ctrl Pts',(-20.3577564167394,17.8526203149127,
-7.82423621950626));
#108172=CARTESIAN_POINT('Ctrl Pts',(-20.3785534625371,17.8777095209664,
-7.82616204714698));
#108173=CARTESIAN_POINT('Ctrl Pts',(-20.3929636359234,17.8956828106609,
-7.82751157974486));
#108174=CARTESIAN_POINT('Ctrl Pts',(-20.514233917635,18.0521031367659,-7.83901212718583));
#108175=CARTESIAN_POINT('Ctrl Pts',(-20.6038503418906,18.2030609311729,
-7.84841818174308));
#108176=CARTESIAN_POINT('Ctrl Pts',(-20.6913710393355,18.4033523037698,
-7.86031012484889));
#108177=CARTESIAN_POINT('Ctrl Pts',(-20.7076100910747,18.4438903116821,
-7.86269368616636));
#108178=CARTESIAN_POINT('Ctrl Pts',(-20.72258060468,18.4848896924774,-7.86510589144174));
#108179=CARTESIAN_POINT('',(-20.8523540255571,19.2092594247491,-6.88905704671363));
#108180=CARTESIAN_POINT('Ctrl Pts',(-20.7249099383763,18.4840591618169,
-7.64456003119576));
#108181=CARTESIAN_POINT('Ctrl Pts',(-20.6989346215926,18.4111456946262,
-7.6398894877592));
#108182=CARTESIAN_POINT('Ctrl Pts',(-20.3954319387082,17.6922647742514,
-7.59282700876215));
#108183=CARTESIAN_POINT('Ctrl Pts',(-19.0148744805716,16.7235434527702,
-7.5033725942046));
#108184=CARTESIAN_POINT('Ctrl Pts',(-16.7944747214404,17.6284159605188,
-7.37619678752319));
#108185=CARTESIAN_POINT('Ctrl Pts',(-16.3534690248723,19.9852110982479,
-7.24902098084175));
#108186=CARTESIAN_POINT('Ctrl Pts',(-18.0964527455682,21.6317156062949,
-7.12184517416031));
#108187=CARTESIAN_POINT('Ctrl Pts',(-20.2927766547169,21.0898254884639,
-7.00185719611761));
#108188=CARTESIAN_POINT('Ctrl Pts',(-20.8471440721213,19.7934638825817,
-6.92426115363537));
#108189=CARTESIAN_POINT('Ctrl Pts',(-20.8523540255571,19.2092594247491,
-6.88905704671363));
#108190=CARTESIAN_POINT('Ctrl Pts',(-20.8509992391718,19.2092051891481,
-6.88983567993721));
#108191=CARTESIAN_POINT('Ctrl Pts',(-20.8509308802699,19.1285751086996,
-6.88542685664988));
#108192=CARTESIAN_POINT('Ctrl Pts',(-20.8462561258519,19.0480199742941,
-6.88096330535665));
#108193=CARTESIAN_POINT('Ctrl Pts',(-20.834275194884,18.9443612817674,-6.87493026745674));
#108194=CARTESIAN_POINT('Ctrl Pts',(-20.8311546079904,18.920837034468,-6.87354153241672));
#108195=CARTESIAN_POINT('Ctrl Pts',(-20.8267567249006,18.8914788094755,
-6.87177828995945));
#108196=CARTESIAN_POINT('Ctrl Pts',(-20.8258491620947,18.8855901323302,
-6.87142309733171));
#108197=CARTESIAN_POINT('Ctrl Pts',(-20.824284219736,18.8757132293002,-6.87082467057525));
#108198=CARTESIAN_POINT('Ctrl Pts',(-20.8236402485044,18.8717228727096,
-6.87058216746203));
#108199=CARTESIAN_POINT('Ctrl Pts',(-20.8224405319189,18.8644218499878,
-6.87013708432283));
#108200=CARTESIAN_POINT('Ctrl Pts',(-20.8218883302108,18.8611106037104,
-6.86993470344753));
#108201=CARTESIAN_POINT('Ctrl Pts',(-20.8207318334646,18.8542759683693,
-6.86951587247673));
#108202=CARTESIAN_POINT('Ctrl Pts',(-20.8201264940997,18.8507528216931,
-6.86929936162679));
#108203=CARTESIAN_POINT('Ctrl Pts',(-20.8187199415165,18.8426889554922,
-6.8688024187287));
#108204=CARTESIAN_POINT('Ctrl Pts',(-20.8179128176727,18.8381493228197,
-6.86852165476489));
#108205=CARTESIAN_POINT('Ctrl Pts',(-20.8153705414134,18.824116554734,-6.86765073281342));
#108206=CARTESIAN_POINT('Ctrl Pts',(-20.8135853303695,18.8146327756965,
-6.86705783825151));
#108207=CARTESIAN_POINT('Ctrl Pts',(-20.7945684265934,18.7172735616643,
-6.86092934697766));
#108208=CARTESIAN_POINT('Ctrl Pts',(-20.7718441214467,18.6305728922017,
-6.85512350878007));
#108209=CARTESIAN_POINT('Ctrl Pts',(-20.7369695777151,18.525244321258,-6.84783211541534));
#108210=CARTESIAN_POINT('Ctrl Pts',(-20.7299277512409,18.5050111446256,
-6.84642004455659));
#108211=CARTESIAN_POINT('Ctrl Pts',(-20.7225806151895,18.4848897212595,
-6.84500607926505));
#108212=CARTESIAN_POINT('Origin',(-18.734,19.211,0.));
#108213=CARTESIAN_POINT('',(-20.7225806138063,18.4848897174713,-6.04247212253779));
#108214=CARTESIAN_POINT('',(-20.7225804911066,18.4848893814367,-6.26710637686285));
#108215=CARTESIAN_POINT('',(-20.7225806137986,18.4848897174502,0.));
#108216=CARTESIAN_POINT('Ctrl Pts',(-20.7225804911066,18.4848893814367,
-6.26710637686285));
#108217=CARTESIAN_POINT('Ctrl Pts',(-20.7522829247855,18.5662346732453,
-6.27277686239517));
#108218=CARTESIAN_POINT('Ctrl Pts',(-20.7769957136057,18.6494073289697,
-6.27836339991924));
#108219=CARTESIAN_POINT('Ctrl Pts',(-20.8065479247142,18.7771762058336,
-6.2865811338612));
#108220=CARTESIAN_POINT('Ctrl Pts',(-20.8151860535273,18.8207141299219,
-6.2893203645065));
#108221=CARTESIAN_POINT('Ctrl Pts',(-20.8243855577728,18.8761611051668,
-6.29273465623541));
#108222=CARTESIAN_POINT('Ctrl Pts',(-20.8262235206868,18.8878442882777,
-6.29344996453055));
#108223=CARTESIAN_POINT('Ctrl Pts',(-20.8290114867732,18.9065880921723,
-6.29459112400719));
#108224=CARTESIAN_POINT('Ctrl Pts',(-20.8300239035339,18.913639045797,-6.29501894449509));
#108225=CARTESIAN_POINT('Ctrl Pts',(-20.8318772340533,18.9270264694107,
-6.2958285191774));
#108226=CARTESIAN_POINT('Ctrl Pts',(-20.8327250735366,18.9333618860314,
-6.29621048826961));
#108227=CARTESIAN_POINT('Ctrl Pts',(-20.8345859303218,18.9477627962086,
-6.29707616430485));
#108228=CARTESIAN_POINT('Ctrl Pts',(-20.835581216702,18.9558305101549,-6.29755930657332));
#108229=CARTESIAN_POINT('Ctrl Pts',(-20.8380346045802,18.9767062766664,
-6.29880485697251));
#108230=CARTESIAN_POINT('Ctrl Pts',(-20.8394222487224,18.989522390211,-6.2995650439401));
#108231=CARTESIAN_POINT('Ctrl Pts',(-20.8476032826374,19.0721247104989,
-6.3044370202131));
#108232=CARTESIAN_POINT('Ctrl Pts',(-20.85104361841,19.1422033440889,-6.30844168028271));
#108233=CARTESIAN_POINT('Ctrl Pts',(-20.8508787727464,19.4047165711849,
-6.3231406661448));
#108234=CARTESIAN_POINT('Ctrl Pts',(-20.8245352152959,19.5961656074274,
-6.3331749947728));
#108235=CARTESIAN_POINT('Ctrl Pts',(-20.759294768958,19.8293426961447,-6.34683371733216));
#108236=CARTESIAN_POINT('Ctrl Pts',(-20.744197911464,19.8767853283336,-6.34969721589345));
#108237=CARTESIAN_POINT('Ctrl Pts',(-20.7248154872869,19.9310025717403,
-6.35311512618809));
#108238=CARTESIAN_POINT('Ctrl Pts',(-20.7221455108881,19.9383427190911,
-6.35358099542427));
#108239=CARTESIAN_POINT('Ctrl Pts',(-20.7178168244118,19.9500409666448,
-6.35432874286635));
#108240=CARTESIAN_POINT('Ctrl Pts',(-20.7161841991077,19.9544087321618,
-6.35460910856059));
#108241=CARTESIAN_POINT('Ctrl Pts',(-20.7132689666539,19.9621299811691,
-6.35510688388085));
#108242=CARTESIAN_POINT('Ctrl Pts',(-20.7119922426185,19.9654856386655,
-6.35532393996009));
#108243=CARTESIAN_POINT('Ctrl Pts',(-20.7092701406778,19.972585833281,-6.35578476004516));
#108244=CARTESIAN_POINT('Ctrl Pts',(-20.7078226709785,19.9763294539083,
-6.35602864303979));
#108245=CARTESIAN_POINT('Ctrl Pts',(-20.7038921036952,19.9864098403162,
-6.35668776167519));
#108246=CARTESIAN_POINT('Ctrl Pts',(-20.7013891043818,19.9927387221509,
-6.35710416642735));
#108247=CARTESIAN_POINT('Ctrl Pts',(-20.6888792570119,20.0239294822189,
-6.35916872648583));
#108248=CARTESIAN_POINT('Ctrl Pts',(-20.6784319275977,20.0486106350645,
-6.36084135417825));
#108249=CARTESIAN_POINT('Ctrl Pts',(-20.6469617713902,20.1191931528088,
-6.36572421461722));
#108250=CARTESIAN_POINT('Ctrl Pts',(-20.6247626534134,20.1645478225075,
-6.36898505356392));
#108251=CARTESIAN_POINT('Ctrl Pts',(-20.5384183076348,20.3260626716198,
-6.38094758587727));
#108252=CARTESIAN_POINT('Ctrl Pts',(-20.4650106877013,20.4369262161604,
-6.38981579055469));
#108253=CARTESIAN_POINT('Ctrl Pts',(-20.3168836997383,20.6205484449742,
-6.40514171561398));
#108254=CARTESIAN_POINT('Ctrl Pts',(-20.2462642120733,20.6960623089784,
-6.41168265810236));
#108255=CARTESIAN_POINT('Ctrl Pts',(-20.1600892182026,20.7756583478519,
-6.41884330918656));
#108256=CARTESIAN_POINT('Ctrl Pts',(-20.1496786641039,20.7850839045917,
-6.41969611750575));
#108257=CARTESIAN_POINT('Ctrl Pts',(-20.1329049473183,20.7999695468413,
-6.4210510100854));
#108258=CARTESIAN_POINT('Ctrl Pts',(-20.1266019393969,20.8054965079818,
-6.42155589508113));
#108259=CARTESIAN_POINT('Ctrl Pts',(-20.1153950600402,20.8152064170283,
-6.42244619581993));
#108260=CARTESIAN_POINT('Ctrl Pts',(-20.1105046337667,20.8194046552351,
-6.42283224426577));
#108261=CARTESIAN_POINT('Ctrl Pts',(-20.1003178001555,20.8280691594151,
-6.42363134648645));
#108262=CARTESIAN_POINT('Ctrl Pts',(-20.0950184819654,20.8325318963423,
-6.4240442523738));
#108263=CARTESIAN_POINT('Ctrl Pts',(-20.081291059947,20.8439775228058,-6.4251067288252));
#108264=CARTESIAN_POINT('Ctrl Pts',(-20.0728304727572,20.8509212670814,
-6.42575470158249));
#108265=CARTESIAN_POINT('Ctrl Pts',(-20.0366931626524,20.8801136864495,
-6.42849390558301));
#108266=CARTESIAN_POINT('Ctrl Pts',(-20.0085118697073,20.9017305183268,
-6.4305597982846));
#108267=CARTESIAN_POINT('Ctrl Pts',(-19.9330683160028,20.9566416482939,
-6.43592260490661));
#108268=CARTESIAN_POINT('Ctrl Pts',(-19.8849623786337,20.9887277411595,
-6.43917558827396));
#108269=CARTESIAN_POINT('Ctrl Pts',(-19.6972065164932,21.103138197676,-6.45137510084861));
#108270=CARTESIAN_POINT('Ctrl Pts',(-19.5495978239829,21.1712929665874,
-6.45992613101447));
#108271=CARTESIAN_POINT('Ctrl Pts',(-19.3750774393533,21.2287161915827,
-6.47018702923805));
#108272=CARTESIAN_POINT('Ctrl Pts',(-19.3543836773646,21.2351746354237,
-6.4714067492847));
#108273=CARTESIAN_POINT('Ctrl Pts',(-19.2933193433325,21.2532082341672,
-6.47502442112291));
#108274=CARTESIAN_POINT('Ctrl Pts',(-19.2527016856321,21.2639005409562,
-6.47745420047644));
#108275=CARTESIAN_POINT('Ctrl Pts',(-19.2045508740802,21.2750557614865,
-6.48039068188202));
#108276=CARTESIAN_POINT('Ctrl Pts',(-19.1972969151105,21.2766960755133,
-6.48083455017466));
#108277=CARTESIAN_POINT('Ctrl Pts',(-19.1855407958701,21.2792894107184,
-6.48155652699095));
#108278=CARTESIAN_POINT('Ctrl Pts',(-19.1810438352741,21.2802660498957,
-6.48183331769278));
#108279=CARTESIAN_POINT('Ctrl Pts',(-19.1730488257041,21.2819751088501,
-6.48232657289057));
#108280=CARTESIAN_POINT('Ctrl Pts',(-19.1695520699089,21.2827133409351,
-6.48254270135557));
#108281=CARTESIAN_POINT('Ctrl Pts',(-19.1620432162948,21.2842787525061,
-6.48300767415887));
#108282=CARTESIAN_POINT('Ctrl Pts',(-19.1580306418605,21.2851031302024,
-6.48325666897805));
#108283=CARTESIAN_POINT('Ctrl Pts',(-19.1469792033555,21.2873402224293,
-6.48394384159974));
#108284=CARTESIAN_POINT('Ctrl Pts',(-19.1399355826728,21.2887287698348,
-6.4843833611645));
#108285=CARTESIAN_POINT('Ctrl Pts',(-19.1018130747293,21.2960428182941,
-6.48677006437656));
#108286=CARTESIAN_POINT('Ctrl Pts',(-19.0706131410091,21.3013065221611,
-6.4887515819924));
#108287=CARTESIAN_POINT('Ctrl Pts',(-18.8775474781523,21.3294441723526,
-6.50113876062034));
#108288=CARTESIAN_POINT('Ctrl Pts',(-18.7136045527413,21.3342040473118,
-6.51214901648214));
#108289=CARTESIAN_POINT('Ctrl Pts',(-18.4341372787239,21.309921658899,-6.53047401822961));
#108290=CARTESIAN_POINT('Ctrl Pts',(-18.3185530455791,21.2901347868,-6.53793076980914));
#108291=CARTESIAN_POINT('Ctrl Pts',(-18.1913415451304,21.2573174426433,
-6.54595263466364));
#108292=CARTESIAN_POINT('Ctrl Pts',(-18.1775384217965,21.2536071091668,
-6.54682080307756));
#108293=CARTESIAN_POINT('Ctrl Pts',(-18.1556307484283,21.2474796839016,
-6.54819535772543));
#108294=CARTESIAN_POINT('Ctrl Pts',(-18.1475014632004,21.2451533776193,
-6.54870467365861));
#108295=CARTESIAN_POINT('Ctrl Pts',(-18.1331892997412,21.2409648257023,
-6.54960011616502));
#108296=CARTESIAN_POINT('Ctrl Pts',(-18.1270006362122,21.2391228919689,
-6.549986899162));
#108297=CARTESIAN_POINT('Ctrl Pts',(-18.1142184291863,21.2352547721593,
-6.55078495567323));
#108298=CARTESIAN_POINT('Ctrl Pts',(-18.1076261601405,21.2332246147748,
-6.55119609396212));
#108299=CARTESIAN_POINT('Ctrl Pts',(-18.0907312374964,21.2279311068824,
-6.55224868361479));
#108300=CARTESIAN_POINT('Ctrl Pts',(-18.080443356312,21.2246209948174,-6.55288859436772));
#108301=CARTESIAN_POINT('Ctrl Pts',(-18.0376199801715,21.210479859638,-6.55554830669822));
#108302=CARTESIAN_POINT('Ctrl Pts',(-18.0053236369473,21.1989375733158,
-6.55754460104756));
#108303=CARTESIAN_POINT('Ctrl Pts',(-17.9219258491713,21.1668265721188,
-6.56268604595992));
#108304=CARTESIAN_POINT('Ctrl Pts',(-17.8713205893471,21.1450390082726,
-6.56579186038222));
#108305=CARTESIAN_POINT('Ctrl Pts',(-17.7229738117296,21.0741870079356,
-6.57493322723091));
#108306=CARTESIAN_POINT('Ctrl Pts',(-17.6281227950019,21.0195011125469,
-6.580820040185));
#108307=CARTESIAN_POINT('Ctrl Pts',(-17.5024504865063,20.9334467406348,
-6.58911240233665));
#108308=CARTESIAN_POINT('Ctrl Pts',(-17.4677299316055,20.9080848247028,
-6.59146229245138));
#108309=CARTESIAN_POINT('Ctrl Pts',(-17.3741856982365,20.8352849509247,
-6.59802420181248));
#108310=CARTESIAN_POINT('Ctrl Pts',(-17.3170978473414,20.7857324389769,
-6.60229302295449));
#108311=CARTESIAN_POINT('Ctrl Pts',(-17.2559602780968,20.7266443209607,
-6.6073321514166));
#108312=CARTESIAN_POINT('Ctrl Pts',(-17.2491784944956,20.7200010657329,
-6.60789803232228));
#108313=CARTESIAN_POINT('Ctrl Pts',(-17.2391914686884,20.7100855322071,
-6.60874209085317));
#108314=CARTESIAN_POINT('Ctrl Pts',(-17.2359516876903,20.7068479973701,
-6.60901759838665));
#108315=CARTESIAN_POINT('Ctrl Pts',(-17.2302041607973,20.7010670561246,
-6.60950944674124));
#108316=CARTESIAN_POINT('Ctrl Pts',(-17.227692320267,20.6985277918404,-6.60972545880299));
#108317=CARTESIAN_POINT('Ctrl Pts',(-17.2223034932822,20.6930524850478,
-6.61019118541858));
#108318=CARTESIAN_POINT('Ctrl Pts',(-17.2194286705741,20.6901144594914,
-6.61044105573938));
#108319=CARTESIAN_POINT('Ctrl Pts',(-17.2115115303713,20.681975978684,-6.61113305984481));
#108320=CARTESIAN_POINT('Ctrl Pts',(-17.2064873748197,20.6767580449853,
-6.6115765661542));
#108321=CARTESIAN_POINT('Ctrl Pts',(-17.1790222527096,20.6479390440077,
-6.61402463751384));
#108322=CARTESIAN_POINT('Ctrl Pts',(-17.1571027199689,20.6238497121559,
-6.61606561252066));
#108323=CARTESIAN_POINT('Ctrl Pts',(-17.0290696329091,20.4764507184679,
-6.62847227844776));
#108324=CARTESIAN_POINT('Ctrl Pts',(-16.9369045195771,20.3417523362035,
-6.63942738463181));
#108325=CARTESIAN_POINT('Ctrl Pts',(-16.8066265838216,20.0944949328792,
-6.65768271341527));
#108326=CARTESIAN_POINT('Ctrl Pts',(-16.7608185099317,19.9868184022987,
-6.66512287719615));
#108327=CARTESIAN_POINT('Ctrl Pts',(-16.7196357893792,19.862329416315,-6.67312930487364));
#108328=CARTESIAN_POINT('Ctrl Pts',(-16.7152852966763,19.8487179187452,
-6.67399727271548));
#108329=CARTESIAN_POINT('Ctrl Pts',(-16.7085806013527,19.8269843648363,
-6.67537157082266));
#108330=CARTESIAN_POINT('Ctrl Pts',(-16.7061367258244,19.8188906337728,
-6.67588082908637));
#108331=CARTESIAN_POINT('Ctrl Pts',(-16.7019120767193,19.8045902300333,
-6.67677620451176));
#108332=CARTESIAN_POINT('Ctrl Pts',(-16.700111102041,19.7983896843884,-6.67716297778781));
#108333=CARTESIAN_POINT('Ctrl Pts',(-16.6964447762704,19.7855479037243,
-6.67796104709484));
#108334=CARTESIAN_POINT('Ctrl Pts',(-16.6945834592252,19.7789055893083,
-6.67837220773847));
#108335=CARTESIAN_POINT('Ctrl Pts',(-16.6898890402123,19.7618322907801,
-6.67942492262433));
#108336=CARTESIAN_POINT('Ctrl Pts',(-16.6871032755738,19.7513884108513,
-6.68006493553586));
#108337=CARTESIAN_POINT('Ctrl Pts',(-16.6758102297431,19.7077099292253,
-6.68272564062173));
#108338=CARTESIAN_POINT('Ctrl Pts',(-16.6680311486553,19.6742912540351,
-6.68472280316241));
#108339=CARTESIAN_POINT('Ctrl Pts',(-16.6498821999752,19.5867375488995,
-6.68986698947393));
#108340=CARTESIAN_POINT('Ctrl Pts',(-16.6408076278669,19.5323596874423,
-6.69297462206998));
#108341=CARTESIAN_POINT('Ctrl Pts',(-16.6200900117121,19.3692101175599,
-6.70211916104053));
#108342=CARTESIAN_POINT('Ctrl Pts',(-16.6147400498285,19.2598264985895,
-6.70800733845812));
#108343=CARTESIAN_POINT('Ctrl Pts',(-16.6191737607425,19.1046963925756,
-6.71645672587226));
#108344=CARTESIAN_POINT('Ctrl Pts',(-16.6219714298163,19.0589291001994,
-6.71896329434194));
#108345=CARTESIAN_POINT('Ctrl Pts',(-16.628356127554,18.9908630336243,-6.72275443083819));
#108346=CARTESIAN_POINT('Ctrl Pts',(-16.6308175885516,18.968471453882,-6.72401191825206));
#108347=CARTESIAN_POINT('Ctrl Pts',(-16.6343250878182,18.9406583429107,
-6.72559123515573));
#108348=CARTESIAN_POINT('Ctrl Pts',(-16.6350356851202,18.9351954453078,
-6.72590227249363));
#108349=CARTESIAN_POINT('Ctrl Pts',(-16.6419010499118,18.8839798565246,
-6.72882665627511));
#108350=CARTESIAN_POINT('Ctrl Pts',(-16.6495290524978,18.8384407793363,
-6.73148942284214));
#108351=CARTESIAN_POINT('Ctrl Pts',(-16.6601486761626,18.7856904313191,
-6.73468473442779));
#108352=CARTESIAN_POINT('Ctrl Pts',(-16.6616993583049,18.7781979794171,
-6.73514121618079));
#108353=CARTESIAN_POINT('Ctrl Pts',(-16.6642506545308,18.7661989701166,
-6.73587672601004));
#108354=CARTESIAN_POINT('Ctrl Pts',(-16.6652254690867,18.7616869147515,
-6.73615431852071));
#108355=CARTESIAN_POINT('Ctrl Pts',(-16.6669833785169,18.7536772110023,
-6.73664895645544));
#108356=CARTESIAN_POINT('Ctrl Pts',(-16.667760607178,18.7501783227761,-6.73686566370459));
#108357=CARTESIAN_POINT('Ctrl Pts',(-16.6694328948811,18.7427393963541,
-6.73732777068667));
#108358=CARTESIAN_POINT('Ctrl Pts',(-16.6703303348727,18.7388000031049,
-6.73757329967693));
#108359=CARTESIAN_POINT('Ctrl Pts',(-16.6727967116562,18.7281149516898,
-6.73824142612402));
#108360=CARTESIAN_POINT('Ctrl Pts',(-16.6743874667519,18.7213744537036,
-6.73866524702791));
#108361=CARTESIAN_POINT('Ctrl Pts',(-16.682637001227,18.687170413667,-6.7408273809394));
#108362=CARTESIAN_POINT('Ctrl Pts',(-16.6898117975037,18.6598357774309,
-6.74259296999075));
#108363=CARTESIAN_POINT('Ctrl Pts',(-16.712457274106,18.5800965700325,-6.74783830432024));
#108364=CARTESIAN_POINT('Ctrl Pts',(-16.7294115317018,18.528139554758,-6.75137725606256));
#108365=CARTESIAN_POINT('Ctrl Pts',(-16.7969219262492,18.3455326422181,
-6.76412363157466));
#108366=CARTESIAN_POINT('Ctrl Pts',(-16.8584109970873,18.2192963971882,
-6.77348418486953));
#108367=CARTESIAN_POINT('Ctrl Pts',(-16.9794541901585,18.0229497807339,
-6.78837879912124));
#108368=CARTESIAN_POINT('Ctrl Pts',(-17.0318942637748,17.9489642843847,
-6.79408884258619));
#108369=CARTESIAN_POINT('Ctrl Pts',(-17.0975627644199,17.8678876773667,
-6.80045486775424));
#108370=CARTESIAN_POINT('Ctrl Pts',(-17.1063087585728,17.857301815866,-6.80128847572375));
#108371=CARTESIAN_POINT('Ctrl Pts',(-17.1205003442702,17.840461197254,-6.80261874543974));
#108372=CARTESIAN_POINT('Ctrl Pts',(-17.125880658652,17.8341521740186,-6.80311805040682));
#108373=CARTESIAN_POINT('Ctrl Pts',(-17.1354996762285,17.823006097242,-6.80400191373796));
#108374=CARTESIAN_POINT('Ctrl Pts',(-17.139723591022,17.8181564723982,-6.80438707506775));
#108375=CARTESIAN_POINT('Ctrl Pts',(-17.1485704758822,17.8080920243343,
-6.80518768537809));
#108376=CARTESIAN_POINT('Ctrl Pts',(-17.1531972341162,17.8028806225004,
-6.80560296985693));
#108377=CARTESIAN_POINT('Ctrl Pts',(-17.1652798908828,17.7894057926614,
-6.80667870921732));
#108378=CARTESIAN_POINT('Ctrl Pts',(-17.1727754322762,17.781178078439,-6.80733748840182));
#108379=CARTESIAN_POINT('Ctrl Pts',(-17.2056108239345,17.7457013580921,
-6.81018703159708));
#108380=CARTESIAN_POINT('Ctrl Pts',(-17.2316026522373,17.7190629900207,
-6.8123497891572));
#108381=CARTESIAN_POINT('Ctrl Pts',(-17.3025205197055,17.6501150062675,
-6.81802622880685));
#108382=CARTESIAN_POINT('Ctrl Pts',(-17.3486175935594,17.6090599543998,
-6.82148893816861));
#108383=CARTESIAN_POINT('Ctrl Pts',(-17.510474011078,17.4771271710602,-6.83304165867512));
#108384=CARTESIAN_POINT('Ctrl Pts',(-17.6338736056185,17.3963238434515,
-6.84084414466426));
#108385=CARTESIAN_POINT('Ctrl Pts',(-17.8276038252418,17.2965418731574,
-6.85294326235159));
#108386=CARTESIAN_POINT('Ctrl Pts',(-17.8921409447088,17.2672986072854,
-6.85695772225955));
#108387=CARTESIAN_POINT('Ctrl Pts',(-17.9667339813452,17.2379111281438,
-6.86171041364105));
#108388=CARTESIAN_POINT('Ctrl Pts',(-17.9754764715837,17.2345337369055,
-6.86226915901613));
#108389=CARTESIAN_POINT('Ctrl Pts',(-17.9885018949849,17.2296009146905,
-6.86310458630137));
#108390=CARTESIAN_POINT('Ctrl Pts',(-17.9927680260369,17.2280010288126,
-6.8633786768183));
#108391=CARTESIAN_POINT('Ctrl Pts',(-18.000385584567,17.2251723056559,-6.86386898060121));
#108392=CARTESIAN_POINT('Ctrl Pts',(-18.0037349863966,17.2239381610488,
-6.86408487314373));
#108393=CARTESIAN_POINT('Ctrl Pts',(-18.0109633788425,17.2212954806104,
-6.86455147327139));
#108394=CARTESIAN_POINT('Ctrl Pts',(-18.0148433157067,17.2198898340928,
-6.86480234262199));
#108395=CARTESIAN_POINT('Ctrl Pts',(-18.0256142362982,17.2160232703419,
-6.86549987114949));
#108396=CARTESIAN_POINT('Ctrl Pts',(-18.032513829831,17.2135867499298,-6.86594793840112));
#108397=CARTESIAN_POINT('Ctrl Pts',(-18.0712295120077,17.2001400417858,
-6.86846859594852));
#108398=CARTESIAN_POINT('Ctrl Pts',(-18.103290183334,17.1898549477508,-6.87058013347566));
#108399=CARTESIAN_POINT('Ctrl Pts',(-18.2043692895027,17.1600677288264,
-6.87728319908461));
#108400=CARTESIAN_POINT('Ctrl Pts',(-18.2741394099589,17.1433059507845,
-6.88197474973276));
#108401=CARTESIAN_POINT('Ctrl Pts',(-18.3753408009632,17.124368888511,-6.88876052556498));
#108402=CARTESIAN_POINT('Ctrl Pts',(-18.4061850192679,17.1193013758637,
-6.89082642451158));
#108403=CARTESIAN_POINT('Ctrl Pts',(-18.5985933373778,17.0920503959333,
-6.90366803488408));
#108404=CARTESIAN_POINT('Ctrl Pts',(-18.7621881789397,17.0879110161657,
-6.91432574939461));
#108405=CARTESIAN_POINT('Ctrl Pts',(-18.9482508918191,17.1047363139869,
-6.92583284203347));
#108406=CARTESIAN_POINT('Ctrl Pts',(-18.9718066771048,17.1072656499619,
-6.92727960971582));
#108407=CARTESIAN_POINT('Ctrl Pts',(-19.0049038406595,17.1113825439887,
-6.92929897342414));
#108408=CARTESIAN_POINT('Ctrl Pts',(-19.014483703288,17.112640819711,-6.92988188640347));
#108409=CARTESIAN_POINT('Ctrl Pts',(-19.0299862142399,17.1147850738926,
-6.93082269485222));
#108410=CARTESIAN_POINT('Ctrl Pts',(-19.0359142258081,17.1156306633781,
-6.93118186156488));
#108411=CARTESIAN_POINT('Ctrl Pts',(-19.0482764447246,17.1174475986493,
-6.93192966384728));
#108412=CARTESIAN_POINT('Ctrl Pts',(-19.054709929736,17.1184234820832,-6.93231815158711));
#108413=CARTESIAN_POINT('Ctrl Pts',(-19.0699338547895,17.1208046289212,
-6.93323588982979));
#108414=CARTESIAN_POINT('Ctrl Pts',(-19.0787201767533,17.1222357127958,
-6.93376431632037));
#108415=CARTESIAN_POINT('Ctrl Pts',(-19.1079652454826,17.1271886008144,
-6.93551924328855));
#108416=CARTESIAN_POINT('Ctrl Pts',(-19.1283815922944,17.1309559723268,
-6.9367379476779));
#108417=CARTESIAN_POINT('Ctrl Pts',(-19.2371590455703,17.1526875904462,
-6.94320143754973));
#108418=CARTESIAN_POINT('Ctrl Pts',(-19.3243649225639,17.1759837954818,
-6.94827249001944));
#108419=CARTESIAN_POINT('Ctrl Pts',(-19.5349343910049,17.246917277589,-6.96052633409362));
#108420=CARTESIAN_POINT('Ctrl Pts',(-19.6558194708651,17.3006691694042,
-6.96756063895633));
#108421=CARTESIAN_POINT('Ctrl Pts',(-19.8394367948869,17.4038262746204,
-6.97919951131585));
#108422=CARTESIAN_POINT('Ctrl Pts',(-19.9057603173634,17.4461084208513,
-6.98363193070267));
#108423=CARTESIAN_POINT('Ctrl Pts',(-19.9773035017372,17.4975309849909,
-6.98885340915815));
#108424=CARTESIAN_POINT('Ctrl Pts',(-19.984997480935,17.5031402405748,-6.98942094753584));
#108425=CARTESIAN_POINT('Ctrl Pts',(-19.9963403970242,17.511527508061,-6.99026700976626));
#108426=CARTESIAN_POINT('Ctrl Pts',(-20.0000186902265,17.5142658711791,
-6.99054284508725));
#108427=CARTESIAN_POINT('Ctrl Pts',(-20.0064228817851,17.5190659908539,
-6.99102572912091));
#108428=CARTESIAN_POINT('Ctrl Pts',(-20.0091527195476,17.5211224236487,
-6.9912324042085));
#108429=CARTESIAN_POINT('Ctrl Pts',(-20.0150418834089,17.525581225576,-6.99168010982486));
#108430=CARTESIAN_POINT('Ctrl Pts',(-20.0181993896464,17.5279858350976,
-6.99192129442607));
#108431=CARTESIAN_POINT('Ctrl Pts',(-20.0265812281815,17.5344063729837,
-6.99256454690003));
#108432=CARTESIAN_POINT('Ctrl Pts',(-20.0317935544019,17.5384378011236,
-6.99296768502342));
#108433=CARTESIAN_POINT('Ctrl Pts',(-20.0433747956963,17.5474819403293,
-6.99387024860555));
#108434=CARTESIAN_POINT('Ctrl Pts',(-20.0497338839925,17.5525069996192,
-6.9943704856369));
#108435=CARTESIAN_POINT('Ctrl Pts',(-20.0689204842056,17.5678483719936,
-6.9958935592754));
#108436=CARTESIAN_POINT('Ctrl Pts',(-20.0816563706499,17.578277658892,-6.99692337480648));
#108437=CARTESIAN_POINT('Ctrl Pts',(-20.1287027893391,17.6177289679715,
-7.00079427755288));
#108438=CARTESIAN_POINT('Ctrl Pts',(-20.1622064138246,17.6476912088858,
-7.00368541326625));
#108439=CARTESIAN_POINT('Ctrl Pts',(-20.248824004471,17.7302627623181,-7.01147319279298));
#108440=CARTESIAN_POINT('Ctrl Pts',(-20.3001487515164,17.7846578152127,
-7.01642138706372));
#108441=CARTESIAN_POINT('Ctrl Pts',(-20.4495444043509,17.9607981133953,
-7.031679511117));
#108442=CARTESIAN_POINT('Ctrl Pts',(-20.5371182239641,18.0907862353464,
-7.04186364993614));
#108443=CARTESIAN_POINT('Ctrl Pts',(-20.6206850155805,18.250437389378,-7.05296529491066));
#108444=CARTESIAN_POINT('Ctrl Pts',(-20.6314155510558,18.2718114262032,
-7.05442602382381));
#108445=CARTESIAN_POINT('Ctrl Pts',(-20.6459864025894,18.3021044725683,
-7.05646143602513));
#108446=CARTESIAN_POINT('Ctrl Pts',(-20.6501307560522,18.3108744453788,
-7.05704665600075));
#108447=CARTESIAN_POINT('Ctrl Pts',(-20.656738795033,18.3251103539889,-7.0579901865129));
#108448=CARTESIAN_POINT('Ctrl Pts',(-20.6592397583875,18.3305587397744,
-7.05834978263468));
#108449=CARTESIAN_POINT('Ctrl Pts',(-20.6644047567989,18.3419380081105,
-7.05909770203643));
#108450=CARTESIAN_POINT('Ctrl Pts',(-20.667064684467,18.3478706945424,-7.0594858808922));
#108451=CARTESIAN_POINT('Ctrl Pts',(-20.673289288512,18.361927120322,-7.06040150549724));
#108452=CARTESIAN_POINT('Ctrl Pts',(-20.6768303331593,18.3700612390023,
-7.06092813776373));
#108453=CARTESIAN_POINT('Ctrl Pts',(-20.6884167855165,18.3971402726274,
-7.0626708696102));
#108454=CARTESIAN_POINT('Ctrl Pts',(-20.6962371957432,18.4161806123037,
-7.06387932326408));
#108455=CARTESIAN_POINT('Ctrl Pts',(-20.7102536332852,18.4517748357084,
-7.06610874928887));
#108456=CARTESIAN_POINT('Ctrl Pts',(-20.7165212951111,18.4682952089492,
-7.06713179939855));
#108457=CARTESIAN_POINT('Ctrl Pts',(-20.7225806056755,18.4848896952038,
-7.06814847058112));
#108458=CARTESIAN_POINT('Ctrl Pts',(-20.7225806151895,18.4848897212595,
-6.84500607926505));
#108459=CARTESIAN_POINT('Ctrl Pts',(-20.7143220134754,18.4622720889823,
-6.84341670129537));
#108460=CARTESIAN_POINT('Ctrl Pts',(-20.7056776513276,18.4397956571551,
-6.84182493616512));
#108461=CARTESIAN_POINT('Ctrl Pts',(-20.6822899809051,18.3819505148498,
-6.83770208830836));
#108462=CARTESIAN_POINT('Ctrl Pts',(-20.6669669998539,18.346826663267,-6.83517292694144));
#108463=CARTESIAN_POINT('Ctrl Pts',(-20.6103477411035,18.2260939710641,
-6.8264140542921));
#108464=CARTESIAN_POINT('Ctrl Pts',(-20.5642446745063,18.1428573145741,
-6.82026493568266));
#108465=CARTESIAN_POINT('Ctrl Pts',(-20.4876289407121,18.0241504991971,
-6.81139913780444));
#108466=CARTESIAN_POINT('Ctrl Pts',(-20.4612924311316,17.986137729419,-6.80854276315538));
#108467=CARTESIAN_POINT('Ctrl Pts',(-20.4265842496443,17.9393902837932,
-6.80500504977845));
#108468=CARTESIAN_POINT('Ctrl Pts',(-20.4193562226583,17.9298258804877,
-6.80427984972165));
#108469=CARTESIAN_POINT('Ctrl Pts',(-20.4076826075114,17.9146486664867,
-6.80312668118412));
#108470=CARTESIAN_POINT('Ctrl Pts',(-20.4032891942628,17.9089962217928,
-6.80269666963867));
#108471=CARTESIAN_POINT('Ctrl Pts',(-20.3949230794441,17.8983445631575,
-6.80188527536604));
#108472=CARTESIAN_POINT('Ctrl Pts',(-20.3909562767742,17.8933408369608,
-6.80150366454686));
#108473=CARTESIAN_POINT('Ctrl Pts',(-20.381926168831,17.8820555183535,-6.80064192087892));
#108474=CARTESIAN_POINT('Ctrl Pts',(-20.3768494522396,17.8757847464745,
-6.80016233273327));
#108475=CARTESIAN_POINT('Ctrl Pts',(-20.3617613994614,17.8573642803901,
-6.79875117671033));
#108476=CARTESIAN_POINT('Ctrl Pts',(-20.351650110109,17.845296893096,-6.79782366284704));
#108477=CARTESIAN_POINT('Ctrl Pts',(-20.2603461998441,17.738766476022,-6.78960486120131));
#108478=CARTESIAN_POINT('Ctrl Pts',(-20.1710943863378,17.6515225211304,
-6.7826764506399));
#108479=CARTESIAN_POINT('Ctrl Pts',(-19.9449994152531,17.4665098406586,
-6.76672098599696));
#108480=CARTESIAN_POINT('Ctrl Pts',(-19.8032014748065,17.3761816864413,
-6.75786105594184));
#108481=CARTESIAN_POINT('Ctrl Pts',(-19.6328583142164,17.2941779716061,
-6.74686290809761));
#108482=CARTESIAN_POINT('Ctrl Pts',(-19.6133098192053,17.2851321129742,
-6.74559528639951));
#108483=CARTESIAN_POINT('Ctrl Pts',(-19.5878774508088,17.273831475815,-6.7439348128286));
#108484=CARTESIAN_POINT('Ctrl Pts',(-19.5821160421196,17.271302144944,-6.74355790950506));
#108485=CARTESIAN_POINT('Ctrl Pts',(-19.5732581848009,17.2674604431169,
-6.7429771770025));
#108486=CARTESIAN_POINT('Ctrl Pts',(-19.5701696836641,17.2661296779264,
-6.74277445606564));
#108487=CARTESIAN_POINT('Ctrl Pts',(-19.5637959026683,17.2634013487738,
-6.74235558845871));
#108488=CARTESIAN_POINT('Ctrl Pts',(-19.5605102829406,17.2620047465699,
-6.7421393841452));
#108489=CARTESIAN_POINT('Ctrl Pts',(-19.5530175758088,17.2588422121783,
-6.74164570564581));
#108490=CARTESIAN_POINT('Ctrl Pts',(-19.5488083187603,17.2570815726303,
-6.74136791603673));
#108491=CARTESIAN_POINT('Ctrl Pts',(-19.5378428223199,17.2525365418416,
-6.7406431409666));
#108492=CARTESIAN_POINT('Ctrl Pts',(-19.5310778652378,17.2497735283403,
-6.74019491368503));
#108493=CARTESIAN_POINT('Ctrl Pts',(-19.4877772395379,17.2323492767911,
-6.73731960983018));
#108494=CARTESIAN_POINT('Ctrl Pts',(-19.4508553833683,17.2186755495305,
-6.73483929506114));
#108495=CARTESIAN_POINT('Ctrl Pts',(-19.2328008268541,17.1447664450555,
-6.72011176022653));
#108496=CARTESIAN_POINT('Ctrl Pts',(-19.0445651574952,17.1082199585982,
-6.70718190373954));
#108497=CARTESIAN_POINT('Ctrl Pts',(-18.7989504908739,17.0942792503341,
-6.6913689942318));
#108498=CARTESIAN_POINT('Ctrl Pts',(-18.7438321414033,17.0933056291223,
-6.68787969213037));
#108499=CARTESIAN_POINT('Ctrl Pts',(-18.6544382366206,17.0952174711428,
-6.68232189017504));
#108500=CARTESIAN_POINT('Ctrl Pts',(-18.62016323703,17.0967844974204,-6.68021494757116));
#108501=CARTESIAN_POINT('Ctrl Pts',(-18.5751577141615,17.0999398508508,
-6.67747833512118));
#108502=CARTESIAN_POINT('Ctrl Pts',(-18.5643814100127,17.1007783609742,
-6.67682532216682));
#108503=CARTESIAN_POINT('Ctrl Pts',(-18.5467388892616,17.1022871557849,
-6.67575981217204));
#108504=CARTESIAN_POINT('Ctrl Pts',(-18.5398687887741,17.1029085272378,
-6.67534578563145));
#108505=CARTESIAN_POINT('Ctrl Pts',(-18.5265742260694,17.1041765053469,
-6.67454626925512));
#108506=CARTESIAN_POINT('Ctrl Pts',(-18.5201494520033,17.1048189456127,
-6.67416065306325));
#108507=CARTESIAN_POINT('Ctrl Pts',(-18.5053189933518,17.1063704656718,
-6.67327223785971));
#108508=CARTESIAN_POINT('Ctrl Pts',(-18.4969155784984,17.1073005300631,
-6.67277010488811));
#108509=CARTESIAN_POINT('Ctrl Pts',(-18.4743247514978,17.1099378982511,
-6.67142351508182));
#108510=CARTESIAN_POINT('Ctrl Pts',(-18.4601485262874,17.1117385643171,
-6.67058199951463));
#108511=CARTESIAN_POINT('Ctrl Pts',(-18.3302621524138,17.1295748725372,
-6.66290141150551));
#108512=CARTESIAN_POINT('Ctrl Pts',(-18.2160397733325,17.1550191451251,
-6.65637889965437));
#108513=CARTESIAN_POINT('Ctrl Pts',(-17.9491280413759,17.2381485870596,
-6.64107455735116));
#108514=CARTESIAN_POINT('Ctrl Pts',(-17.7998848724256,17.3042793139915,
-6.63247574464883));
#108515=CARTESIAN_POINT('Ctrl Pts',(-17.6316679018545,17.4033463694684,
-6.62126682880853));
#108516=CARTESIAN_POINT('Ctrl Pts',(-17.6040170937382,17.4205011666582,
-6.619369121449));
#108517=CARTESIAN_POINT('Ctrl Pts',(-17.57071039928,17.442243729078,-6.61700087346868));
#108518=CARTESIAN_POINT('Ctrl Pts',(-17.564666925745,17.4462332734673,-6.61656776808855));
#108519=CARTESIAN_POINT('Ctrl Pts',(-17.5552256638617,17.4525356251233,
-6.61588563279881));
#108520=CARTESIAN_POINT('Ctrl Pts',(-17.5518138742039,17.4548274980619,
-6.61563798963811));
#108521=CARTESIAN_POINT('Ctrl Pts',(-17.5454496171984,17.4591296435288,
-6.61517386531391));
#108522=CARTESIAN_POINT('Ctrl Pts',(-17.542495555898,17.4611374575784,-6.61495754968225));
#108523=CARTESIAN_POINT('Ctrl Pts',(-17.5357645335208,17.4657373403748,
-6.61446264424152));
#108524=CARTESIAN_POINT('Ctrl Pts',(-17.5319909088529,17.4683341892092,
-6.6141837327842));
#108525=CARTESIAN_POINT('Ctrl Pts',(-17.5204198562389,17.476352362637,-6.61332411128808));
#108526=CARTESIAN_POINT('Ctrl Pts',(-17.5126505815199,17.4818138384214,
-6.61274076420295));
#108527=CARTESIAN_POINT('Ctrl Pts',(-17.4068825182073,17.5572327798541,
-6.60471755657163));
#108528=CARTESIAN_POINT('Ctrl Pts',(-17.3150002233062,17.6353668714839,
-6.59679439738272));
#108529=CARTESIAN_POINT('Ctrl Pts',(-17.1537485064117,17.7980910068835,
-6.58165946836446));
#108530=CARTESIAN_POINT('Ctrl Pts',(-17.0832853054485,17.8810935801749,
-6.5744754061784));
#108531=CARTESIAN_POINT('Ctrl Pts',(-16.9757264633497,18.0295885239447,
-6.56269744811341));
#108532=CARTESIAN_POINT('Ctrl Pts',(-16.9351698668512,18.0923082771127,
-6.55800287880983));
#108533=CARTESIAN_POINT('Ctrl Pts',(-16.8886708917684,18.1733096987392,
-6.55228154797359));
#108534=CARTESIAN_POINT('Ctrl Pts',(-16.8795508992046,18.1896972794019,
-6.55114057520357));
#108535=CARTESIAN_POINT('Ctrl Pts',(-16.8665942314234,18.2137248621869,
-6.54949110757985));
#108536=CARTESIAN_POINT('Ctrl Pts',(-16.8625843571402,18.2212699863012,
-6.54897645862849));
#108537=CARTESIAN_POINT('Ctrl Pts',(-16.8556288987312,18.2345510365307,
-6.54807629759175));
#108538=CARTESIAN_POINT('Ctrl Pts',(-16.8526636557792,18.2402764895799,
-6.54769009297099));
#108539=CARTESIAN_POINT('Ctrl Pts',(-16.8469529201325,18.2514275476424,
-6.54694146807916));
#108540=CARTESIAN_POINT('Ctrl Pts',(-16.8442045577679,18.256851604484,-6.54657894953628));
#108541=CARTESIAN_POINT('Ctrl Pts',(-16.8376844453821,18.2698581216867,
-6.54571349320474));
#108542=CARTESIAN_POINT('Ctrl Pts',(-16.8339347305135,18.277451558483,-6.54521132939325));
#108543=CARTESIAN_POINT('Ctrl Pts',(-16.820534356187,18.3050034790034,-6.54340029987387));
#108544=CARTESIAN_POINT('Ctrl Pts',(-16.8111515678527,18.32509118537,-6.54210072537341));
#108545=CARTESIAN_POINT('Ctrl Pts',(-16.7264458176462,18.5141273633586,
-6.53005381234589));
#108546=CARTESIAN_POINT('Ctrl Pts',(-16.6732559435664,18.692111505969,-6.52015640957286));
#108547=CARTESIAN_POINT('Ctrl Pts',(-16.6310807936875,18.9542764684892,
-6.50568281724552));
#108548=CARTESIAN_POINT('Ctrl Pts',(-16.6228376561477,19.0344562683373,
-6.50125469187608));
#108549=CARTESIAN_POINT('Ctrl Pts',(-16.6175417613026,19.1510043347839,
-6.49458190957017));
#108550=CARTESIAN_POINT('Ctrl Pts',(-16.6168261179675,19.1871387822826,
-6.4924800688684));
#108551=CARTESIAN_POINT('Ctrl Pts',(-16.6170788824418,19.2307439697001,
-6.48988507322991));
#108552=CARTESIAN_POINT('Ctrl Pts',(-16.6171617641848,19.2382162068831,
-6.48943831376105));
#108553=CARTESIAN_POINT('Ctrl Pts',(-16.6173523789404,19.2498479094962,
-6.4887394121124));
#108554=CARTESIAN_POINT('Ctrl Pts',(-16.6174328179095,19.2540078460606,
-6.48848877116767));
#108555=CARTESIAN_POINT('Ctrl Pts',(-16.6176049653505,19.2617323563995,
-6.48802203975642));
#108556=CARTESIAN_POINT('Ctrl Pts',(-16.6176934163981,19.2652969453461,
-6.48780613339093));
#108557=CARTESIAN_POINT('Ctrl Pts',(-16.617914101094,19.2733682300484,-6.48731607123002));
#108558=CARTESIAN_POINT('Ctrl Pts',(-16.618051725722,19.2778747140442,-6.48704161856702));
#108559=CARTESIAN_POINT('Ctrl Pts',(-16.6185017589033,19.2912141579863,
-6.48622682442084));
#108560=CARTESIAN_POINT('Ctrl Pts',(-16.618855085394,19.3000455119049,-6.48568427695643));
#108561=CARTESIAN_POINT('Ctrl Pts',(-16.6218723043404,19.3652375790354,
-6.48165753514319));
#108562=CARTESIAN_POINT('Ctrl Pts',(-16.6267329986812,19.4214690410508,
-6.47806481547717));
#108563=CARTESIAN_POINT('Ctrl Pts',(-16.654862484207,19.6432002214296,-6.46359157221598));
#108564=CARTESIAN_POINT('Ctrl Pts',(-16.6954432956854,19.8058983258611,
-6.45234682466899));
#108565=CARTESIAN_POINT('Ctrl Pts',(-16.7754971229906,20.0168400066529,
-6.43780560662173));
#108566=CARTESIAN_POINT('Ctrl Pts',(-16.7985146582946,20.0706563838884,
-6.43409242974263));
#108567=CARTESIAN_POINT('Ctrl Pts',(-16.8391736067629,20.1557778306183,
-6.42822140406911));
#108568=CARTESIAN_POINT('Ctrl Pts',(-16.8554319310722,20.1877059261988,
-6.4260194916168));
#108569=CARTESIAN_POINT('Ctrl Pts',(-16.8777223982199,20.2288619811032,
-6.42317971533229));
#108570=CARTESIAN_POINT('Ctrl Pts',(-16.8830263732737,20.2384756385058,
-6.42251625139232));
#108571=CARTESIAN_POINT('Ctrl Pts',(-16.8918025091519,20.2540941987987,
-6.4214380561763));
#108572=CARTESIAN_POINT('Ctrl Pts',(-16.8952297634089,20.2601239782134,
-6.42102172455256));
#108573=CARTESIAN_POINT('Ctrl Pts',(-16.9018975938012,20.2717220549832,
-6.42022073097131));
#108574=CARTESIAN_POINT('Ctrl Pts',(-16.9051340726756,20.2772926080656,
-6.41983592702379));
#108575=CARTESIAN_POINT('Ctrl Pts',(-16.91263135217,20.29006219788,-6.41895358075498));
#108576=CARTESIAN_POINT('Ctrl Pts',(-16.9169095128342,20.297250957518,-6.41845667524244));
#108577=CARTESIAN_POINT('Ctrl Pts',(-16.9284521998043,20.3163875602612,
-6.41713329240401));
#108578=CARTESIAN_POINT('Ctrl Pts',(-16.9357927533133,20.3282892325262,
-6.41630959801596));
#108579=CARTESIAN_POINT('Ctrl Pts',(-16.9968745760143,20.4251633150974,
-6.40959772715613));
#108580=CARTESIAN_POINT('Ctrl Pts',(-17.0564919467087,20.5062867489956,
-6.40393904103445));
#108581=CARTESIAN_POINT('Ctrl Pts',(-17.2327398687421,20.7134283558584,
-6.38895543931456));
#108582=CARTESIAN_POINT('Ctrl Pts',(-17.3592547165705,20.8299925173283,
-6.37994389051388));
#108583=CARTESIAN_POINT('Ctrl Pts',(-17.5308108760238,20.9533019762175,
-6.36790651871291));
#108584=CARTESIAN_POINT('Ctrl Pts',(-17.5638514432103,20.975662045985,-6.36559298713685));
#108585=CARTESIAN_POINT('Ctrl Pts',(-17.6039858000269,21.0011999835059,
-6.36276336840678));
#108586=CARTESIAN_POINT('Ctrl Pts',(-17.6104925632376,21.0052906978873,
-6.36230402440016));
#108587=CARTESIAN_POINT('Ctrl Pts',(-17.6205951005058,21.0115655302254,
-6.36158968850719));
#108588=CARTESIAN_POINT('Ctrl Pts',(-17.624175429748,21.0137745620049,-6.36133630688304));
#108589=CARTESIAN_POINT('Ctrl Pts',(-17.630799218448,21.0178341714007,-6.36086708381862));
#108590=CARTESIAN_POINT('Ctrl Pts',(-17.6338407731781,21.0196877459752,
-6.36065144311388));
#108591=CARTESIAN_POINT('Ctrl Pts',(-17.640691805315,21.0238392051238,-6.36016531637365));
#108592=CARTESIAN_POINT('Ctrl Pts',(-17.6445038316379,21.0261327473458,
-6.35989455408282));
#108593=CARTESIAN_POINT('Ctrl Pts',(-17.6542761337772,21.0319704717892,
-6.35919980170283));
#108594=CARTESIAN_POINT('Ctrl Pts',(-17.6602465925175,21.0354973837458,
-6.35877473024137));
#108595=CARTESIAN_POINT('Ctrl Pts',(-17.6952237161171,21.0559281728967,
-6.35628146000999));
#108596=CARTESIAN_POINT('Ctrl Pts',(-17.7246101391587,21.0721684361755,
-6.35417456947352));
#108597=CARTESIAN_POINT('Ctrl Pts',(-17.770557674362,21.0961528847494,-6.35087603535773));
#108598=CARTESIAN_POINT('Ctrl Pts',(-17.7868553396699,21.1043936384059,
-6.34970522002475));
#108599=CARTESIAN_POINT('Ctrl Pts',(-17.8254409867647,21.1232812451234,
-6.34693460951328));
#108600=CARTESIAN_POINT('Ctrl Pts',(-17.8478126038333,21.1337508609787,
-6.34532929755426));
#108601=CARTESIAN_POINT('Ctrl Pts',(-17.9113735152393,21.1621515713041,
-6.34078043255332));
#108602=CARTESIAN_POINT('Ctrl Pts',(-17.9529573742445,21.1791664119522,
-6.33781864804257));
#108603=CARTESIAN_POINT('Ctrl Pts',(-18.0975169317308,21.2330124952325,
-6.32762842442968));
#108604=CARTESIAN_POINT('Ctrl Pts',(-18.2027949927039,21.2631866226279,
-6.32039839227555));
#108605=CARTESIAN_POINT('Ctrl Pts',(-18.3638784422062,21.2961211313912,
-6.30983055555864));
#108606=CARTESIAN_POINT('Ctrl Pts',(-18.4182309585997,21.3050417454674,
-6.30634435451977));
#108607=CARTESIAN_POINT('Ctrl Pts',(-18.5068944692338,21.3160623261965,
-6.3007909136273));
#108608=CARTESIAN_POINT('Ctrl Pts',(-18.5410147437896,21.3194641865828,
-6.29868530619467));
#108609=CARTESIAN_POINT('Ctrl Pts',(-18.5859799012722,21.3228465432972,
-6.29595014797637));
#108610=CARTESIAN_POINT('Ctrl Pts',(-18.5967617714073,21.3235746016313,
-6.29529728509838));
#108611=CARTESIAN_POINT('Ctrl Pts',(-18.6144340882067,21.3246320796817,
-6.29423195721404));
#108612=CARTESIAN_POINT('Ctrl Pts',(-18.6213213086204,21.3250104280214,
-6.29381796371635));
#108613=CARTESIAN_POINT('Ctrl Pts',(-18.6346591958927,21.3256777761072,
-6.29301846778467));
#108614=CARTESIAN_POINT('Ctrl Pts',(-18.6411095693651,21.325970936312,-6.29263283922168));
#108615=CARTESIAN_POINT('Ctrl Pts',(-18.6560100725481,21.326579843261,-6.29174433354024));
#108616=CARTESIAN_POINT('Ctrl Pts',(-18.6644609907015,21.3268744838357,
-6.29124212289746));
#108617=CARTESIAN_POINT('Ctrl Pts',(-18.68720167596,21.3275309442009,-6.28989518723335));
#108618=CARTESIAN_POINT('Ctrl Pts',(-18.7014938729718,21.3277986884734,
-6.2890534058719));
#108619=CARTESIAN_POINT('Ctrl Pts',(-18.8329520787702,21.328929634035,-6.28135190565202));
#108620=CARTESIAN_POINT('Ctrl Pts',(-18.9500047707518,21.3202094924316,
-6.27481081589188));
#108621=CARTESIAN_POINT('Ctrl Pts',(-19.227594783444,21.2761651349409,-6.25942589144886));
#108622=CARTESIAN_POINT('Ctrl Pts',(-19.3858920386363,21.2317838238735,
-6.25076847213039));
#108623=CARTESIAN_POINT('Ctrl Pts',(-19.5663317561777,21.1577630041048,
-6.23955367023813));
#108624=CARTESIAN_POINT('Ctrl Pts',(-19.5949289670148,21.1452862837592,
-6.23773215292194));
#108625=CARTESIAN_POINT('Ctrl Pts',(-19.6297251086953,21.129180550204,-6.2354487192003));
#108626=CARTESIAN_POINT('Ctrl Pts',(-19.6361965599818,21.126145283619,-6.23502114721715));
#108627=CARTESIAN_POINT('Ctrl Pts',(-19.646346070374,21.1213220597708,-6.2343458117799));
#108628=CARTESIAN_POINT('Ctrl Pts',(-19.6500346006386,21.1195560861436,
-6.23409938980113));
#108629=CARTESIAN_POINT('Ctrl Pts',(-19.6569379777609,21.1162263041503,
-6.23363628738182));
#108630=CARTESIAN_POINT('Ctrl Pts',(-19.6601539882115,21.1146650362561,
-6.23341976477569));
#108631=CARTESIAN_POINT('Ctrl Pts',(-19.6675103803381,21.1110706949841,
-6.23292270314923));
#108632=CARTESIAN_POINT('Ctrl Pts',(-19.671648069908,21.1090322368717,-6.23264183161785));
#108633=CARTESIAN_POINT('Ctrl Pts',(-19.6824718198024,21.103655819941,-6.23190377325335));
#108634=CARTESIAN_POINT('Ctrl Pts',(-19.6891468576182,21.1002959858926,
-6.23144527038847));
#108635=CARTESIAN_POINT('Ctrl Pts',(-19.7338277752976,21.0775088511716,
-6.2283544045501));
#108636=CARTESIAN_POINT('Ctrl Pts',(-19.771253658907,21.0569726842075,-6.2256594437529));
#108637=CARTESIAN_POINT('Ctrl Pts',(-19.8142373859244,21.0316669306559,
-6.22246032614407));
#108638=CARTESIAN_POINT('Ctrl Pts',(-19.8204257537986,21.0279810020234,
-6.22199716670866));
#108639=CARTESIAN_POINT('Ctrl Pts',(-19.9612667849399,20.9431162177966,
-6.21139892056264));
#108640=CARTESIAN_POINT('Ctrl Pts',(-20.0864795940046,20.8472189992898,
-6.20082566701259));
#108641=CARTESIAN_POINT('Ctrl Pts',(-20.2683631239063,20.6726489957371,
-6.18444653877917));
#108642=CARTESIAN_POINT('Ctrl Pts',(-20.3323175750643,20.6024284380669,
-6.17842091286517));
#108643=CARTESIAN_POINT('Ctrl Pts',(-20.4046232442814,20.5114468131507,
-6.17128283460061));
#108644=CARTESIAN_POINT('Ctrl Pts',(-20.4176410418737,20.4945485314317,
-6.16998278769079));
#108645=CARTESIAN_POINT('Ctrl Pts',(-20.435785262638,20.4702445777675,-6.16814856148964));
#108646=CARTESIAN_POINT('Ctrl Pts',(-20.4411229320124,20.462998916004,-6.16760612817427));
#108647=CARTESIAN_POINT('Ctrl Pts',(-20.4502504309371,20.4504418205428,
-6.16667354115692));
#108648=CARTESIAN_POINT('Ctrl Pts',(-20.4540621751653,20.4451465404267,
-6.16628254019508));
#108649=CARTESIAN_POINT('Ctrl Pts',(-20.4613129507941,20.4349749073252,
-6.16553576202989));
#108650=CARTESIAN_POINT('Ctrl Pts',(-20.4647559590963,20.4301014785153,
-6.16517983400147));
#108651=CARTESIAN_POINT('Ctrl Pts',(-20.4736538398603,20.4173932423729,
-6.16425649597891));
#108652=CARTESIAN_POINT('Ctrl Pts',(-20.4790764412075,20.4095359221416,
-6.16369032208042));
#108653=CARTESIAN_POINT('Ctrl Pts',(-20.4973780625558,20.3826294352831,
-6.16176726432045));
#108654=CARTESIAN_POINT('Ctrl Pts',(-20.5100000826025,20.3634068260241,
-6.16042007253108));
#108655=CARTESIAN_POINT('Ctrl Pts',(-20.6162011446523,20.1957782924256,
-6.14888912527794));
#108656=CARTESIAN_POINT('Ctrl Pts',(-20.6913089129596,20.0364804387942,
-6.1394558683824));
#108657=CARTESIAN_POINT('Ctrl Pts',(-20.7729859957996,19.7870200369861,
-6.12517356199045));
#108658=CARTESIAN_POINT('Ctrl Pts',(-20.7949379458987,19.7027269166773,
-6.12040921269416));
#108659=CARTESIAN_POINT('Ctrl Pts',(-20.8189001284145,19.5802038973624,
-6.11328134095437));
#108660=CARTESIAN_POINT('Ctrl Pts',(-20.8251640445067,19.542892456784,-6.11108394711787));
#108661=CARTESIAN_POINT('Ctrl Pts',(-20.8314778225086,19.4979374848787,
-6.10838299811422));
#108662=CARTESIAN_POINT('Ctrl Pts',(-20.8324907016688,19.4904335470698,
-6.10793037519611));
#108663=CARTESIAN_POINT('Ctrl Pts',(-20.8340004990705,19.4787767650944,
-6.1072242799401));
#108664=CARTESIAN_POINT('Ctrl Pts',(-20.8345254153759,19.4746275226261,
-6.10697235921564));
#108665=CARTESIAN_POINT('Ctrl Pts',(-20.8354748337342,19.4669398830099,
-6.10650447622598));
#108666=CARTESIAN_POINT('Ctrl Pts',(-20.8359026977808,19.4634019592107,
-6.10628870586585));
#108667=CARTESIAN_POINT('Ctrl Pts',(-20.836848273436,19.4554140124471,-6.1058005355452));
#108668=CARTESIAN_POINT('Ctrl Pts',(-20.8373607907553,19.4509634422841,
-6.10552784856523));
#108669=CARTESIAN_POINT('Ctrl Pts',(-20.8388276186781,19.4378600411612,
-6.10472301637945));
#108670=CARTESIAN_POINT('Ctrl Pts',(-20.8397426748065,19.4292030342257,
-6.10418874306042));
#108671=CARTESIAN_POINT('Ctrl Pts',(-20.8458591846126,19.367711116328,-6.10037684633282));
#108672=CARTESIAN_POINT('Ctrl Pts',(-20.8491244446042,19.3147070409703,
-6.0970030715376));
#108673=CARTESIAN_POINT('Ctrl Pts',(-20.8507874983554,19.2452051698429,
-6.09251070877059));
#108674=CARTESIAN_POINT('Ctrl Pts',(-20.8509892979952,19.2287651387287,
-6.09144303796163));
#108675=CARTESIAN_POINT('Ctrl Pts',(-20.8510113338403,19.1935501678798,
-6.08914730328518));
#108676=CARTESIAN_POINT('Ctrl Pts',(-20.8507733287336,19.1747765698913,
-6.08791808606016));
#108677=CARTESIAN_POINT('Ctrl Pts',(-20.8462294574967,18.9999094588411,
-6.076431256371));
#108678=CARTESIAN_POINT('Ctrl Pts',(-20.8249133169856,18.8447155084867,
-6.06600952224626));
#108679=CARTESIAN_POINT('Ctrl Pts',(-20.7855431282212,18.6886181110422,
-6.05574908623547));
#108680=CARTESIAN_POINT('Ctrl Pts',(-20.7843532949711,18.6839673528277,
-6.05544354651447));
#108681=CARTESIAN_POINT('Ctrl Pts',(-20.7672425722882,18.6180208430043,
-6.05111338419313));
#108682=CARTESIAN_POINT('Ctrl Pts',(-20.7485937396552,18.5574611490693,
-6.04716677887305));
#108683=CARTESIAN_POINT('Ctrl Pts',(-20.7257113393618,18.4935071735124,
-6.04302921523241));
#108684=CARTESIAN_POINT('Ctrl Pts',(-20.7241529735247,18.4891959008834,
-6.0427504354363));
#108685=CARTESIAN_POINT('Ctrl Pts',(-20.7225806138063,18.4848897174713,
-6.04247212253779));
#108686=CARTESIAN_POINT('Origin',(-18.734,19.211,0.));
#108687=CARTESIAN_POINT('',(-20.7225806829213,18.484889906755,-5.2445270986103));
#108688=CARTESIAN_POINT('',(-20.7225806137986,18.4848897174502,-5.46434831804488));
#108689=CARTESIAN_POINT('',(-20.7225806137986,18.4848897174502,0.));
#108690=CARTESIAN_POINT('',(-20.8509993557837,19.2093484518076,-5.51218501636556));
#108691=CARTESIAN_POINT('Ctrl Pts',(-20.7225806137986,18.4848897174502,
-5.46434831804488));
#108692=CARTESIAN_POINT('Ctrl Pts',(-20.7233024841825,18.4868666863565,
-5.46447496720223));
#108693=CARTESIAN_POINT('Ctrl Pts',(-20.7240214029106,18.4888447221103,
-5.46460179002157));
#108694=CARTESIAN_POINT('Ctrl Pts',(-20.7259509440324,18.4941784303195,
-5.46494405560274));
#108695=CARTESIAN_POINT('Ctrl Pts',(-20.7271560109878,18.4975360262837,
-5.46515982705691));
#108696=CARTESIAN_POINT('Ctrl Pts',(-20.7297430820435,18.5048019154282,
-5.4656274508845));
#108697=CARTESIAN_POINT('Ctrl Pts',(-20.7311220758324,18.5087111721524,
-5.46587947189699));
#108698=CARTESIAN_POINT('Ctrl Pts',(-20.7349315291103,18.5196124017892,
-5.46658338460756));
#108699=CARTESIAN_POINT('Ctrl Pts',(-20.7373367833058,18.5266130304581,
-5.46703672596418));
#108700=CARTESIAN_POINT('Ctrl Pts',(-20.7509022232985,18.5667803152235,
-5.46964468032722));
#108701=CARTESIAN_POINT('Ctrl Pts',(-20.7612746976398,18.6002049846049,
-5.47184140961292));
#108702=CARTESIAN_POINT('Ctrl Pts',(-20.7916316012822,18.7073407034207,
-5.47893320443435));
#108703=CARTESIAN_POINT('Ctrl Pts',(-20.8084577951946,18.7818802512658,
-5.48394075702676));
#108704=CARTESIAN_POINT('Ctrl Pts',(-20.8409451160576,18.9735153717483,
-5.49676495883049));
#108705=CARTESIAN_POINT('Ctrl Pts',(-20.8509072796362,19.0913227436705,
-5.50459118708685));
#108706=CARTESIAN_POINT('Ctrl Pts',(-20.8509993557837,19.2093484518076,
-5.51218501636556));
#108707=CARTESIAN_POINT('Ctrl Pts',(-20.8509993578191,19.2093510629101,
-5.51218518436507));
#108708=CARTESIAN_POINT('Ctrl Pts',(-20.8510649772347,19.2935970062879,
-5.51760560536095));
#108709=CARTESIAN_POINT('Ctrl Pts',(-20.8461018019886,19.377781816377,-5.52290050009876));
#108710=CARTESIAN_POINT('Ctrl Pts',(-20.8349011953471,19.4717899931963,
-5.52867288887937));
#108711=CARTESIAN_POINT('Ctrl Pts',(-20.8335940955098,19.4821123260401,
-5.52930486670546));
#108712=CARTESIAN_POINT('Ctrl Pts',(-20.8312616515329,19.4995022658,-5.53036653139996));
#108713=CARTESIAN_POINT('Ctrl Pts',(-20.8302765594365,19.5065750000842,
-5.5307974806336));
#108714=CARTESIAN_POINT('Ctrl Pts',(-20.8283990631231,19.5195732817317,
-5.53158796381311));
#108715=CARTESIAN_POINT('Ctrl Pts',(-20.8275172536352,19.5255002634194,
-5.53194782910823));
#108716=CARTESIAN_POINT('Ctrl Pts',(-20.8256463308097,19.5377188201829,
-5.53268852674375));
#108717=CARTESIAN_POINT('Ctrl Pts',(-20.824653966422,19.5440098417555,-5.53306925197143));
#108718=CARTESIAN_POINT('Ctrl Pts',(-20.8223696977555,19.5580780266519,
-5.53391924827786));
#108719=CARTESIAN_POINT('Ctrl Pts',(-20.8210627052719,19.5658526707286,
-5.53438803530431));
#108720=CARTESIAN_POINT('Ctrl Pts',(-20.8176411998699,19.5855324390729,
-5.53557234197291));
#108721=CARTESIAN_POINT('Ctrl Pts',(-20.8154680491618,19.5974271821816,
-5.53628599504366));
#108722=CARTESIAN_POINT('Ctrl Pts',(-20.8024833895109,19.6652088085229,
-5.54034128987405));
#108723=CARTESIAN_POINT('Ctrl Pts',(-20.7895226757927,19.7206631593222,
-5.54361373169995));
#108724=CARTESIAN_POINT('Ctrl Pts',(-20.7635221396755,19.8146348325442,
-5.54912154478234));
#108725=CARTESIAN_POINT('Ctrl Pts',(-20.7515806173787,19.8534202691554,
-5.55138379417188));
#108726=CARTESIAN_POINT('Ctrl Pts',(-20.7078178717039,19.9822667105859,
-5.55890208225654));
#108727=CARTESIAN_POINT('Ctrl Pts',(-20.6710200248754,20.0705133733609,
-5.56405154180234));
#108728=CARTESIAN_POINT('Ctrl Pts',(-20.5903959124699,20.2321406065725,
-5.57388370684294));
#108729=CARTESIAN_POINT('Ctrl Pts',(-20.5478456863164,20.305940848901,-5.57854916575188));
#108730=CARTESIAN_POINT('Ctrl Pts',(-20.4804070699152,20.4081406417986,
-5.58554356811992));
#108731=CARTESIAN_POINT('Ctrl Pts',(-20.4590211132936,20.4387561417503,
-5.58771340802182));
#108732=CARTESIAN_POINT('Ctrl Pts',(-20.4323561989831,20.47485605703,-5.59038381356568));
#108733=CARTESIAN_POINT('Ctrl Pts',(-20.4278417190277,20.4809000506001,
-5.59083477774178));
#108734=CARTESIAN_POINT('Ctrl Pts',(-20.4207780787938,20.4902521854258,
-5.59153883837267));
#108735=CARTESIAN_POINT('Ctrl Pts',(-20.4182512182753,20.4935772000399,
-5.59179039754004));
#108736=CARTESIAN_POINT('Ctrl Pts',(-20.4135495530391,20.4997261164267,
-5.59225795300536));
#108737=CARTESIAN_POINT('Ctrl Pts',(-20.4113774491847,20.5025520108197,
-5.59247375959621));
#108738=CARTESIAN_POINT('Ctrl Pts',(-20.4064541892731,20.5089237753775,
-5.59296245445069));
#108739=CARTESIAN_POINT('Ctrl Pts',(-20.4036989032278,20.5124663705257,
-5.59323563247517));
#108740=CARTESIAN_POINT('Ctrl Pts',(-20.3955433323692,20.5228838294314,
-5.59404322936797));
#108741=CARTESIAN_POINT('Ctrl Pts',(-20.3901117798278,20.5297339359879,
-5.59457979782281));
#108742=CARTESIAN_POINT('Ctrl Pts',(-20.3510460038105,20.5783805005251,
-5.59842869908015));
#108743=CARTESIAN_POINT('Ctrl Pts',(-20.31587891269,20.6189152196025,-5.60183917827301));
#108744=CARTESIAN_POINT('Ctrl Pts',(-20.2701324030142,20.6677644838475,
-5.60616539159853));
#108745=CARTESIAN_POINT('Ctrl Pts',(-20.2609597733075,20.6773762685511,
-5.60702766373061));
#108746=CARTESIAN_POINT('Ctrl Pts',(-20.1456055252199,20.7959972692869,
-5.61780141355003));
#108747=CARTESIAN_POINT('Ctrl Pts',(-20.0280577798011,20.8933396221013,
-5.62800596734606));
#108748=CARTESIAN_POINT('Ctrl Pts',(-19.8498064431852,21.0111227154827,
-5.64180605232577));
#108749=CARTESIAN_POINT('Ctrl Pts',(-19.7970787269455,21.0427561362285,
-5.64571421651713));
#108750=CARTESIAN_POINT('Ctrl Pts',(-19.7214392817925,21.0837671247593,
-5.65107488895773));
#108751=CARTESIAN_POINT('Ctrl Pts',(-19.6996304608007,21.0951048089231,
-5.65259330477595));
#108752=CARTESIAN_POINT('Ctrl Pts',(-19.661171483041,21.1142551123886,-5.65522440798555));
#108753=CARTESIAN_POINT('Ctrl Pts',(-19.6446081145374,21.1222351705132,
-5.65634279822551));
#108754=CARTESIAN_POINT('Ctrl Pts',(-19.6202911421272,21.1335629400343,
-5.65796373567001));
#108755=CARTESIAN_POINT('Ctrl Pts',(-19.6126184753653,21.1370814689355,
-5.65847217363576));
#108756=CARTESIAN_POINT('Ctrl Pts',(-19.5993943819441,21.1430503050897,
-5.65934338313637));
#108757=CARTESIAN_POINT('Ctrl Pts',(-19.5938531312243,21.1455227865318,
-5.65970691439905));
#108758=CARTESIAN_POINT('Ctrl Pts',(-19.5828196169244,21.1503891181994,
-5.66042776097299));
#108759=CARTESIAN_POINT('Ctrl Pts',(-19.577327670893,21.1527835447104,-5.66078509342141));
#108760=CARTESIAN_POINT('Ctrl Pts',(-19.5629365444683,21.1589853425098,
-5.6617176544521));
#108761=CARTESIAN_POINT('Ctrl Pts',(-19.5540212214647,21.1627550795279,
-5.66229159681302));
#108762=CARTESIAN_POINT('Ctrl Pts',(-19.523102918332,21.1755792635213,-5.66426925577876));
#108763=CARTESIAN_POINT('Ctrl Pts',(-19.5009728627888,21.1843240467543,
-5.66566250928614));
#108764=CARTESIAN_POINT('Ctrl Pts',(-19.3287272854687,21.2490520867295,
-5.67634629520721));
#108765=CARTESIAN_POINT('Ctrl Pts',(-19.1728412039705,21.2882053888621,
-5.68502830292001));
#108766=CARTESIAN_POINT('Ctrl Pts',(-18.8829078354626,21.3268947828466,
-5.70091667579017));
#108767=CARTESIAN_POINT('Ctrl Pts',(-18.750467595902,21.3320617312806,-5.70810129178447));
#108768=CARTESIAN_POINT('Ctrl Pts',(-18.6065505479636,21.3241936184566,
-5.71660684789848));
#108769=CARTESIAN_POINT('Ctrl Pts',(-18.5946733697303,21.3234437761401,
-5.7173140860814));
#108770=CARTESIAN_POINT('Ctrl Pts',(-18.5777949211286,21.3222352278593,
-5.71832745442766));
#108771=CARTESIAN_POINT('Ctrl Pts',(-18.5727877383108,21.3218587872043,
-5.71862912459734));
#108772=CARTESIAN_POINT('Ctrl Pts',(-18.5641599262325,21.3211792696706,
-5.71915079918951));
#108773=CARTESIAN_POINT('Ctrl Pts',(-18.5605386127916,21.3208846764226,
-5.71937032841991));
#108774=CARTESIAN_POINT('Ctrl Pts',(-18.5535178032749,21.3202953373065,
-5.71979707054641));
#108775=CARTESIAN_POINT('Ctrl Pts',(-18.5501182541012,21.3200016942763,
-5.72000421498617));
#108776=CARTESIAN_POINT('Ctrl Pts',(-18.5409461584418,21.3191870904055,
-5.72056445063816));
#108777=CARTESIAN_POINT('Ctrl Pts',(-18.5351750669417,21.3186506442176,
-5.72091839850437));
#108778=CARTESIAN_POINT('Ctrl Pts',(-18.5137519313256,21.3165705067397,
-5.72223749707443));
#108779=CARTESIAN_POINT('Ctrl Pts',(-18.4981154814572,21.3148761444119,
-5.72321058726142));
#108780=CARTESIAN_POINT('Ctrl Pts',(-18.3497769522213,21.2971278016013,
-5.73253072918418));
#108781=CARTESIAN_POINT('Ctrl Pts',(-18.2188682292552,21.2687146627467,
-5.7414116018875));
#108782=CARTESIAN_POINT('Ctrl Pts',(-17.9416054217305,21.1804049336318,
-5.76063027322858));
#108783=CARTESIAN_POINT('Ctrl Pts',(-17.7974501093668,21.1160818426246,
-5.77086528931925));
#108784=CARTESIAN_POINT('Ctrl Pts',(-17.6433919414537,21.0255841769066,
-5.78183904219307));
#108785=CARTESIAN_POINT('Ctrl Pts',(-17.6252098497493,21.0145315708405,
-5.78313580139118));
#108786=CARTESIAN_POINT('Ctrl Pts',(-17.5995859739166,20.998421226839,-5.78496623610069));
#108787=CARTESIAN_POINT('Ctrl Pts',(-17.5920054856057,20.9935875455977,
-5.7855081192895));
#108788=CARTESIAN_POINT('Ctrl Pts',(-17.5789785459452,20.9851637431653,
-5.78644005772953));
#108789=CARTESIAN_POINT('Ctrl Pts',(-17.5735175177193,20.9815964974231,
-5.78683095712439));
#108790=CARTESIAN_POINT('Ctrl Pts',(-17.5630910410947,20.9747167675602,
-5.78757774363431));
#108791=CARTESIAN_POINT('Ctrl Pts',(-17.5581229520907,20.9714084172547,
-5.78793378060146));
#108792=CARTESIAN_POINT('Ctrl Pts',(-17.5452367186009,20.962748325783,-5.78885783909681));
#108793=CARTESIAN_POINT('Ctrl Pts',(-17.5373406472939,20.9573638607746,
-5.78942462063207));
#108794=CARTESIAN_POINT('Ctrl Pts',(-17.5105200522233,20.9388071214526,
-5.7913519872035));
#108795=CARTESIAN_POINT('Ctrl Pts',(-17.4917739676509,20.9253789480587,
-5.79270282020472));
#108796=CARTESIAN_POINT('Ctrl Pts',(-17.3330266496184,20.8076939522846,
-5.80418499218966));
#108797=CARTESIAN_POINT('Ctrl Pts',(-17.2061981499819,20.6868001741757,
-5.81357468432394));
#108798=CARTESIAN_POINT('Ctrl Pts',(-17.0401292948202,20.4838607140944,
-5.82784065594843));
#108799=CARTESIAN_POINT('Ctrl Pts',(-16.9888884612902,20.4126470561164,
-5.83263736680235));
#108800=CARTESIAN_POINT('Ctrl Pts',(-16.9219814317527,20.3063176510739,
-5.83980884853194));
#108801=CARTESIAN_POINT('Ctrl Pts',(-16.9026205671445,20.2736292943877,
-5.84201516170409));
#108802=CARTESIAN_POINT('Ctrl Pts',(-16.8804643955397,20.2338158365741,
-5.84472599626804));
#108803=CARTESIAN_POINT('Ctrl Pts',(-16.8768136002998,20.2271718089862,
-5.84517915070592));
#108804=CARTESIAN_POINT('Ctrl Pts',(-16.8712033153791,20.2168305126279,
-5.84588589785408));
#108805=CARTESIAN_POINT('Ctrl Pts',(-16.8692189267295,20.2131467240102,
-5.84613793434782));
#108806=CARTESIAN_POINT('Ctrl Pts',(-16.86556475507,20.2063147416167,-5.84660592255908));
#108807=CARTESIAN_POINT('Ctrl Pts',(-16.8638919949633,20.2031682056456,
-5.84682168166879));
#108808=CARTESIAN_POINT('Ctrl Pts',(-16.8601353965849,20.1960586256707,
-5.84730968562893));
#108809=CARTESIAN_POINT('Ctrl Pts',(-16.8580561940066,20.1920932085399,
-5.84758221662765));
#108810=CARTESIAN_POINT('Ctrl Pts',(-16.8519769960045,20.1804090937888,
-5.84838617153706));
#108811=CARTESIAN_POINT('Ctrl Pts',(-16.848012005372,20.1726724270002,-5.84891971676906));
#108812=CARTESIAN_POINT('Ctrl Pts',(-16.820301828012,20.1177725804081,-5.85271310695916));
#108813=CARTESIAN_POINT('Ctrl Pts',(-16.7982828544642,20.0697638383392,
-5.85606807119919));
#108814=CARTESIAN_POINT('Ctrl Pts',(-16.7720816975599,20.0064945790881,
-5.86049228171665));
#108815=CARTESIAN_POINT('Ctrl Pts',(-16.766241426347,19.9919361235487,-5.86151052440592));
#108816=CARTESIAN_POINT('Ctrl Pts',(-16.7421267843932,19.9298353542444,
-5.86585135097812));
#108817=CARTESIAN_POINT('Ctrl Pts',(-16.7254099322273,19.8817077066625,
-5.869208583509));
#108818=CARTESIAN_POINT('Ctrl Pts',(-16.6782974638417,19.7284428611841,
-5.87980028943694));
#108819=CARTESIAN_POINT('Ctrl Pts',(-16.65430310197,19.6215171239257,-5.88703521426393));
#108820=CARTESIAN_POINT('Ctrl Pts',(-16.6308108371743,19.4586376726489,
-5.89761332839874));
#108821=CARTESIAN_POINT('Ctrl Pts',(-16.6250743300697,19.4037755503269,
-5.90110487989195));
#108822=CARTESIAN_POINT('Ctrl Pts',(-16.6192531183309,19.3145010745006,
-5.90666584479976));
#108823=CARTESIAN_POINT('Ctrl Pts',(-16.6178530393138,19.2802033479213,
-5.90877375553695));
#108824=CARTESIAN_POINT('Ctrl Pts',(-16.6171093085936,19.2350762159063,
-5.91151142237625));
#108825=CARTESIAN_POINT('Ctrl Pts',(-16.6170139622384,19.2242659808238,
-5.91216454408876));
#108826=CARTESIAN_POINT('Ctrl Pts',(-16.6169934229573,19.2065569047683,
-5.91323018605293));
#108827=CARTESIAN_POINT('Ctrl Pts',(-16.6170191407032,19.1996584189663,
-5.91364423653605));
#108828=CARTESIAN_POINT('Ctrl Pts',(-16.6171342072677,19.1863037889918,
-5.91444376773099));
#108829=CARTESIAN_POINT('Ctrl Pts',(-16.6172193730737,19.1798476939327,
-5.91482937496355));
#108830=CARTESIAN_POINT('Ctrl Pts',(-16.6174842503578,19.164939769398,-5.91571772463919));
#108831=CARTESIAN_POINT('Ctrl Pts',(-16.617685053987,19.1564883886591,-5.91621980135753));
#108832=CARTESIAN_POINT('Ctrl Pts',(-16.6183613633517,19.1337584663539,
-5.91756614071017));
#108833=CARTESIAN_POINT('Ctrl Pts',(-16.6189307931224,19.1194830047645,
-5.91840746380878));
#108834=CARTESIAN_POINT('Ctrl Pts',(-16.6254695501611,18.9887920505441,
-5.92607338714303));
#108835=CARTESIAN_POINT('Ctrl Pts',(-16.640900093674,18.8730428279378,-5.93258287206407));
#108836=CARTESIAN_POINT('Ctrl Pts',(-16.700362160854,18.600878542959,-5.94783519675533));
#108837=CARTESIAN_POINT('Ctrl Pts',(-16.7529850934015,18.4471286309441,
-5.95639703814145));
#108838=CARTESIAN_POINT('Ctrl Pts',(-16.836973585782,18.2707362443149,-5.9676036359387));
#108839=CARTESIAN_POINT('Ctrl Pts',(-16.8520471684738,18.2409183517398,
-5.96955082452033));
#108840=CARTESIAN_POINT('Ctrl Pts',(-16.8712656670052,18.2050362344626,
-5.9719740953264));
#108841=CARTESIAN_POINT('Ctrl Pts',(-16.8747456172116,18.1986189307154,
-5.97241066143764));
#108842=CARTESIAN_POINT('Ctrl Pts',(-16.8802427763706,18.1886056753827,
-5.97309704809824));
#108843=CARTESIAN_POINT('Ctrl Pts',(-16.8822374561672,18.1849973295554,
-5.97334545325473));
#108844=CARTESIAN_POINT('Ctrl Pts',(-16.8859789753791,18.1782754296004,
-5.97381022747824));
#108845=CARTESIAN_POINT('Ctrl Pts',(-16.8877231542394,18.1751604593793,
-5.97402642625152));
#108846=CARTESIAN_POINT('Ctrl Pts',(-16.8917139493268,18.1680753061379,
-5.97452004226621));
#108847=CARTESIAN_POINT('Ctrl Pts',(-16.8939655151901,18.1641079791198,
-5.97479777461323));
#108848=CARTESIAN_POINT('Ctrl Pts',(-16.8998557044989,18.1538069909157,
-5.97552230358343));
#108849=CARTESIAN_POINT('Ctrl Pts',(-16.9035142815429,18.1474848914291,
-5.97597034067082));
#108850=CARTESIAN_POINT('Ctrl Pts',(-16.9270757699051,18.1072518826028,
-5.97884251541472));
#108851=CARTESIAN_POINT('Ctrl Pts',(-16.9478861388533,18.0738843938315,
-5.98131976352892));
#108852=CARTESIAN_POINT('Ctrl Pts',(-16.9763283964887,18.0309884496147,
-5.98461188090347));
#108853=CARTESIAN_POINT('Ctrl Pts',(-16.9831319684865,18.0209168723103,
-5.98539283862582));
#108854=CARTESIAN_POINT('Ctrl Pts',(-16.9904473522303,18.0102861589587,
-5.9862252610686));
#108855=CARTESIAN_POINT('Ctrl Pts',(-16.990873264747,18.0096679274835,-5.98627370009617));
#108856=CARTESIAN_POINT('Ctrl Pts',(-17.004264453133,17.9902521205601,-5.98779586557816));
#108857=CARTESIAN_POINT('Ctrl Pts',(-17.0175323814377,17.9716657798494,
-5.98928004239451));
#108858=CARTESIAN_POINT('Ctrl Pts',(-17.0582314791836,17.9165600515037,
-5.99375480662154));
#108859=CARTESIAN_POINT('Ctrl Pts',(-17.0865461054743,17.8807104110526,
-5.99676606348786));
#108860=CARTESIAN_POINT('Ctrl Pts',(-17.1865154004732,17.7622286926707,
-6.00700644329614));
#108861=CARTESIAN_POINT('Ctrl Pts',(-17.263408736637,17.6842348938267,-6.01423702409776));
#108862=CARTESIAN_POINT('Ctrl Pts',(-17.3875659536343,17.5764246839066,
-6.02480601306636));
#108863=CARTESIAN_POINT('Ctrl Pts',(-17.4305385390984,17.5419553197506,
-6.02829281389283));
#108864=CARTESIAN_POINT('Ctrl Pts',(-17.5023719697226,17.4888045995001,
-6.03384709831494));
#108865=CARTESIAN_POINT('Ctrl Pts',(-17.5304270016017,17.4690824198566,
-6.03595296402337));
#108866=CARTESIAN_POINT('Ctrl Pts',(-17.5679391542238,17.4440512496766,
-6.03868840355027));
#108867=CARTESIAN_POINT('Ctrl Pts',(-17.5769741499679,17.4381218396458,
-6.03934129545955));
#108868=CARTESIAN_POINT('Ctrl Pts',(-17.5918497670957,17.4285215506393,
-6.04040665856749));
#108869=CARTESIAN_POINT('Ctrl Pts',(-17.5976635460145,17.4248096288317,
-6.04082065845261));
#108870=CARTESIAN_POINT('Ctrl Pts',(-17.6089545756466,17.417678086701,-6.04162015832602));
#108871=CARTESIAN_POINT('Ctrl Pts',(-17.6144295268518,17.4142549850751,
-6.04200578448717));
#108872=CARTESIAN_POINT('Ctrl Pts',(-17.6271101530793,17.4064071471837,
-6.04289427263789));
#108873=CARTESIAN_POINT('Ctrl Pts',(-17.6343268786544,17.4020004071293,
-6.04339646823619));
#108874=CARTESIAN_POINT('Ctrl Pts',(-17.6538130492785,17.3902612908354,
-6.0447433369212));
#108875=CARTESIAN_POINT('Ctrl Pts',(-17.6661308035135,17.3830096582104,
-6.0455850668113));
#108876=CARTESIAN_POINT('Ctrl Pts',(-17.7800282851797,17.3175008211735,
-6.05328245400493));
#108877=CARTESIAN_POINT('Ctrl Pts',(-17.8862102251636,17.2676372034031,
-6.05981988974111));
#108878=CARTESIAN_POINT('Ctrl Pts',(-18.1493512056869,17.1697625688518,
-6.0751882643298));
#108879=CARTESIAN_POINT('Ctrl Pts',(-18.3087951247446,17.1306988123705,
-6.08383351307016));
#108880=CARTESIAN_POINT('Ctrl Pts',(-18.5023525833226,17.1064765400254,
-6.09504687432979));
#108881=CARTESIAN_POINT('Ctrl Pts',(-18.5336629199799,17.1032655918991,
-6.09688399228954));
#108882=CARTESIAN_POINT('Ctrl Pts',(-18.5721758845913,17.1001818342797,
-6.09918480224686));
#108883=CARTESIAN_POINT('Ctrl Pts',(-18.5793232614034,17.0996460561393,
-6.09961352810246));
#108884=CARTESIAN_POINT('Ctrl Pts',(-18.5905569766248,17.0988613070054,
-6.10029028172232));
#108885=CARTESIAN_POINT('Ctrl Pts',(-18.5946416279887,17.0985878709642,
-6.10053695862382));
#108886=CARTESIAN_POINT('Ctrl Pts',(-18.6022940394019,17.0980978925119,
-6.10100027229927));
#108887=CARTESIAN_POINT('Ctrl Pts',(-18.605861563443,17.0978785372606,-6.10121674962493));
#108888=CARTESIAN_POINT('Ctrl Pts',(-18.6140274898488,17.0973971965551,
-6.10171335169056));
#108889=CARTESIAN_POINT('Ctrl Pts',(-18.618626188686,17.0971411833665,-6.10199380663432));
#108890=CARTESIAN_POINT('Ctrl Pts',(-18.632837179259,17.0963965574835,-6.10286283766763));
#108891=CARTESIAN_POINT('Ctrl Pts',(-18.6424518385142,17.0959584965065,
-6.10345413354853));
#108892=CARTESIAN_POINT('Ctrl Pts',(-18.738598852769,17.0922346736948,-6.10939825158321));
#108893=CARTESIAN_POINT('Ctrl Pts',(-18.8252434011508,17.0941960822023,
-6.11500406507168));
#108894=CARTESIAN_POINT('Ctrl Pts',(-19.0379880080281,17.1120980439608,
-6.12902170527436));
#108895=CARTESIAN_POINT('Ctrl Pts',(-19.1632593892837,17.1340941089328,
-6.13748308260308));
#108896=CARTESIAN_POINT('Ctrl Pts',(-19.379010787905,17.1923444584453,-6.1519473104327));
#108897=CARTESIAN_POINT('Ctrl Pts',(-19.4703935159452,17.223856764454,-6.15804199020151));
#108898=CARTESIAN_POINT('Ctrl Pts',(-19.572782778184,17.2672031314735,-6.16482092097132));
#108899=CARTESIAN_POINT('Ctrl Pts',(-19.5861890639793,17.2730431813018,
-6.16570768030029));
#108900=CARTESIAN_POINT('Ctrl Pts',(-19.6065883434729,17.2821821407976,
-6.16705594888665));
#108901=CARTESIAN_POINT('Ctrl Pts',(-19.6136253618458,17.2853811445636,
-6.16752086249995));
#108902=CARTESIAN_POINT('Ctrl Pts',(-19.6264196544637,17.2912821551568,
-6.16836584596404));
#108903=CARTESIAN_POINT('Ctrl Pts',(-19.6321825512969,17.2939716878995,
-6.16874633967788));
#108904=CARTESIAN_POINT('Ctrl Pts',(-19.644624184719,17.299846593227,-6.16956759669094));
#108905=CARTESIAN_POINT('Ctrl Pts',(-19.6512985329181,17.303041102735,-6.17000803772745));
#108906=CARTESIAN_POINT('Ctrl Pts',(-19.6694152812477,17.31182926927,-6.17120331116676));
#108907=CARTESIAN_POINT('Ctrl Pts',(-19.6808242875425,17.3174913541168,
-6.17195575586583));
#108908=CARTESIAN_POINT('Ctrl Pts',(-19.7368646384045,17.345936335266,-6.17565125888036));
#108909=CARTESIAN_POINT('Ctrl Pts',(-19.7807305081523,17.3701969738104,
-6.17854195084981));
#108910=CARTESIAN_POINT('Ctrl Pts',(-19.9725202030574,17.4853439778855,
-6.19124131817274));
#108911=CARTESIAN_POINT('Ctrl Pts',(-20.1097822100573,17.5926538725432,
-6.20043480306611));
#108912=CARTESIAN_POINT('Ctrl Pts',(-20.2767028355463,17.7599007239427,
-6.21342104815364));
#108913=CARTESIAN_POINT('Ctrl Pts',(-20.3190029643256,17.80622756216,-6.21691353812115));
#108914=CARTESIAN_POINT('Ctrl Pts',(-20.3790002901429,17.8781010943263,
-6.22229879364762));
#108915=CARTESIAN_POINT('Ctrl Pts',(-20.3982951629098,17.9022728202578,
-6.2241048180542));
#108916=CARTESIAN_POINT('Ctrl Pts',(-20.421376501477,17.9325242058161,-6.22637099027759));
#108917=CARTESIAN_POINT('Ctrl Pts',(-20.4256717674372,17.9382131199545,
-6.22679740542314));
#108918=CARTESIAN_POINT('Ctrl Pts',(-20.4323832437174,17.9471961994309,
-6.22747131891753));
#108919=CARTESIAN_POINT('Ctrl Pts',(-20.4348188353693,17.9504759115839,
-6.22771748517498));
#108920=CARTESIAN_POINT('Ctrl Pts',(-20.4393684431548,17.9566395019801,
-6.22818037679325));
#108921=CARTESIAN_POINT('Ctrl Pts',(-20.4414846510105,17.9595216934423,
-6.22839694594243));
#108922=CARTESIAN_POINT('Ctrl Pts',(-20.4463180504041,17.9661396730962,
-6.2288944736895));
#108923=CARTESIAN_POINT('Ctrl Pts',(-20.4490303152467,17.9698789921648,
-6.2291757671354));
#108924=CARTESIAN_POINT('Ctrl Pts',(-20.4573967030695,17.9814932743113,
-6.23004993459246));
#108925=CARTESIAN_POINT('Ctrl Pts',(-20.4630088932696,17.9893980912523,
-6.23064557410465));
#108926=CARTESIAN_POINT('Ctrl Pts',(-20.525858317636,18.0792227489039,-6.23741895062477));
#108927=CARTESIAN_POINT('Ctrl Pts',(-20.5772738131753,18.1650492918994,
-6.24393187552144));
#108928=CARTESIAN_POINT('Ctrl Pts',(-20.6603886046325,18.3290879047529,
-6.25604814573764));
#108929=CARTESIAN_POINT('Ctrl Pts',(-20.6938230869984,18.4061322178279,
-6.26161630673243));
#108930=CARTESIAN_POINT('Ctrl Pts',(-20.7225804911066,18.4848893814367,
-6.26710637686285));
#108931=CARTESIAN_POINT('',(-20.8509997150786,19.2120983429817,-5.28730630211274));
#108932=CARTESIAN_POINT('Ctrl Pts',(-20.7225806138063,18.4848897174713,
-6.04247212253779));
#108933=CARTESIAN_POINT('Ctrl Pts',(-20.7198614621432,18.477442842784,-6.04199082365182));
#108934=CARTESIAN_POINT('Ctrl Pts',(-20.7171004599269,18.4700111880572,
-6.04151092132984));
#108935=CARTESIAN_POINT('Ctrl Pts',(-20.7114649079107,18.4550993790409,
-6.04054876329006));
#108936=CARTESIAN_POINT('Ctrl Pts',(-20.7085895172297,18.4476197199386,
-6.04006654790803));
#108937=CARTESIAN_POINT('Ctrl Pts',(-20.7033486788313,18.434214648031,-6.03920297565442));
#108938=CARTESIAN_POINT('Ctrl Pts',(-20.7009987945502,18.4282832916904,
-6.03882110180472));
#108939=CARTESIAN_POINT('Ctrl Pts',(-20.6959425293938,18.4156873251404,
-6.03801060091683));
#108940=CARTESIAN_POINT('Ctrl Pts',(-20.6932289167103,18.40902569036,-6.03758222352211));
#108941=CARTESIAN_POINT('Ctrl Pts',(-20.6858435948529,18.3911567184248,
-6.03643381295184));
#108942=CARTESIAN_POINT('Ctrl Pts',(-20.6811092890116,18.3799754209312,
-6.03571590704927));
#108943=CARTESIAN_POINT('Ctrl Pts',(-20.657153366327,18.324726032539,-6.03217125619475));
#108944=CARTESIAN_POINT('Ctrl Pts',(-20.6365297918646,18.2812788987519,
-6.02939279002619));
#108945=CARTESIAN_POINT('Ctrl Pts',(-20.537431340742,18.0896467430304,-6.01711812413672));
#108946=CARTESIAN_POINT('Ctrl Pts',(-20.4430052929719,17.9504048372787,
-6.00819989208419));
#108947=CARTESIAN_POINT('Ctrl Pts',(-20.2684509412495,17.74918797159,-5.99361602285774));
#108948=CARTESIAN_POINT('Ctrl Pts',(-20.1986342586465,17.6792443202059,
-5.98812327491185));
#108949=CARTESIAN_POINT('Ctrl Pts',(-20.1168931575858,17.6080684639141,
-5.98170202225121));
#108950=CARTESIAN_POINT('Ctrl Pts',(-20.1095379825726,17.6017522735439,
-5.98112428390987));
#108951=CARTESIAN_POINT('Ctrl Pts',(-20.0986146031857,17.5925015214897,
-5.98026590102706));
#108952=CARTESIAN_POINT('Ctrl Pts',(-20.0950796404054,17.5895276592817,
-5.97998805981999));
#108953=CARTESIAN_POINT('Ctrl Pts',(-20.0887912538401,17.5842724738487,
-5.97949364733824));
#108954=CARTESIAN_POINT('Ctrl Pts',(-20.0860417540153,17.5819865313602,
-5.97927741804499));
#108955=CARTESIAN_POINT('Ctrl Pts',(-20.0801385590092,17.577103837967,-5.97881303717233));
#108956=CARTESIAN_POINT('Ctrl Pts',(-20.0769831827091,17.5745092854936,
-5.97856473934054));
#108957=CARTESIAN_POINT('Ctrl Pts',(-20.0683014444765,17.5674126231789,
-5.97788140683934));
#108958=CARTESIAN_POINT('Ctrl Pts',(-20.0627598819095,17.5629293149645,
-5.97744505464086));
#108959=CARTESIAN_POINT('Ctrl Pts',(-20.0330577929898,17.53914652113,-5.9751057905538));
#108960=CARTESIAN_POINT('Ctrl Pts',(-20.0085005702278,17.5203512287885,
-5.97317010611272));
#108961=CARTESIAN_POINT('Ctrl Pts',(-19.932933748562,17.4650969610725,-5.9672307357491));
#108962=CARTESIAN_POINT('Ctrl Pts',(-19.8807099036406,17.4303611109995,
-5.96314961963098));
#108963=CARTESIAN_POINT('Ctrl Pts',(-19.7118261345998,17.3285442591615,
-5.95019059956498));
#108964=CARTESIAN_POINT('Ctrl Pts',(-19.5902575770625,17.2702239376253,
-5.94122494624613));
#108965=CARTESIAN_POINT('Ctrl Pts',(-19.4256423302445,17.2097535373328,
-5.92993149527873));
#108966=CARTESIAN_POINT('Ctrl Pts',(-19.3869104091957,17.1967843128682,
-5.92732954855638));
#108967=CARTESIAN_POINT('Ctrl Pts',(-19.3014161498651,17.1708824909948,
-5.92171057413525));
#108968=CARTESIAN_POINT('Ctrl Pts',(-19.2545345789874,17.1584199420785,
-5.91870896433799));
#108969=CARTESIAN_POINT('Ctrl Pts',(-19.1949880124128,17.1447624393269,
-5.91499309747588));
#108970=CARTESIAN_POINT('Ctrl Pts',(-19.1826878248616,17.1420565857681,
-5.91423062934022));
#108971=CARTESIAN_POINT('Ctrl Pts',(-19.1631556905309,17.1379421959932,
-5.91302775897249));
#108972=CARTESIAN_POINT('Ctrl Pts',(-19.1559394234829,17.1364614029822,
-5.91258505135177));
#108973=CARTESIAN_POINT('Ctrl Pts',(-19.1424772954541,17.1337720954769,
-5.91176228633943));
#108974=CARTESIAN_POINT('Ctrl Pts',(-19.1362334512421,17.1325540131389,
-5.91138192725712));
#108975=CARTESIAN_POINT('Ctrl Pts',(-19.1223512231174,17.1299106935208,
-5.91053898161985));
#108976=CARTESIAN_POINT('Ctrl Pts',(-19.1147102678429,17.1284993232986,
-5.91007684170201));
#108977=CARTESIAN_POINT('Ctrl Pts',(-19.092479206305,17.1245194414676,-5.90873746286848));
#108978=CARTESIAN_POINT('Ctrl Pts',(-19.0778695078084,17.1220619346721,
-5.90786375536702));
#108979=CARTESIAN_POINT('Ctrl Pts',(-18.961238213152,17.1037000734621,-5.90093813149453));
#108980=CARTESIAN_POINT('Ctrl Pts',(-18.8581967084162,17.0951244404664,
-5.89512924265497));
#108981=CARTESIAN_POINT('Ctrl Pts',(-18.595291539024,17.0925251571705,-5.88065391693254));
#108982=CARTESIAN_POINT('Ctrl Pts',(-18.4360031144689,17.1090091203861,
-5.87222556514472));
#108983=CARTESIAN_POINT('Ctrl Pts',(-18.2326858998322,17.1536402720964,
-5.86047047933077));
#108984=CARTESIAN_POINT('Ctrl Pts',(-18.1856531319034,17.1656736688338,
-5.85767570280846));
#108985=CARTESIAN_POINT('Ctrl Pts',(-18.1316337524453,17.181491661299,-5.85433398107354));
#108986=CARTESIAN_POINT('Ctrl Pts',(-18.1242001559643,17.1837128128721,
-5.85387119253759));
#108987=CARTESIAN_POINT('Ctrl Pts',(-18.1123333379977,17.1873297793388,
-5.85312745923925));
#108988=CARTESIAN_POINT('Ctrl Pts',(-18.1078921331725,17.188699444002,-5.85284800153556));
#108989=CARTESIAN_POINT('Ctrl Pts',(-18.1000300526545,17.1911524854589,
-5.85235125666072));
#108990=CARTESIAN_POINT('Ctrl Pts',(-18.0966073787929,17.1922299481115,
-5.85213431800261));
#108991=CARTESIAN_POINT('Ctrl Pts',(-18.0893538418128,17.1945336577665,
-5.85167309128154));
#108992=CARTESIAN_POINT('Ctrl Pts',(-18.0855237891369,17.1957621028903,
-5.85142868092559));
#108993=CARTESIAN_POINT('Ctrl Pts',(-18.0751860252404,17.1991103432874,
-5.85076667849918));
#108994=CARTESIAN_POINT('Ctrl Pts',(-18.0686851205157,17.2012507737768,
-5.85034790003425));
#108995=CARTESIAN_POINT('Ctrl Pts',(-18.0363453407776,17.2120727886043,
-5.84825265757752));
#108996=CARTESIAN_POINT('Ctrl Pts',(-18.0106667357245,17.2212209053297,
-5.84655085670326));
#108997=CARTESIAN_POINT('Ctrl Pts',(-17.9367518163412,17.2491732257531,
-5.84155546591997));
#108998=CARTESIAN_POINT('Ctrl Pts',(-17.889021345343,17.2692535411416,-5.83820866876273));
#108999=CARTESIAN_POINT('Ctrl Pts',(-17.7166743288491,17.3493186293195,
-5.82578656298283));
#109000=CARTESIAN_POINT('Ctrl Pts',(-17.5972690262176,17.4197278828816,
-5.81654003223718));
#109001=CARTESIAN_POINT('Ctrl Pts',(-17.4079534444384,17.557963641679,-5.80136173524123));
#109002=CARTESIAN_POINT('Ctrl Pts',(-17.3342656355115,17.6198756040067,
-5.79528901843943));
#109003=CARTESIAN_POINT('Ctrl Pts',(-17.2550407733338,17.6962191095029,
-5.78857468787628));
#109004=CARTESIAN_POINT('Ctrl Pts',(-17.2451437466784,17.7059456449375,
-5.78773215837909));
#109005=CARTESIAN_POINT('Ctrl Pts',(-17.2294565675115,17.7216687688662,
-5.78639044133519));
#109006=CARTESIAN_POINT('Ctrl Pts',(-17.2236050824061,17.7276033395333,
-5.78588853788793));
#109007=CARTESIAN_POINT('Ctrl Pts',(-17.213296031286,17.7381830114306,-5.78500168230809));
#109008=CARTESIAN_POINT('Ctrl Pts',(-17.2088243498558,17.7428141534846,
-5.78461611337973));
#109009=CARTESIAN_POINT('Ctrl Pts',(-17.199569512493,17.7524869306145,-5.78381623301755));
#109010=CARTESIAN_POINT('Ctrl Pts',(-17.194789911567,17.757531871696,-5.7834020782515));
#109011=CARTESIAN_POINT('Ctrl Pts',(-17.1824805137973,17.7706534409504,
-5.7823326330014));
#109012=CARTESIAN_POINT('Ctrl Pts',(-17.1749888490189,17.7787656740823,
-5.78167898108254));
#109013=CARTESIAN_POINT('Ctrl Pts',(-17.143079395792,17.813865378173,-5.7788823463047));
#109014=CARTESIAN_POINT('Ctrl Pts',(-17.1192954062883,17.8414223903696,
-5.77676607225918));
#109015=CARTESIAN_POINT('Ctrl Pts',(-17.0583345653391,17.9158507505079,
-5.77124096245622));
#109016=CARTESIAN_POINT('Ctrl Pts',(-17.0224126007662,17.96370869685,-5.76787962242608));
#109017=CARTESIAN_POINT('Ctrl Pts',(-16.8936198752804,18.1513585474914,
-5.75527051065746));
#109018=CARTESIAN_POINT('Ctrl Pts',(-16.8154661405173,18.3004731198014,
-5.74643984015733));
#109019=CARTESIAN_POINT('Ctrl Pts',(-16.7365386377461,18.5076195074023,
-5.73397914262836));
#109020=CARTESIAN_POINT('Ctrl Pts',(-16.7192749236401,18.5587133844757,
-5.73088659255996));
#109021=CARTESIAN_POINT('Ctrl Pts',(-16.7015015511334,18.6187876510889,
-5.72716901417719));
#109022=CARTESIAN_POINT('Ctrl Pts',(-16.6990736176738,18.6271849407554,
-5.72664753855623));
#109023=CARTESIAN_POINT('Ctrl Pts',(-16.6954780245903,18.6399156840981,
-5.72585385932323));
#109024=CARTESIAN_POINT('Ctrl Pts',(-16.6942719918172,18.6442383288546,
-5.72558383249738));
#109025=CARTESIAN_POINT('Ctrl Pts',(-16.6921327836786,18.6520009168243,
-5.72509790112799));
#109026=CARTESIAN_POINT('Ctrl Pts',(-16.6911945435307,18.6554394085201,
-5.72488229420803));
#109027=CARTESIAN_POINT('Ctrl Pts',(-16.6891757635245,18.6629121564715,
-5.72441292972801));
#109028=CARTESIAN_POINT('Ctrl Pts',(-16.6880984910884,18.6669471924167,
-5.72415899218083));
#109029=CARTESIAN_POINT('Ctrl Pts',(-16.6851086425479,18.6782804419156,
-5.72344441532025));
#109030=CARTESIAN_POINT('Ctrl Pts',(-16.6832231535289,18.6855856451814,
-5.72298225567902));
#109031=CARTESIAN_POINT('Ctrl Pts',(-16.6722351572208,18.7291182533743,
-5.72021958464714));
#109032=CARTESIAN_POINT('Ctrl Pts',(-16.6640543255889,18.7655689798445,
-5.71787102464256));
#109033=CARTESIAN_POINT('Ctrl Pts',(-16.6403977670609,18.8857747405225,
-5.71005239539296));
#109034=CARTESIAN_POINT('Ctrl Pts',(-16.6290112838938,18.9702461485174,
-5.70444490279422));
#109035=CARTESIAN_POINT('Ctrl Pts',(-16.6096334004436,19.2327823223064,
-5.68705420474811));
#109036=CARTESIAN_POINT('Ctrl Pts',(-16.6189869202772,19.4113798457865,
-5.67535026087291));
#109037=CARTESIAN_POINT('Ctrl Pts',(-16.6546513085106,19.6091421928189,
-5.66298375792962));
#109038=CARTESIAN_POINT('Ctrl Pts',(-16.6590571167547,19.6315000374013,
-5.66159295495752));
#109039=CARTESIAN_POINT('Ctrl Pts',(-16.6658127329985,19.6630850734839,
-5.6596378324023));
#109040=CARTESIAN_POINT('Ctrl Pts',(-16.6678649975143,19.6723736459497,
-5.6590640565413));
#109041=CARTESIAN_POINT('Ctrl Pts',(-16.6713049976595,19.6874597120256,
-5.65813401181504));
#109042=CARTESIAN_POINT('Ctrl Pts',(-16.6726547189639,19.6932656564005,
-5.65777652800008));
#109043=CARTESIAN_POINT('Ctrl Pts',(-16.6755343998046,19.7054198747651,
-5.65702907849844));
#109044=CARTESIAN_POINT('Ctrl Pts',(-16.6770692481107,19.711766934967,-5.6566392744995));
#109045=CARTESIAN_POINT('Ctrl Pts',(-16.6807963422214,19.7268733067208,
-5.65571271409452));
#109046=CARTESIAN_POINT('Ctrl Pts',(-16.6830153204296,19.7356259399958,
-5.65517682577423));
#109047=CARTESIAN_POINT('Ctrl Pts',(-16.6907089317176,19.7651779347203,
-5.65337052474706));
#109048=CARTESIAN_POINT('Ctrl Pts',(-16.6964446151451,19.7859084073686,
-5.65210855789065));
#109049=CARTESIAN_POINT('Ctrl Pts',(-16.7531069261878,19.9791920036931,
-5.64038142589846));
#109050=CARTESIAN_POINT('Ctrl Pts',(-16.825516469301,20.1446776122042,-5.63071760710449));
#109051=CARTESIAN_POINT('Ctrl Pts',(-16.9796612851757,20.4019591023959,
-5.61439336705209));
#109052=CARTESIAN_POINT('Ctrl Pts',(-17.0499641430449,20.4994497497098,
-5.60780805151875));
#109053=CARTESIAN_POINT('Ctrl Pts',(-17.1343293722125,20.597662673797,-5.60013489953289));
#109054=CARTESIAN_POINT('Ctrl Pts',(-17.1405762171617,20.6048364785569,
-5.59956790063481));
#109055=CARTESIAN_POINT('Ctrl Pts',(-17.1499045671602,20.6154043833545,
-5.59872249052285));
#109056=CARTESIAN_POINT('Ctrl Pts',(-17.1529491910044,20.6188310803491,
-5.59844676183229));
#109057=CARTESIAN_POINT('Ctrl Pts',(-17.158386179031,20.6249104807088,-5.5979546715447));
#109058=CARTESIAN_POINT('Ctrl Pts',(-17.1607741516917,20.6275670440444,
-5.59773863996061));
#109059=CARTESIAN_POINT('Ctrl Pts',(-17.1659229072422,20.6332658358075,
-5.59727304572888));
#109060=CARTESIAN_POINT('Ctrl Pts',(-17.1686857844283,20.6363060311397,
-5.59702332823503));
#109061=CARTESIAN_POINT('Ctrl Pts',(-17.1763371418638,20.6446762980538,
-5.59633216816887));
#109062=CARTESIAN_POINT('Ctrl Pts',(-17.1812440605447,20.6499893315196,
-5.59588935846801));
#109063=CARTESIAN_POINT('Ctrl Pts',(-17.2082840034164,20.6789678563894,
-5.59345214687355));
#109064=CARTESIAN_POINT('Ctrl Pts',(-17.2309296210877,20.7021465721444,
-5.59142170700483));
#109065=CARTESIAN_POINT('Ctrl Pts',(-17.3705213873353,20.8386130813369,
-5.57901857875062));
#109066=CARTESIAN_POINT('Ctrl Pts',(-17.4996839447417,20.9386174512351,
-5.56805381332734));
#109067=CARTESIAN_POINT('Ctrl Pts',(-17.7390295010385,21.0832646383837,
-5.54978643656016));
#109068=CARTESIAN_POINT('Ctrl Pts',(-17.8438727455666,21.1353238949974,
-5.54234351682457));
#109069=CARTESIAN_POINT('Ctrl Pts',(-17.9657760155113,21.183745593241,-5.53433437114166));
#109070=CARTESIAN_POINT('Ctrl Pts',(-17.9791120156076,21.1888871081894,
-5.53346622149141));
#109071=CARTESIAN_POINT('Ctrl Pts',(-18.0004190293026,21.1968548416351,
-5.53209169083875));
#109072=CARTESIAN_POINT('Ctrl Pts',(-18.0083564952692,21.1997689659428,
-5.53158238029628));
#109073=CARTESIAN_POINT('Ctrl Pts',(-18.0223857892135,21.2048244421099,
-5.53068694405578));
#109074=CARTESIAN_POINT('Ctrl Pts',(-18.028470314185,21.2069856098717,-5.53030016196275));
#109075=CARTESIAN_POINT('Ctrl Pts',(-18.0410750656224,21.2113978639122,
-5.52950210424154));
#109076=CARTESIAN_POINT('Ctrl Pts',(-18.0475966044011,21.2136449907232,
-5.5290909638539));
#109077=CARTESIAN_POINT('Ctrl Pts',(-18.0643637429713,21.2193309183333,
-5.52803836246365));
#109078=CARTESIAN_POINT('Ctrl Pts',(-18.0746249828955,21.2227232383295,
-5.52739844213928));
#109079=CARTESIAN_POINT('Ctrl Pts',(-18.1175522224221,21.236551054962,-5.52473863686662));
#109080=CARTESIAN_POINT('Ctrl Pts',(-18.1504444476018,21.2462710021974,
-5.5227422612433));
#109081=CARTESIAN_POINT('Ctrl Pts',(-18.2367413468168,21.2695082426363,
-5.51760055973521));
#109082=CARTESIAN_POINT('Ctrl Pts',(-18.2904639391543,21.2817483575811,
-5.51449457513981));
#109083=CARTESIAN_POINT('Ctrl Pts',(-18.4520628622403,21.3119882915455,
-5.50535291137145));
#109084=CARTESIAN_POINT('Ctrl Pts',(-18.5609189914801,21.3237432881816,
-5.49946597068928));
#109085=CARTESIAN_POINT('Ctrl Pts',(-18.7134445135988,21.3283423530161,
-5.49115818590459));
#109086=CARTESIAN_POINT('Ctrl Pts',(-18.7567221411009,21.3283201641636,
-5.48879290318467));
#109087=CARTESIAN_POINT('Ctrl Pts',(-18.8752016225692,21.3246264537201,
-5.48222974381557));
#109088=CARTESIAN_POINT('Ctrl Pts',(-18.9502490327657,21.3182703889049,
-5.4779757947743));
#109089=CARTESIAN_POINT('Ctrl Pts',(-19.034186345117,21.3066304913513,-5.472953445476));
#109090=CARTESIAN_POINT('Ctrl Pts',(-19.0435740917873,21.305264279453,-5.47238796482603));
#109091=CARTESIAN_POINT('Ctrl Pts',(-19.0574787294372,21.3031451855739,
-5.47154439022515));
#109092=CARTESIAN_POINT('Ctrl Pts',(-19.0620030198026,21.302440647978,-5.4712689619221));
#109093=CARTESIAN_POINT('Ctrl Pts',(-19.0700522777361,21.3011604300814,
-5.47077720018088));
#109094=CARTESIAN_POINT('Ctrl Pts',(-19.0735781089767,21.3005905016347,
-5.47056119505293));
#109095=CARTESIAN_POINT('Ctrl Pts',(-19.0811596414179,21.2993452989248,
-5.4700954207417));
#109096=CARTESIAN_POINT('Ctrl Pts',(-19.0852147633053,21.2986671414626,
-5.46984549546054));
#109097=CARTESIAN_POINT('Ctrl Pts',(-19.0964127235129,21.2967609034773,
-5.46915318776421));
#109098=CARTESIAN_POINT('Ctrl Pts',(-19.1035511916393,21.2955079615817,
-5.46870943088116));
#109099=CARTESIAN_POINT('Ctrl Pts',(-19.1427887234668,21.2884131174835,
-5.46625743888596));
#109100=CARTESIAN_POINT('Ctrl Pts',(-19.1747539975205,21.281866756592,-5.46421265903628));
#109101=CARTESIAN_POINT('Ctrl Pts',(-19.3650776320553,21.2382833653326,
-5.45180470637538));
#109102=CARTESIAN_POINT('Ctrl Pts',(-19.5188868831278,21.1838378908713,
-5.44085307670154));
#109103=CARTESIAN_POINT('Ctrl Pts',(-19.7698225600987,21.0609720412171,
-5.4226029810598));
#109104=CARTESIAN_POINT('Ctrl Pts',(-19.8702833837605,21.0010259214969,
-5.41516465564124));
#109105=CARTESIAN_POINT('Ctrl Pts',(-19.9769292840044,20.924773661339,-5.40715950387927));
#109106=CARTESIAN_POINT('Ctrl Pts',(-19.9884739256701,20.9163411837187,
-5.40629113600111));
#109107=CARTESIAN_POINT('Ctrl Pts',(-20.0067103295512,20.9027354778578,
-5.40491632623092));
#109108=CARTESIAN_POINT('Ctrl Pts',(-20.0134578828898,20.8976380877775,
-5.40440695294765));
#109109=CARTESIAN_POINT('Ctrl Pts',(-20.0253035015431,20.8885774080583,
-5.40351144372293));
#109110=CARTESIAN_POINT('Ctrl Pts',(-20.030414282376,20.884630993681,-5.4031246510499));
#109111=CARTESIAN_POINT('Ctrl Pts',(-20.0407754087462,20.8765544581456,
-5.4023395953425));
#109112=CARTESIAN_POINT('Ctrl Pts',(-20.0460244242168,20.8724227438505,
-5.40194140165657));
#109113=CARTESIAN_POINT('Ctrl Pts',(-20.0593328865063,20.8618447070201,
-5.40093053084449));
#109114=CARTESIAN_POINT('Ctrl Pts',(-20.0673649720068,20.8553641214436,
-5.40031923123136));
#109115=CARTESIAN_POINT('Ctrl Pts',(-20.0846849211483,20.8411793918405,
-5.39899822040494));
#109116=CARTESIAN_POINT('Ctrl Pts',(-20.093954985742,20.83345402137,-5.39828938423295));
#109117=CARTESIAN_POINT('Ctrl Pts',(-20.1204060637922,20.8110245606152,
-5.39626109780758));
#109118=CARTESIAN_POINT('Ctrl Pts',(-20.1374184930236,20.796123640981,-5.39494957154413));
#109119=CARTESIAN_POINT('Ctrl Pts',(-20.1946136016826,20.7443845712997,
-5.39051143173487));
#109120=CARTESIAN_POINT('Ctrl Pts',(-20.2336122123264,20.7062672595046,
-5.38743606980876));
#109121=CARTESIAN_POINT('Ctrl Pts',(-20.3459462182262,20.587650653921,-5.37834788157023));
#109122=CARTESIAN_POINT('Ctrl Pts',(-20.4145892434939,20.5029591200392,
-5.37248395855781));
#109123=CARTESIAN_POINT('Ctrl Pts',(-20.5445159918407,20.3146748968004,
-5.36003273210043));
#109124=CARTESIAN_POINT('Ctrl Pts',(-20.6041001691299,20.2103915264019,
-5.35345196348697));
#109125=CARTESIAN_POINT('Ctrl Pts',(-20.6585345816035,20.0930125806035,
-5.34578397365668));
#109126=CARTESIAN_POINT('Ctrl Pts',(-20.6624795982953,20.0843532958917,
-5.34521678977393));
#109127=CARTESIAN_POINT('Ctrl Pts',(-20.6682385290129,20.0714831961549,
-5.34437115604783));
#109128=CARTESIAN_POINT('Ctrl Pts',(-20.6700974197501,20.067292472414,-5.34409539078719));
#109129=CARTESIAN_POINT('Ctrl Pts',(-20.6733804847907,20.0598257158696,
-5.34360326047251));
#109130=CARTESIAN_POINT('Ctrl Pts',(-20.6748099943035,20.0565520838434,
-5.34338722563867));
#109131=CARTESIAN_POINT('Ctrl Pts',(-20.6778655301907,20.0495062156744,
-5.34292165319898));
#109132=CARTESIAN_POINT('Ctrl Pts',(-20.679488841256,20.0457329160121,-5.3426719608987));
#109133=CARTESIAN_POINT('Ctrl Pts',(-20.6839392340168,20.0353047155353,
-5.34198093994415));
#109134=CARTESIAN_POINT('Ctrl Pts',(-20.6867431878243,20.0286400915702,
-5.34153824504982));
#109135=CARTESIAN_POINT('Ctrl Pts',(-20.7019150576371,19.9920553797923,
-5.33910281758421));
#109136=CARTESIAN_POINT('Ctrl Pts',(-20.7136287844909,19.9618706883165,
-5.33707410796012));
#109137=CARTESIAN_POINT('Ctrl Pts',(-20.7800606006944,19.7783109685087,
-5.32467155729117));
#109138=CARTESIAN_POINT('Ctrl Pts',(-20.8176233577576,19.6193127826616,
-5.31370520091951));
#109139=CARTESIAN_POINT('Ctrl Pts',(-20.8461452897875,19.3761078302404,
-5.29771008832249));
#109140=CARTESIAN_POINT('Ctrl Pts',(-20.8509571489542,19.2941423626708,
-5.29243882933731));
#109141=CARTESIAN_POINT('Ctrl Pts',(-20.8509997150786,19.2120983429817,
-5.28730630211274));
#109142=CARTESIAN_POINT('Ctrl Pts',(-20.8509997162508,19.212096081275,-5.28730616062444));
#109143=CARTESIAN_POINT('Ctrl Pts',(-20.8510131380423,19.1861728860207,
-5.28568445267461));
#109144=CARTESIAN_POINT('Ctrl Pts',(-20.8505504063707,19.1602505638564,
-5.28407676135363));
#109145=CARTESIAN_POINT('Ctrl Pts',(-20.848973668512,19.1167355904135,-5.2814009878188));
#109146=CARTESIAN_POINT('Ctrl Pts',(-20.8481159291783,19.0991372946227,
-5.28032517195835));
#109147=CARTESIAN_POINT('Ctrl Pts',(-20.8465415722552,19.0734384836758,
-5.27876307643348));
#109148=CARTESIAN_POINT('Ctrl Pts',(-20.8459978401128,19.065328480728,-5.27827141041774));
#109149=CARTESIAN_POINT('Ctrl Pts',(-20.8449526650894,19.0509780126566,
-5.27740366600639));
#109150=CARTESIAN_POINT('Ctrl Pts',(-20.8444702258813,19.0447363008249,
-5.27702699539688));
#109151=CARTESIAN_POINT('Ctrl Pts',(-20.8434611334825,19.0323936642418,
-5.27628361072404));
#109152=CARTESIAN_POINT('Ctrl Pts',(-20.8429356825822,19.0262927050715,
-5.27591686263781));
#109153=CARTESIAN_POINT('Ctrl Pts',(-20.8418361331652,19.0141428099679,
-5.27518787020845));
#109154=CARTESIAN_POINT('Ctrl Pts',(-20.8412624496712,19.008093896263,-5.27482561649629));
#109155=CARTESIAN_POINT('Ctrl Pts',(-20.8398285584689,18.9936373811815,
-5.273961440145));
#109156=CARTESIAN_POINT('Ctrl Pts',(-20.8389440263602,18.9852322548256,
-5.27346028624028));
#109157=CARTESIAN_POINT('Ctrl Pts',(-20.8360988523223,18.9596681874912,
-5.27193979154803));
#109158=CARTESIAN_POINT('Ctrl Pts',(-20.833978522619,18.9425274771431,-5.27092546456861));
#109159=CARTESIAN_POINT('Ctrl Pts',(-20.8260338111836,18.8841729794934,
-5.26748815691785));
#109160=CARTESIAN_POINT('Ctrl Pts',(-20.8192037342712,18.8431045235691,
-5.26509642151262));
#109161=CARTESIAN_POINT('Ctrl Pts',(-20.7899099159963,18.6942361451609,
-5.2564925000987));
#109162=CARTESIAN_POINT('Ctrl Pts',(-20.7602778853229,18.5881303508605,
-5.25049686993618));
#109163=CARTESIAN_POINT('Ctrl Pts',(-20.7225806829213,18.4848899067551,
-5.2445270986103));
#109164=CARTESIAN_POINT('Origin',(-18.734,19.211,0.));
#109165=CARTESIAN_POINT('',(-20.722580615654,18.4848897225317,-4.44630506752222));
#109166=CARTESIAN_POINT('',(-20.7225805995351,18.4848896783871,-4.66702134980151));
#109167=CARTESIAN_POINT('',(-20.7225806137986,18.4848897174502,0.));
#109168=CARTESIAN_POINT('Ctrl Pts',(-20.7225805995351,18.4848896783871,
-4.66702134980151));
#109169=CARTESIAN_POINT('Ctrl Pts',(-20.7691765746879,18.6125009372375,
-4.67446198781971));
#109170=CARTESIAN_POINT('Ctrl Pts',(-20.8033897591205,18.7443251558462,
-4.68169550656151));
#109171=CARTESIAN_POINT('Ctrl Pts',(-20.8309456072997,18.9176173210361,
-4.69152884528225));
#109172=CARTESIAN_POINT('Ctrl Pts',(-20.8360618081696,18.9568542469709,
-4.69377781537916));
#109173=CARTESIAN_POINT('Ctrl Pts',(-20.8416060197797,19.0112165349641,
-4.69695246402515));
#109174=CARTESIAN_POINT('Ctrl Pts',(-20.8429760800736,19.026239521453,-4.69783594811567));
#109175=CARTESIAN_POINT('Ctrl Pts',(-20.8450676744916,19.0522443113994,
-4.69937788773868));
#109176=CARTESIAN_POINT('Ctrl Pts',(-20.8458643545381,19.0632196518257,
-4.70003254732585));
#109177=CARTESIAN_POINT('Ctrl Pts',(-20.8468897380146,19.0790544973032,
-4.70098330192273));
#109178=CARTESIAN_POINT('Ctrl Pts',(-20.8471873277636,19.0839095700263,
-4.70127565419431));
#109179=CARTESIAN_POINT('Ctrl Pts',(-20.8476764825879,19.0923671965251,
-4.70178647414755));
#109180=CARTESIAN_POINT('Ctrl Pts',(-20.84787557773,19.0959693221584,-4.70200452015391));
#109181=CARTESIAN_POINT('Ctrl Pts',(-20.8482735902895,19.1035206038077,
-4.70246266329076));
#109182=CARTESIAN_POINT('Ctrl Pts',(-20.8484706505092,19.1074697979176,
-4.70270285852817));
#109183=CARTESIAN_POINT('Ctrl Pts',(-20.848964202122,19.1179506854619,-4.70334185429437));
#109184=CARTESIAN_POINT('Ctrl Pts',(-20.8492414964507,19.1244831790916,
-4.70374170623453));
#109185=CARTESIAN_POINT('Ctrl Pts',(-20.8502933314094,19.1523033146856,
-4.70545099609565));
#109186=CARTESIAN_POINT('Ctrl Pts',(-20.8507767753185,19.1735998854538,
-4.70677548760904));
#109187=CARTESIAN_POINT('Ctrl Pts',(-20.8509781232032,19.2000731000563,
-4.70843884822058));
#109188=CARTESIAN_POINT('Ctrl Pts',(-20.8509985064406,19.2052471210507,
-4.70876474515027));
#109189=CARTESIAN_POINT('Ctrl Pts',(-20.8510131828851,19.2589278683963,
-4.7121539328038));
#109190=CARTESIAN_POINT('Ctrl Pts',(-20.8493592891371,19.3074176151465,
-4.71528277626609));
#109191=CARTESIAN_POINT('Ctrl Pts',(-20.832613865767,19.5516578066844,-4.73125348668508));
#109192=CARTESIAN_POINT('Ctrl Pts',(-20.7920024870032,19.7447399655909,
-4.74444612677021));
#109193=CARTESIAN_POINT('Ctrl Pts',(-20.7092042732007,19.9742315272296,
-4.75978162116536));
#109194=CARTESIAN_POINT('Ctrl Pts',(-20.6915455002663,20.018446884523,-4.7627264078559));
#109195=CARTESIAN_POINT('Ctrl Pts',(-20.6673796319026,20.0734898719441,
-4.76638235984744));
#109196=CARTESIAN_POINT('Ctrl Pts',(-20.662247765335,20.0849028242802,-4.76713988539493));
#109197=CARTESIAN_POINT('Ctrl Pts',(-20.6539422341594,20.1029443980147,
-4.76833671410158));
#109198=CARTESIAN_POINT('Ctrl Pts',(-20.6508347893938,20.1096030179948,
-4.7687782839561));
#109199=CARTESIAN_POINT('Ctrl Pts',(-20.6449719433175,20.121997100207,-4.76959998081871));
#109200=CARTESIAN_POINT('Ctrl Pts',(-20.6422252384812,20.1277365626624,
-4.76998040307929));
#109201=CARTESIAN_POINT('Ctrl Pts',(-20.6360566866592,20.1404784025923,
-4.77082479695357));
#109202=CARTESIAN_POINT('Ctrl Pts',(-20.6326219523546,20.1474744655748,
-4.77128831416521));
#109203=CARTESIAN_POINT('Ctrl Pts',(-20.6224963103992,20.1678142466625,
-4.77263570211444));
#109204=CARTESIAN_POINT('Ctrl Pts',(-20.6157027253359,20.1811065341187,
-4.77351597527304));
#109205=CARTESIAN_POINT('Ctrl Pts',(-20.558759768144,20.2896716260239,-4.78070600382613));
#109206=CARTESIAN_POINT('Ctrl Pts',(-20.5015469788767,20.3810695699785,
-4.78674995809186));
#109207=CARTESIAN_POINT('Ctrl Pts',(-20.3582447177962,20.575330257831,-4.80001594074904));
#109208=CARTESIAN_POINT('Ctrl Pts',(-20.2688570844537,20.6751648623422,
-4.80713493129164));
#109209=CARTESIAN_POINT('Ctrl Pts',(-20.1586027802066,20.7770348723684,
-4.81548102759713));
#109210=CARTESIAN_POINT('Ctrl Pts',(-20.1464207329849,20.7880307404332,
-4.81639816825224));
#109211=CARTESIAN_POINT('Ctrl Pts',(-20.0943095302242,20.8339796585553,
-4.82030630858372));
#109212=CARTESIAN_POINT('Ctrl Pts',(-20.0532046867677,20.8675636056931,
-4.82335191687341));
#109213=CARTESIAN_POINT('Ctrl Pts',(-20.003943197236,20.9048149355989,-4.82701708480235));
#109214=CARTESIAN_POINT('Ctrl Pts',(-19.9969684920759,20.9100218781408,
-4.82753636384703));
#109215=CARTESIAN_POINT('Ctrl Pts',(-19.9863558179364,20.9178432773327,
-4.82832734833898));
#109216=CARTESIAN_POINT('Ctrl Pts',(-19.982741235141,20.9204895129556,-4.82859689903229));
#109217=CARTESIAN_POINT('Ctrl Pts',(-19.9762361354366,20.9252202554302,
-4.82908232405857));
#109218=CARTESIAN_POINT('Ctrl Pts',(-19.9733487323991,20.9273089522324,
-4.82929790348169));
#109219=CARTESIAN_POINT('Ctrl Pts',(-19.9670610085826,20.9318332408804,
-4.82976761890079));
#109220=CARTESIAN_POINT('Ctrl Pts',(-19.9636587841079,20.9342660177041,
-4.83002193712546));
#109221=CARTESIAN_POINT('Ctrl Pts',(-19.9540761796022,20.9410752778455,
-4.83073863844566));
#109222=CARTESIAN_POINT('Ctrl Pts',(-19.9478795653868,20.9454286516895,
-4.83120255612889));
#109223=CARTESIAN_POINT('Ctrl Pts',(-19.9105753596477,20.9713385450178,
-4.83399748170086));
#109224=CARTESIAN_POINT('Ctrl Pts',(-19.8789196688878,20.9920895292447,
-4.83637782586188));
#109225=CARTESIAN_POINT('Ctrl Pts',(-19.7726333764,21.0577580499199,-4.84435459582894));
#109226=CARTESIAN_POINT('Ctrl Pts',(-19.6957896019241,21.0989177493281,
-4.85009413751182));
#109227=CARTESIAN_POINT('Ctrl Pts',(-19.4572820078323,21.2083203148315,
-4.8674314078552));
#109228=CARTESIAN_POINT('Ctrl Pts',(-19.2894325710295,21.2613520087403,
-4.878941108188));
#109229=CARTESIAN_POINT('Ctrl Pts',(-19.0943196570524,21.2972377133742,
-4.89115222507541));
#109230=CARTESIAN_POINT('Ctrl Pts',(-19.071630994555,21.3010295282562,-4.8925563738403));
#109231=CARTESIAN_POINT('Ctrl Pts',(-19.0394427402428,21.3058710921219,
-4.89452680396895));
#109232=CARTESIAN_POINT('Ctrl Pts',(-19.0299915462981,21.3072273658568,
-4.89510274391011));
#109233=CARTESIAN_POINT('Ctrl Pts',(-19.0146191859176,21.3093273049685,
-4.89603533532351));
#109234=CARTESIAN_POINT('Ctrl Pts',(-19.0087035597605,21.3101099451123,
-4.89639321500522));
#109235=CARTESIAN_POINT('Ctrl Pts',(-18.9963132097617,21.3116959193959,
-4.89714073136632));
#109236=CARTESIAN_POINT('Ctrl Pts',(-18.9898379136981,21.3124943562061,
-4.8975302096955));
#109237=CARTESIAN_POINT('Ctrl Pts',(-18.9744233690518,21.314322745566,-4.89845461297006));
#109238=CARTESIAN_POINT('Ctrl Pts',(-18.9654809949011,21.3153256689991,
-4.89898868062658));
#109239=CARTESIAN_POINT('Ctrl Pts',(-18.9353272527073,21.3185129938539,
-4.90078234748879));
#109240=CARTESIAN_POINT('Ctrl Pts',(-18.9140889178629,21.3204339791789,
-4.90203366321955));
#109241=CARTESIAN_POINT('Ctrl Pts',(-18.7982761315433,21.3291472072138,
-4.90879695704966));
#109242=CARTESIAN_POINT('Ctrl Pts',(-18.7033508508947,21.3299012893246,
-4.91411575375226));
#109243=CARTESIAN_POINT('Ctrl Pts',(-18.4395215028324,21.3142566389095,
-4.92865780770001));
#109244=CARTESIAN_POINT('Ctrl Pts',(-18.2721941620099,21.2839519864042,
-4.93757509024029));
#109245=CARTESIAN_POINT('Ctrl Pts',(-18.0737538983856,21.2227717633758,
-4.94941814878349));
#109246=CARTESIAN_POINT('Ctrl Pts',(-18.0375349713775,21.210521592313,-4.951636370292));
#109247=CARTESIAN_POINT('Ctrl Pts',(-17.9948878103104,21.1947979796451,
-4.95433812312448));
#109248=CARTESIAN_POINT('Ctrl Pts',(-17.9881184371085,21.1922627144682,
-4.95476970105525));
#109249=CARTESIAN_POINT('Ctrl Pts',(-17.9771200668849,21.1880792515937,
-4.95547555231606));
#109250=CARTESIAN_POINT('Ctrl Pts',(-17.9728830883416,21.1864520105893,
-4.95574860210258));
#109251=CARTESIAN_POINT('Ctrl Pts',(-17.9653246456289,21.1835212118046,
-4.95623777778179));
#109252=CARTESIAN_POINT('Ctrl Pts',(-17.9620012144587,21.1822228707841,
-4.95645358885821));
#109253=CARTESIAN_POINT('Ctrl Pts',(-17.9548296228134,21.1794002780123,
-4.95692085923091));
#109254=CARTESIAN_POINT('Ctrl Pts',(-17.9509826995798,21.1778731625931,
-4.95717248481111));
#109255=CARTESIAN_POINT('Ctrl Pts',(-17.940295425491,21.173594306322,-4.9578742035031));
#109256=CARTESIAN_POINT('Ctrl Pts',(-17.9334650121597,21.17081812737,-4.95832573192174));
#109257=CARTESIAN_POINT('Ctrl Pts',(-17.8947278876086,21.1548373708101,
-4.96090325753113));
#109258=CARTESIAN_POINT('Ctrl Pts',(-17.8631354718184,21.1408901674283,
-4.96307025179287));
#109259=CARTESIAN_POINT('Ctrl Pts',(-17.7643048239258,21.0943383068067,
-4.97002488772784));
#109260=CARTESIAN_POINT('Ctrl Pts',(-17.6984466828193,21.0589447247882,
-4.97492054677147));
#109261=CARTESIAN_POINT('Ctrl Pts',(-17.4687641306777,20.9193692854144,
-4.99264725939744));
#109262=CARTESIAN_POINT('Ctrl Pts',(-17.3175289671192,20.7962409338101,
-5.00547118345634));
#109263=CARTESIAN_POINT('Ctrl Pts',(-17.1707717429345,20.6387440610431,
-5.01869701004288));
#109264=CARTESIAN_POINT('Ctrl Pts',(-17.1565955201768,20.6230661618369,
-5.01998563759317));
#109265=CARTESIAN_POINT('Ctrl Pts',(-17.1371815480636,20.6009383928977,
-5.02176659476284));
#109266=CARTESIAN_POINT('Ctrl Pts',(-17.1317437440633,20.594666433024,-5.02226726499616));
#109267=CARTESIAN_POINT('Ctrl Pts',(-17.1224153529102,20.5837783383507,
-5.02312938811789));
#109268=CARTESIAN_POINT('Ctrl Pts',(-17.1185073911103,20.5791772811945,
-5.02349155747948));
#109269=CARTESIAN_POINT('Ctrl Pts',(-17.110450064857,20.5696082967367,-5.02424037796577));
#109270=CARTESIAN_POINT('Ctrl Pts',(-17.1063036925789,20.5646379235632,
-5.02462690412941));
#109271=CARTESIAN_POINT('Ctrl Pts',(-17.096636871529,20.5529413920255,-5.02553086844356));
#109272=CARTESIAN_POINT('Ctrl Pts',(-17.09113494064,20.5462000278192,-5.02604755105093));
#109273=CARTESIAN_POINT('Ctrl Pts',(-17.0733642628319,20.5241499597974,
-5.02772372748138));
#109274=CARTESIAN_POINT('Ctrl Pts',(-17.0612664883158,20.5087043213395,
-5.0288763675597));
#109275=CARTESIAN_POINT('Ctrl Pts',(-17.0002432388907,20.4285223517193,
-5.03475463679033));
#109276=CARTESIAN_POINT('Ctrl Pts',(-16.9548515451049,20.3611765254235,
-5.03934111643026));
#109277=CARTESIAN_POINT('Ctrl Pts',(-16.8273869862402,20.1463849159155,
-5.0531834560534));
#109278=CARTESIAN_POINT('Ctrl Pts',(-16.7589776858456,19.9916389950774,
-5.06205516023817));
#109279=CARTESIAN_POINT('Ctrl Pts',(-16.6938951184651,19.778943811717,-5.07455912022939));
#109280=CARTESIAN_POINT('Ctrl Pts',(-16.6801120430088,19.726879167981,-5.07764762117836));
#109281=CARTESIAN_POINT('Ctrl Pts',(-16.6664168246377,19.6658243312195,
-5.08136069197208));
#109282=CARTESIAN_POINT('Ctrl Pts',(-16.6645570906476,19.6572862291036,
-5.08188199393419));
#109283=CARTESIAN_POINT('Ctrl Pts',(-16.6618224896651,19.6443468588404,
-5.08267546015003));
#109284=CARTESIAN_POINT('Ctrl Pts',(-16.6609086438301,19.6399537999906,
-5.08294544936315));
#109285=CARTESIAN_POINT('Ctrl Pts',(-16.6592939844144,19.6320660906188,
-5.08343134068244));
#109286=CARTESIAN_POINT('Ctrl Pts',(-16.6585880239935,19.6285725485843,
-5.08364694537929));
#109287=CARTESIAN_POINT('Ctrl Pts',(-16.6570738986891,19.6209809947263,
-5.08411633735494));
#109288=CARTESIAN_POINT('Ctrl Pts',(-16.6562690491018,19.6168824230329,
-5.08437030479705));
#109289=CARTESIAN_POINT('Ctrl Pts',(-16.6540440284857,19.6053717945954,
-5.08508504842686));
#109290=CARTESIAN_POINT('Ctrl Pts',(-16.6526513722592,19.5979545731375,
-5.08554734605958));
#109291=CARTESIAN_POINT('Ctrl Pts',(-16.6445949017933,19.5537440623794,
-5.08831253120777));
#109292=CARTESIAN_POINT('Ctrl Pts',(-16.6388676284481,19.5167893152632,
-5.09066356707414));
#109293=CARTESIAN_POINT('Ctrl Pts',(-16.6232937521079,19.3950825083755,
-5.09849443678796));
#109294=CARTESIAN_POINT('Ctrl Pts',(-16.6175911268477,19.3098880430378,
-5.10411213130873));
#109295=CARTESIAN_POINT('Ctrl Pts',(-16.6159018569454,19.0467103331915,
-5.12149861875124));
#109296=CARTESIAN_POINT('Ctrl Pts',(-16.6371840536535,18.8693596482302,
-5.13318742502556));
#109297=CARTESIAN_POINT('Ctrl Pts',(-16.6859509173027,18.6746195928484,
-5.14554188538172));
#109298=CARTESIAN_POINT('Ctrl Pts',(-16.6918474567328,18.6525897205716,
-5.14693377490617));
#109299=CARTESIAN_POINT('Ctrl Pts',(-16.7007074227669,18.6215079853256,
-5.14889014403152));
#109300=CARTESIAN_POINT('Ctrl Pts',(-16.7033775721471,18.6123748250191,
-5.14946409630717));
#109301=CARTESIAN_POINT('Ctrl Pts',(-16.7078205653842,18.5975495661295,
-5.15039434856947));
#109302=CARTESIAN_POINT('Ctrl Pts',(-16.7095560126518,18.5918464816418,
-5.15075186458501));
#109303=CARTESIAN_POINT('Ctrl Pts',(-16.7132427569742,18.5799122102266,
-5.15149931912294));
#109304=CARTESIAN_POINT('Ctrl Pts',(-16.7151988422498,18.5736825590166,
-5.15188909623111));
#109305=CARTESIAN_POINT('Ctrl Pts',(-16.7199277478882,18.5588624025487,
-5.15281547913382));
#109306=CARTESIAN_POINT('Ctrl Pts',(-16.7227267666955,18.550280341164,-5.15335121773151));
#109307=CARTESIAN_POINT('Ctrl Pts',(-16.7323753618707,18.5213263613745,
-5.15515647736733));
#109308=CARTESIAN_POINT('Ctrl Pts',(-16.7394803852505,18.501040510862,-5.15641756600282));
#109309=CARTESIAN_POINT('Ctrl Pts',(-16.8087628236532,18.3124839420369,
-5.16811368785506));
#109310=CARTESIAN_POINT('Ctrl Pts',(-16.8917804855617,18.152650556414,-5.1777525891409));
#109311=CARTESIAN_POINT('Ctrl Pts',(-17.0626408164904,17.9060925369895,
-5.1940778535634));
#109312=CARTESIAN_POINT('Ctrl Pts',(-17.1396434648458,17.8130573118082,
-5.20069209329022));
#109313=CARTESIAN_POINT('Ctrl Pts',(-17.2307836023472,17.7203224366964,
-5.2083981773159));
#109314=CARTESIAN_POINT('Ctrl Pts',(-17.2374837298306,17.71359618625,-5.20896408525885));
#109315=CARTESIAN_POINT('Ctrl Pts',(-17.2474829264602,17.7036921452285,
-5.20980817647847));
#109316=CARTESIAN_POINT('Ctrl Pts',(-17.2507475386143,17.7004795221945,
-5.21008368936304));
#109317=CARTESIAN_POINT('Ctrl Pts',(-17.256576471903,17.6947805315728,-5.2105755435686));
#109318=CARTESIAN_POINT('Ctrl Pts',(-17.2591366849665,17.6922900344208,
-5.21079155609991));
#109319=CARTESIAN_POINT('Ctrl Pts',(-17.2646568836004,17.6869472769438,
-5.2112572794998));
#109320=CARTESIAN_POINT('Ctrl Pts',(-17.2676188337563,17.6840971966141,
-5.21150714611296));
#109321=CARTESIAN_POINT('Ctrl Pts',(-17.2758230784177,17.6762487069792,
-5.21219912973855));
#109322=CARTESIAN_POINT('Ctrl Pts',(-17.281082697005,17.671268603545,-5.21264261914473));
#109323=CARTESIAN_POINT('Ctrl Pts',(-17.310127522781,17.6440486546061,-5.21509042629719));
#109324=CARTESIAN_POINT('Ctrl Pts',(-17.33439648886,17.6223341786083,-5.21713114492648));
#109325=CARTESIAN_POINT('Ctrl Pts',(-17.4828610820487,17.4955392507688,
-5.2295377243308));
#109326=CARTESIAN_POINT('Ctrl Pts',(-17.6183289249666,17.4045027926796,
-5.24049306500456));
#109327=CARTESIAN_POINT('Ctrl Pts',(-17.8667114725002,17.2762770854998,
-5.25875157455107));
#109328=CARTESIAN_POINT('Ctrl Pts',(-17.9748111309381,17.2313580573907,
-5.2661945320723));
#109329=CARTESIAN_POINT('Ctrl Pts',(-18.0996627134878,17.1912206345028,
-5.27420196279347));
#109330=CARTESIAN_POINT('Ctrl Pts',(-18.1132868275275,17.1869921809681,
-5.27506841447953));
#109331=CARTESIAN_POINT('Ctrl Pts',(-18.1350455017289,17.1804794099915,
-5.27644077317913));
#109332=CARTESIAN_POINT('Ctrl Pts',(-18.1431526121031,17.1781055795014,
-5.27694959534783));
#109333=CARTESIAN_POINT('Ctrl Pts',(-18.1574799708308,17.1740033554253,
-5.27784446364162));
#109334=CARTESIAN_POINT('Ctrl Pts',(-18.1636942828096,17.1722547818784,
-5.27823116354203));
#109335=CARTESIAN_POINT('Ctrl Pts',(-18.1765680460805,17.1686958501921,
-5.27902933029003));
#109336=CARTESIAN_POINT('Ctrl Pts',(-18.1832285533561,17.1668895727313,
-5.27944066052309));
#109337=CARTESIAN_POINT('Ctrl Pts',(-18.2003562700842,17.1623344624698,
-5.28049432529007));
#109338=CARTESIAN_POINT('Ctrl Pts',(-18.2108360221574,17.1596332424422,
-5.281135113029));
#109339=CARTESIAN_POINT('Ctrl Pts',(-18.2547329082635,17.1486768247096,
-5.28380335969078));
#109340=CARTESIAN_POINT('Ctrl Pts',(-18.2883292540094,17.1411566220439,
-5.28580711839118));
#109341=CARTESIAN_POINT('Ctrl Pts',(-18.3763995201453,17.1236869300678,
-5.2909721489968));
#109342=CARTESIAN_POINT('Ctrl Pts',(-18.4311076203829,17.1150489474822,
-5.29409360975679));
#109343=CARTESIAN_POINT('Ctrl Pts',(-18.5949003264753,17.0957355807034,
-5.30326226489374));
#109344=CARTESIAN_POINT('Ctrl Pts',(-18.7045407716048,17.091371425147,-5.30916081290938));
#109345=CARTESIAN_POINT('Ctrl Pts',(-18.8742915571145,17.0977928571337,
-5.31841054153964));
#109346=CARTESIAN_POINT('Ctrl Pts',(-18.9344296986124,17.1026467482511,
-5.32171287893654));
#109347=CARTESIAN_POINT('Ctrl Pts',(-19.0521169367126,17.1172264727426,
-5.32835560136133));
#109348=CARTESIAN_POINT('Ctrl Pts',(-19.1096323309069,17.126777116787,-5.33168831918916));
#109349=CARTESIAN_POINT('Ctrl Pts',(-19.1753930486656,17.1405071843618,
-5.3356734271783));
#109350=CARTESIAN_POINT('Ctrl Pts',(-19.184099648586,17.1423824367301,-5.33620462067294));
#109351=CARTESIAN_POINT('Ctrl Pts',(-19.1972096009958,17.1452927787057,
-5.33701021233555));
#109352=CARTESIAN_POINT('Ctrl Pts',(-19.2016220191159,17.1462871616305,
-5.33728233499326));
#109353=CARTESIAN_POINT('Ctrl Pts',(-19.2095082259081,17.1480909740058,
-5.33777051039889));
#109354=CARTESIAN_POINT('Ctrl Pts',(-19.2129831854314,17.1488950486842,
-5.33798625359744));
#109355=CARTESIAN_POINT('Ctrl Pts',(-19.2204970850207,17.1506537159885,
-5.33845414236567));
#109356=CARTESIAN_POINT('Ctrl Pts',(-19.2245351991588,17.1516113913403,
-5.33870645832793));
#109357=CARTESIAN_POINT('Ctrl Pts',(-19.2357892121002,17.1543153606621,
-5.33941200890397));
#109358=CARTESIAN_POINT('Ctrl Pts',(-19.2429986971229,17.1560877289673,
-5.33986670393191));
#109359=CARTESIAN_POINT('Ctrl Pts',(-19.2844761458584,17.1665161440709,
-5.34249767490051));
#109360=CARTESIAN_POINT('Ctrl Pts',(-19.3185302414702,17.1759908398913,
-5.34471692407298));
#109361=CARTESIAN_POINT('Ctrl Pts',(-19.4265704926763,17.2089857628015,
-5.35191368388791));
#109362=CARTESIAN_POINT('Ctrl Pts',(-19.4995040794923,17.2357236234289,
-5.357007154015));
#109363=CARTESIAN_POINT('Ctrl Pts',(-19.7408833899257,17.3395940313429,
-5.37434910975497));
#109364=CARTESIAN_POINT('Ctrl Pts',(-19.9006689751638,17.434800452723,-5.3865722435985));
#109365=CARTESIAN_POINT('Ctrl Pts',(-20.0654595660431,17.5649390226409,
-5.39951917268111));
#109366=CARTESIAN_POINT('Ctrl Pts',(-20.0846094189555,17.5806148933025,
-5.40103147641083));
#109367=CARTESIAN_POINT('Ctrl Pts',(-20.1109857464919,17.6029900146471,
-5.40312631445175));
#109368=CARTESIAN_POINT('Ctrl Pts',(-20.1184464140189,17.6094089189606,
-5.40372021400209));
#109369=CARTESIAN_POINT('Ctrl Pts',(-20.1303991086684,17.6198385419045,
-5.4046739996304));
#109370=CARTESIAN_POINT('Ctrl Pts',(-20.1349191947848,17.6238167505714,
-5.40503522572458));
#109371=CARTESIAN_POINT('Ctrl Pts',(-20.1439745301161,17.6318553334297,
-5.40576000532202));
#109372=CARTESIAN_POINT('Ctrl Pts',(-20.148509362761,17.6359160919527,-5.40612353770611));
#109373=CARTESIAN_POINT('Ctrl Pts',(-20.1592223937094,17.645592757452,-5.40698373637908));
#109374=CARTESIAN_POINT('Ctrl Pts',(-20.1653850385675,17.651225791672,-5.40747967371305));
#109375=CARTESIAN_POINT('Ctrl Pts',(-20.1845723145197,17.6689736185084,
-5.40902740829496));
#109376=CARTESIAN_POINT('Ctrl Pts',(-20.1974778979819,17.681216397125,-5.41007373642303));
#109377=CARTESIAN_POINT('Ctrl Pts',(-20.2271757093824,17.7101088026172,
-5.41249526894861));
#109378=CARTESIAN_POINT('Ctrl Pts',(-20.243846498808,17.7268801603108,-5.41386514614617));
#109379=CARTESIAN_POINT('Ctrl Pts',(-20.3005066310864,17.7858251661314,
-5.41856358981311));
#109380=CARTESIAN_POINT('Ctrl Pts',(-20.3390395385547,17.829365044568,-5.42183366041554));
#109381=CARTESIAN_POINT('Ctrl Pts',(-20.4797765659393,18.0022360320717,
-5.43419924150301));
#109382=CARTESIAN_POINT('Ctrl Pts',(-20.5685325627749,18.1417338121171,
-5.44288447751858));
#109383=CARTESIAN_POINT('Ctrl Pts',(-20.6659521660254,18.3433873181785,
-5.4554206781514));
#109384=CARTESIAN_POINT('Ctrl Pts',(-20.689446336058,18.3977231612727,-5.45880237458842));
#109385=CARTESIAN_POINT('Ctrl Pts',(-20.713832068521,18.4613108250018,-5.46284207578789));
#109386=CARTESIAN_POINT('Ctrl Pts',(-20.716979372528,18.4696757251889,-5.46337510271013));
#109387=CARTESIAN_POINT('Ctrl Pts',(-20.7209131560224,18.4803352400332,
-5.46405668761308));
#109388=CARTESIAN_POINT('Ctrl Pts',(-20.7217488443111,18.4826117705353,
-5.46420238754676));
#109389=CARTESIAN_POINT('Ctrl Pts',(-20.7225806137986,18.4848897174502,
-5.46434831804488));
#109390=CARTESIAN_POINT('Ctrl Pts',(-20.7225806829213,18.4848899067551,
-5.24452709861031));
#109391=CARTESIAN_POINT('Ctrl Pts',(-20.7014125433041,18.4269172192414,
-5.24117488823769));
#109392=CARTESIAN_POINT('Ctrl Pts',(-20.6777012897646,18.3698481845845,
-5.23782825408735));
#109393=CARTESIAN_POINT('Ctrl Pts',(-20.6249328374919,18.2570646671581,
-5.23098491305862));
#109394=CARTESIAN_POINT('Ctrl Pts',(-20.5958563006109,18.2014904246063,
-5.22749307031487));
#109395=CARTESIAN_POINT('Ctrl Pts',(-20.5488220101447,18.1205568429588,
-5.22210871730596));
#109396=CARTESIAN_POINT('Ctrl Pts',(-20.5327016390253,18.0941663534545,
-5.22030291401821));
#109397=CARTESIAN_POINT('Ctrl Pts',(-20.5121619838508,18.0621397956072,
-5.21803698818975));
#109398=CARTESIAN_POINT('Ctrl Pts',(-20.5082836603195,18.0561591886834,
-5.21761058962982));
#109399=CARTESIAN_POINT('Ctrl Pts',(-20.5021352906482,18.0467821156106,
-5.21693669652013));
#109400=CARTESIAN_POINT('Ctrl Pts',(-20.4998854489977,18.0433723758248,
-5.21669053392754));
#109401=CARTESIAN_POINT('Ctrl Pts',(-20.4956478283958,18.0369903259839,
-5.2162276453178));
#109402=CARTESIAN_POINT('Ctrl Pts',(-20.4936623833455,18.0340165328543,
-5.21601107548901));
#109403=CARTESIAN_POINT('Ctrl Pts',(-20.4890946288609,18.0272123569264,
-5.215513541008));
#109404=CARTESIAN_POINT('Ctrl Pts',(-20.4865073169418,18.0233853978325,
-5.21523224147417));
#109405=CARTESIAN_POINT('Ctrl Pts',(-20.478451206119,18.0115530507845,-5.21435803667393));
#109406=CARTESIAN_POINT('Ctrl Pts',(-20.47294001505,18.0035768718607,-5.21376236557274));
#109407=CARTESIAN_POINT('Ctrl Pts',(-20.4106715053545,17.9147681654412,
-5.20706098688228));
#109408=CARTESIAN_POINT('Ctrl Pts',(-20.3483849544847,17.8379738181674,
-5.20062772543763));
#109409=CARTESIAN_POINT('Ctrl Pts',(-20.1664593538686,17.643234191429,-5.18307327694679));
#109410=CARTESIAN_POINT('Ctrl Pts',(-20.0377574008985,17.5346758714274,
-5.17192757325268));
#109411=CARTESIAN_POINT('Ctrl Pts',(-19.8712093636095,17.425099666453,-5.15940141897003));
#109412=CARTESIAN_POINT('Ctrl Pts',(-19.8444569313007,17.408343430679,-5.15743879867111));
#109413=CARTESIAN_POINT('Ctrl Pts',(-19.8041717225822,17.3843483202024,
-5.1545552746295));
#109414=CARTESIAN_POINT('Ctrl Pts',(-19.7909197488194,17.3766487416391,
-5.15361796646791));
#109415=CARTESIAN_POINT('Ctrl Pts',(-19.7666473255767,17.3628965021666,
-5.15192126657722));
#109416=CARTESIAN_POINT('Ctrl Pts',(-19.7556544359079,17.3567968660354,
-5.15116021287474));
#109417=CARTESIAN_POINT('Ctrl Pts',(-19.7382624489895,17.3473481873539,
-5.14996752839326));
#109418=CARTESIAN_POINT('Ctrl Pts',(-19.7318995657547,17.343933422744,-5.14953355739942));
#109419=CARTESIAN_POINT('Ctrl Pts',(-19.7254731426295,17.3405267951213,
-5.14909761334312));
#109420=CARTESIAN_POINT('Ctrl Pts',(-19.7254270105499,17.3405023428304,
-5.14909448404078));
#109421=CARTESIAN_POINT('Ctrl Pts',(-19.7253331203011,17.3404525807897,
-5.14908811538135));
#109422=CARTESIAN_POINT('Ctrl Pts',(-19.7252853611042,17.3404272706519,
-5.14908487596325));
#109423=CARTESIAN_POINT('Ctrl Pts',(-19.7251881573754,17.3403757619958,
-5.14907828308036));
#109424=CARTESIAN_POINT('Ctrl Pts',(-19.7251387117589,17.3403495630709,
-5.14907492955136));
#109425=CARTESIAN_POINT('Ctrl Pts',(-19.7250380735856,17.3402962447093,
-5.1490681042969));
#109426=CARTESIAN_POINT('Ctrl Pts',(-19.7249868802129,17.3402691250206,
-5.14906463252616));
#109427=CARTESIAN_POINT('Ctrl Pts',(-19.7248826827138,17.340213931874,-5.14905756649119));
#109428=CARTESIAN_POINT('Ctrl Pts',(-19.7248296777858,17.3401858581848,
-5.14905397218336));
#109429=CARTESIAN_POINT('Ctrl Pts',(-19.7247217910763,17.3401287226155,
-5.14904665662473));
#109430=CARTESIAN_POINT('Ctrl Pts',(-19.7246669085466,17.3400996605466,
-5.14904293533475));
#109431=CARTESIAN_POINT('Ctrl Pts',(-19.7245551981646,17.3400405125918,
-5.14903536120447));
#109432=CARTESIAN_POINT('Ctrl Pts',(-19.724498369524,17.340010426511,-5.14903150832312));
#109433=CARTESIAN_POINT('Ctrl Pts',(-19.7243826959561,17.3399491936393,
-5.14902366623662));
#109434=CARTESIAN_POINT('Ctrl Pts',(-19.7243238502478,17.3399180466738,
-5.14901967699182));
#109435=CARTESIAN_POINT('Ctrl Pts',(-19.7242040688028,17.3398546537271,
-5.14901155721985));
#109436=CARTESIAN_POINT('Ctrl Pts',(-19.724143132582,17.3398224077461,-5.14900742667415));
#109437=CARTESIAN_POINT('Ctrl Pts',(-19.7240190939745,17.3397567772569,
-5.14899901918283));
#109438=CARTESIAN_POINT('Ctrl Pts',(-19.7239559908874,17.3397233926534,
-5.14899474220509));
#109439=CARTESIAN_POINT('Ctrl Pts',(-19.7238275395831,17.3396554439795,
-5.14898603654433));
#109440=CARTESIAN_POINT('Ctrl Pts',(-19.7237621908733,17.3396208799438,
-5.14898160784439));
#109441=CARTESIAN_POINT('Ctrl Pts',(-19.7236291644548,17.3395505289426,
-5.14897259310541));
#109442=CARTESIAN_POINT('Ctrl Pts',(-19.7235614894262,17.3395147437117,
-5.14896800726576));
#109443=CARTESIAN_POINT('Ctrl Pts',(-19.7234348804973,17.3394478041748,
-5.1489594283989));
#109444=CARTESIAN_POINT('Ctrl Pts',(-19.7233759456494,17.3394166482323,
-5.14895543524413));
#109445=CARTESIAN_POINT('Ctrl Pts',(-19.7232483249391,17.3393491891808,
-5.14894678868114));
#109446=CARTESIAN_POINT('Ctrl Pts',(-19.7231796374951,17.3393128865111,
-5.14894213523691));
#109447=CARTESIAN_POINT('Ctrl Pts',(-19.7230309151709,17.3392342943013,
-5.14893206016565));
#109448=CARTESIAN_POINT('Ctrl Pts',(-19.7229508786399,17.3391920056183,
-5.14892663852325));
#109449=CARTESIAN_POINT('Ctrl Pts',(-19.7227776081786,17.3391004693942,
-5.1489149020452));
#109450=CARTESIAN_POINT('Ctrl Pts',(-19.7226843726364,17.3390512233444,
-5.14890858723104));
#109451=CARTESIAN_POINT('Ctrl Pts',(-19.722482564125,17.3389446494573,-5.14889491987937));
#109452=CARTESIAN_POINT('Ctrl Pts',(-19.7223739893192,17.3388873238205,
-5.14888756739431));
#109453=CARTESIAN_POINT('Ctrl Pts',(-19.722139031633,17.3387632963257,-5.1488716579522));
#109454=CARTESIAN_POINT('Ctrl Pts',(-19.7220126472998,17.3386965979849,
-5.14886310113573));
#109455=CARTESIAN_POINT('Ctrl Pts',(-19.7217267234242,17.338545740914,-5.14884374480244));
#109456=CARTESIAN_POINT('Ctrl Pts',(-19.7215671798329,17.3384615897524,
-5.14883294555272));
#109457=CARTESIAN_POINT('Ctrl Pts',(-19.7156957213096,17.3353656519479,
-5.14843556941465));
#109458=CARTESIAN_POINT('Ctrl Pts',(-19.7099700189701,17.3323799691455,
-5.14804992011967));
#109459=CARTESIAN_POINT('Ctrl Pts',(-19.696713171875,17.3255441165983,-5.14716126293205));
#109460=CARTESIAN_POINT('Ctrl Pts',(-19.6891724024991,17.3217127734971,
-5.14665892224424));
#109461=CARTESIAN_POINT('Ctrl Pts',(-19.6688198146561,17.3115249530066,
-5.14531140744099));
#109462=CARTESIAN_POINT('Ctrl Pts',(-19.6559660706415,17.3052528710352,
-5.14446918099384));
#109463=CARTESIAN_POINT('Ctrl Pts',(-19.5375059312837,17.2489283902529,
-5.13678499774756));
#109464=CARTESIAN_POINT('Ctrl Pts',(-19.4279819250668,17.207567661172,-5.13025988143086));
#109465=CARTESIAN_POINT('Ctrl Pts',(-19.1589193143186,17.1306918040814,
-5.1149410087118));
#109466=CARTESIAN_POINT('Ctrl Pts',(-18.9976237312764,17.1041708180831,
-5.10633095074161));
#109467=CARTESIAN_POINT('Ctrl Pts',(-18.8026648418282,17.0948676944578,
-5.09512111302561));
#109468=CARTESIAN_POINT('Ctrl Pts',(-18.7703956710023,17.0940668659299,
-5.09323823541426));
#109469=CARTESIAN_POINT('Ctrl Pts',(-18.7308991355655,17.0939899464402,
-5.09088648674902));
#109470=CARTESIAN_POINT('Ctrl Pts',(-18.723675515846,17.0940128522262,-5.09045443858482));
#109471=CARTESIAN_POINT('Ctrl Pts',(-18.7123462099846,17.0941067636048,
-5.08977360226996));
#109472=CARTESIAN_POINT('Ctrl Pts',(-18.7082402941069,17.0941527457534,
-5.0895261921682));
#109473=CARTESIAN_POINT('Ctrl Pts',(-18.7005624824496,17.0942610706968,
-5.08906226477376));
#109474=CARTESIAN_POINT('Ctrl Pts',(-18.6969906018764,17.0943205093357,
-5.08884591155034));
#109475=CARTESIAN_POINT('Ctrl Pts',(-18.6888329401159,17.0944769135551,
-5.08835060330778));
#109476=CARTESIAN_POINT('Ctrl Pts',(-18.6842473284257,17.094579741755,-5.08807132460394));
#109477=CARTESIAN_POINT('Ctrl Pts',(-18.6701380455842,17.0949420095614,
-5.08720946956608));
#109478=CARTESIAN_POINT('Ctrl Pts',(-18.6606159162784,17.0952508332552,
-5.0866242366605));
#109479=CARTESIAN_POINT('Ctrl Pts',(-18.5315791820128,17.1003079053782,
-5.07864800885465));
#109480=CARTESIAN_POINT('Ctrl Pts',(-18.4126873485253,17.1151119175829,
-5.07078011330997));
#109481=CARTESIAN_POINT('Ctrl Pts',(-18.1890882319371,17.1624310789412,
-5.05568137314921));
#109482=CARTESIAN_POINT('Ctrl Pts',(-18.0843720809438,17.1931916586331,
-5.04847842249467));
#109483=CARTESIAN_POINT('Ctrl Pts',(-17.9123334388415,17.2585185535274,
-5.03665456987097));
#109484=CARTESIAN_POINT('Ctrl Pts',(-17.843642548131,17.2888695436925,-5.0319334881336));
#109485=CARTESIAN_POINT('Ctrl Pts',(-17.7599263962632,17.3313129614492,
-5.02618353657497));
#109486=CARTESIAN_POINT('Ctrl Pts',(-17.743264689758,17.3400413341629,-5.02503916606737));
#109487=CARTESIAN_POINT('Ctrl Pts',(-17.7191970199992,17.3530610639241,
-5.02338572328093));
#109488=CARTESIAN_POINT('Ctrl Pts',(-17.7116976121879,17.357176920622,-5.02287045509809));
#109489=CARTESIAN_POINT('Ctrl Pts',(-17.6985884661601,17.3644752782391,
-5.02196958001907));
#109490=CARTESIAN_POINT('Ctrl Pts',(-17.6929679781688,17.3676381463661,
-5.02158327719278));
#109491=CARTESIAN_POINT('Ctrl Pts',(-17.6820791682244,17.3738313903971,
-5.02083472989412));
#109492=CARTESIAN_POINT('Ctrl Pts',(-17.6768092755527,17.3768588631839,
-5.0204723858907));
#109493=CARTESIAN_POINT('Ctrl Pts',(-17.6642373732314,17.3841534143028,
-5.01960777290718));
#109494=CARTESIAN_POINT('Ctrl Pts',(-17.6569477165769,17.3884416587577,
-5.01910627444909));
#109495=CARTESIAN_POINT('Ctrl Pts',(-17.6307061322636,17.4040910695468,
-5.01730018326313));
#109496=CARTESIAN_POINT('Ctrl Pts',(-17.6119062466824,17.4157053432614,
-5.01600481466161));
#109497=CARTESIAN_POINT('Ctrl Pts',(-17.4368626908648,17.527668504883,-5.0039196874903));
#109498=CARTESIAN_POINT('Ctrl Pts',(-17.2942816929144,17.6478661852732,
-4.99398766922138));
#109499=CARTESIAN_POINT('Ctrl Pts',(-17.115269924403,17.8443201817385,-4.97949851819132));
#109500=CARTESIAN_POINT('Ctrl Pts',(-17.0647433244534,17.9065150704033,
-4.97509479861646));
#109501=CARTESIAN_POINT('Ctrl Pts',(-16.996778301074,18.0006089018065,-4.96845519607244));
#109502=CARTESIAN_POINT('Ctrl Pts',(-16.9764418056879,18.0303329481552,
-4.96636050073923));
#109503=CARTESIAN_POINT('Ctrl Pts',(-16.9528178321274,18.0668257068903,
-4.96377343218186));
#109504=CARTESIAN_POINT('Ctrl Pts',(-16.9487943018253,18.0731136526,-4.96332712398541));
#109505=CARTESIAN_POINT('Ctrl Pts',(-16.9425810720058,18.0829377134332,
-4.96262877614957));
#109506=CARTESIAN_POINT('Ctrl Pts',(-16.9403683486528,18.086459295289,-4.96237823389833));
#109507=CARTESIAN_POINT('Ctrl Pts',(-16.9362777748711,18.0930122911458,
-4.96191159038382));
#109508=CARTESIAN_POINT('Ctrl Pts',(-16.9343972010295,18.0960419374689,
-4.9616956726169));
#109509=CARTESIAN_POINT('Ctrl Pts',(-16.9301550168041,18.1029148838485,
-4.96120546042073));
#109510=CARTESIAN_POINT('Ctrl Pts',(-16.927798042358,18.1067609699994,-4.96093086834725));
#109511=CARTESIAN_POINT('Ctrl Pts',(-16.921743663612,18.1167116884139,-4.96021979833486));
#109512=CARTESIAN_POINT('Ctrl Pts',(-16.9180648406238,18.1228274809193,
-4.95978215306416));
#109513=CARTESIAN_POINT('Ctrl Pts',(-16.8956530086545,18.1605157820108,
-4.95708197459196));
#109514=CARTESIAN_POINT('Ctrl Pts',(-16.8777141751826,18.1925505340961,
-4.95477313849696));
#109515=CARTESIAN_POINT('Ctrl Pts',(-16.7812829005166,18.3757742940944,
-4.94155914478204));
#109516=CARTESIAN_POINT('Ctrl Pts',(-16.7204309672991,18.5355380342309,
-4.93006551385103));
#109517=CARTESIAN_POINT('Ctrl Pts',(-16.6563716337719,18.7935463910746,
-4.91278849619484));
#109518=CARTESIAN_POINT('Ctrl Pts',(-16.6396560513731,18.8876815297255,
-4.90672131456489));
#109519=CARTESIAN_POINT('Ctrl Pts',(-16.6270441935145,19.0039146054185,
-4.89953963636454));
#109520=CARTESIAN_POINT('Ctrl Pts',(-16.6250580902273,19.025228083011,-4.89823496983708));
#109521=CARTESIAN_POINT('Ctrl Pts',(-16.6226955351678,19.0555533177765,
-4.89639541802049));
#109522=CARTESIAN_POINT('Ctrl Pts',(-16.622052933817,19.0645424709978,-4.89585221337528));
#109523=CARTESIAN_POINT('Ctrl Pts',(-16.6210439409712,19.0800485174159,
-4.89491871662535));
#109524=CARTESIAN_POINT('Ctrl Pts',(-16.6206502548811,19.0865634520563,
-4.89452757288727));
#109525=CARTESIAN_POINT('Ctrl Pts',(-16.6199544827135,19.0990351691825,
-4.8937808047889));
#109526=CARTESIAN_POINT('Ctrl Pts',(-16.6196474293291,19.1049916016644,
-4.89342502824345));
#109527=CARTESIAN_POINT('Ctrl Pts',(-16.6189150546905,19.1204708000555,
-4.89250269354047));
#109528=CARTESIAN_POINT('Ctrl Pts',(-16.6185288673296,19.1299953503005,
-4.89193736605631));
#109529=CARTESIAN_POINT('Ctrl Pts',(-16.6174336269316,19.162415280981,-4.89002031478329));
#109530=CARTESIAN_POINT('Ctrl Pts',(-16.6170318187375,19.1853199238369,
-4.88867819975365));
#109531=CARTESIAN_POINT('Ctrl Pts',(-16.6167705015412,19.3848364057372,
-4.87708360917363));
#109532=CARTESIAN_POINT('Ctrl Pts',(-16.6386380161249,19.5607779961173,
-4.86759334118126));
#109533=CARTESIAN_POINT('Ctrl Pts',(-16.7033214164755,19.8155383417283,
-4.85328915377275));
#109534=CARTESIAN_POINT('Ctrl Pts',(-16.7296216245108,19.8977219923509,
-4.84856684807259));
#109535=CARTESIAN_POINT('Ctrl Pts',(-16.7744878253125,20.0131324782004,
-4.84149568318189));
#109536=CARTESIAN_POINT('Ctrl Pts',(-16.7890513645391,20.0478266770472,
-4.83930994886156));
#109537=CARTESIAN_POINT('Ctrl Pts',(-16.8076413156073,20.0890024920954,
-4.8366219235295));
#109538=CARTESIAN_POINT('Ctrl Pts',(-16.8107890657166,20.0958761808335,
-4.83616999940829));
#109539=CARTESIAN_POINT('Ctrl Pts',(-16.8157341373979,20.1065236182853,
-4.83546476126004));
#109540=CARTESIAN_POINT('Ctrl Pts',(-16.8175059682376,20.1103092327208,
-4.83521299280402));
#109541=CARTESIAN_POINT('Ctrl Pts',(-16.8208093443362,20.117312979696,-4.83474524795382));
#109542=CARTESIAN_POINT('Ctrl Pts',(-16.8223378094702,20.120532501233,-4.83452946253968));
#109543=CARTESIAN_POINT('Ctrl Pts',(-16.8258074053121,20.1277933911589,
-4.83404107224157));
#109544=CARTESIAN_POINT('Ctrl Pts',(-16.827753237573,20.1318324388157,-4.83376817918748));
#109545=CARTESIAN_POINT('Ctrl Pts',(-16.8335217755547,20.1437098000355,
-4.83296218729391));
#109546=CARTESIAN_POINT('Ctrl Pts',(-16.8373800481002,20.1515305974386,
-4.83242695134667));
#109547=CARTESIAN_POINT('Ctrl Pts',(-16.8651905788954,20.2070360913482,
-4.82859720603469));
#109548=CARTESIAN_POINT('Ctrl Pts',(-16.8908879536521,20.2538199726222,
-4.82520557095097));
#109549=CARTESIAN_POINT('Ctrl Pts',(-16.9273703885928,20.3146702716838,
-4.82062016617669));
#109550=CARTESIAN_POINT('Ctrl Pts',(-16.9366060600847,20.329648122504,-4.81947691282786));
#109551=CARTESIAN_POINT('Ctrl Pts',(-16.9719974396182,20.3854737364625,
-4.81516492702491));
#109552=CARTESIAN_POINT('Ctrl Pts',(-16.9993672338391,20.4255330415147,
-4.81196743665102));
#109553=CARTESIAN_POINT('Ctrl Pts',(-17.0928606654789,20.5527582809314,
-4.80153807568917));
#109554=CARTESIAN_POINT('Ctrl Pts',(-17.1643724611866,20.6357548753799,
-4.79430527611817));
#109555=CARTESIAN_POINT('Ctrl Pts',(-17.2810732760338,20.7516911134269,
-4.78373162680585));
#109556=CARTESIAN_POINT('Ctrl Pts',(-17.3216673750704,20.7889868661811,
-4.78024239991532));
#109557=CARTESIAN_POINT('Ctrl Pts',(-17.3898211554562,20.8468633750935,
-4.77468470372269));
#109558=CARTESIAN_POINT('Ctrl Pts',(-17.4165057514967,20.8684302005164,
-4.77257779349461));
#109559=CARTESIAN_POINT('Ctrl Pts',(-17.452272882883,20.8959277198318,-4.76984121630616));
#109560=CARTESIAN_POINT('Ctrl Pts',(-17.4608922236801,20.902449798389,-4.76918820698987));
#109561=CARTESIAN_POINT('Ctrl Pts',(-17.4750937144903,20.9130257186884,
-4.76812270140971));
#109562=CARTESIAN_POINT('Ctrl Pts',(-17.480646319645,20.9171187345743,-4.76770867567016));
#109563=CARTESIAN_POINT('Ctrl Pts',(-17.4914348499393,20.9249902383723,
-4.76690915978977));
#109564=CARTESIAN_POINT('Ctrl Pts',(-17.4966682443373,20.928772050429,-4.76652354329821));
#109565=CARTESIAN_POINT('Ctrl Pts',(-17.5087941194647,20.9374504135402,
-4.76563512590242));
#109566=CARTESIAN_POINT('Ctrl Pts',(-17.5156988242927,20.9423297573094,
-4.76513299104892));
#109567=CARTESIAN_POINT('Ctrl Pts',(-17.5343516773014,20.9553443166718,
-4.76378639286306));
#109568=CARTESIAN_POINT('Ctrl Pts',(-17.5461533971386,20.9634022529772,
-4.76294487085612));
#109569=CARTESIAN_POINT('Ctrl Pts',(-17.6551779317309,21.0362341542191,
-4.75526378553406));
#109570=CARTESIAN_POINT('Ctrl Pts',(-17.7575304245802,21.0929801282206,
-4.74874083189837));
#109571=CARTESIAN_POINT('Ctrl Pts',(-18.0124244107475,21.207873484547,-4.73343466735366));
#109572=CARTESIAN_POINT('Ctrl Pts',(-18.1679920385624,21.2574110480607,
-4.72483454736412));
#109573=CARTESIAN_POINT('Ctrl Pts',(-18.3595787487887,21.2948796631286,
-4.71362552949456));
#109574=CARTESIAN_POINT('Ctrl Pts',(-18.3916191808121,21.3003828842905,
-4.71172955135087));
#109575=CARTESIAN_POINT('Ctrl Pts',(-18.4309329495605,21.3062068570694,
-4.70936322705093));
#109576=CARTESIAN_POINT('Ctrl Pts',(-18.4380996147278,21.3072309914524,
-4.70893024446441));
#109577=CARTESIAN_POINT('Ctrl Pts',(-18.4493425548703,21.3087788321044,
-4.70824826004283));
#109578=CARTESIAN_POINT('Ctrl Pts',(-18.4534154197205,21.3093274725701,
-4.70800064394495));
#109579=CARTESIAN_POINT('Ctrl Pts',(-18.4610311638127,21.310330791771,-4.70753654253321));
#109580=CARTESIAN_POINT('Ctrl Pts',(-18.4645736050249,21.3107883645363,
-4.70732022258151));
#109581=CARTESIAN_POINT('Ctrl Pts',(-18.472662440328,21.3118123834415,-4.70682527057329));
#109582=CARTESIAN_POINT('Ctrl Pts',(-18.4772095099472,21.3123730353803,
-4.70654631663277));
#109583=CARTESIAN_POINT('Ctrl Pts',(-18.4911910424031,21.3140508952117,
-4.70568643692749));
#109584=CARTESIAN_POINT('Ctrl Pts',(-18.5006310832383,21.3151193404124,
-4.70510287186301));
#109585=CARTESIAN_POINT('Ctrl Pts',(-18.585489176585,21.3241457018089,-4.6998321930468));
#109586=CARTESIAN_POINT('Ctrl Pts',(-18.6612692340638,21.3281083857921,
-4.69495035632745));
#109587=CARTESIAN_POINT('Ctrl Pts',(-18.9220127555302,21.3277278977201,
-4.67789742716739));
#109588=CARTESIAN_POINT('Ctrl Pts',(-19.1061435778507,21.3032272344487,
-4.66550056075186));
#109589=CARTESIAN_POINT('Ctrl Pts',(-19.3361783441231,21.2412480017666,
-4.65047356627224));
#109590=CARTESIAN_POINT('Ctrl Pts',(-19.3870671384211,21.2254552162038,
-4.64717203415066));
#109591=CARTESIAN_POINT('Ctrl Pts',(-19.4491381314976,21.2035922108457,
-4.64317041112002));
#109592=CARTESIAN_POINT('Ctrl Pts',(-19.4609293599016,21.1993208951696,
-4.64241136204275));
#109593=CARTESIAN_POINT('Ctrl Pts',(-19.479505556347,21.1924044208384,-4.64121713601289));
#109594=CARTESIAN_POINT('Ctrl Pts',(-19.4863158855397,21.1898286494515,
-4.64077965532218));
#109595=CARTESIAN_POINT('Ctrl Pts',(-19.4990580064809,21.1849340938054,
-4.63996172408139));
#109596=CARTESIAN_POINT('Ctrl Pts',(-19.5049928695549,21.1826235838602,
-4.63958100164126));
#109597=CARTESIAN_POINT('Ctrl Pts',(-19.5182501137179,21.1773933733746,
-4.63873105058719));
#109598=CARTESIAN_POINT('Ctrl Pts',(-19.5255668200928,21.1744594754203,
-4.63826230578819));
#109599=CARTESIAN_POINT('Ctrl Pts',(-19.5440621743795,21.1669229061899,
-4.63707817819079));
#109600=CARTESIAN_POINT('Ctrl Pts',(-19.5552181928735,21.1622651870272,
-4.63636466096839));
#109601=CARTESIAN_POINT('Ctrl Pts',(-19.6186396612221,21.1351459941704,
-4.63231157404071));
#109602=CARTESIAN_POINT('Ctrl Pts',(-19.6700255571715,21.1106794793352,
-4.62904111383941));
#109603=CARTESIAN_POINT('Ctrl Pts',(-19.7441246037395,21.0716606925732,
-4.62431035120919));
#109604=CARTESIAN_POINT('Ctrl Pts',(-19.7676425881203,21.0586993795897,
-4.62280643641715));
#109605=CARTESIAN_POINT('Ctrl Pts',(-19.8912830483217,20.9874585490753,
-4.61486906495003));
#109606=CARTESIAN_POINT('Ctrl Pts',(-19.986740954256,20.9214823632751,-4.60864416855414));
#109607=CARTESIAN_POINT('Ctrl Pts',(-20.1382144281337,20.7972776432238,
-4.59796527147532));
#109608=CARTESIAN_POINT('Ctrl Pts',(-20.197172748877,20.7430634541797,-4.59356345628013));
#109609=CARTESIAN_POINT('Ctrl Pts',(-20.2779936572084,20.6598163158203,
-4.58692644359765));
#109610=CARTESIAN_POINT('Ctrl Pts',(-20.3024069196683,20.6333517557169,
-4.58483230703258));
#109611=CARTESIAN_POINT('Ctrl Pts',(-20.3310516797729,20.6006656617167,
-4.58224585839903));
#109612=CARTESIAN_POINT('Ctrl Pts',(-20.3359416188343,20.5950259265279,
-4.58179958556928));
#109613=CARTESIAN_POINT('Ctrl Pts',(-20.3435094032093,20.5862039040975,
-4.58110128113724));
#109614=CARTESIAN_POINT('Ctrl Pts',(-20.3462079251059,20.5830393224708,
-4.58085074662194));
#109615=CARTESIAN_POINT('Ctrl Pts',(-20.3512028426161,20.5771466545727,
-4.58038410999141));
#109616=CARTESIAN_POINT('Ctrl Pts',(-20.3535016768327,20.574420710601,-4.58016819132513));
#109617=CARTESIAN_POINT('Ctrl Pts',(-20.3586930668443,20.5682331370054,
-4.57967796734314));
#109618=CARTESIAN_POINT('Ctrl Pts',(-20.3615814373997,20.5647680796201,
-4.57940336432214));
#109619=CARTESIAN_POINT('Ctrl Pts',(-20.3701034393598,20.5544778957299,
-4.57858771918393));
#109620=CARTESIAN_POINT('Ctrl Pts',(-20.3757052908646,20.5476267438118,
-4.57804446437036));
#109621=CARTESIAN_POINT('Ctrl Pts',(-20.416896854037,20.4965992241032,-4.57399809228173));
#109622=CARTESIAN_POINT('Ctrl Pts',(-20.4507378826997,20.4510471804908,
-4.57038527969595));
#109623=CARTESIAN_POINT('Ctrl Pts',(-20.517595504503,20.3530630292599,-4.56270258985737));
#109624=CARTESIAN_POINT('Ctrl Pts',(-20.5502243660562,20.3004261541394,
-4.55862492025321));
#109625=CARTESIAN_POINT('Ctrl Pts',(-20.6341053630717,20.1508409512255,
-4.5472967590275));
#109626=CARTESIAN_POINT('Ctrl Pts',(-20.6802112915795,20.0512181100901,
-4.54004817867238));
#109627=CARTESIAN_POINT('Ctrl Pts',(-20.7376833194159,19.8965708333749,
-4.52944135634561));
#109628=CARTESIAN_POINT('Ctrl Pts',(-20.7549277192372,19.8439345920452,
-4.52593485085462));
#109629=CARTESIAN_POINT('Ctrl Pts',(-20.7795153163776,19.7575720471792,
-4.52035286679903));
#109630=CARTESIAN_POINT('Ctrl Pts',(-20.7881324556578,19.7242387217262,
-4.5182385271321));
#109631=CARTESIAN_POINT('Ctrl Pts',(-20.7983855413429,19.680167832704,-4.51549385997609));
#109632=CARTESIAN_POINT('Ctrl Pts',(-20.8007569904306,19.6696084036162,
-4.51484001718692));
#109633=CARTESIAN_POINT('Ctrl Pts',(-20.8045078944324,19.6522863958362,
-4.51377350019948));
#109634=CARTESIAN_POINT('Ctrl Pts',(-20.8059354156874,19.6455345314609,
-4.51335929091796));
#109635=CARTESIAN_POINT('Ctrl Pts',(-20.8086343583903,19.6324533815842,
-4.512559661088));
#109636=CARTESIAN_POINT('Ctrl Pts',(-20.8099098928683,19.6261250317416,
-4.51217411292849));
#109637=CARTESIAN_POINT('Ctrl Pts',(-20.812787627958,19.6115026265349,-4.51128619626175));
#109638=CARTESIAN_POINT('Ctrl Pts',(-20.8143691798414,19.6032045827547,
-4.510784491395));
#109639=CARTESIAN_POINT('Ctrl Pts',(-20.818487729919,19.5808694012497,-4.50943980732034));
#109640=CARTESIAN_POINT('Ctrl Pts',(-20.8209326214634,19.5668155680512,
-4.50859975621447));
#109641=CARTESIAN_POINT('Ctrl Pts',(-20.8418093123264,19.4391846314612,
-4.50102309292269));
#109642=CARTESIAN_POINT('Ctrl Pts',(-20.8510962907031,19.3242992172063,
-4.49459289099642));
#109643=CARTESIAN_POINT('Ctrl Pts',(-20.8508421937423,19.0229639402604,
-4.47808646799875));
#109644=CARTESIAN_POINT('Ctrl Pts',(-20.8261075478324,18.8375810118745,
-4.46831888325726));
#109645=CARTESIAN_POINT('Ctrl Pts',(-20.7737437540966,18.6441344243448,
-4.45654192610075));
#109646=CARTESIAN_POINT('Ctrl Pts',(-20.7698906310994,18.6304481272354,
-4.45569953652088));
#109647=CARTESIAN_POINT('Ctrl Pts',(-20.7643392702254,18.6114648718975,
-4.45451699730324));
#109648=CARTESIAN_POINT('Ctrl Pts',(-20.7627574776398,18.6061338847515,
-4.45418335222364));
#109649=CARTESIAN_POINT('Ctrl Pts',(-20.7601843571559,18.5975855522441,
-4.45364575121933));
#109650=CARTESIAN_POINT('Ctrl Pts',(-20.7592063131376,18.5943641895252,
-4.45344256784534));
#109651=CARTESIAN_POINT('Ctrl Pts',(-20.7571469223496,18.5876389673479,
-4.4530171162032));
#109652=CARTESIAN_POINT('Ctrl Pts',(-20.7560641552701,18.5841355826974,
-4.45279476244682));
#109653=CARTESIAN_POINT('Ctrl Pts',(-20.7534222720431,18.5756656114123,
-4.45225546737612));
#109654=CARTESIAN_POINT('Ctrl Pts',(-20.7518539336428,18.5707019449483,
-4.45193798991217));
#109655=CARTESIAN_POINT('Ctrl Pts',(-20.7463005682226,18.5533490303559,
-4.45082319401964));
#109656=CARTESIAN_POINT('Ctrl Pts',(-20.7422197096073,18.5409910796789,
-4.45002052948399));
#109657=CARTESIAN_POINT('Ctrl Pts',(-20.7330366708962,18.5140201227554,
-4.44825071070825));
#109658=CARTESIAN_POINT('Ctrl Pts',(-20.7278880991585,18.4994251989497,
-4.44728132108652));
#109659=CARTESIAN_POINT('Ctrl Pts',(-20.722580615654,18.4848897225317,-4.44630506752222));
#109660=CARTESIAN_POINT('Origin',(-18.734,19.211,0.));
#109661=CARTESIAN_POINT('',(-20.7225806137986,18.4848897174502,-3.64442447432525));
#109662=CARTESIAN_POINT('',(-20.7225805460717,18.4848895319684,-3.86819362763421));
#109663=CARTESIAN_POINT('',(-20.7225806137986,18.4848897174502,0.));
#109664=CARTESIAN_POINT('',(-20.8509990913949,19.212945854356,-3.91098517251486));
#109665=CARTESIAN_POINT('Ctrl Pts',(-20.7225805460717,18.4848895319684,
-3.86819362763421));
#109666=CARTESIAN_POINT('Ctrl Pts',(-20.7339918661314,18.5161414283049,
-3.87027305953112));
#109667=CARTESIAN_POINT('Ctrl Pts',(-20.7446701890291,18.5476725148875,
-3.87233005867685));
#109668=CARTESIAN_POINT('Ctrl Pts',(-20.7593062383098,18.5945001734164,
-3.87532606019889));
#109669=CARTESIAN_POINT('Ctrl Pts',(-20.7638398855016,18.6095954311567,
-3.87628298084949));
#109670=CARTESIAN_POINT('Ctrl Pts',(-20.7704399629066,18.6324963854922,
-3.87772165193606));
#109671=CARTESIAN_POINT('Ctrl Pts',(-20.7726309379284,18.6402653363781,
-3.87820745032604));
#109672=CARTESIAN_POINT('Ctrl Pts',(-20.7764755276552,18.6542024643816,
-3.87907496958561));
#109673=CARTESIAN_POINT('Ctrl Pts',(-20.7781457595611,18.6603659184232,
-3.87945722668699));
#109674=CARTESIAN_POINT('Ctrl Pts',(-20.7816286851116,18.6734528061553,
-3.88026597292423));
#109675=CARTESIAN_POINT('Ctrl Pts',(-20.78343421329,18.6803780771307,-3.88069222567083));
#109676=CARTESIAN_POINT('Ctrl Pts',(-20.7870375877586,18.6944919473566,
-3.88155750779302));
#109677=CARTESIAN_POINT('Ctrl Pts',(-20.7888328801823,18.7016811000631,
-3.88199644993303));
#109678=CARTESIAN_POINT('Ctrl Pts',(-20.7932123060644,18.7196184020906,
-3.88308722853753));
#109679=CARTESIAN_POINT('Ctrl Pts',(-20.7957500889239,18.7303777222018,
-3.88373758024108));
#109680=CARTESIAN_POINT('Ctrl Pts',(-20.8334344277575,18.8959395700739,
-3.89368678770169));
#109681=CARTESIAN_POINT('Ctrl Pts',(-20.8511450350875,19.0541908602725,
-3.90236293223036));
#109682=CARTESIAN_POINT('Ctrl Pts',(-20.8509991056219,19.2129459691744,
-3.9109852020952));
#109683=CARTESIAN_POINT('Ctrl Pts',(-20.8509991057286,19.2129458531049,
-3.91098519579126));
#109684=CARTESIAN_POINT('Ctrl Pts',(-20.850867753823,19.355850713657,-3.91874661073577));
#109685=CARTESIAN_POINT('Ctrl Pts',(-20.8362669050489,19.4983604443446,
-3.92644252221242));
#109686=CARTESIAN_POINT('Ctrl Pts',(-20.8054595308778,19.6478519609443,
-3.93541366789966));
#109687=CARTESIAN_POINT('Ctrl Pts',(-20.8034239064502,19.6573954653553,
-3.93599045272699));
#109688=CARTESIAN_POINT('Ctrl Pts',(-20.8001171080786,19.6723896595962,
-3.93690356019448));
#109689=CARTESIAN_POINT('Ctrl Pts',(-20.7988901457165,19.6778500903219,
-3.93723753031756));
#109690=CARTESIAN_POINT('Ctrl Pts',(-20.796524907932,19.688184508945,-3.9378724508969));
#109691=CARTESIAN_POINT('Ctrl Pts',(-20.7953909685151,19.6930594622758,
-3.93817315943133));
#109692=CARTESIAN_POINT('Ctrl Pts',(-20.7934047157095,19.7014634516889,
-3.9386937048062));
#109693=CARTESIAN_POINT('Ctrl Pts',(-20.7925605836276,19.7049944371324,
-3.93891307202772));
#109694=CARTESIAN_POINT('Ctrl Pts',(-20.7909043902426,19.7118442907665,
-3.93933993107386));
#109695=CARTESIAN_POINT('Ctrl Pts',(-20.790093375697,19.7151633705692,-3.9395473563947));
#109696=CARTESIAN_POINT('Ctrl Pts',(-20.7878794157588,19.7241298146693,
-3.94010928592489));
#109697=CARTESIAN_POINT('Ctrl Pts',(-20.7864612271095,19.7297733325405,
-3.94046465583406));
#109698=CARTESIAN_POINT('Ctrl Pts',(-20.7810862687942,19.7507952962876,
-3.94179451832977));
#109699=CARTESIAN_POINT('Ctrl Pts',(-20.7769798907992,19.7661344748211,
-3.94277711452664));
#109700=CARTESIAN_POINT('Ctrl Pts',(-20.7391454582484,19.9013547930535,
-3.9515386807508));
#109701=CARTESIAN_POINT('Ctrl Pts',(-20.6950755517545,20.0180780298046,
-3.95978243884308));
#109702=CARTESIAN_POINT('Ctrl Pts',(-20.610136300618,20.1942889213471,-3.9727087389708));
#109703=CARTESIAN_POINT('Ctrl Pts',(-20.576054047705,20.256744816396,-3.97739737811818));
#109704=CARTESIAN_POINT('Ctrl Pts',(-20.4899911222872,20.3971448593993,
-3.98809703190452));
#109705=CARTESIAN_POINT('Ctrl Pts',(-20.4358500575675,20.4735984462119,
-3.99404315000294));
#109706=CARTESIAN_POINT('Ctrl Pts',(-20.3628825375995,20.5633753163385,
-4.00115615185354));
#109707=CARTESIAN_POINT('Ctrl Pts',(-20.3486769825774,20.580304793528,-4.00250405331161));
#109708=CARTESIAN_POINT('Ctrl Pts',(-20.3295476156363,20.6023904871968,
-4.00427189747669));
#109709=CARTESIAN_POINT('Ctrl Pts',(-20.3248595492177,20.6077482157587,
-4.00470150638706));
#109710=CARTESIAN_POINT('Ctrl Pts',(-20.3155382914039,20.6182931476713,
-4.00554858295229));
#109711=CARTESIAN_POINT('Ctrl Pts',(-20.3109063895642,20.6234813666053,
-4.00596609667235));
#109712=CARTESIAN_POINT('Ctrl Pts',(-20.3019392991922,20.63342636798,-4.00676788458745));
#109713=CARTESIAN_POINT('Ctrl Pts',(-20.2976078285496,20.6381863852303,
-4.00715230863392));
#109714=CARTESIAN_POINT('Ctrl Pts',(-20.287625817159,20.649056005087,-4.00803171756957));
#109715=CARTESIAN_POINT('Ctrl Pts',(-20.2819607997217,20.6551522146411,
-4.00852607981863));
#109716=CARTESIAN_POINT('Ctrl Pts',(-20.2667829295621,20.6712934226505,
-4.00983822117618));
#109717=CARTESIAN_POINT('Ctrl Pts',(-20.257207211776,20.6812789507222,-4.01065329248753));
#109718=CARTESIAN_POINT('Ctrl Pts',(-20.1814300812609,20.7587641498101,
-4.01700635350522));
#109719=CARTESIAN_POINT('Ctrl Pts',(-20.1108679839604,20.8218586141094,
-4.02234301004089));
#109720=CARTESIAN_POINT('Ctrl Pts',(-19.95614958634,20.9425827669569,-4.03318418439675));
#109721=CARTESIAN_POINT('Ctrl Pts',(-19.8715808680843,20.9992781203805,
-4.03865651750859));
#109722=CARTESIAN_POINT('Ctrl Pts',(-19.7137013728215,21.0893740505019,
-4.0485661575746));
#109723=CARTESIAN_POINT('Ctrl Pts',(-19.6419468757021,21.1250883784408,
-4.05297087424225));
#109724=CARTESIAN_POINT('Ctrl Pts',(-19.5352918338546,21.1708250111655,
-4.05960902222522));
#109725=CARTESIAN_POINT('Ctrl Pts',(-19.5018816381541,21.1841548647885,
-4.0617011052978));
#109726=CARTESIAN_POINT('Ctrl Pts',(-19.4611837250776,21.1992022030791,
-4.06428317001842));
#109727=CARTESIAN_POINT('Ctrl Pts',(-19.4542035952326,21.2017413061604,
-4.06472720069057));
#109728=CARTESIAN_POINT('Ctrl Pts',(-19.4432708698648,21.2056531878449,
-4.06542472214234));
#109729=CARTESIAN_POINT('Ctrl Pts',(-19.4393272427994,21.2070510981656,
-4.06567674625059));
#109730=CARTESIAN_POINT('Ctrl Pts',(-19.4320171661059,21.2096179563189,
-4.0661447231962));
#109731=CARTESIAN_POINT('Ctrl Pts',(-19.4286518992927,21.2107900984174,
-4.06636048350092));
#109732=CARTESIAN_POINT('Ctrl Pts',(-19.4210513783714,21.2134159043103,
-4.06684850522044));
#109733=CARTESIAN_POINT('Ctrl Pts',(-19.4168144870604,21.2148646226142,
-4.06712105287655));
#109734=CARTESIAN_POINT('Ctrl Pts',(-19.4043369949964,21.2190868789935,
-4.06792510144432));
#109735=CARTESIAN_POINT('Ctrl Pts',(-19.3960839826243,21.221823063935,-4.06845872440251));
#109736=CARTESIAN_POINT('Ctrl Pts',(-19.3375454000889,21.2408313666465,
-4.07225524890462));
#109737=CARTESIAN_POINT('Ctrl Pts',(-19.2866869885862,21.2552647843692,
-4.07561344863672));
#109738=CARTESIAN_POINT('Ctrl Pts',(-19.2204507581921,21.2714100897796,
-4.08001813576164));
#109739=CARTESIAN_POINT('Ctrl Pts',(-19.2055158934127,21.2748790720485,
-4.08101333744537));
#109740=CARTESIAN_POINT('Ctrl Pts',(-19.0333978799346,21.3128919203837,
-4.09249706823895));
#109741=CARTESIAN_POINT('Ctrl Pts',(-18.8727842150772,21.3295693034362,
-4.10329751587653));
#109742=CARTESIAN_POINT('Ctrl Pts',(-18.6568162402587,21.3273078474708,
-4.11717923825511));
#109743=CARTESIAN_POINT('Ctrl Pts',(-18.6018389500776,21.3245871197092,
-4.12066313369305));
#109744=CARTESIAN_POINT('Ctrl Pts',(-18.5130216741427,21.3167119886622,
-4.12620530749371));
#109745=CARTESIAN_POINT('Ctrl Pts',(-18.4790935954973,21.312874719827,-4.12830208991675));
#109746=CARTESIAN_POINT('Ctrl Pts',(-18.4348180102212,21.306779207003,-4.13101329655986));
#109747=CARTESIAN_POINT('Ctrl Pts',(-18.4243752397669,21.3052618894685,
-4.13165093414245));
#109748=CARTESIAN_POINT('Ctrl Pts',(-18.4070455278146,21.3026114545042,
-4.13270616650376));
#109749=CARTESIAN_POINT('Ctrl Pts',(-18.4001521513913,21.3015222599364,
-4.13312514446392));
#109750=CARTESIAN_POINT('Ctrl Pts',(-18.3869200970723,21.2993643981073,
-4.13392794825625));
#109751=CARTESIAN_POINT('Ctrl Pts',(-18.3805806637557,21.2983009108593,
-4.13431193354371));
#109752=CARTESIAN_POINT('Ctrl Pts',(-18.366096296104,21.2958031704144,-4.13518785563192));
#109753=CARTESIAN_POINT('Ctrl Pts',(-18.3579546928115,21.2943500245073,
-4.13567918663906));
#109754=CARTESIAN_POINT('Ctrl Pts',(-18.3363902971673,21.2903705948904,
-4.13697797063632));
#109755=CARTESIAN_POINT('Ctrl Pts',(-18.3229829435348,21.2877620323529,
-4.13778280380238));
#109756=CARTESIAN_POINT('Ctrl Pts',(-18.2236278534332,21.2674314331196,
-4.14372894601878));
#109757=CARTESIAN_POINT('Ctrl Pts',(-18.1388255651056,21.2445092882201,
-4.14869838640902));
#109758=CARTESIAN_POINT('Ctrl Pts',(-17.8817834971522,21.157565404442,-4.16373887211798));
#109759=CARTESIAN_POINT('Ctrl Pts',(-17.7162961194409,21.0763834248619,
-4.17333900079684));
#109760=CARTESIAN_POINT('Ctrl Pts',(-17.5291761549508,20.9521986035126,
-4.18611989109039));
#109761=CARTESIAN_POINT('Ctrl Pts',(-17.4956531643278,20.928518468108,-4.18849791955397));
#109762=CARTESIAN_POINT('Ctrl Pts',(-17.4566477509203,20.8992299114168,
-4.19139895718403));
#109763=CARTESIAN_POINT('Ctrl Pts',(-17.450479185991,20.8945448665962,-4.19186185463731));
#109764=CARTESIAN_POINT('Ctrl Pts',(-17.4409900393778,20.8872553653996,
-4.19258054501992));
#109765=CARTESIAN_POINT('Ctrl Pts',(-17.4376512266735,20.8846745996403,
-4.19283469628949));
#109766=CARTESIAN_POINT('Ctrl Pts',(-17.4315091613293,20.8798976292132,
-4.19330463565417));
#109767=CARTESIAN_POINT('Ctrl Pts',(-17.4287037245924,20.8777043272517,
-4.19352021839222));
#109768=CARTESIAN_POINT('Ctrl Pts',(-17.4224183459432,20.872764789715,-4.19400531532362));
#109769=CARTESIAN_POINT('Ctrl Pts',(-17.4189415126374,20.8700147153002,
-4.1942751002937));
#109770=CARTESIAN_POINT('Ctrl Pts',(-17.4100884139221,20.8629668543128,
-4.1949657047671));
#109771=CARTESIAN_POINT('Ctrl Pts',(-17.4047244717151,20.8586537689771,
-4.19538758426108));
#109772=CARTESIAN_POINT('Ctrl Pts',(-17.3738967156335,20.8336170022429,
-4.19783174972346));
#109773=CARTESIAN_POINT('Ctrl Pts',(-17.3488981942359,20.812330569676,-4.19989102638432));
#109774=CARTESIAN_POINT('Ctrl Pts',(-17.3101941905744,20.7777893528849,
-4.20319014382381));
#109775=CARTESIAN_POINT('Ctrl Pts',(-17.2961542531789,20.764914871017,-4.20441101973025));
#109776=CARTESIAN_POINT('Ctrl Pts',(-17.2642475181225,20.734854045894,-4.20723807508665));
#109777=CARTESIAN_POINT('Ctrl Pts',(-17.2465051133088,20.7175398786752,
-4.2088492569036));
#109778=CARTESIAN_POINT('Ctrl Pts',(-17.2259375552873,20.6967511623634,
-4.21076009609222));
#109779=CARTESIAN_POINT('Ctrl Pts',(-17.2228137848039,20.6935738013047,
-4.21105151378628));
#109780=CARTESIAN_POINT('Ctrl Pts',(-17.1169471842426,20.5852087646541,
-4.22096824518655));
#109781=CARTESIAN_POINT('Ctrl Pts',(-17.0254207144633,20.4695995216088,
-4.23080151624972));
#109782=CARTESIAN_POINT('Ctrl Pts',(-16.9048380449123,20.2796129005143,
-4.24528565078378));
#109783=CARTESIAN_POINT('Ctrl Pts',(-16.8667251726405,20.2115269131023,
-4.25019769506056));
#109784=CARTESIAN_POINT('Ctrl Pts',(-16.8240129462674,20.124239891412,-4.25615329087348));
#109785=CARTESIAN_POINT('Ctrl Pts',(-16.8158087092046,20.1068793751025,
-4.2573218374985));
#109786=CARTESIAN_POINT('Ctrl Pts',(-16.8042623546933,20.0815607554497,
-4.25900352774926));
#109787=CARTESIAN_POINT('Ctrl Pts',(-16.8007311027176,20.073690432823,-4.25952316859085));
#109788=CARTESIAN_POINT('Ctrl Pts',(-16.7946394142881,20.0598882472299,
-4.26042909863537));
#109789=CARTESIAN_POINT('Ctrl Pts',(-16.7920578627787,20.0539658799842,
-4.26081610780249));
#109790=CARTESIAN_POINT('Ctrl Pts',(-16.7871085860755,20.0424682854453,
-4.26156416036925));
#109791=CARTESIAN_POINT('Ctrl Pts',(-16.7847376009153,20.0368945380628,
-4.26192531206315));
#109792=CARTESIAN_POINT('Ctrl Pts',(-16.7791437389479,20.0235861238449,
-4.26278413862725));
#109793=CARTESIAN_POINT('Ctrl Pts',(-16.7759427818912,20.0158423098474,
-4.26328106659437));
#109794=CARTESIAN_POINT('Ctrl Pts',(-16.7646521127736,19.988061650068,-4.26505395761008));
#109795=CARTESIAN_POINT('Ctrl Pts',(-16.7568231245874,19.9679197863902,
-4.2663211393306));
#109796=CARTESIAN_POINT('Ctrl Pts',(-16.6831083100044,19.7693189137754,
-4.2786480987041));
#109797=CARTESIAN_POINT('Ctrl Pts',(-16.6412528391418,19.582875784331,-4.28879940722632));
#109798=CARTESIAN_POINT('Ctrl Pts',(-16.6232250431409,19.374344729596,-4.30022170439996));
#109799=CARTESIAN_POINT('Ctrl Pts',(-16.6218397323961,19.3553308972484,
-4.30126479176621));
#109800=CARTESIAN_POINT('Ctrl Pts',(-16.6169932428338,19.2735915825331,
-4.30576463364844));
#109801=CARTESIAN_POINT('Ctrl Pts',(-16.6160684380832,19.2107519804423,
-4.30926310047622));
#109802=CARTESIAN_POINT('Ctrl Pts',(-16.6188603926347,19.1170207153443,
-4.31465668960879));
#109803=CARTESIAN_POINT('Ctrl Pts',(-16.6204610476827,19.0860979029405,
-4.31646475486993));
#109804=CARTESIAN_POINT('Ctrl Pts',(-16.6232638245978,19.0481115448497,
-4.31873320122534));
#109805=CARTESIAN_POINT('Ctrl Pts',(-16.6238244702782,19.0410027016634,
-4.31915976938654));
#109806=CARTESIAN_POINT('Ctrl Pts',(-16.6247628177317,19.0298254916432,
-4.3198338709681));
#109807=CARTESIAN_POINT('Ctrl Pts',(-16.6251164062439,19.0257550786701,
-4.32008007105755));
#109808=CARTESIAN_POINT('Ctrl Pts',(-16.6258015267469,19.0181244375402,
-4.32054299049901));
#109809=CARTESIAN_POINT('Ctrl Pts',(-16.6261302959739,19.0145640170673,
-4.32075955342447));
#109810=CARTESIAN_POINT('Ctrl Pts',(-16.6269044006765,19.0064065832896,
-4.32125701920273));
#109811=CARTESIAN_POINT('Ctrl Pts',(-16.627355759526,19.0018101962475,-4.32153825659306));
#109812=CARTESIAN_POINT('Ctrl Pts',(-16.6288006813727,18.9875750174225,
-4.32241208012259));
#109813=CARTESIAN_POINT('Ctrl Pts',(-16.6298453679556,18.9779417020514,
-4.3230074286903));
#109814=CARTESIAN_POINT('Ctrl Pts',(-16.6419739042845,18.8728385405845,
-4.32954421755733));
#109815=CARTESIAN_POINT('Ctrl Pts',(-16.6594796819683,18.7782328137331,
-4.33579614055746));
#109816=CARTESIAN_POINT('Ctrl Pts',(-16.7131899272828,18.5687771107065,
-4.35003100339635));
#109817=CARTESIAN_POINT('Ctrl Pts',(-16.7528880351878,18.4551412718751,
-4.35802202617072));
#109818=CARTESIAN_POINT('Ctrl Pts',(-16.8275413648485,18.2885016939195,
-4.36982475130907));
#109819=CARTESIAN_POINT('Ctrl Pts',(-16.8555791961253,18.2326728059808,
-4.37379798928017));
#109820=CARTESIAN_POINT('Ctrl Pts',(-16.9043557041124,18.1454019907518,
-4.38002898448372));
#109821=CARTESIAN_POINT('Ctrl Pts',(-16.9235335981507,18.1131343172881,
-4.3823378146174));
#109822=CARTESIAN_POINT('Ctrl Pts',(-16.9495169516862,18.0719504519015,
-4.38529310840281));
#109823=CARTESIAN_POINT('Ctrl Pts',(-16.9555483241883,18.0625561541704,
-4.38596783290082));
#109824=CARTESIAN_POINT('Ctrl Pts',(-16.965469136165,18.0473693662882,-4.38705970168538));
#109825=CARTESIAN_POINT('Ctrl Pts',(-16.9693133374077,18.0415477125032,
-4.38747852396685));
#109826=CARTESIAN_POINT('Ctrl Pts',(-16.9767551984081,18.0303980197172,
-4.38828121813574));
#109827=CARTESIAN_POINT('Ctrl Pts',(-16.9803484827893,18.025067166252,-4.38866524846408));
#109828=CARTESIAN_POINT('Ctrl Pts',(-16.9886226992773,18.0129117051789,
-4.38954153362237));
#109829=CARTESIAN_POINT('Ctrl Pts',(-16.993319495717,18.006097983634,-4.39003318090292));
#109830=CARTESIAN_POINT('Ctrl Pts',(-17.0058841011221,17.9880971060124,
-4.39133335651856));
#109831=CARTESIAN_POINT('Ctrl Pts',(-17.0138206512216,17.9769582384652,
-4.39213925593046));
#109832=CARTESIAN_POINT('Ctrl Pts',(-17.0738934335507,17.8943524473931,
-4.39812779157076));
#109833=CARTESIAN_POINT('Ctrl Pts',(-17.1303586670236,17.8261347407728,
-4.40313560774494));
#109834=CARTESIAN_POINT('Ctrl Pts',(-17.2869184064686,17.6594523244136,
-4.41580640508079));
#109835=CARTESIAN_POINT('Ctrl Pts',(-17.3928134520657,17.5670528452157,
-4.42326352914345));
#109836=CARTESIAN_POINT('Ctrl Pts',(-17.5528127412453,17.453263537347,-4.43410166282991));
#109837=CARTESIAN_POINT('Ctrl Pts',(-17.599836630912,17.4225611885036,-4.43724511438607));
#109838=CARTESIAN_POINT('Ctrl Pts',(-17.6727199838165,17.379006112474,-4.44214098553462));
#109839=CARTESIAN_POINT('Ctrl Pts',(-17.6977155844563,17.3647521017972,
-4.44382414222081));
#109840=CARTESIAN_POINT('Ctrl Pts',(-17.7291130519032,17.3476858151744,
-4.44595321629649));
#109841=CARTESIAN_POINT('Ctrl Pts',(-17.7352499320191,17.3443892134516,
-4.44637005293538));
#109842=CARTESIAN_POINT('Ctrl Pts',(-17.7449795400622,17.3392243918855,
-4.4470321890741));
#109843=CARTESIAN_POINT('Ctrl Pts',(-17.7485616122287,17.3373360545226,
-4.44727623309904));
#109844=CARTESIAN_POINT('Ctrl Pts',(-17.7553228323461,17.3337965387391,
-4.44773742111767));
#109845=CARTESIAN_POINT('Ctrl Pts',(-17.7585007614253,17.3321431485381,
-4.44795442252671));
#109846=CARTESIAN_POINT('Ctrl Pts',(-17.765769891302,17.3283846313849,-4.44845130456129));
#109847=CARTESIAN_POINT('Ctrl Pts',(-17.7698637629372,17.3262847735014,
-4.44873151177234));
#109848=CARTESIAN_POINT('Ctrl Pts',(-17.7807378852902,17.3207518420043,
-4.44947671133752));
#109849=CARTESIAN_POINT('Ctrl Pts',(-17.7875297616807,17.3173419415997,
-4.44994309542689));
#109850=CARTESIAN_POINT('Ctrl Pts',(-17.8348595061783,17.293898005068,-4.45319887261588));
#109851=CARTESIAN_POINT('Ctrl Pts',(-17.8760087626475,17.2751322208204,
-4.45605849265602));
#109852=CARTESIAN_POINT('Ctrl Pts',(-17.9232435710595,17.2553929832994,
-4.45934827655616));
#109853=CARTESIAN_POINT('Ctrl Pts',(-17.9287732160307,17.2531096516789,
-4.45973351625342));
#109854=CARTESIAN_POINT('Ctrl Pts',(-18.080150210469,17.191351984878,-4.47028145726577));
#109855=CARTESIAN_POINT('Ctrl Pts',(-18.2321727060649,17.1483146819254,
-4.48087272568225));
#109856=CARTESIAN_POINT('Ctrl Pts',(-18.48917793289,17.1056829974042,-4.49778528429286));
#109857=CARTESIAN_POINT('Ctrl Pts',(-18.5918928706555,17.0962639513629,
-4.50430458954931));
#109858=CARTESIAN_POINT('Ctrl Pts',(-18.7097045144223,17.0940876277254,
-4.51149028355642));
#109859=CARTESIAN_POINT('Ctrl Pts',(-18.7245122508698,17.093969470554,-4.5123884112522));
#109860=CARTESIAN_POINT('Ctrl Pts',(-18.7470889492496,17.0940262090546,
-4.51375030993496));
#109861=CARTESIAN_POINT('Ctrl Pts',(-18.7548575018227,17.0940884951729,
-4.51421759231199));
#109862=CARTESIAN_POINT('Ctrl Pts',(-18.7689864260217,17.0942795609051,
-4.51506506775789));
#109863=CARTESIAN_POINT('Ctrl Pts',(-18.7753468677778,17.0943942489966,
-4.51544569748398));
#109864=CARTESIAN_POINT('Ctrl Pts',(-18.7890725173878,17.0947036360848,
-4.51626522605051));
#109865=CARTESIAN_POINT('Ctrl Pts',(-18.7964374378144,17.0949081185932,
-4.51670381355174));
#109866=CARTESIAN_POINT('Ctrl Pts',(-18.8163930954638,17.0955664496639,
-4.51788914297227));
#109867=CARTESIAN_POINT('Ctrl Pts',(-18.8289812177151,17.0960942558418,
-4.51863356399546));
#109868=CARTESIAN_POINT('Ctrl Pts',(-18.8900494265401,17.0992011247927,
-4.52222983657622));
#109869=CARTESIAN_POINT('Ctrl Pts',(-18.9384379720135,17.1033350455996,
-4.52503271372375));
#109870=CARTESIAN_POINT('Ctrl Pts',(-19.0271583474604,17.1139992203487,
-4.530111560573));
#109871=CARTESIAN_POINT('Ctrl Pts',(-19.0675242673698,17.1200394801967,
-4.53239924350846));
#109872=CARTESIAN_POINT('Ctrl Pts',(-19.2400317911566,17.1509762307576,
-4.5421260116405));
#109873=CARTESIAN_POINT('Ctrl Pts',(-19.3698055324556,17.1872616942401,
-4.54929584435369));
#109874=CARTESIAN_POINT('Ctrl Pts',(-19.5537915259837,17.2581647536107,
-4.56013215296928));
#109875=CARTESIAN_POINT('Ctrl Pts',(-19.6112868762622,17.2833096118014,
-4.5636256974789));
#109876=CARTESIAN_POINT('Ctrl Pts',(-19.6953392136571,17.324608536178,-4.56901242347579));
#109877=CARTESIAN_POINT('Ctrl Pts',(-19.7227978279106,17.3388556501038,
-4.57081880811596));
#109878=CARTESIAN_POINT('Ctrl Pts',(-19.7561871366722,17.357119400233,-4.5730853817558));
#109879=CARTESIAN_POINT('Ctrl Pts',(-19.7624240533147,17.360571999822,-4.57351182392422));
#109880=CARTESIAN_POINT('Ctrl Pts',(-19.7722074706896,17.3660525922125,
-4.57418577063532));
#109881=CARTESIAN_POINT('Ctrl Pts',(-19.7757658083966,17.3680594991958,
-4.57443194286774));
#109882=CARTESIAN_POINT('Ctrl Pts',(-19.7824276935411,17.3718422696254,
-4.5748948393983));
#109883=CARTESIAN_POINT('Ctrl Pts',(-19.7855325583813,17.3736157005773,
-4.57511140744684));
#109884=CARTESIAN_POINT('Ctrl Pts',(-19.7926381775716,17.3776981844922,
-4.5756089242432));
#109885=CARTESIAN_POINT('Ctrl Pts',(-19.7966358658039,17.3800124649442,
-4.57589020778408));
#109886=CARTESIAN_POINT('Ctrl Pts',(-19.8089993382034,17.3872238647522,
-4.57676431446321));
#109887=CARTESIAN_POINT('Ctrl Pts',(-19.8173389461491,17.3921652938784,
-4.57735990255948));
#109888=CARTESIAN_POINT('Ctrl Pts',(-19.907813927974,17.4466170017964,-4.58388414933513));
#109889=CARTESIAN_POINT('Ctrl Pts',(-19.9865190427039,17.5015912719082,
-4.59012195312501));
#109890=CARTESIAN_POINT('Ctrl Pts',(-20.1599368045378,17.6411434207766,
-4.60477496383618));
#109891=CARTESIAN_POINT('Ctrl Pts',(-20.2513330239269,17.7292947692964,
-4.61320501593265));
#109892=CARTESIAN_POINT('Ctrl Pts',(-20.3724508404403,17.8691489566997,
-4.62512679296181));
#109893=CARTESIAN_POINT('Ctrl Pts',(-20.4087701638008,17.9147626614726,
-4.62882514460463));
#109894=CARTESIAN_POINT('Ctrl Pts',(-20.4642424294529,17.9906614172447,
-4.6346755254161));
#109895=CARTESIAN_POINT('Ctrl Pts',(-20.4845889790407,18.0200324975842,
-4.63687123419375));
#109896=CARTESIAN_POINT('Ctrl Pts',(-20.5101992606089,18.0590774792216,
-4.63970428781388));
#109897=CARTESIAN_POINT('Ctrl Pts',(-20.5161437649286,18.0682957882801,
-4.64036708227154));
#109898=CARTESIAN_POINT('Ctrl Pts',(-20.5257284806865,18.0834158031858,
-4.6414444646975));
#109899=CARTESIAN_POINT('Ctrl Pts',(-20.5294117603708,18.089289840507,-4.64186064843995));
#109900=CARTESIAN_POINT('Ctrl Pts',(-20.5364622461458,18.1006575451075,
-4.64266154433391));
#109901=CARTESIAN_POINT('Ctrl Pts',(-20.5398333538535,18.1061486907982,
-4.64304639748499));
#109902=CARTESIAN_POINT('Ctrl Pts',(-20.5475262914819,18.1188088715705,
-4.64392911922893));
#109903=CARTESIAN_POINT('Ctrl Pts',(-20.5518307935931,18.1259883503612,
-4.64442634920298));
#109904=CARTESIAN_POINT('Ctrl Pts',(-20.5632211986325,18.1452444677378,
-4.64575116850041));
#109905=CARTESIAN_POINT('Ctrl Pts',(-20.5702301397846,18.1573663179927,
-4.6465759652113));
#109906=CARTESIAN_POINT('Ctrl Pts',(-20.6269889107861,18.2578165014144,
-4.65333768728098));
#109907=CARTESIAN_POINT('Ctrl Pts',(-20.6704588979085,18.3495497424042,
-4.6590410392201));
#109908=CARTESIAN_POINT('Ctrl Pts',(-20.7124627579728,18.4576170828737,
-4.66542622172685));
#109909=CARTESIAN_POINT('Ctrl Pts',(-20.7175926300245,18.4712292481404,
-4.66622485020144));
#109910=CARTESIAN_POINT('Ctrl Pts',(-20.7225805995351,18.4848896783871,
-4.66702134980151));
#109911=CARTESIAN_POINT('',(-20.8509999970067,19.2108919587094,-3.68920544123732));
#109912=CARTESIAN_POINT('Ctrl Pts',(-20.722580615654,18.4848897225317,-4.44630506752222));
#109913=CARTESIAN_POINT('Ctrl Pts',(-20.7059750647656,18.4394125028398,
-4.44325065798364));
#109914=CARTESIAN_POINT('Ctrl Pts',(-20.687813946497,18.3945171880631,-4.44012932677062));
#109915=CARTESIAN_POINT('Ctrl Pts',(-20.5919077352346,18.1790049071769,
-4.42474712639804));
#109916=CARTESIAN_POINT('Ctrl Pts',(-20.4932538286155,18.0185737177301,
-4.41214844665518));
#109917=CARTESIAN_POINT('Ctrl Pts',(-20.3393454720932,17.8298067791279,
-4.39674511146122));
#109918=CARTESIAN_POINT('Ctrl Pts',(-20.3022242257996,17.7877985027087,
-4.39326457188379));
#109919=CARTESIAN_POINT('Ctrl Pts',(-20.2551574930418,17.7386163329588,
-4.3891206613092));
#109920=CARTESIAN_POINT('Ctrl Pts',(-20.2467641308248,17.7299941001212,
-4.38839142612606));
#109921=CARTESIAN_POINT('Ctrl Pts',(-20.2327633239974,17.715854734914,-4.38719082706546));
#109922=CARTESIAN_POINT('Ctrl Pts',(-20.22719791156,17.7102965434215,-4.38671763388843));
#109923=CARTESIAN_POINT('Ctrl Pts',(-20.2170712326321,17.7002951106483,
-4.38586386176407));
#109924=CARTESIAN_POINT('Ctrl Pts',(-20.2125206719013,17.6958412070332,
-4.38548281432127));
#109925=CARTESIAN_POINT('Ctrl Pts',(-20.2027146322228,17.6863296991088,
-4.38466722087729));
#109926=CARTESIAN_POINT('Ctrl Pts',(-20.1974529597136,17.6812785763177,
-4.38423296041831));
#109927=CARTESIAN_POINT('Ctrl Pts',(-20.1830322479959,17.6675774231107,
-4.38305183146454));
#109928=CARTESIAN_POINT('Ctrl Pts',(-20.1738218416472,17.6589817071865,
-4.38230730786569));
#109929=CARTESIAN_POINT('Ctrl Pts',(-20.1246864970084,17.613939464373,-4.3783862137726));
#109930=CARTESIAN_POINT('Ctrl Pts',(-20.0834512253969,17.5789481009122,
-4.37527148823535));
#109931=CARTESIAN_POINT('Ctrl Pts',(-19.8904546629418,17.4274970951095,
-4.36137502640494));
#109932=CARTESIAN_POINT('Ctrl Pts',(-19.7246990486941,17.3303672047068,
-4.35135083627903));
#109933=CARTESIAN_POINT('Ctrl Pts',(-19.5328889714748,17.2504543797712,
-4.33979977051271));
#109934=CARTESIAN_POINT('Ctrl Pts',(-19.5175431875423,17.2442710479173,
-4.33887527946643));
#109935=CARTESIAN_POINT('Ctrl Pts',(-19.4525630585937,17.2189695945454,
-4.33495312214234));
#109936=CARTESIAN_POINT('Ctrl Pts',(-19.402293945906,17.2015472893796,-4.33190075803477));
#109937=CARTESIAN_POINT('Ctrl Pts',(-19.3430951221604,17.1834971006527,
-4.32822798148205));
#109938=CARTESIAN_POINT('Ctrl Pts',(-19.3347477731283,17.1810081325573,
-4.32770831536781));
#109939=CARTESIAN_POINT('Ctrl Pts',(-19.322083321175,17.1773168663385,-4.32691685596373));
#109940=CARTESIAN_POINT('Ctrl Pts',(-19.3177772525911,17.1760766109527,
-4.3266472213027));
#109941=CARTESIAN_POINT('Ctrl Pts',(-19.3100395890977,17.1738745515415,
-4.32616170707437));
#109942=CARTESIAN_POINT('Ctrl Pts',(-19.306609477271,17.1729077333922,-4.32594612289562));
#109943=CARTESIAN_POINT('Ctrl Pts',(-19.2991493967633,17.1708253398275,
-4.3254764697924));
#109944=CARTESIAN_POINT('Ctrl Pts',(-19.2951186120151,17.1697130561275,
-4.32522221903621));
#109945=CARTESIAN_POINT('Ctrl Pts',(-19.2837833131081,17.1666212230823,
-4.32450589440381));
#109946=CARTESIAN_POINT('Ctrl Pts',(-19.2764715266618,17.1646689139651,
-4.32404228847298));
#109947=CARTESIAN_POINT('Ctrl Pts',(-19.2326172483193,17.1532110035142,
-4.32125311852511));
#109948=CARTESIAN_POINT('Ctrl Pts',(-19.195838646655,17.1446458747669,-4.31887844929928));
#109949=CARTESIAN_POINT('Ctrl Pts',(-19.0738704374249,17.1196601704844,
-4.31093007550174));
#109950=CARTESIAN_POINT('Ctrl Pts',(-18.9879029346462,17.107492075934,-4.30521428398382));
#109951=CARTESIAN_POINT('Ctrl Pts',(-18.7261743169917,17.0867263830177,
-4.28786757581524));
#109952=CARTESIAN_POINT('Ctrl Pts',(-18.5498243946029,17.0947054605463,
-4.27632320851312));
#109953=CARTESIAN_POINT('Ctrl Pts',(-18.3538351297174,17.1282875791455,
-4.26408422115121));
#109954=CARTESIAN_POINT('Ctrl Pts',(-18.3312646901161,17.1325340532159,
-4.26268235718761));
#109955=CARTESIAN_POINT('Ctrl Pts',(-18.2994198446103,17.1390636754515,
-4.26071454750265));
#109956=CARTESIAN_POINT('Ctrl Pts',(-18.2900855430588,17.1410434777456,
-4.26013897797442));
#109957=CARTESIAN_POINT('Ctrl Pts',(-18.2749371557044,17.1443636270118,
-4.25920682258078));
#109958=CARTESIAN_POINT('Ctrl Pts',(-18.2691148663045,17.145665546026,-4.25884901077867));
#109959=CARTESIAN_POINT('Ctrl Pts',(-18.2569362435264,17.1484429097456,
-4.25810150661029));
#109960=CARTESIAN_POINT('Ctrl Pts',(-18.250581063225,17.1499231670467,-4.25771197316286));
#109961=CARTESIAN_POINT('Ctrl Pts',(-18.235473507884,17.1535157594482,-4.2567872037155));
#109962=CARTESIAN_POINT('Ctrl Pts',(-18.2267275190173,17.1556546038896,
-4.25625282683619));
#109963=CARTESIAN_POINT('Ctrl Pts',(-18.1972849081804,17.1630542184312,
-4.25445701876249));
#109964=CARTESIAN_POINT('Ctrl Pts',(-18.1766538907685,17.1685724302502,
-4.25320389844311));
#109965=CARTESIAN_POINT('Ctrl Pts',(-18.0646434242797,17.200355729808,-4.24642379584635));
#109966=CARTESIAN_POINT('Ctrl Pts',(-17.9750242182833,17.2324430964639,
-4.24109112091645));
#109967=CARTESIAN_POINT('Ctrl Pts',(-17.7316872667449,17.3385459389017,
-4.22648647745302));
#109968=CARTESIAN_POINT('Ctrl Pts',(-17.5843272499079,17.4252352698438,
-4.21752391412763));
#109969=CARTESIAN_POINT('Ctrl Pts',(-17.4194462256235,17.5511756457574,
-4.20567782967415));
#109970=CARTESIAN_POINT('Ctrl Pts',(-17.3905302472254,17.5744923895132,
-4.20352096207324));
#109971=CARTESIAN_POINT('Ctrl Pts',(-17.356788313006,17.603197684604,-4.20088735424399));
#109972=CARTESIAN_POINT('Ctrl Pts',(-17.351355787271,17.607867037987,-4.20045961333416));
#109973=CARTESIAN_POINT('Ctrl Pts',(-17.342535131102,17.6155267349443,-4.19975880212612));
#109974=CARTESIAN_POINT('Ctrl Pts',(-17.3391326419715,17.6185005577641,
-4.19948692657381));
#109975=CARTESIAN_POINT('Ctrl Pts',(-17.3330618671946,17.6238408812672,
-4.19899901699868));
#109976=CARTESIAN_POINT('Ctrl Pts',(-17.3303900175179,17.6262032505929,
-4.1987832911206));
#109977=CARTESIAN_POINT('Ctrl Pts',(-17.3246196760867,17.6313312526248,
-4.19831523404082));
#109978=CARTESIAN_POINT('Ctrl Pts',(-17.3215233919688,17.6340992168344,
-4.19806273133768));
#109979=CARTESIAN_POINT('Ctrl Pts',(-17.3129046318491,17.6418498225444,
-4.19735614318283));
#109980=CARTESIAN_POINT('Ctrl Pts',(-17.3074003041195,17.6468524274458,
-4.19690059048515));
#109981=CARTESIAN_POINT('Ctrl Pts',(-17.2757272576154,17.6759447152149,
-4.19425490305327));
#109982=CARTESIAN_POINT('Ctrl Pts',(-17.2501442479108,17.7006603428095,
-4.19202124248181));
#109983=CARTESIAN_POINT('Ctrl Pts',(-17.170173703602,17.7819130657839,-4.18475680991518));
#109984=CARTESIAN_POINT('Ctrl Pts',(-17.1183030536216,17.8408307157983,
-4.17960781614375));
#109985=CARTESIAN_POINT('Ctrl Pts',(-16.9535271245193,18.050393603072,-4.16201216346093));
#109986=CARTESIAN_POINT('Ctrl Pts',(-16.8574399055746,18.213181446054,-4.14960339835183));
#109987=CARTESIAN_POINT('Ctrl Pts',(-16.7756311802523,18.4066633888918,
-4.13668824432176));
#109988=CARTESIAN_POINT('Ctrl Pts',(-16.7674387063076,18.4269065410672,
-4.13535622741268));
#109989=CARTESIAN_POINT('Ctrl Pts',(-16.756524488722,18.4551227400292,-4.13352546182279));
#109990=CARTESIAN_POINT('Ctrl Pts',(-16.7535351252433,18.4629901652382,
-4.1330177513417));
#109991=CARTESIAN_POINT('Ctrl Pts',(-16.7484717503316,18.4765591416759,
-4.1321467723836));
#109992=CARTESIAN_POINT('Ctrl Pts',(-16.7463752024883,18.4822521217081,
-4.13178275285782));
#109993=CARTESIAN_POINT('Ctrl Pts',(-16.7420984657371,18.4940209588976,
-4.13103310100896));
#109994=CARTESIAN_POINT('Ctrl Pts',(-16.739921534041,18.5000979388113,-4.1306475805136));
#109995=CARTESIAN_POINT('Ctrl Pts',(-16.7349119396592,18.5142864679103,
-4.12975107784716));
#109996=CARTESIAN_POINT('Ctrl Pts',(-16.7321007820105,18.5224055307174,
-4.12924081421579));
#109997=CARTESIAN_POINT('Ctrl Pts',(-16.7232281509539,18.5485446979623,
-4.12760664635381));
#109998=CARTESIAN_POINT('Ctrl Pts',(-16.7173598591104,18.5666297390906,
-4.12648911944515));
#109999=CARTESIAN_POINT('Ctrl Pts',(-16.6890915632315,18.6579188087531,
-4.12091036382826));
#110000=CARTESIAN_POINT('Ctrl Pts',(-16.6704290036546,18.7322246281499,
-4.11657226150934));
#110001=CARTESIAN_POINT('Ctrl Pts',(-16.6348788992771,18.9152679743165,
-4.10620976643113));
#110002=CARTESIAN_POINT('Ctrl Pts',(-16.6223585149199,19.0246189832096,
-4.10029474841313));
#110003=CARTESIAN_POINT('Ctrl Pts',(-16.6158392212417,19.2047929696516,
-4.09047561005596));
#110004=CARTESIAN_POINT('Ctrl Pts',(-16.6168040098771,19.275215132183,-4.08661644390735));
#110005=CARTESIAN_POINT('Ctrl Pts',(-16.6243183281359,19.3932906483853,
-4.07993139949352));
#110006=CARTESIAN_POINT('Ctrl Pts',(-16.6289862469277,19.4410064665367,
-4.07717017350487));
#110007=CARTESIAN_POINT('Ctrl Pts',(-16.6362824266962,19.4961837374563,
-4.07386566470026));
#110008=CARTESIAN_POINT('Ctrl Pts',(-16.6373379659448,19.5038431188875,
-4.07340444064743));
#110009=CARTESIAN_POINT('Ctrl Pts',(-16.6390940231692,19.5160892927219,
-4.07266274657372));
#110010=CARTESIAN_POINT('Ctrl Pts',(-16.639767715947,19.5206799441147,-4.07238375076097));
#110011=CARTESIAN_POINT('Ctrl Pts',(-16.6409890215128,19.5288158470887,
-4.07188752889022));
#110012=CARTESIAN_POINT('Ctrl Pts',(-16.6415305602545,19.5323619646026,
-4.07167064878496));
#110013=CARTESIAN_POINT('Ctrl Pts',(-16.642699111912,19.5398857089864,-4.07120920979719));
#110014=CARTESIAN_POINT('Ctrl Pts',(-16.6433284510067,19.5438628662043,
-4.07096452691937));
#110015=CARTESIAN_POINT('Ctrl Pts',(-16.6450612823622,19.5546148278431,
-4.07030103345757));
#110016=CARTESIAN_POINT('Ctrl Pts',(-16.6461863728701,19.5613860318957,
-4.06988102750178));
#110017=CARTESIAN_POINT('Ctrl Pts',(-16.6519835356465,19.5952559195814,
-4.06776971895603));
#110018=CARTESIAN_POINT('Ctrl Pts',(-16.6571501298382,19.6222658739377,
-4.06605262054874));
#110019=CARTESIAN_POINT('Ctrl Pts',(-16.6736966018307,19.7004790971315,
-4.06099777990903));
#110020=CARTESIAN_POINT('Ctrl Pts',(-16.6864546820172,19.7513677512802,
-4.0576054311363));
#110021=CARTESIAN_POINT('Ctrl Pts',(-16.7401427624127,19.9361286281072,
-4.04502369798133));
#110022=CARTESIAN_POINT('Ctrl Pts',(-16.79243408485,20.0663388274407,-4.0356644091744));
#110023=CARTESIAN_POINT('Ctrl Pts',(-16.900499725592,20.2734155992247,-4.02055860764105));
#110024=CARTESIAN_POINT('Ctrl Pts',(-16.9492643995588,20.3534417420942,
-4.01465120724975));
#110025=CARTESIAN_POINT('Ctrl Pts',(-17.011125094351,20.4412771087141,-4.00809548250086));
#110026=CARTESIAN_POINT('Ctrl Pts',(-17.0191872008816,20.4524897433753,
-4.00725703246946));
#110027=CARTESIAN_POINT('Ctrl Pts',(-17.0322783287679,20.4703258062753,
-4.00592054850583));
#110028=CARTESIAN_POINT('Ctrl Pts',(-17.0372375582211,20.4769997440524,
-4.00541983201658));
#110029=CARTESIAN_POINT('Ctrl Pts',(-17.0461042224076,20.4887864641762,
-4.00453434448291));
#110030=CARTESIAN_POINT('Ctrl Pts',(-17.0499958671259,20.4939109423211,
-4.00414896296385));
#110031=CARTESIAN_POINT('Ctrl Pts',(-17.0581443281952,20.5045397882266,
-4.00334875529804));
#110032=CARTESIAN_POINT('Ctrl Pts',(-17.0624050450654,20.5100410789732,
-4.00293408937593));
#110033=CARTESIAN_POINT('Ctrl Pts',(-17.0735215436073,20.5242490626487,
-4.00186179521339));
#110034=CARTESIAN_POINT('Ctrl Pts',(-17.080418760196,20.5329231804923,-4.00120582230734));
#110035=CARTESIAN_POINT('Ctrl Pts',(-17.1104884222961,20.5701359542076,
-3.9983853637443));
#110036=CARTESIAN_POINT('Ctrl Pts',(-17.1343347539008,20.5981235437464,
-3.99624816700779));
#110037=CARTESIAN_POINT('Ctrl Pts',(-17.1994260566657,20.6706064196943,
-3.99065513274964));
#110038=CARTESIAN_POINT('Ctrl Pts',(-17.2418758012716,20.7139751442436,
-3.98724833320382));
#110039=CARTESIAN_POINT('Ctrl Pts',(-17.4049735342669,20.8668722265933,
-3.9748706233802));
#110040=CARTESIAN_POINT('Ctrl Pts',(-17.5362656309755,20.964182844412,-3.96628104198771));
#110041=CARTESIAN_POINT('Ctrl Pts',(-17.7270418601467,21.074063453883,-3.95393910670973));
#110042=CARTESIAN_POINT('Ctrl Pts',(-17.7778138397209,21.1006234864385,
-3.95066139504684));
#110043=CARTESIAN_POINT('Ctrl Pts',(-17.837614992549,21.128879453842,-3.94673759169723));
#110044=CARTESIAN_POINT('Ctrl Pts',(-17.8456586124068,21.1326183944585,
-3.94620852465209));
#110045=CARTESIAN_POINT('Ctrl Pts',(-17.8578318697443,21.1381841625579,
-3.94540553833769));
#110046=CARTESIAN_POINT('Ctrl Pts',(-17.8619443604361,21.1400485606969,
-3.94513387280138));
#110047=CARTESIAN_POINT('Ctrl Pts',(-17.8693154969831,21.1433618782294,
-3.94464618890131));
#110048=CARTESIAN_POINT('Ctrl Pts',(-17.8725718664981,21.144815732879,-3.94443047748826));
#110049=CARTESIAN_POINT('Ctrl Pts',(-17.8796309339621,21.1479459902976,
-3.94396227619773));
#110050=CARTESIAN_POINT('Ctrl Pts',(-17.883434847053,21.1496194031421,-3.94370961387164));
#110051=CARTESIAN_POINT('Ctrl Pts',(-17.89407163929,21.1542613951569,-3.94300213842293));
#110052=CARTESIAN_POINT('Ctrl Pts',(-17.9009152194604,21.1572050882865,
-3.94254585220056));
#110053=CARTESIAN_POINT('Ctrl Pts',(-17.9406995721641,21.1740696165025,
-3.93988749512523));
#110054=CARTESIAN_POINT('Ctrl Pts',(-17.9739712480407,21.1871892200748,
-3.93764141976049));
#110055=CARTESIAN_POINT('Ctrl Pts',(-18.0819002114488,21.2266188792609,
-3.93031837172091));
#110056=CARTESIAN_POINT('Ctrl Pts',(-18.1577034764265,21.2495863320778,
-3.92512120296864));
#110057=CARTESIAN_POINT('Ctrl Pts',(-18.4163930834376,21.3123823230059,
-3.90754875652674));
#110058=CARTESIAN_POINT('Ctrl Pts',(-18.6032674921169,21.3322305685399,
-3.89521656054633));
#110059=CARTESIAN_POINT('Ctrl Pts',(-18.8122853022599,21.3266659299767,
-3.88235981438239));
#110060=CARTESIAN_POINT('Ctrl Pts',(-18.8342203090713,21.3257403770736,
-3.88102059158552));
#110061=CARTESIAN_POINT('Ctrl Pts',(-18.8645581898705,21.3239871513727,
-3.87918159010935));
#110062=CARTESIAN_POINT('Ctrl Pts',(-18.8729758702505,21.3234502014291,
-3.87867274426296));
#110063=CARTESIAN_POINT('Ctrl Pts',(-18.887447045316,21.3224402355236,-3.87780033486632));
#110064=CARTESIAN_POINT('Ctrl Pts',(-18.8935020792573,21.3219914618044,
-3.87743601465167));
#110065=CARTESIAN_POINT('Ctrl Pts',(-18.9059877768061,21.3210120468745,
-3.87668621498173));
#110066=CARTESIAN_POINT('Ctrl Pts',(-18.9124181189947,21.3204780419723,
-3.87630084527842));
#110067=CARTESIAN_POINT('Ctrl Pts',(-18.9273880644794,21.3191659290448,
-3.87540549167693));
#110068=CARTESIAN_POINT('Ctrl Pts',(-18.9359256204032,21.3183653159795,
-3.87489622062075));
#110069=CARTESIAN_POINT('Ctrl Pts',(-18.9632838113231,21.3156320049038,
-3.87326848578385));
#110070=CARTESIAN_POINT('Ctrl Pts',(-18.9820838221897,21.3134988451238,
-3.87215632796617));
#110071=CARTESIAN_POINT('Ctrl Pts',(-19.076111084982,21.3015511723619,-3.86662268681255));
#110072=CARTESIAN_POINT('Ctrl Pts',(-19.1508051352289,21.2879495495841,
-3.86232201239333));
#110073=CARTESIAN_POINT('Ctrl Pts',(-19.3897571046286,21.2310227002554,
-3.84866507305576));
#110074=CARTESIAN_POINT('Ctrl Pts',(-19.5495534728259,21.17196273852,-3.83973272497251));
#110075=CARTESIAN_POINT('Ctrl Pts',(-19.7070546496591,21.0911347633064,
-3.82981948014393));
#110076=CARTESIAN_POINT('Ctrl Pts',(-19.7135192273012,21.0877749361364,
-3.82941042806757));
#110077=CARTESIAN_POINT('Ctrl Pts',(-19.7658461518226,21.0602351244969,
-3.82608076115078));
#110078=CARTESIAN_POINT('Ctrl Pts',(-19.8108195617706,21.0344132046163,
-3.82310258205018));
#110079=CARTESIAN_POINT('Ctrl Pts',(-19.862078072236,21.002424725352,-3.81951656572646));
#110080=CARTESIAN_POINT('Ctrl Pts',(-19.8693324423462,20.9978360090875,
-3.81900444039618));
#110081=CARTESIAN_POINT('Ctrl Pts',(-19.8802669595482,20.9908259639047,
-3.81822518775246));
#110082=CARTESIAN_POINT('Ctrl Pts',(-19.8839678855247,20.9884369934817,
-3.81796015980053));
#110083=CARTESIAN_POINT('Ctrl Pts',(-19.8905072638132,20.9841868118488,
-3.81748954560463));
#110084=CARTESIAN_POINT('Ctrl Pts',(-19.8933487235558,20.9823303074161,
-3.81728427480743));
#110085=CARTESIAN_POINT('Ctrl Pts',(-19.8962080372767,20.9804523104059,
-3.81707691835121));
#110086=CARTESIAN_POINT('Ctrl Pts',(-19.8962303296467,20.9804376681762,
-3.81707530166751));
#110087=CARTESIAN_POINT('Ctrl Pts',(-19.8962744428708,20.9804086922277,
-3.8170721023991));
#110088=CARTESIAN_POINT('Ctrl Pts',(-19.8962962637689,20.9803943585053,
-3.81707051981324));
#110089=CARTESIAN_POINT('Ctrl Pts',(-19.8963394627228,20.9803659808111,
-3.81706738666693));
#110090=CARTESIAN_POINT('Ctrl Pts',(-19.8963608410129,20.9803519367085,
-3.81706583609136));
#110091=CARTESIAN_POINT('Ctrl Pts',(-19.8964031821414,20.9803241203286,
-3.81706276498454));
#110092=CARTESIAN_POINT('Ctrl Pts',(-19.8964241447903,20.9803103481972,
-3.81706124446875));
#110093=CARTESIAN_POINT('Ctrl Pts',(-19.896465679522,20.9802830594733,-3.81705823168152));
#110094=CARTESIAN_POINT('Ctrl Pts',(-19.896486251433,20.9802695430135,-3.81705673942413));
#110095=CARTESIAN_POINT('Ctrl Pts',(-19.8965270271773,20.9802427509154,
-3.81705378152711));
#110096=CARTESIAN_POINT('Ctrl Pts',(-19.8965472311577,20.9802294751987,
-3.81705231587829));
#110097=CARTESIAN_POINT('Ctrl Pts',(-19.8965872927629,20.9802031503677,
-3.81704940962698));
#110098=CARTESIAN_POINT('Ctrl Pts',(-19.8966071503057,20.980190101324,-3.81704796903181));
#110099=CARTESIAN_POINT('Ctrl Pts',(-19.8966465386126,20.9801642170241,
-3.8170451114716));
#110100=CARTESIAN_POINT('Ctrl Pts',(-19.8966660694778,20.980151381717,-3.81704369450048));
#110101=CARTESIAN_POINT('Ctrl Pts',(-19.8967048233049,20.9801259125321,
-3.8170408828227));
#110102=CARTESIAN_POINT('Ctrl Pts',(-19.8967240461949,20.980113278716,-3.81703948812242));
#110103=CARTESIAN_POINT('Ctrl Pts',(-19.8967622007905,20.9800882015677,
-3.81703671977675));
#110104=CARTESIAN_POINT('Ctrl Pts',(-19.8967811327355,20.9800757580917,
-3.81703534611507));
#110105=CARTESIAN_POINT('Ctrl Pts',(-19.8968187226173,20.980051050374,-3.81703261860354));
#110106=CARTESIAN_POINT('Ctrl Pts',(-19.8968373802171,20.9800387863663,
-3.81703126477916));
#110107=CARTESIAN_POINT('Ctrl Pts',(-19.8968744356703,20.9800144282479,
-3.81702857591038));
#110108=CARTESIAN_POINT('Ctrl Pts',(-19.8968928337469,20.9800023340021,
-3.81702724085072));
#110109=CARTESIAN_POINT('Ctrl Pts',(-19.8969293855696,20.9799783053081,
-3.8170245883955));
#110110=CARTESIAN_POINT('Ctrl Pts',(-19.8969475389266,20.9799663711265,
-3.81702327102905));
#110111=CARTESIAN_POINT('Ctrl Pts',(-19.8969836133572,20.9799426546733,
-3.81702065308862));
#110112=CARTESIAN_POINT('Ctrl Pts',(-19.8970015349597,20.9799308720641,
-3.81701935247707));
#110113=CARTESIAN_POINT('Ctrl Pts',(-19.897037159241,20.9799074500023,-3.81701676707932));
#110114=CARTESIAN_POINT('Ctrl Pts',(-19.8970548619125,20.9798958105639,
-3.8170154822944));
#110115=CARTESIAN_POINT('Ctrl Pts',(-19.8970900604822,20.9798726668831,
-3.81701292767036));
#110116=CARTESIAN_POINT('Ctrl Pts',(-19.8971075562713,20.9798611627211,
-3.81701165783986));
#110117=CARTESIAN_POINT('Ctrl Pts',(-19.8971423522257,20.979838282288,-3.81700913231754));
#110118=CARTESIAN_POINT('Ctrl Pts',(-19.8971596524187,20.9798269060069,
-3.81700787662437));
#110119=CARTESIAN_POINT('Ctrl Pts',(-19.8971940678818,20.9798042743233,
-3.81700537860199));
#110120=CARTESIAN_POINT('Ctrl Pts',(-19.8972111832209,20.9797930188831,
-3.81700413626839));
#110121=CARTESIAN_POINT('Ctrl Pts',(-19.8972452388249,20.9797706224274,
-3.81700166425211));
#110122=CARTESIAN_POINT('Ctrl Pts',(-19.8972621792767,20.9797594812963,
-3.81700043455645));
#110123=CARTESIAN_POINT('Ctrl Pts',(-19.8972958956464,20.9797373065482,
-3.81699798705266));
#110124=CARTESIAN_POINT('Ctrl Pts',(-19.8973126712783,20.9797262731261,
-3.81699676926585));
#110125=CARTESIAN_POINT('Ctrl Pts',(-19.8973460657701,20.979704308711,-3.81699434501791));
#110126=CARTESIAN_POINT('Ctrl Pts',(-19.8973626851149,20.9796933774055,
-3.8169931385221));
#110127=CARTESIAN_POINT('Ctrl Pts',(-19.8973957775178,20.9796716103456,
-3.81699073609651));
#110128=CARTESIAN_POINT('Ctrl Pts',(-19.8974122498914,20.9796607750474,
-3.81698954021688));
#110129=CARTESIAN_POINT('Ctrl Pts',(-19.8974450561344,20.9796391949006,
-3.81698715846008));
#110130=CARTESIAN_POINT('Ctrl Pts',(-19.8974613898706,20.9796284501451,
-3.816985972593));
#110131=CARTESIAN_POINT('Ctrl Pts',(-19.8974939258221,20.9796070465062,
-3.81698361035562));
#110132=CARTESIAN_POINT('Ctrl Pts',(-19.8975101284448,20.9795963873599,
-3.81698243395613));
#110133=CARTESIAN_POINT('Ctrl Pts',(-19.9010366626355,20.9772763327961,
-3.81672638259861));
#110134=CARTESIAN_POINT('Ctrl Pts',(-19.90454007555,20.9749565149277,-3.81647080495603));
#110135=CARTESIAN_POINT('Ctrl Pts',(-19.9146438603917,20.9682228436645,
-3.81573028884217));
#110136=CARTESIAN_POINT('Ctrl Pts',(-19.9212262516046,20.9637823225676,
-3.81524360649331));
#110137=CARTESIAN_POINT('Ctrl Pts',(-19.9649805550544,20.9339058640675,
-3.81198090566468));
#110138=CARTESIAN_POINT('Ctrl Pts',(-20.0013547278463,20.9073281151426,
-3.80913489913387));
#110139=CARTESIAN_POINT('Ctrl Pts',(-20.1314017937029,20.805787560074,-3.79853955773096));
#110140=CARTESIAN_POINT('Ctrl Pts',(-20.2195034184797,20.7240621272268,
-3.79054128137616));
#110141=CARTESIAN_POINT('Ctrl Pts',(-20.3983278644827,20.5274235264769,
-3.77303710140993));
#110142=CARTESIAN_POINT('Ctrl Pts',(-20.4850526415925,20.4096607018668,
-3.76364162942936));
#110143=CARTESIAN_POINT('Ctrl Pts',(-20.5662145455078,20.2716045912233,
-3.75386354284211));
#110144=CARTESIAN_POINT('Ctrl Pts',(-20.573315395492,20.2592419239892,-3.75299760626831));
#110145=CARTESIAN_POINT('Ctrl Pts',(-20.5844228950989,20.2394432049183,
-3.75162590654722));
#110146=CARTESIAN_POINT('Ctrl Pts',(-20.5885107681369,20.2320534415698,
-3.75111723260238));
#110147=CARTESIAN_POINT('Ctrl Pts',(-20.5956451443323,20.2189722344933,
-3.75022253661821));
#110148=CARTESIAN_POINT('Ctrl Pts',(-20.5987100188426,20.2132909836896,
-3.74983586159837));
#110149=CARTESIAN_POINT('Ctrl Pts',(-20.6049980505754,20.2015064018072,
-3.74903766144175));
#110150=CARTESIAN_POINT('Ctrl Pts',(-20.6082174450039,20.1954011417382,
-3.74862627333748));
#110151=CARTESIAN_POINT('Ctrl Pts',(-20.6164099513422,20.1796789912534,
-3.74757228452061));
#110152=CARTESIAN_POINT('Ctrl Pts',(-20.6213392921878,20.1700394234663,
-3.74693123246866));
#110153=CARTESIAN_POINT('Ctrl Pts',(-20.6416483698221,20.1295609626519,
-3.74426040839557));
#110154=CARTESIAN_POINT('Ctrl Pts',(-20.656348412728,20.0983856682844,-3.74225439505245));
#110155=CARTESIAN_POINT('Ctrl Pts',(-20.6926986687246,20.0161479234924,
-3.73708223303656));
#110156=CARTESIAN_POINT('Ctrl Pts',(-20.7131157143972,19.9645683766573,
-3.73395603980857));
#110157=CARTESIAN_POINT('Ctrl Pts',(-20.7650951439492,19.8165055270243,
-3.72523304451047));
#110158=CARTESIAN_POINT('Ctrl Pts',(-20.7917797123911,19.7184721801879,
-3.71975545207146));
#110159=CARTESIAN_POINT('Ctrl Pts',(-20.8346708694905,19.5000398021504,
-3.70765144336622));
#110160=CARTESIAN_POINT('Ctrl Pts',(-20.8477626284588,19.3794088283171,
-3.70102956499715));
#110161=CARTESIAN_POINT('Ctrl Pts',(-20.8507280218477,19.2468325356147,
-3.69321457045652));
#110162=CARTESIAN_POINT('Ctrl Pts',(-20.8508915532428,19.2353233999873,
-3.69253165719203));
#110163=CARTESIAN_POINT('Ctrl Pts',(-20.8509827839472,19.2202512109919,
-3.69163079221853));
#110164=CARTESIAN_POINT('Ctrl Pts',(-20.8509953546732,19.2166886124106,
-3.69141737774716));
#110165=CARTESIAN_POINT('Ctrl Pts',(-20.8509997176845,19.2123441308279,
-3.69115652413364));
#110166=CARTESIAN_POINT('Ctrl Pts',(-20.8510000697334,19.2115622346711,
-3.69110955337614));
#110167=CARTESIAN_POINT('Ctrl Pts',(-20.850999988604,19.2107803400989,-3.6910625588116));
#110168=CARTESIAN_POINT('Ctrl Pts',(-20.8509999976816,19.2109009238279,
-3.6890562790225));
#110169=CARTESIAN_POINT('Ctrl Pts',(-20.8509997507685,19.2056250329455,
-3.68873698393553));
#110170=CARTESIAN_POINT('Ctrl Pts',(-20.8509797813958,19.2003491960952,
-3.68841768884856));
#110171=CARTESIAN_POINT('Ctrl Pts',(-20.8509400905189,19.1950735078034,
-3.68809839376159));
#110172=CARTESIAN_POINT('Ctrl Pts',(-20.8503947174663,19.1225828384675,
-3.68371111511857));
#110173=CARTESIAN_POINT('Ctrl Pts',(-20.8461205125477,19.0499787438565,
-3.67932383647555));
#110174=CARTESIAN_POINT('Ctrl Pts',(-20.8381029246807,18.9776764427882,
-3.67493655783253));
#110175=CARTESIAN_POINT('Ctrl Pts',(-20.8300957679091,18.9054682089396,
-3.67055498715589));
#110176=CARTESIAN_POINT('Ctrl Pts',(-20.8183549391171,18.8335614650894,
-3.66617341647925));
#110177=CARTESIAN_POINT('Ctrl Pts',(-20.8029178766155,18.7623711781205,
-3.66179184580261));
#110178=CARTESIAN_POINT('Ctrl Pts',(-20.7874985864815,18.6912628510425,
-3.6574153195368));
#110179=CARTESIAN_POINT('Ctrl Pts',(-20.7683916165293,18.6208698115597,
-3.65303879327099));
#110180=CARTESIAN_POINT('Ctrl Pts',(-20.745685938542,18.5515997538124,-3.64866226700518));
#110181=CARTESIAN_POINT('Ctrl Pts',(-20.7383572985718,18.5292416760561,
-3.64724966944521));
#110182=CARTESIAN_POINT('Ctrl Pts',(-20.7306541493028,18.5070005132541,
-3.64583707188523));
#110183=CARTESIAN_POINT('Ctrl Pts',(-20.7225806137986,18.4848897174502,
-3.64442447432525));
#110184=CARTESIAN_POINT('Origin',(-18.734,19.211,0.));
#110185=CARTESIAN_POINT('',(-20.7202231698227,18.4857291668959,-2.84456322999407));
#110186=CARTESIAN_POINT('',(-20.7225805974208,18.4848896725968,-3.06515445288237));
#110187=CARTESIAN_POINT('',(-20.7225806137986,18.4848897174502,0.));
#110188=CARTESIAN_POINT('Ctrl Pts',(-20.7225805974208,18.4848896725968,
-3.06515445288237));
#110189=CARTESIAN_POINT('Ctrl Pts',(-20.775012214741,18.6284828607934,-3.07512670877195));
#110190=CARTESIAN_POINT('Ctrl Pts',(-20.8117530652564,18.7773757226491,
-3.085373849156));
#110191=CARTESIAN_POINT('Ctrl Pts',(-20.8399080750925,18.9868384898001,
-3.09899376967294));
#110192=CARTESIAN_POINT('Ctrl Pts',(-20.8452891067731,19.0449985660853,
-3.10269880438067));
#110193=CARTESIAN_POINT('Ctrl Pts',(-20.8500786760388,19.1390322794493,
-3.10855849336733));
#110194=CARTESIAN_POINT('Ctrl Pts',(-20.8509926290692,19.1747954495418,
-3.11075700017239));
#110195=CARTESIAN_POINT('Ctrl Pts',(-20.8510022031441,19.221539806733,-3.11359308617401));
#110196=CARTESIAN_POINT('Ctrl Pts',(-20.8509191302513,19.2325132220007,
-3.11425618280915));
#110197=CARTESIAN_POINT('Ctrl Pts',(-20.8506443290578,19.250419142171,-3.11533393209238));
#110198=CARTESIAN_POINT('Ctrl Pts',(-20.8505038547006,19.2573521231421,
-3.11575018257836));
#110199=CARTESIAN_POINT('Ctrl Pts',(-20.8501671509656,19.2707252043125,
-3.11655112251225));
#110200=CARTESIAN_POINT('Ctrl Pts',(-20.849975581304,19.2771653353186,-3.11693595340708));
#110201=CARTESIAN_POINT('Ctrl Pts',(-20.8494626510919,19.2921125322765,
-3.11782712519268));
#110202=CARTESIAN_POINT('Ctrl Pts',(-20.8491193701468,19.3006187721233,
-3.11833277398264));
#110203=CARTESIAN_POINT('Ctrl Pts',(-20.847863432287,19.3276865154241,-3.11993717187166));
#110204=CARTESIAN_POINT('Ctrl Pts',(-20.8467576611286,19.3462384974586,
-3.12102987033051));
#110205=CARTESIAN_POINT('Ctrl Pts',(-20.843613922483,19.3894038934937,-3.12355755269016));
#110206=CARTESIAN_POINT('Ctrl Pts',(-20.8413892435542,19.4140012283545,
-3.12498673363693));
#110207=CARTESIAN_POINT('Ctrl Pts',(-20.8320826229699,19.5000814633134,
-3.12995533127274));
#110208=CARTESIAN_POINT('Ctrl Pts',(-20.8227356741548,19.561289781124,-3.13342816695607));
#110209=CARTESIAN_POINT('Ctrl Pts',(-20.7831185790056,19.7614667236369,
-3.14471626565864));
#110210=CARTESIAN_POINT('Ctrl Pts',(-20.7415412504979,19.8977869162543,
-3.15226972708296));
#110211=CARTESIAN_POINT('Ctrl Pts',(-20.6575318191133,20.0983454768993,
-3.16430899961774));
#110212=CARTESIAN_POINT('Ctrl Pts',(-20.6247655991321,20.1661751433871,
-3.16856365020628));
#110213=CARTESIAN_POINT('Ctrl Pts',(-20.5838856182396,20.2404183812028,
-3.1735867907708));
#110214=CARTESIAN_POINT('Ctrl Pts',(-20.5792539450497,20.2486978726146,
-3.17415229018995));
#110215=CARTESIAN_POINT('Ctrl Pts',(-20.5723045719363,20.2609267913955,
-3.17499588748264));
#110216=CARTESIAN_POINT('Ctrl Pts',(-20.5700293810929,20.2649004114961,
-3.17527131949992));
#110217=CARTESIAN_POINT('Ctrl Pts',(-20.5659565704835,20.2719603577674,
-3.17576308529832));
#110218=CARTESIAN_POINT('Ctrl Pts',(-20.5641640141925,20.2750495466917,
-3.17597909074816));
#110219=CARTESIAN_POINT('Ctrl Pts',(-20.5602911420992,20.2816850928805,
-3.17644486281203));
#110220=CARTESIAN_POINT('Ctrl Pts',(-20.5582083408837,20.2852298786632,
-3.17669478550824));
#110221=CARTESIAN_POINT('Ctrl Pts',(-20.5524255451225,20.295006486479,-3.17738707893546));
#110222=CARTESIAN_POINT('Ctrl Pts',(-20.5487038952051,20.301225341437,-3.17783082404308));
#110223=CARTESIAN_POINT('Ctrl Pts',(-20.5280542177102,20.3353321408251,
-3.18028263168886));
#110224=CARTESIAN_POINT('Ctrl Pts',(-20.5105162007989,20.3628433991225,
-3.18232723262178));
#110225=CARTESIAN_POINT('Ctrl Pts',(-20.40178357793,20.5250150383694,-3.19473512450942));
#110226=CARTESIAN_POINT('Ctrl Pts',(-20.295956055093,20.6492040214767,-3.20568691734734));
#110227=CARTESIAN_POINT('Ctrl Pts',(-20.0915016472688,20.8396550263871,
-3.22393800697634));
#110228=CARTESIAN_POINT('Ctrl Pts',(-19.9995963150936,20.9120589895192,
-3.23137712523197));
#110229=CARTESIAN_POINT('Ctrl Pts',(-19.8902556615087,20.9844052049271,
-3.23938257961643));
#110230=CARTESIAN_POINT('Ctrl Pts',(-19.8782592753593,20.9921692513918,
-3.24025053463299));
#110231=CARTESIAN_POINT('Ctrl Pts',(-19.8590411983013,21.0043328690579,
-3.24162481633562));
#110232=CARTESIAN_POINT('Ctrl Pts',(-19.8518703318491,21.0088115589598,
-3.24213407091119));
#110233=CARTESIAN_POINT('Ctrl Pts',(-19.8391760174011,21.0166346971543,
-3.24302944204619));
#110234=CARTESIAN_POINT('Ctrl Pts',(-19.8336637739074,21.0199970355959,
-3.24341621470033));
#110235=CARTESIAN_POINT('Ctrl Pts',(-19.8222308205539,21.0268992992335,
-3.24421428482523));
#110236=CARTESIAN_POINT('Ctrl Pts',(-19.8163080120847,21.030435613719,-3.24462544689818));
#110237=CARTESIAN_POINT('Ctrl Pts',(-19.801060512177,21.0394385946097,-3.24567816979294));
#110238=CARTESIAN_POINT('Ctrl Pts',(-19.7917109742872,21.0448629535321,
-3.24631818923801));
#110239=CARTESIAN_POINT('Ctrl Pts',(-19.7525150439798,21.067203937102,-3.24897895783253));
#110240=CARTESIAN_POINT('Ctrl Pts',(-19.7223002287249,21.0834659691048,
-3.25097617591453));
#110241=CARTESIAN_POINT('Ctrl Pts',(-19.6425552123937,21.1239175029515,
-3.2561205376204));
#110242=CARTESIAN_POINT('Ctrl Pts',(-19.5924513012576,21.1469204415304,
-3.25922828654674));
#110243=CARTESIAN_POINT('Ctrl Pts',(-19.4404219972875,21.209653104444,-3.26837302845841));
#110244=CARTESIAN_POINT('Ctrl Pts',(-19.3362575590134,21.2434696765374,
-3.27426129316222));
#110245=CARTESIAN_POINT('Ctrl Pts',(-19.1852135492876,21.2798674789338,
-3.28272017110981));
#110246=CARTESIAN_POINT('Ctrl Pts',(-19.1401414519775,21.2891855525484,
-3.28523620590521));
#110247=CARTESIAN_POINT('Ctrl Pts',(-19.073001551379,21.3007981888584,-3.28901509784947));
#110248=CARTESIAN_POINT('Ctrl Pts',(-19.0511428507339,21.3042269076325,
-3.29025024055008));
#110249=CARTESIAN_POINT('Ctrl Pts',(-18.978253818477,21.3144922634723,-3.29439637283993));
#110250=CARTESIAN_POINT('Ctrl Pts',(-18.9270320586601,21.3198094577491,
-3.29735453965841));
#110251=CARTESIAN_POINT('Ctrl Pts',(-18.8670520534064,21.3238324097688,
-3.30092250667448));
#110252=CARTESIAN_POINT('Ctrl Pts',(-18.8584286452259,21.3243577896704,
-3.3014379830703));
#110253=CARTESIAN_POINT('Ctrl Pts',(-18.845343308835,21.3250746465095,-3.3022243006764));
#110254=CARTESIAN_POINT('Ctrl Pts',(-18.8408834728445,21.3253048185702,
-3.30249302502683));
#110255=CARTESIAN_POINT('Ctrl Pts',(-18.8328642775101,21.3256932516972,
-3.30297757446185));
#110256=CARTESIAN_POINT('Ctrl Pts',(-18.8293052210298,21.3258566402184,
-3.30319310935092));
#110257=CARTESIAN_POINT('Ctrl Pts',(-18.8215562313466,21.3261927787466,
-3.30366344825236));
#110258=CARTESIAN_POINT('Ctrl Pts',(-18.8173662457479,21.3263620619827,
-3.30391843844027));
#110259=CARTESIAN_POINT('Ctrl Pts',(-18.8055579570647,21.3268040013217,
-3.30463889504533));
#110260=CARTESIAN_POINT('Ctrl Pts',(-18.7979387349794,21.3270479548772,
-3.30510592140441));
#110261=CARTESIAN_POINT('Ctrl Pts',(-18.7515937563836,21.3282813056429,
-3.30795910531823));
#110262=CARTESIAN_POINT('Ctrl Pts',(-18.7128507610393,21.328248672019,-3.3103969694704));
#110263=CARTESIAN_POINT('Ctrl Pts',(-18.5834923031677,21.3245890866357,
-3.31866562074778));
#110264=CARTESIAN_POINT('Ctrl Pts',(-18.4931149887585,21.3162039811179,
-3.32465026798381));
#110265=CARTESIAN_POINT('Ctrl Pts',(-18.3372625355312,21.2915752780926,
-3.33507719097317));
#110266=CARTESIAN_POINT('Ctrl Pts',(-18.2714988683308,21.2779512213385,
-3.33951171173244));
#110267=CARTESIAN_POINT('Ctrl Pts',(-18.0953552671279,21.232630759643,-3.35138293638831));
#110268=CARTESIAN_POINT('Ctrl Pts',(-17.9867140704593,21.1950436445113,
-3.35868689673394));
#110269=CARTESIAN_POINT('Ctrl Pts',(-17.8685880837743,21.1430855425856,
-3.36656625559629));
#110270=CARTESIAN_POINT('Ctrl Pts',(-17.8555936912105,21.1372125274513,
-3.3674323841291));
#110271=CARTESIAN_POINT('Ctrl Pts',(-17.8349986670949,21.1276525337581,
-3.36880432942311));
#110272=CARTESIAN_POINT('Ctrl Pts',(-17.8273592228718,21.1240506622157,
-3.3693130586054));
#110273=CARTESIAN_POINT('Ctrl Pts',(-17.813919174055,21.11761531111,-3.37020781879654));
#110274=CARTESIAN_POINT('Ctrl Pts',(-17.8081096296087,21.1148008546797,
-3.37059450308193));
#110275=CARTESIAN_POINT('Ctrl Pts',(-17.7961157028666,21.1089224634733,
-3.37139269076218));
#110276=CARTESIAN_POINT('Ctrl Pts',(-17.7899332414578,21.1058547673412,
-3.37180405728046));
#110277=CARTESIAN_POINT('Ctrl Pts',(-17.7740927566258,21.0978980525252,
-3.3728579252438));
#110278=CARTESIAN_POINT('Ctrl Pts',(-17.7644569541153,21.0929650542106,
-3.37349887872411));
#110279=CARTESIAN_POINT('Ctrl Pts',(-17.7243189894809,21.072026541128,-3.37616874133761));
#110280=CARTESIAN_POINT('Ctrl Pts',(-17.6941709200601,21.0553511632146,
-3.37817391360766));
#110281=CARTESIAN_POINT('Ctrl Pts',(-17.6166177366247,21.0099488348847,
-3.38334341493393));
#110282=CARTESIAN_POINT('Ctrl Pts',(-17.5699091969802,20.9800826125672,
-3.38646784241915));
#110283=CARTESIAN_POINT('Ctrl Pts',(-17.4344713874162,20.8857918156409,
-3.39564166942676));
#110284=CARTESIAN_POINT('Ctrl Pts',(-17.3495158114413,20.8162746262539,
-3.40154244090375));
#110285=CARTESIAN_POINT('Ctrl Pts',(-17.225310181684,20.6974138547889,-3.41090368402622));
#110286=CARTESIAN_POINT('Ctrl Pts',(-17.1822206234332,20.6523712729702,
-3.41431616019914));
#110287=CARTESIAN_POINT('Ctrl Pts',(-17.1041137128793,20.5631562324361,
-3.4209687322884));
#110288=CARTESIAN_POINT('Ctrl Pts',(-17.0687514768634,20.5193585000381,
-3.42419111435789));
#110289=CARTESIAN_POINT('Ctrl Pts',(-17.0299084709903,20.4671206474124,
-3.4280532717781));
#110290=CARTESIAN_POINT('Ctrl Pts',(-17.024682418431,20.4599997675315,-3.42858014025258));
#110291=CARTESIAN_POINT('Ctrl Pts',(-17.0168571005632,20.4491960990727,
-3.42938043207831));
#110292=CARTESIAN_POINT('Ctrl Pts',(-17.0142247101722,20.4455372689714,
-3.42965162410959));
#110293=CARTESIAN_POINT('Ctrl Pts',(-17.009530899628,20.4389690695605,-3.4301388000767));
#110294=CARTESIAN_POINT('Ctrl Pts',(-17.0074651277757,20.4360628753863,
-3.43035447975497));
#110295=CARTESIAN_POINT('Ctrl Pts',(-17.0030041564275,20.4297533420393,
-3.43082301017017));
#110296=CARTESIAN_POINT('Ctrl Pts',(-17.0006116797986,20.4263482010923,
-3.4310760355064));
#110297=CARTESIAN_POINT('Ctrl Pts',(-16.9939489536351,20.4168056473766,
-3.43178553014063));
#110298=CARTESIAN_POINT('Ctrl Pts',(-16.9897012045009,20.410652704489,-3.43224348589867));
#110299=CARTESIAN_POINT('Ctrl Pts',(-16.9650749828866,20.3745738607738,
-3.43493097030043));
#110300=CARTESIAN_POINT('Ctrl Pts',(-16.9454356177525,20.3441535347104,
-3.43720561419485));
#110301=CARTESIAN_POINT('Ctrl Pts',(-16.8845208226642,20.2442683094055,
-3.44466468408632));
#110302=CARTESIAN_POINT('Ctrl Pts',(-16.8464403662523,20.1729425754835,
-3.4499739400314));
#110303=CARTESIAN_POINT('Ctrl Pts',(-16.7350609161826,19.9321063296024,
-3.46749411760044));
#110304=CARTESIAN_POINT('Ctrl Pts',(-16.679811808078,19.7551413958542,-3.47965067302103));
#110305=CARTESIAN_POINT('Ctrl Pts',(-16.644420229391,19.5513505656333,-3.49237226884231));
#110306=CARTESIAN_POINT('Ctrl Pts',(-16.6409649746219,19.5294125731856,
-3.49372720568573));
#110307=CARTESIAN_POINT('Ctrl Pts',(-16.6366688351066,19.4990326387749,
-3.49558412386552));
#110308=CARTESIAN_POINT('Ctrl Pts',(-16.6355326196902,19.490634535199,-3.49609540437961));
#110309=CARTESIAN_POINT('Ctrl Pts',(-16.6336676155139,19.4761977871781,
-3.49697088317598));
#110310=CARTESIAN_POINT('Ctrl Pts',(-16.632914372631,19.4701624573689,-3.49733585020302));
#110311=CARTESIAN_POINT('Ctrl Pts',(-16.6314163088384,19.45772329401,-3.49808597904101));
#110312=CARTESIAN_POINT('Ctrl Pts',(-16.6306747091785,19.4513191306483,
-3.49847103551335));
#110313=CARTESIAN_POINT('Ctrl Pts',(-16.6290188618575,19.4364247658055,
-3.49936397324148));
#110314=CARTESIAN_POINT('Ctrl Pts',(-16.6281267018042,19.4279321833656,
-3.49987115363617));
#110315=CARTESIAN_POINT('Ctrl Pts',(-16.6254423100766,19.4008001579353,
-3.50148539257099));
#110316=CARTESIAN_POINT('Ctrl Pts',(-16.6238459509339,19.3821419125915,
-3.50258629347942));
#110317=CARTESIAN_POINT('Ctrl Pts',(-16.6207016583426,19.3385961507694,
-3.50513574072868));
#110318=CARTESIAN_POINT('Ctrl Pts',(-16.6193454211627,19.3136973424467,
-3.50657834281728));
#110319=CARTESIAN_POINT('Ctrl Pts',(-16.6161237009833,19.2260680069441,
-3.51160889038332));
#110320=CARTESIAN_POINT('Ctrl Pts',(-16.6166075134445,19.1632819493389,
-3.51512831832152));
#110321=CARTESIAN_POINT('Ctrl Pts',(-16.6250814651082,19.0009996818185,
-3.52411210307554));
#110322=CARTESIAN_POINT('Ctrl Pts',(-16.6373157489602,18.9018832699166,
-3.52948492666197));
#110323=CARTESIAN_POINT('Ctrl Pts',(-16.670520079978,18.7323939734988,-3.53889238245229));
#110324=CARTESIAN_POINT('Ctrl Pts',(-16.6882399484974,18.6615661329534,
-3.5428948538745));
#110325=CARTESIAN_POINT('Ctrl Pts',(-16.7227536191045,18.548726786343,-3.54957986307738));
#110326=CARTESIAN_POINT('Ctrl Pts',(-16.7372983176322,18.5060889678022,
-3.55218006203142));
#110327=CARTESIAN_POINT('Ctrl Pts',(-16.7558692171201,18.4568480036578,
-3.55530559412347));
#110328=CARTESIAN_POINT('Ctrl Pts',(-16.758586181469,18.4497596506939,-3.55575854114978));
#110329=CARTESIAN_POINT('Ctrl Pts',(-16.7630100799767,18.438401215764,-3.55648943866805));
#110330=CARTESIAN_POINT('Ctrl Pts',(-16.7646929344959,18.4341217424347,
-3.55676598209404));
#110331=CARTESIAN_POINT('Ctrl Pts',(-16.7677114402685,18.4265185592222,
-3.55725944103238));
#110332=CARTESIAN_POINT('Ctrl Pts',(-16.7690415984745,18.423192719539,-3.55747602418443));
#110333=CARTESIAN_POINT('Ctrl Pts',(-16.7718940390878,18.416112833291,-3.55793865400805));
#110334=CARTESIAN_POINT('Ctrl Pts',(-16.7734186337819,18.4123598335622,
-3.5581848339624));
#110335=CARTESIAN_POINT('Ctrl Pts',(-16.7775969723956,18.4021583472559,
-3.55885652889874));
#110336=CARTESIAN_POINT('Ctrl Pts',(-16.7802717936093,18.395718626447,-3.55928328913915));
#110337=CARTESIAN_POINT('Ctrl Pts',(-16.7941805734154,18.3626943136724,
-3.56148553290922));
#110338=CARTESIAN_POINT('Ctrl Pts',(-16.8059249198367,18.3363296400597,
-3.56328949110968));
#110339=CARTESIAN_POINT('Ctrl Pts',(-16.8422023566247,18.2591745322882,
-3.56868780836322));
#110340=CARTESIAN_POINT('Ctrl Pts',(-16.8682294792941,18.2091170064076,
-3.57234519506903));
#110341=CARTESIAN_POINT('Ctrl Pts',(-16.9654409722727,18.0391068316999,
-3.58517874746336));
#110342=CARTESIAN_POINT('Ctrl Pts',(-17.0464589019846,17.9251754368153,
-3.59449352641585));
#110343=CARTESIAN_POINT('Ctrl Pts',(-17.1964521749631,17.7530821288048,
-3.60922168229466));
#110344=CARTESIAN_POINT('Ctrl Pts',(-17.2589716316657,17.6898580932503,
-3.6148165912939));
#110345=CARTESIAN_POINT('Ctrl Pts',(-17.3355028063266,17.6216347455071,
-3.6210718365345));
#110346=CARTESIAN_POINT('Ctrl Pts',(-17.345807302394,17.6126266515538,-3.621902697442));
#110347=CARTESIAN_POINT('Ctrl Pts',(-17.3624837694347,17.5983311683606,
-3.62322944020701));
#110348=CARTESIAN_POINT('Ctrl Pts',(-17.3688005311341,17.5929802397703,
-3.62372794308412));
#110349=CARTESIAN_POINT('Ctrl Pts',(-17.3800785175705,17.5835397229358,
-3.62461088479693));
#110350=CARTESIAN_POINT('Ctrl Pts',(-17.3850272611905,17.579435448605,-3.6249959223352));
#110351=CARTESIAN_POINT('Ctrl Pts',(-17.3953836569019,17.5709256311373,
-3.62579676809093));
#110352=CARTESIAN_POINT('Ctrl Pts',(-17.4007945460114,17.5665241355817,
-3.62621240935285));
#110353=CARTESIAN_POINT('Ctrl Pts',(-17.4149172235604,17.5551515417235,
-3.62729013481532));
#110354=CARTESIAN_POINT('Ctrl Pts',(-17.4236626164871,17.5482223731205,
-3.62795053153846));
#110355=CARTESIAN_POINT('Ctrl Pts',(-17.462015249492,17.5183252297807,-3.63081698006998));
#110356=CARTESIAN_POINT('Ctrl Pts',(-17.4921756353886,17.4960756329734,
-3.63299460364542));
#110357=CARTESIAN_POINT('Ctrl Pts',(-17.5740157056846,17.438993369862,-3.63871976806956));
#110358=CARTESIAN_POINT('Ctrl Pts',(-17.6266702472416,17.4056211601673,
-3.64221518485314));
#110359=CARTESIAN_POINT('Ctrl Pts',(-17.762143187295,17.3279192000335,-3.65085181638876));
#110360=CARTESIAN_POINT('Ctrl Pts',(-17.846580207941,17.2866856687517,-3.65591752775121));
#110361=CARTESIAN_POINT('Ctrl Pts',(-18.0473370176224,17.2046823227886,
-3.66771458562423));
#110362=CARTESIAN_POINT('Ctrl Pts',(-18.1650196021426,17.1681908909157,
-3.67445165462703));
#110363=CARTESIAN_POINT('Ctrl Pts',(-18.2944123109063,17.1401207531809,
-3.6822994345334));
#110364=CARTESIAN_POINT('Ctrl Pts',(-18.3036548467078,17.1381803665373,
-3.68286240744297));
#110365=CARTESIAN_POINT('Ctrl Pts',(-18.3173890072432,17.1353928189708,
-3.6837029494335));
#110366=CARTESIAN_POINT('Ctrl Pts',(-18.321871037331,17.1344982286412,-3.68397788062969));
#110367=CARTESIAN_POINT('Ctrl Pts',(-18.3298599463691,17.1329305670111,
-3.68446909959897));
#110368=CARTESIAN_POINT('Ctrl Pts',(-18.333365665195,17.1322518476713,-3.68468506188026));
#110369=CARTESIAN_POINT('Ctrl Pts',(-18.3409171302157,17.1308096702755,
-3.68515113846112));
#110370=CARTESIAN_POINT('Ctrl Pts',(-18.344963332439,17.1300491545875,-3.68540141094654));
#110371=CARTESIAN_POINT('Ctrl Pts',(-18.356163642402,17.1279777757268,-3.68609563745951));
#110372=CARTESIAN_POINT('Ctrl Pts',(-18.3633222474316,17.1266919852972,
-3.68654097826476));
#110373=CARTESIAN_POINT('Ctrl Pts',(-18.4017758653499,17.1199895155955,
-3.68894141929202));
#110374=CARTESIAN_POINT('Ctrl Pts',(-18.433181384346,17.1152410370282,-3.69093103096621));
#110375=CARTESIAN_POINT('Ctrl Pts',(-18.6266011995849,17.0904330108766,
-3.70331483793629));
#110376=CARTESIAN_POINT('Ctrl Pts',(-18.7903765906892,17.0884636910055,
-3.71430960285014));
#110377=CARTESIAN_POINT('Ctrl Pts',(-19.06910665696,17.1174199346002,-3.73261520146276));
#110378=CARTESIAN_POINT('Ctrl Pts',(-19.1842754611946,17.1391327721815,
-3.74006744734212));
#110379=CARTESIAN_POINT('Ctrl Pts',(-19.3108534488288,17.1740578436693,
-3.74808511989548));
#110380=CARTESIAN_POINT('Ctrl Pts',(-19.3245916551918,17.1779985828325,
-3.74895323436935));
#110381=CARTESIAN_POINT('Ctrl Pts',(-19.3463925578859,17.1844917111299,
-3.75032772002597));
#110382=CARTESIAN_POINT('Ctrl Pts',(-19.3544815022176,17.1869537558496,
-3.75083702045052));
#110383=CARTESIAN_POINT('Ctrl Pts',(-19.3687212327373,17.1913813114083,
-3.75173244491683));
#110384=CARTESIAN_POINT('Ctrl Pts',(-19.3748781427888,17.1933266126242,
-3.75211922529926));
#110385=CARTESIAN_POINT('Ctrl Pts',(-19.3875938385896,17.1974082653848,
-3.75291728524955));
#110386=CARTESIAN_POINT('Ctrl Pts',(-19.3941512831376,17.1995485676616,
-3.75332842954848));
#110387=CARTESIAN_POINT('Ctrl Pts',(-19.4109557320203,17.2051244460932,
-3.7543810528705));
#110388=CARTESIAN_POINT('Ctrl Pts',(-19.4211871809567,17.2086065357275,
-3.75502099108923));
#110389=CARTESIAN_POINT('Ctrl Pts',(-19.4631586577787,17.2232503584544,
-3.75764265725923));
#110390=CARTESIAN_POINT('Ctrl Pts',(-19.4946581167938,17.2350899816157,
-3.75960185967755));
#110391=CARTESIAN_POINT('Ctrl Pts',(-19.5758765108759,17.2678476240938,
-3.76464255716061));
#110392=CARTESIAN_POINT('Ctrl Pts',(-19.6251029110884,17.2899238879782,
-3.76768639875721));
#110393=CARTESIAN_POINT('Ctrl Pts',(-19.787510999905,17.3703458239725,-3.77777308367551));
#110394=CARTESIAN_POINT('Ctrl Pts',(-19.8962574913671,17.4370070110241,
-3.78458681435731));
#110395=CARTESIAN_POINT('Ctrl Pts',(-20.0802516645691,17.5740147547939,
-3.79713117903374));
#110396=CARTESIAN_POINT('Ctrl Pts',(-20.1576160129603,17.6408324598594,
-3.80279979731956));
#110397=CARTESIAN_POINT('Ctrl Pts',(-20.2367056105132,17.7198062621271,
-3.80942142489032));
#110398=CARTESIAN_POINT('Ctrl Pts',(-20.2435159628775,17.7267006819732,
-3.8099989237236));
#110399=CARTESIAN_POINT('Ctrl Pts',(-20.2535018100779,17.7369495999,-3.81085701749585));
#110400=CARTESIAN_POINT('Ctrl Pts',(-20.256714157878,17.740268234743,-3.81113481182217));
#110401=CARTESIAN_POINT('Ctrl Pts',(-20.2623940492995,17.7461746126948,
-3.81162917255182));
#110402=CARTESIAN_POINT('Ctrl Pts',(-20.2648659241496,17.7487581228484,
-3.81184539723922));
#110403=CARTESIAN_POINT('Ctrl Pts',(-20.2701482858008,17.7543071234984,
-3.81230980404747));
#110404=CARTESIAN_POINT('Ctrl Pts',(-20.2729566942511,17.7572744464699,
-3.81255813260732));
#110405=CARTESIAN_POINT('Ctrl Pts',(-20.2787023604173,17.7633805412943,
-3.81306907659211));
#110406=CARTESIAN_POINT('Ctrl Pts',(-20.2816386810215,17.7665201656755,
-3.8133317601623));
#110407=CARTESIAN_POINT('Ctrl Pts',(-20.2950923997718,17.780993500406,-3.81454245989279));
#110408=CARTESIAN_POINT('Ctrl Pts',(-20.3054946781769,17.7924329363557,
-3.81549868737895));
#110409=CARTESIAN_POINT('Ctrl Pts',(-20.3738026541683,17.8692249566307,
-3.82190713037721));
#110410=CARTESIAN_POINT('Ctrl Pts',(-20.4277374315831,17.9379864932015,
-3.82759173623723));
#110411=CARTESIAN_POINT('Ctrl Pts',(-20.5185485967195,18.0697861553104,
-3.83812738061853));
#110412=CARTESIAN_POINT('Ctrl Pts',(-20.5567134709897,18.131788025879,-3.84295322228073));
#110413=CARTESIAN_POINT('Ctrl Pts',(-20.5938938258958,18.199809306751,-3.84805125631605));
#110414=CARTESIAN_POINT('Ctrl Pts',(-20.5961629620878,18.2039941586156,
-3.84836414488516));
#110415=CARTESIAN_POINT('Ctrl Pts',(-20.6463823918028,18.2973614898272,
-3.85532785540514));
#110416=CARTESIAN_POINT('Ctrl Pts',(-20.6878719037659,18.3898338429119,
-3.86186883282244));
#110417=CARTESIAN_POINT('Ctrl Pts',(-20.7225805460717,18.4848895319684,
-3.86819362763421));
#110418=CARTESIAN_POINT('',(-20.8509991606888,19.2128851108726,-2.8890562790225));
#110419=CARTESIAN_POINT('Ctrl Pts',(-20.7225806137986,18.4848897174502,
-3.64442447432525));
#110420=CARTESIAN_POINT('Ctrl Pts',(-20.697586191156,18.4164380985782,-3.64005128981157));
#110421=CARTESIAN_POINT('Ctrl Pts',(-20.6690382458922,18.3492373239759,
-3.6356781052979));
#110422=CARTESIAN_POINT('Ctrl Pts',(-20.6370917888833,18.2836755459468,
-3.63130492078422));
#110423=CARTESIAN_POINT('Ctrl Pts',(-20.6051516528636,18.2181267401009,
-3.62693260155749));
#110424=CARTESIAN_POINT('Ctrl Pts',(-20.5698145519931,18.1542167202052,
-3.62256028233075));
#110425=CARTESIAN_POINT('Ctrl Pts',(-20.5312826515011,18.0923114505756,
-3.61818796310402));
#110426=CARTESIAN_POINT('Ctrl Pts',(-20.4927456644625,18.030398008911,-3.61381506669306));
#110427=CARTESIAN_POINT('Ctrl Pts',(-20.4510132974867,17.9704902511049,
-3.60944217028209));
#110428=CARTESIAN_POINT('Ctrl Pts',(-20.4063315674442,17.9129259926608,
-3.60506927387112));
#110429=CARTESIAN_POINT('Ctrl Pts',(-20.3616005534068,17.8552982407795,
-3.60069155415084));
#110430=CARTESIAN_POINT('Ctrl Pts',(-20.313913981681,17.8000195274286,-3.59631383443056));
#110431=CARTESIAN_POINT('Ctrl Pts',(-20.2635582109227,17.7473946298954,
-3.59193611471028));
#110432=CARTESIAN_POINT('Ctrl Pts',(-20.2131701327735,17.694735969139,-3.58755558632081));
#110433=CARTESIAN_POINT('Ctrl Pts',(-20.1601097989142,17.6447348427113,
-3.58317505793135));
#110434=CARTESIAN_POINT('Ctrl Pts',(-20.1046985222746,17.5976573330398,
-3.57879452954188));
#110435=CARTESIAN_POINT('Ctrl Pts',(-20.049194460902,17.55050099331,-3.57440666607223));
#110436=CARTESIAN_POINT('Ctrl Pts',(-19.9913319847969,17.5062783305872,
-3.57001880260258));
#110437=CARTESIAN_POINT('Ctrl Pts',(-19.931462691737,17.4652130422363,-3.56563093913294));
#110438=CARTESIAN_POINT('Ctrl Pts',(-19.9100486473828,17.4505248129083,
-3.56406148844868));
#110439=CARTESIAN_POINT('Ctrl Pts',(-19.8883780972448,17.4362400977019,
-3.56249203776441));
#110440=CARTESIAN_POINT('Ctrl Pts',(-19.8664678605235,17.4223676887405,
-3.56092258708015));
#110441=CARTESIAN_POINT('Ctrl Pts',(-19.8052064921928,17.3835802139256,
-3.55653437814987));
#110442=CARTESIAN_POINT('Ctrl Pts',(-19.7418305075797,17.3478680068776,
-3.55214616921958));
#110443=CARTESIAN_POINT('Ctrl Pts',(-19.6766813842658,17.3154681992225,
-3.54775796028929));
#110444=CARTESIAN_POINT('Ctrl Pts',(-19.6116289530529,17.2831164782541,
-3.54337626418865));
#110445=CARTESIAN_POINT('Ctrl Pts',(-19.5448090356316,17.254067610473,-3.538994568088));
#110446=CARTESIAN_POINT('Ctrl Pts',(-19.4765908557835,17.22851473627,-3.53461287198736));
#110447=CARTESIAN_POINT('Ctrl Pts',(-19.4084528377258,17.2029918887278,
-3.53023632472834));
#110448=CARTESIAN_POINT('Ctrl Pts',(-19.3389202706951,17.180957042421,-3.52585977746933));
#110449=CARTESIAN_POINT('Ctrl Pts',(-19.2683841301345,17.1625560536201,
-3.52148323021032));
#110450=CARTESIAN_POINT('Ctrl Pts',(-19.1978927225693,17.144166734459,-3.51710945849398));
#110451=CARTESIAN_POINT('Ctrl Pts',(-19.1263994698853,17.129406821763,-3.51273568677764));
#110452=CARTESIAN_POINT('Ctrl Pts',(-19.0543110010047,17.1183724978785,
-3.50836191506129));
#110453=CARTESIAN_POINT('Ctrl Pts',(-18.9822444688873,17.1073415317758,
-3.50398947429838));
#110454=CARTESIAN_POINT('Ctrl Pts',(-18.9095835567026,17.1000339766643,
-3.49961703353547));
#110455=CARTESIAN_POINT('Ctrl Pts',(-18.8367439345939,17.0964946952291,
-3.49524459277255));
#110456=CARTESIAN_POINT('Ctrl Pts',(-18.7639024499681,17.0929553232941,
-3.49087204020585));
#110457=CARTESIAN_POINT('Ctrl Pts',(-18.6908827282521,17.0931844377534,
-3.48649948763914));
#110458=CARTESIAN_POINT('Ctrl Pts',(-18.6181027067728,17.0971748375463,
-3.48212693507243));
#110459=CARTESIAN_POINT('Ctrl Pts',(-18.5452471514419,17.1011693787266,
-3.47774984450575));
#110460=CARTESIAN_POINT('Ctrl Pts',(-18.4726322757184,17.1089329725838,
-3.47337275393906));
#110461=CARTESIAN_POINT('Ctrl Pts',(-18.4006723159502,17.1204063869212,
-3.46899566337237));
#110462=CARTESIAN_POINT('Ctrl Pts',(-18.3286730561771,17.1318860673159,
-3.46461618231407));
#110463=CARTESIAN_POINT('Ctrl Pts',(-18.257329896609,17.1470795015326,-3.46023670125577));
#110464=CARTESIAN_POINT('Ctrl Pts',(-18.1870456019972,17.1658765595922,
-3.45585722019747));
#110465=CARTESIAN_POINT('Ctrl Pts',(-18.1166367289449,17.1847069353111,
-3.45146997653838));
#110466=CARTESIAN_POINT('Ctrl Pts',(-18.0472909281422,17.2071535415658,
-3.4470827328793));
#110467=CARTESIAN_POINT('Ctrl Pts',(-17.9793940004948,17.23305693067,-3.44269548922021));
#110468=CARTESIAN_POINT('Ctrl Pts',(-17.9332306321323,17.2506687392522,
-3.43971258627972));
#110469=CARTESIAN_POINT('Ctrl Pts',(-17.8877366290248,17.2698774944525,
-3.43672968333922));
#110470=CARTESIAN_POINT('Ctrl Pts',(-17.8430266573744,17.290621000237,-3.43374678039872));
#110471=CARTESIAN_POINT('Ctrl Pts',(-17.7772529124843,17.3211371917539,
-3.42935857146461));
#110472=CARTESIAN_POINT('Ctrl Pts',(-17.7129203794319,17.3550960250395,
-3.4249703625305));
#110473=CARTESIAN_POINT('Ctrl Pts',(-17.6504132837264,17.3923387263387,
-3.42058215359639));
#110474=CARTESIAN_POINT('Ctrl Pts',(-17.5879989589145,17.4295261532943,
-3.4162004574919));
#110475=CARTESIAN_POINT('Ctrl Pts',(-17.5274051041883,17.469987528232,-3.41181876138741));
#110476=CARTESIAN_POINT('Ctrl Pts',(-17.4689939738816,17.5135169356119,
-3.40743706528292));
#110477=CARTESIAN_POINT('Ctrl Pts',(-17.4106514813017,17.556995192474,-3.40306051802006));
#110478=CARTESIAN_POINT('Ctrl Pts',(-17.354487002868,17.6035340332478,-3.3986839707572));
#110479=CARTESIAN_POINT('Ctrl Pts',(-17.3008348082142,17.6528836586912,
-3.39430742349434));
#110480=CARTESIAN_POINT('Ctrl Pts',(-17.2472166390025,17.7022019873193,
-3.38993365177416));
#110481=CARTESIAN_POINT('Ctrl Pts',(-17.1961079465059,17.7543272380327,
-3.38555988005397));
#110482=CARTESIAN_POINT('Ctrl Pts',(-17.14780970538,17.8089695619377,-3.38118610833378));
#110483=CARTESIAN_POINT('Ctrl Pts',(-17.099526161571,17.8635952579999,-3.37681366756702));
#110484=CARTESIAN_POINT('Ctrl Pts',(-17.0540516905114,17.9207361453885,
-3.37244122680026));
#110485=CARTESIAN_POINT('Ctrl Pts',(-17.0116490089847,17.980066994614,-3.3680687860335));
#110486=CARTESIAN_POINT('Ctrl Pts',(-16.9692452432169,18.0393993609357,
-3.36369623346297));
#110487=CARTESIAN_POINT('Ctrl Pts',(-16.92991370178,18.100921406656,-3.35932368089243));
#110488=CARTESIAN_POINT('Ctrl Pts',(-16.8938745512702,18.1642778148253,
-3.3549511283219));
#110489=CARTESIAN_POINT('Ctrl Pts',(-16.857797997971,18.227699976664,-3.35057403775142));
#110490=CARTESIAN_POINT('Ctrl Pts',(-16.82502089682,18.2929598817714,-3.34619694718094));
#110491=CARTESIAN_POINT('Ctrl Pts',(-16.7957176611922,18.3596771616679,
-3.34181985661046));
#110492=CARTESIAN_POINT('Ctrl Pts',(-16.76639842198,18.4264308783469,-3.33744037554839));
#110493=CARTESIAN_POINT('Ctrl Pts',(-16.7405569966208,18.4946431030916,
-3.33306089448631));
#110494=CARTESIAN_POINT('Ctrl Pts',(-16.718318792152,18.5639155632158,-3.32868141342424));
#110495=CARTESIAN_POINT('Ctrl Pts',(-16.6960411706153,18.6333108083096,
-3.32429416976145));
#110496=CARTESIAN_POINT('Ctrl Pts',(-16.6773796475306,18.7037695748786,
-3.31990692609866));
#110497=CARTESIAN_POINT('Ctrl Pts',(-16.6624089793399,18.7748811594065,
-3.31551968243587));
#110498=CARTESIAN_POINT('Ctrl Pts',(-16.6522303676452,18.8232301840919,
-3.31253677952968));
#110499=CARTESIAN_POINT('Ctrl Pts',(-16.6437568500118,18.8718807754355,
-3.30955387662348));
#110500=CARTESIAN_POINT('Ctrl Pts',(-16.6369981960583,18.920702851779,-3.30657097371728));
#110501=CARTESIAN_POINT('Ctrl Pts',(-16.6270554032346,18.9925259978739,
-3.30218276479083));
#110502=CARTESIAN_POINT('Ctrl Pts',(-16.6207874279489,19.0650007495852,
-3.29779455586437));
#110503=CARTESIAN_POINT('Ctrl Pts',(-16.6182687405808,19.1377180928438,
-3.29340634693792));
#110504=CARTESIAN_POINT('Ctrl Pts',(-16.6157537913624,19.2103275115083,
-3.28902465084108));
#110505=CARTESIAN_POINT('Ctrl Pts',(-16.6169771002007,19.2831783288758,
-3.28464295474424));
#110506=CARTESIAN_POINT('Ctrl Pts',(-16.6219616061144,19.3558544882043,
-3.2802612586474));
#110507=CARTESIAN_POINT('Ctrl Pts',(-16.6269402548369,19.4284452472623,
-3.27588471139215));
#110508=CARTESIAN_POINT('Ctrl Pts',(-16.6356712880179,19.5008612771275,
-3.27150816413689));
#110509=CARTESIAN_POINT('Ctrl Pts',(-16.6481255978395,19.5726862983464,
-3.26713161688164));
#110510=CARTESIAN_POINT('Ctrl Pts',(-16.6605720093188,19.6444657691812,
-3.26275784516903));
#110511=CARTESIAN_POINT('Ctrl Pts',(-16.6767369302058,19.7156545009234,
-3.25838407345642));
#110512=CARTESIAN_POINT('Ctrl Pts',(-16.6965395553233,19.7858425318102,
-3.2540103017438));
#110513=CARTESIAN_POINT('Ctrl Pts',(-16.7163361544357,19.8560092042441,
-3.24963786098458));
#110514=CARTESIAN_POINT('Ctrl Pts',(-16.7397681292064,19.9251753164071,
-3.24526542022535));
#110515=CARTESIAN_POINT('Ctrl Pts',(-16.766704216716,19.9929439245068,-3.24089297946613));
#110516=CARTESIAN_POINT('Ctrl Pts',(-16.7936409929846,20.0607142654578,
-3.23652042690307));
#110517=CARTESIAN_POINT('Ctrl Pts',(-16.8240818798544,20.1270865838709,
-3.23214787434001));
#110518=CARTESIAN_POINT('Ctrl Pts',(-16.8578472840037,20.1916834281559,
-3.22777532177696));
#110519=CARTESIAN_POINT('Ctrl Pts',(-16.8916477311638,20.2563473134839,
-3.22339823121383));
#110520=CARTESIAN_POINT('Ctrl Pts',(-16.9287793604432,20.3192316172878,
-3.2190211406507));
#110521=CARTESIAN_POINT('Ctrl Pts',(-16.9690167487975,20.3799837992782,
-3.21464405008757));
#110522=CARTESIAN_POINT('Ctrl Pts',(-17.0092761122835,20.4407691602906,
-3.21026456903279));
#110523=CARTESIAN_POINT('Ctrl Pts',(-17.0526443249069,20.4994196929899,
-3.205885087978));
#110524=CARTESIAN_POINT('Ctrl Pts',(-17.0988543828178,20.555614372454,-3.20150560692321));
#110525=CARTESIAN_POINT('Ctrl Pts',(-17.1451463477475,20.6119086566118,
-3.19711836326753));
#110526=CARTESIAN_POINT('Ctrl Pts',(-17.1942898914314,20.6657380382439,
-3.19273111961185));
#110527=CARTESIAN_POINT('Ctrl Pts',(-17.2459801414521,20.7168173529904,
-3.18834387595617));
#110528=CARTESIAN_POINT('Ctrl Pts',(-17.281124531093,20.7515463655087,-3.18536097298273));
#110529=CARTESIAN_POINT('Ctrl Pts',(-17.3174454256988,20.7850048960141,
-3.18237807000929));
#110530=CARTESIAN_POINT('Ctrl Pts',(-17.3548387352823,20.8171143190639,
-3.17939516703585));
#110531=CARTESIAN_POINT('Ctrl Pts',(-17.4098487897264,20.8643511411001,
-3.17500695810762));
#110532=CARTESIAN_POINT('Ctrl Pts',(-17.4673958504113,20.9088507249,-3.1706187491794));
#110533=CARTESIAN_POINT('Ctrl Pts',(-17.5271763106369,20.9503290611015,
-3.16623054025117));
#110534=CARTESIAN_POINT('Ctrl Pts',(-17.5868680467469,20.9917458365741,
-3.16184884415263));
#110535=CARTESIAN_POINT('Ctrl Pts',(-17.6487862091497,21.0301499931519,
-3.15746714805409));
#110536=CARTESIAN_POINT('Ctrl Pts',(-17.7125933764233,21.0652970391266,
-3.15308545195556));
#110537=CARTESIAN_POINT('Ctrl Pts',(-17.7763255651964,21.1004027845246,
-3.14870890469871));
#110538=CARTESIAN_POINT('Ctrl Pts',(-17.8419419289088,21.1322587908217,
-3.14433235744187));
#110539=CARTESIAN_POINT('Ctrl Pts',(-17.9090766869082,21.1606642089133,
-3.13995581018503));
#110540=CARTESIAN_POINT('Ctrl Pts',(-17.9761688690191,21.1890516127013,
-3.1355820384709));
#110541=CARTESIAN_POINT('Ctrl Pts',(-18.044777091656,21.2139925826767,-3.13120826675677));
#110542=CARTESIAN_POINT('Ctrl Pts',(-18.1145129035447,21.2353331586785,
-3.12683449504263));
#110543=CARTESIAN_POINT('Ctrl Pts',(-18.1842274945909,21.2566672406712,
-3.12246205428196));
#110544=CARTESIAN_POINT('Ctrl Pts',(-18.2550685326861,21.2744029627471,
-3.11808961352129));
#110545=CARTESIAN_POINT('Ctrl Pts',(-18.3266312007897,21.2884358381019,
-3.11371717276062));
#110546=CARTESIAN_POINT('Ctrl Pts',(-18.3981956987582,21.3024690722787,
-3.10934462019619));
#110547=CARTESIAN_POINT('Ctrl Pts',(-18.4704813896227,21.3127991808916,
-3.10497206763176));
#110548=CARTESIAN_POINT('Ctrl Pts',(-18.5430736858703,21.3193728661157,
-3.10059951506733));
#110549=CARTESIAN_POINT('Ctrl Pts',(-18.6157413211406,21.3259533737582,
-3.09622242450294));
#110550=CARTESIAN_POINT('Ctrl Pts',(-18.6887157156752,21.3287696306809,
-3.09184533393856));
#110551=CARTESIAN_POINT('Ctrl Pts',(-18.7615784216629,21.3278203586177,
-3.08746824337417));
#110552=CARTESIAN_POINT('Ctrl Pts',(-18.8344809206782,21.3268705681219,
-3.0830887623182));
#110553=CARTESIAN_POINT('Ctrl Pts',(-18.9072711280009,21.3221511854097,
-3.07870928126222));
#110554=CARTESIAN_POINT('Ctrl Pts',(-18.9795345883547,21.3137129537627,
-3.07432980020625));
#110555=CARTESIAN_POINT('Ctrl Pts',(-19.0519261352069,21.3052597654067,
-3.06994255654949));
#110556=CARTESIAN_POINT('Ctrl Pts',(-19.12378859461,21.2930746456018,-3.06555531289274));
#110557=CARTESIAN_POINT('Ctrl Pts',(-19.1947171668079,21.2772595897439,
-3.06116806923599));
#110558=CARTESIAN_POINT('Ctrl Pts',(-19.2429417616898,21.2665068755957,
-3.05818516627546));
#110559=CARTESIAN_POINT('Ctrl Pts',(-19.2907349020845,21.2540772191552,
-3.05520226331494));
#110560=CARTESIAN_POINT('Ctrl Pts',(-19.3379741345029,21.2400155851672,
-3.05221936035441));
#110561=CARTESIAN_POINT('Ctrl Pts',(-19.4074687259705,21.2193292306409,
-3.04783115140145));
#110562=CARTESIAN_POINT('Ctrl Pts',(-19.476034966597,21.195028040176,-3.04344294244849));
#110563=CARTESIAN_POINT('Ctrl Pts',(-19.5432697129023,21.1672135700835,
-3.03905473349553));
#110564=CARTESIAN_POINT('Ctrl Pts',(-19.610404671698,21.1394403812758,-3.03467303737213));
#110565=CARTESIAN_POINT('Ctrl Pts',(-19.6762116170599,21.1081644467917,
-3.03029134124872));
#110566=CARTESIAN_POINT('Ctrl Pts',(-19.7403023303344,21.0735371459285,
-3.02590964512532));
#110567=CARTESIAN_POINT('Ctrl Pts',(-19.8043177319206,21.0389505348994,
-3.02153309784355));
#110568=CARTESIAN_POINT('Ctrl Pts',(-19.8666204853357,21.0010206087535,
-3.01715655056178));
#110569=CARTESIAN_POINT('Ctrl Pts',(-19.926843718136,20.9599462153261,-3.01278000328));
#110570=CARTESIAN_POINT('Ctrl Pts',(-19.9870287582372,20.9188978706821,
-3.00840623154091));
#110571=CARTESIAN_POINT('Ctrl Pts',(-20.0451364968644,20.874709286591,-3.00403245980182));
#110572=CARTESIAN_POINT('Ctrl Pts',(-20.1008272165774,20.8276237533896,
-2.99965868806273));
#110573=CARTESIAN_POINT('Ctrl Pts',(-20.1565009894169,20.7805525484744,
-2.9952862472771));
#110574=CARTESIAN_POINT('Ctrl Pts',(-20.2097588354092,20.7305864558568,
-2.99091380649147));
#110575=CARTESIAN_POINT('Ctrl Pts',(-20.2602937778995,20.6780093058823,
-2.98654136570585));
#110576=CARTESIAN_POINT('Ctrl Pts',(-20.3108300125729,20.6254308115053,
-2.9821688131165));
#110577=CARTESIAN_POINT('Ctrl Pts',(-20.3586428726808,20.5702414763812,
-2.97779626052716));
#110578=CARTESIAN_POINT('Ctrl Pts',(-20.4034631348275,20.5127610539004,
-2.97342370793782));
#110579=CARTESIAN_POINT('Ctrl Pts',(-20.4483299131299,20.4552209760729,
-2.96904661734876));
#110580=CARTESIAN_POINT('Ctrl Pts',(-20.4901975952178,20.3953854447133,
-2.9646695267597));
#110581=CARTESIAN_POINT('Ctrl Pts',(-20.5288386084058,20.3336056163123,
-2.96029243617064));
#110582=CARTESIAN_POINT('Ctrl Pts',(-20.5675007248842,20.2717920476558,
-2.95591295509008));
#110583=CARTESIAN_POINT('Ctrl Pts',(-20.6029324294579,20.2080324897585,
-2.95153347400953));
#110584=CARTESIAN_POINT('Ctrl Pts',(-20.6349520524139,20.1427029002979,
-2.94715399292897));
#110585=CARTESIAN_POINT('Ctrl Pts',(-20.6670284299332,20.0772575145854,
-2.94276674924806));
#110586=CARTESIAN_POINT('Ctrl Pts',(-20.6956804586539,20.0102369839667,
-2.93837950556715));
#110587=CARTESIAN_POINT('Ctrl Pts',(-20.7207747901306,19.9420368891524,
-2.93399226188624));
#110588=CARTESIAN_POINT('Ctrl Pts',(-20.7378365162411,19.8956673997114,
-2.93100935914849));
#110589=CARTESIAN_POINT('Ctrl Pts',(-20.7532546613793,19.8487529982427,
-2.92802645641074));
#110590=CARTESIAN_POINT('Ctrl Pts',(-20.7670007520344,19.8014209872857,
-2.92504355367298));
#110591=CARTESIAN_POINT('Ctrl Pts',(-20.7921933233445,19.7146752287136,
-2.9195767637458));
#110592=CARTESIAN_POINT('Ctrl Pts',(-20.8118478930297,19.6262535084729,
-2.91410997381861));
#110593=CARTESIAN_POINT('Ctrl Pts',(-20.8257819138181,19.5367873923641,
-2.90864318389142));
#110594=CARTESIAN_POINT('Ctrl Pts',(-20.8394880731092,19.448784305735,-2.90326579177394));
#110595=CARTESIAN_POINT('Ctrl Pts',(-20.8476592207556,19.359770608721,-2.89788839965646));
#110596=CARTESIAN_POINT('Ctrl Pts',(-20.8501673751636,19.2703686810797,
-2.89251100753897));
#110597=CARTESIAN_POINT('Ctrl Pts',(-20.8507044999983,19.2512231310868,
-2.89135943136681));
#110598=CARTESIAN_POINT('Ctrl Pts',(-20.8509820862726,19.2320598582094,
-2.89020785519466));
#110599=CARTESIAN_POINT('Ctrl Pts',(-20.8509991606888,19.2128851108726,
-2.8890562790225));
#110600=CARTESIAN_POINT('Ctrl Pts',(-20.8499621049652,19.2128841874121,
-2.8890562790225));
#110601=CARTESIAN_POINT('Ctrl Pts',(-20.8478499548941,18.9660537307247,
-2.87422526267969));
#110602=CARTESIAN_POINT('Ctrl Pts',(-20.8034780943232,18.7185580611686,
-2.85939424633688));
#110603=CARTESIAN_POINT('Ctrl Pts',(-20.7202231698227,18.4857291668958,
-2.84456322999407));
#110604=CARTESIAN_POINT('Origin',(-18.734,19.211,0.));
#110605=CARTESIAN_POINT('',(-20.7225806143688,18.484889719012,-2.04625075898636));
#110606=CARTESIAN_POINT('',(-20.7225806137756,18.4848897173872,-2.26547387919804));
#110607=CARTESIAN_POINT('',(-20.7225806137986,18.4848897174502,0.));
#110608=CARTESIAN_POINT('',(-20.8509992561162,19.2092252878304,-2.31031848245491));
#110609=CARTESIAN_POINT('Ctrl Pts',(-20.7225806137756,18.4848897173872,
-2.26547387919804));
#110610=CARTESIAN_POINT('Ctrl Pts',(-20.7575267776174,18.5805959284211,
-2.27104577281407));
#110611=CARTESIAN_POINT('Ctrl Pts',(-20.7855141372301,18.6786892936843,
-2.27670321222546));
#110612=CARTESIAN_POINT('Ctrl Pts',(-20.8083091756226,18.7878873309347,
-2.28331207106325));
#110613=CARTESIAN_POINT('Ctrl Pts',(-20.8102239921009,18.7973856707489,
-2.28388948204838));
#110614=CARTESIAN_POINT('Ctrl Pts',(-20.8129550905691,18.8114301543172,
-2.28474746974855));
#110615=CARTESIAN_POINT('Ctrl Pts',(-20.8138218376122,18.81596651655,-2.28502524684811));
#110616=CARTESIAN_POINT('Ctrl Pts',(-20.8153332691877,18.8240198873561,
-2.28551958855298));
#110617=CARTESIAN_POINT('Ctrl Pts',(-20.8159838950629,18.8275357311319,
-2.28573581153983));
#110618=CARTESIAN_POINT('Ctrl Pts',(-20.8173589186186,18.835072732932,-2.28620022787933));
#110619=CARTESIAN_POINT('Ctrl Pts',(-20.8180805722734,18.8390942840813,
-2.28644856773996));
#110620=CARTESIAN_POINT('Ctrl Pts',(-20.8195376389239,18.8473514906243,
-2.28695953916183));
#110621=CARTESIAN_POINT('Ctrl Pts',(-20.8202718002692,18.8515873452387,
-2.28722223889673));
#110622=CARTESIAN_POINT('Ctrl Pts',(-20.8220971197962,18.8623128553873,
-2.28788882365087));
#110623=CARTESIAN_POINT('Ctrl Pts',(-20.8231709205875,18.8688053645306,
-2.28829363336577));
#110624=CARTESIAN_POINT('Ctrl Pts',(-20.8419517333687,18.9857438180572,
-2.29560693393806));
#110625=CARTESIAN_POINT('Ctrl Pts',(-20.8509055124976,19.09740142457,-2.30293673158685));
#110626=CARTESIAN_POINT('Ctrl Pts',(-20.8509992561162,19.2092252878304,
-2.31031848245491));
#110627=CARTESIAN_POINT('Ctrl Pts',(-20.8509992546752,19.2092235697065,
-2.3103183690376));
#110628=CARTESIAN_POINT('Ctrl Pts',(-20.8510842733415,19.3105416195705,
-2.31700660648527));
#110629=CARTESIAN_POINT('Ctrl Pts',(-20.8438956122245,19.411744162389,-2.32371997042176));
#110630=CARTESIAN_POINT('Ctrl Pts',(-20.816945499949,19.5993334523545,-2.3359902690649));
#110631=CARTESIAN_POINT('Ctrl Pts',(-20.7989633480779,19.68575741357,-2.34157368887109));
#110632=CARTESIAN_POINT('Ctrl Pts',(-20.7702151430968,19.7906013393171,
-2.34824550970317));
#110633=CARTESIAN_POINT('Ctrl Pts',(-20.7645030413533,19.8103056541231,
-2.34949516767977));
#110634=CARTESIAN_POINT('Ctrl Pts',(-20.7559151380913,19.8383967355679,
-2.35127116134167));
#110635=CARTESIAN_POINT('Ctrl Pts',(-20.7532718148567,19.8468528374542,
-2.35180505435446));
#110636=CARTESIAN_POINT('Ctrl Pts',(-20.7485973731832,19.8614834109189,
-2.35272759918289));
#110637=CARTESIAN_POINT('Ctrl Pts',(-20.7465907736203,19.8676655338283,
-2.35311705013428));
#110638=CARTESIAN_POINT('Ctrl Pts',(-20.7426778410658,19.8795344437417,
-2.35386407396392));
#110639=CARTESIAN_POINT('Ctrl Pts',(-20.7407757522852,19.8852225543821,
-2.35422178228765));
#110640=CARTESIAN_POINT('Ctrl Pts',(-20.7357295714573,19.9001023825438,
-2.35515678928988));
#110641=CARTESIAN_POINT('Ctrl Pts',(-20.7325463160518,19.9092807445782,
-2.35573278836707));
#110642=CARTESIAN_POINT('Ctrl Pts',(-20.7212792307712,19.9410591434125,
-2.35772476148054));
#110643=CARTESIAN_POINT('Ctrl Pts',(-20.7128741355498,19.9635438981978,
-2.35913006618206));
#110644=CARTESIAN_POINT('Ctrl Pts',(-20.6487986693639,20.1264517915341,
-2.3692920817944));
#110645=CARTESIAN_POINT('Ctrl Pts',(-20.5786228615951,20.2607043462482,
-2.37751642346493));
#110646=CARTESIAN_POINT('Ctrl Pts',(-20.4575557914712,20.4420692461861,
-2.38935813821247));
#110647=CARTESIAN_POINT('Ctrl Pts',(-20.4177432945758,20.4959840616474,
-2.39299178975612));
#110648=CARTESIAN_POINT('Ctrl Pts',(-20.3413736394659,20.5897492521361,
-2.3996784945855));
#110649=CARTESIAN_POINT('Ctrl Pts',(-20.3057195788503,20.6302590608486,
-2.40270481271704));
#110650=CARTESIAN_POINT('Ctrl Pts',(-20.2493176372455,20.6896080313168,
-2.40743005519066));
#110651=CARTESIAN_POINT('Ctrl Pts',(-20.2296773230086,20.7094720308871,
-2.40906500584354));
#110652=CARTESIAN_POINT('Ctrl Pts',(-20.2047675557869,20.7336878144113,
-2.41113482568634));
#110653=CARTESIAN_POINT('Ctrl Pts',(-20.1998614359622,20.7384114151063,
-2.41154231133627));
#110654=CARTESIAN_POINT('Ctrl Pts',(-20.1919761568931,20.7459303615268,
-2.41219712197122));
#110655=CARTESIAN_POINT('Ctrl Pts',(-20.189011503163,20.7487409449644,-2.41244328774043));
#110656=CARTESIAN_POINT('Ctrl Pts',(-20.1834366926422,20.7539954827986,
-2.41290617899004));
#110657=CARTESIAN_POINT('Ctrl Pts',(-20.1808284727663,20.7564414112569,
-2.41312274826207));
#110658=CARTESIAN_POINT('Ctrl Pts',(-20.17483648468,20.7620320963126,-2.41362027704958));
#110659=CARTESIAN_POINT('Ctrl Pts',(-20.1714486213068,20.7651723841151,
-2.41390157141762));
#110660=CARTESIAN_POINT('Ctrl Pts',(-20.1609189967142,20.7748686527225,
-2.41477574451773));
#110661=CARTESIAN_POINT('Ctrl Pts',(-20.153742577207,20.7813865741958,-2.4153713888015));
#110662=CARTESIAN_POINT('Ctrl Pts',(-20.0721339819135,20.8544902726283,
-2.42214070564147));
#110663=CARTESIAN_POINT('Ctrl Pts',(-19.993132486254,20.9157707986147,-2.42864913286996));
#110664=CARTESIAN_POINT('Ctrl Pts',(-19.7683137215159,21.065984540022,-2.44646383483442));
#110665=CARTESIAN_POINT('Ctrl Pts',(-19.6155580137379,21.1432644447314,
-2.45778783330393));
#110666=CARTESIAN_POINT('Ctrl Pts',(-19.4275334683066,21.2113910572846,
-2.47032159553595));
#110667=CARTESIAN_POINT('Ctrl Pts',(-19.3996902815741,21.2208282605146,
-2.47214593254641));
#110668=CARTESIAN_POINT('Ctrl Pts',(-19.3513347991858,21.2361027161312,
-2.47526061096035));
#110669=CARTESIAN_POINT('Ctrl Pts',(-19.3309147912726,21.2422154118328,
-2.47655968214315));
#110670=CARTESIAN_POINT('Ctrl Pts',(-19.3017486516981,21.2504684128913,
-2.47839278320209));
#110671=CARTESIAN_POINT('Ctrl Pts',(-19.2930763246305,21.2528627784035,
-2.47893505333509));
#110672=CARTESIAN_POINT('Ctrl Pts',(-19.2780892874396,21.2568979469085,
-2.47986744792713));
#110673=CARTESIAN_POINT('Ctrl Pts',(-19.2717818225323,21.258564962267,-2.48025841872149));
#110674=CARTESIAN_POINT('Ctrl Pts',(-19.2596903612465,21.2617009178522,
-2.48100519921622));
#110675=CARTESIAN_POINT('Ctrl Pts',(-19.2539076720035,21.2631746085804,
-2.48136115945331));
#110676=CARTESIAN_POINT('Ctrl Pts',(-19.23885498646,21.2669430048263,-2.48228471066503));
#110677=CARTESIAN_POINT('Ctrl Pts',(-19.2295754908998,21.2691994883416,
-2.48285106439092));
#110678=CARTESIAN_POINT('Ctrl Pts',(-19.1978835578883,21.2766792174888,
-2.48477539785402));
#110679=CARTESIAN_POINT('Ctrl Pts',(-19.1754008740866,21.2815998923722,
-2.48612366778171));
#110680=CARTESIAN_POINT('Ctrl Pts',(-18.9811155913145,21.3208137639462,
-2.49764070408457));
#110681=CARTESIAN_POINT('Ctrl Pts',(-18.8057534490266,21.3340257628163,
-2.50706151055773));
#110682=CARTESIAN_POINT('Ctrl Pts',(-18.5436506241012,21.3212277460492,
-2.52133910042804));
#110683=CARTESIAN_POINT('Ctrl Pts',(-18.4569002396963,21.3115969010905,
-2.5261126611607));
#110684=CARTESIAN_POINT('Ctrl Pts',(-18.3336850957124,21.2901516186535,
-2.53325294949115));
#110685=CARTESIAN_POINT('Ctrl Pts',(-18.2965551366273,21.2826575650292,
-2.53545288700559));
#110686=CARTESIAN_POINT('Ctrl Pts',(-18.2522667891114,21.2724750759142,
-2.53815665528862));
#110687=CARTESIAN_POINT('Ctrl Pts',(-18.2448940388325,21.2707382673315,
-2.53860943002565));
#110688=CARTESIAN_POINT('Ctrl Pts',(-18.2334646416941,21.2679810042325,
-2.53931571147065));
#110689=CARTESIAN_POINT('Ctrl Pts',(-18.2294013452952,21.2669880091243,
-2.53956766525062));
#110690=CARTESIAN_POINT('Ctrl Pts',(-18.2218817238485,21.2651267174715,
-2.54003557824757));
#110691=CARTESIAN_POINT('Ctrl Pts',(-18.2184246383238,21.26426173345,-2.54025134535867));
#110692=CARTESIAN_POINT('Ctrl Pts',(-18.2106271651465,21.2622898234599,
-2.54073946802716));
#110693=CARTESIAN_POINT('Ctrl Pts',(-18.2062881220939,21.2611778550058,
-2.54101211035463));
#110694=CARTESIAN_POINT('Ctrl Pts',(-18.1935300219413,21.2578651462738,
-2.54181669139144));
#110695=CARTESIAN_POINT('Ctrl Pts',(-18.1851210863471,21.2556262877114,
-2.5423507562694));
#110696=CARTESIAN_POINT('Ctrl Pts',(-18.1255706058161,21.2393772875416,
-2.546158444936));
#110697=CARTESIAN_POINT('Ctrl Pts',(-18.0749617936444,21.2235030114371,
-2.54952798919886));
#110698=CARTESIAN_POINT('Ctrl Pts',(-18.0111276306136,21.2008144417576,
-2.5539054423609));
#110699=CARTESIAN_POINT('Ctrl Pts',(-17.9973002836321,21.1957366294717,
-2.55486148011119));
#110700=CARTESIAN_POINT('Ctrl Pts',(-17.8512118666701,21.1403516647053,
-2.56503816308134));
#110701=CARTESIAN_POINT('Ctrl Pts',(-17.7242571773421,21.0770481513458,
-2.57451403715176));
#110702=CARTESIAN_POINT('Ctrl Pts',(-17.5184240315459,20.947213134106,-2.59030455015483));
#110703=CARTESIAN_POINT('Ctrl Pts',(-17.436309447735,20.8867283503483,-2.59674775968453));
#110704=CARTESIAN_POINT('Ctrl Pts',(-17.3476241084051,20.8109591311117,
-2.60386081414444));
#110705=CARTESIAN_POINT('Ctrl Pts',(-17.3364903823184,20.8012434467342,
-2.60475701407788));
#110706=CARTESIAN_POINT('Ctrl Pts',(-17.3196643931974,20.7862472953726,
-2.60611660249239));
#110707=CARTESIAN_POINT('Ctrl Pts',(-17.3138981102644,20.7810509149454,
-2.60658348410878));
#110708=CARTESIAN_POINT('Ctrl Pts',(-17.3034585791741,20.7715385949314,
-2.60743053660901));
#110709=CARTESIAN_POINT('Ctrl Pts',(-17.2987759757018,20.7672331009249,
-2.60781114198737));
#110710=CARTESIAN_POINT('Ctrl Pts',(-17.2887079573,20.7578918097761,-2.6086309565558));
#110711=CARTESIAN_POINT('Ctrl Pts',(-17.2833292879657,20.7528488405803,
-2.6090698525835));
#110712=CARTESIAN_POINT('Ctrl Pts',(-17.2688147117739,20.7390969786577,
-2.61025683612894));
#110713=CARTESIAN_POINT('Ctrl Pts',(-17.2597300738474,20.7303342292723,
-2.61100259169567));
#110714=CARTESIAN_POINT('Ctrl Pts',(-17.2159005711963,20.687294411445,-2.61461529195019));
#110715=CARTESIAN_POINT('Ctrl Pts',(-17.1822681823724,20.6519024848284,
-2.61743270890948));
#110716=CARTESIAN_POINT('Ctrl Pts',(-17.1228450128653,20.5848742069277,
-2.62252290474575));
#110717=CARTESIAN_POINT('Ctrl Pts',(-17.0966885348781,20.5535953000447,
-2.62480790441187));
#110718=CARTESIAN_POINT('Ctrl Pts',(-16.9982908584207,20.4287718803747,
-2.63362798769001));
#110719=CARTESIAN_POINT('Ctrl Pts',(-16.9330313665142,20.3300026580496,
-2.63996611823286));
#110720=CARTESIAN_POINT('Ctrl Pts',(-16.8405335120332,20.1607642243681,
-2.65050122314283));
#110721=CARTESIAN_POINT('Ctrl Pts',(-16.8082092125215,20.0933806145278,
-2.65462412557213));
#110722=CARTESIAN_POINT('Ctrl Pts',(-16.7662502876465,19.992563733114,-2.66088047095741));
#110723=CARTESIAN_POINT('Ctrl Pts',(-16.7537678437019,19.9603738034231,
-2.66289083546881));
#110724=CARTESIAN_POINT('Ctrl Pts',(-16.7395821471637,19.9209582965944,
-2.66538429801141));
#110725=CARTESIAN_POINT('Ctrl Pts',(-16.7371218198147,19.9140084526406,
-2.66582513861859));
#110726=CARTESIAN_POINT('Ctrl Pts',(-16.7333370748242,19.903137262388,-2.66651677467955));
#110727=CARTESIAN_POINT('Ctrl Pts',(-16.7319877429683,19.8992245652255,
-2.66676611901149));
#110728=CARTESIAN_POINT('Ctrl Pts',(-16.7294965245968,19.8919313832965,
-2.66723170652321));
#110729=CARTESIAN_POINT('Ctrl Pts',(-16.7283517075889,19.8885519597664,
-2.66744777358066));
#110730=CARTESIAN_POINT('Ctrl Pts',(-16.7257699983805,19.8808670482946,
-2.66793985637005));
#110731=CARTESIAN_POINT('Ctrl Pts',(-16.7243384123481,19.8765598425575,
-2.66821617937816));
#110732=CARTESIAN_POINT('Ctrl Pts',(-16.7201155968612,19.8637168315464,
-2.66904158958636));
#110733=CARTESIAN_POINT('Ctrl Pts',(-16.717364860644,19.8551679591185,-2.66959296725551));
#110734=CARTESIAN_POINT('Ctrl Pts',(-16.696514408469,19.7889252941818,-2.67387905300726));
#110735=CARTESIAN_POINT('Ctrl Pts',(-16.6808412807037,19.7305026619888,
-2.67773826526523));
#110736=CARTESIAN_POINT('Ctrl Pts',(-16.6546081667227,19.6127910079383,
-2.68556636106876));
#110737=CARTESIAN_POINT('Ctrl Pts',(-16.6440334074358,19.5535573679836,
-2.6895310614893));
#110738=CARTESIAN_POINT('Ctrl Pts',(-16.6214478066949,19.3860943694899,
-2.70069458271644));
#110739=CARTESIAN_POINT('Ctrl Pts',(-16.6152391521043,19.2772627845727,
-2.70788802040985));
#110740=CARTESIAN_POINT('Ctrl Pts',(-16.618932834134,19.0936120799526,-2.71968874840913));
#110741=CARTESIAN_POINT('Ctrl Pts',(-16.6244037210298,19.0189200440966,
-2.72439646824398));
#110742=CARTESIAN_POINT('Ctrl Pts',(-16.6361827690023,18.9260358429179,
-2.73013199751174));
#110743=CARTESIAN_POINT('Ctrl Pts',(-16.6387933533262,18.9074364170283,
-2.73127465688877));
#110744=CARTESIAN_POINT('Ctrl Pts',(-16.6429520445461,18.8804239284348,
-2.73292609791404));
#110745=CARTESIAN_POINT('Ctrl Pts',(-16.6443041138119,18.8719820097731,
-2.73344105439541));
#110746=CARTESIAN_POINT('Ctrl Pts',(-16.6467656475359,18.8571874221772,
-2.73434156999406));
#110747=CARTESIAN_POINT('Ctrl Pts',(-16.6478530610269,18.8508312440371,
-2.73472782333231));
#110748=CARTESIAN_POINT('Ctrl Pts',(-16.6500219849041,18.8384928358023,
-2.73547640945912));
#110749=CARTESIAN_POINT('Ctrl Pts',(-16.6511002528523,18.8325101067406,
-2.73583884114541));
#110750=CARTESIAN_POINT('Ctrl Pts',(-16.6537412444267,18.818209811902,-2.73670387790195));
#110751=CARTESIAN_POINT('Ctrl Pts',(-16.6553281108973,18.8098967681258,
-2.73720571071442));
#110752=CARTESIAN_POINT('Ctrl Pts',(-16.6612450510339,18.7798784634625,
-2.73901427966966));
#110753=CARTESIAN_POINT('Ctrl Pts',(-16.6658656847988,18.7582314426846,
-2.74031175806969));
#110754=CARTESIAN_POINT('Ctrl Pts',(-16.712353133391,18.5560309379826,-2.75237824688537));
#110755=CARTESIAN_POINT('Ctrl Pts',(-16.7774183885294,18.3816418388984,
-2.76229334120737));
#110756=CARTESIAN_POINT('Ctrl Pts',(-16.9020359879003,18.1470238467712,
-2.77677482499561));
#110757=CARTESIAN_POINT('Ctrl Pts',(-16.9437063932024,18.0783110831566,
-2.78119041845442));
#110758=CARTESIAN_POINT('Ctrl Pts',(-17.0096028490715,17.9824053791749,
-2.78784616610286));
#110759=CARTESIAN_POINT('Ctrl Pts',(-17.0307864442922,17.9532029136862,
-2.78994434140374));
#110760=CARTESIAN_POINT('Ctrl Pts',(-17.0572428022676,17.918626182698,-2.79253527072107));
#110761=CARTESIAN_POINT('Ctrl Pts',(-17.0618127004352,17.9127186687016,
-2.79298179893197));
#110762=CARTESIAN_POINT('Ctrl Pts',(-17.0689763612735,17.9035587633895,
-2.79368041678069));
#110763=CARTESIAN_POINT('Ctrl Pts',(-17.0715486642688,17.9002895589227,
-2.79393100715533));
#110764=CARTESIAN_POINT('Ctrl Pts',(-17.0763437996697,17.894232124939,-2.79439769351204));
#110765=CARTESIAN_POINT('Ctrl Pts',(-17.0785640470679,17.8914419223009,
-2.79461360570287));
#110766=CARTESIAN_POINT('Ctrl Pts',(-17.083608277057,17.8851355654001,-2.79510374466763));
#110767=CARTESIAN_POINT('Ctrl Pts',(-17.0864364378377,17.8816228353622,
-2.79537826870676));
#110768=CARTESIAN_POINT('Ctrl Pts',(-17.0937670488373,17.8725771400632,
-2.79608904794247));
#110769=CARTESIAN_POINT('Ctrl Pts',(-17.0982862375867,17.8670578992284,
-2.79652646891331));
#110770=CARTESIAN_POINT('Ctrl Pts',(-17.1261971632411,17.8333198793415,
-2.79922281403875));
#110771=CARTESIAN_POINT('Ctrl Pts',(-17.1502891175498,17.8056915127307,
-2.8015278937844));
#110772=CARTESIAN_POINT('Ctrl Pts',(-17.2905032389765,17.6530819535127,
-2.81475349719218));
#110773=CARTESIAN_POINT('Ctrl Pts',(-17.4206816316658,17.5418716299619,
-2.82626472652731));
#110774=CARTESIAN_POINT('Ctrl Pts',(-17.6422116312476,17.3947469555842,
-2.84354642740194));
#110775=CARTESIAN_POINT('Ctrl Pts',(-17.7251041819546,17.347425360615,-2.84960310779911));
#110776=CARTESIAN_POINT('Ctrl Pts',(-17.8301604086857,17.2965234873061,
-2.85677377162878));
#110777=CARTESIAN_POINT('Ctrl Pts',(-17.8495462573935,17.287490718936,-2.85807727258134));
#110778=CARTESIAN_POINT('Ctrl Pts',(-17.8772887319129,17.275072325732,-2.85991548089011));
#110779=CARTESIAN_POINT('Ctrl Pts',(-17.8855347495824,17.2714441540344,
-2.86045849109549));
#110780=CARTESIAN_POINT('Ctrl Pts',(-17.8997939338557,17.265278583708,-2.86139175846869));
#110781=CARTESIAN_POINT('Ctrl Pts',(-17.9057960871884,17.2627161729118,
-2.86178286616702));
#110782=CARTESIAN_POINT('Ctrl Pts',(-17.9173067341061,17.2578649074406,
-2.86252963660411));
#110783=CARTESIAN_POINT('Ctrl Pts',(-17.9228132311356,17.2555715028454,
-2.86288545118564));
#110784=CARTESIAN_POINT('Ctrl Pts',(-17.937147622393,17.2496723324459,-2.86380803801545));
#110785=CARTESIAN_POINT('Ctrl Pts',(-17.9459903797506,17.2461028591481,
-2.86437357822826));
#110786=CARTESIAN_POINT('Ctrl Pts',(-17.9761758811916,17.2341547088343,
-2.86629213933818));
#110787=CARTESIAN_POINT('Ctrl Pts',(-17.997630959482,17.226062873325,-2.86763553056476));
#110788=CARTESIAN_POINT('Ctrl Pts',(-18.1851804446528,17.1587877317944,
-2.87921439783776));
#110789=CARTESIAN_POINT('Ctrl Pts',(-18.3579315083373,17.120220899497,-2.88869057347339));
#110790=CARTESIAN_POINT('Ctrl Pts',(-18.6195061113945,17.0953327563968,
-2.90298930981596));
#110791=CARTESIAN_POINT('Ctrl Pts',(-18.7059476050395,17.0924232517146,
-2.90772198839001));
#110792=CARTESIAN_POINT('Ctrl Pts',(-18.8299768237063,17.0958411945691,
-2.91480714904523));
#110793=CARTESIAN_POINT('Ctrl Pts',(-18.8675994300068,17.0978840258145,
-2.91699576751067));
#110794=CARTESIAN_POINT('Ctrl Pts',(-18.9126832038257,17.1015407057472,
-2.91968698980269));
#110795=CARTESIAN_POINT('Ctrl Pts',(-18.9202181521132,17.1021925177128,
-2.92013908719328));
#110796=CARTESIAN_POINT('Ctrl Pts',(-18.9319121858262,17.1032672744012,
-2.92084453786562));
#110797=CARTESIAN_POINT('Ctrl Pts',(-18.9360738713595,17.1036621946923,
-2.92109634407894));
#110798=CARTESIAN_POINT('Ctrl Pts',(-18.9437813106418,17.104416627949,-2.92156412314885));
#110799=CARTESIAN_POINT('Ctrl Pts',(-18.9473273364876,17.1047727689968,
-2.92177990479591));
#110800=CARTESIAN_POINT('Ctrl Pts',(-18.9553313930585,17.1055970676607,
-2.92226824039758));
#110801=CARTESIAN_POINT('Ctrl Pts',(-18.9597888206167,17.1060704285688,
-2.92254108223638));
#110802=CARTESIAN_POINT('Ctrl Pts',(-18.9729099210101,17.1075059935572,
-2.92334678585299));
#110803=CARTESIAN_POINT('Ctrl Pts',(-18.9815690702414,17.1085075422358,
-2.923881782501));
#110804=CARTESIAN_POINT('Ctrl Pts',(-19.0431294769498,17.1160134075918,
-2.92770739209667));
#110805=CARTESIAN_POINT('Ctrl Pts',(-19.0957702381481,17.1244595338442,
-2.93109490621968));
#110806=CARTESIAN_POINT('Ctrl Pts',(-19.1656348808281,17.1383923317878,
-2.93569896422243));
#110807=CARTESIAN_POINT('Ctrl Pts',(-19.183192927769,17.1421266581325,-2.93686531945922));
#110808=CARTESIAN_POINT('Ctrl Pts',(-19.24774156537,17.156715585646,-2.94118294851364));
#110809=CARTESIAN_POINT('Ctrl Pts',(-19.2944039419844,17.1689515089548,
-2.94436226767155));
#110810=CARTESIAN_POINT('Ctrl Pts',(-19.4453996142591,17.2141115457453,
-2.95477317648947));
#110811=CARTESIAN_POINT('Ctrl Pts',(-19.5476143332185,17.2535301809381,
-2.96200574809195));
#110812=CARTESIAN_POINT('Ctrl Pts',(-19.714619340497,17.3332881506789,-2.97390173133479));
#110813=CARTESIAN_POINT('Ctrl Pts',(-19.7811165193729,17.3695426221303,
-2.97866453071452));
#110814=CARTESIAN_POINT('Ctrl Pts',(-19.8616162957819,17.4192055102461,
-2.98445948256182));
#110815=CARTESIAN_POINT('Ctrl Pts',(-19.8775637363913,17.4293412164024,
-2.98560917885865));
#110816=CARTESIAN_POINT('Ctrl Pts',(-19.9005445937735,17.4443828482994,
-2.98726884991084));
#110817=CARTESIAN_POINT('Ctrl Pts',(-19.9076869402443,17.4491199190584,
-2.98778508636765));
#110818=CARTESIAN_POINT('Ctrl Pts',(-19.9201552702724,17.4574988454538,
-2.98868707888915));
#110819=CARTESIAN_POINT('Ctrl Pts',(-19.9254937013597,17.4611218941769,
-2.98907353619654));
#110820=CARTESIAN_POINT('Ctrl Pts',(-19.9358248196863,17.4682025411038,
-2.98982196596707));
#110821=CARTESIAN_POINT('Ctrl Pts',(-19.9408193501042,17.4716573260724,
-2.99018403992115));
#110822=CARTESIAN_POINT('Ctrl Pts',(-19.9527191944609,17.4799645432514,
-2.99104734627265));
#110823=CARTESIAN_POINT('Ctrl Pts',(-19.9596105273439,17.4848368947673,
-2.99154781349463));
#110824=CARTESIAN_POINT('Ctrl Pts',(-19.984347160739,17.5025491562118,-2.99334630862947));
#110825=CARTESIAN_POINT('Ctrl Pts',(-20.0020217238731,17.5156259205698,
-2.99463521496988));
#110826=CARTESIAN_POINT('Ctrl Pts',(-20.16790647912,17.6424036452805,-3.00677958094477));
#110827=CARTESIAN_POINT('Ctrl Pts',(-20.3006546993801,17.7749703104854,
-3.01676512932791));
#110828=CARTESIAN_POINT('Ctrl Pts',(-20.4625579748485,17.9862256044517,
-3.03127850219662));
#110829=CARTESIAN_POINT('Ctrl Pts',(-20.5072417077249,18.0518637374812,
-3.03564442815817));
#110830=CARTESIAN_POINT('Ctrl Pts',(-20.5665927235223,18.1505398963798,
-3.0422326101284));
#110831=CARTESIAN_POINT('Ctrl Pts',(-20.5842696290703,18.1816926219035,
-3.04431618330247));
#110832=CARTESIAN_POINT('Ctrl Pts',(-20.6046593321897,18.2198500553934,
-3.04689091169714));
#110833=CARTESIAN_POINT('Ctrl Pts',(-20.6081371493158,18.2264419815935,
-3.0473365138029));
#110834=CARTESIAN_POINT('Ctrl Pts',(-20.6135001086041,18.2367384242285,
-3.04803399505739));
#110835=CARTESIAN_POINT('Ctrl Pts',(-20.6154093111171,18.2404304354519,
-3.04828438282849));
#110836=CARTESIAN_POINT('Ctrl Pts',(-20.6189363568608,18.2473005404384,
-3.04875088902753));
#110837=CARTESIAN_POINT('Ctrl Pts',(-20.6205570469706,18.2504771081894,
-3.04896682490641));
#110838=CARTESIAN_POINT('Ctrl Pts',(-20.6242112018844,18.2576842116327,
-3.04945727315536));
#110839=CARTESIAN_POINT('Ctrl Pts',(-20.6262397950634,18.2617171458489,
-3.04973208439025));
#110840=CARTESIAN_POINT('Ctrl Pts',(-20.6322139852811,18.2736893438273,
-3.05054890868033));
#110841=CARTESIAN_POINT('Ctrl Pts',(-20.6361225689186,18.2816468235407,
-3.05109314375318));
#110842=CARTESIAN_POINT('Ctrl Pts',(-20.6648569174112,18.3410876886567,
-3.05516698365295));
#110843=CARTESIAN_POINT('Ctrl Pts',(-20.6876363765022,18.39352857509,-3.05880793160253));
#110844=CARTESIAN_POINT('Ctrl Pts',(-20.7131595094723,18.459467874377,-3.06338857213167));
#110845=CARTESIAN_POINT('Ctrl Pts',(-20.7179317366394,18.4721579512576,
-3.06427026063966));
#110846=CARTESIAN_POINT('Ctrl Pts',(-20.7225805974208,18.4848896725968,
-3.06515445288237));
#110847=CARTESIAN_POINT('',(-20.8479141186681,19.210171541465,-2.08900434294145));
#110848=CARTESIAN_POINT('Ctrl Pts',(-20.7202231698227,18.4857291668958,
-2.84456322999407));
#110849=CARTESIAN_POINT('Ctrl Pts',(-20.6328470740777,18.2413750955877,
-2.82899806899323));
#110850=CARTESIAN_POINT('Ctrl Pts',(-20.1480309870729,17.3916716763849,
-2.77104097243191));
#110851=CARTESIAN_POINT('Ctrl Pts',(-18.3741968228298,16.7337288824509,
-2.6706919403101));
#110852=CARTESIAN_POINT('Ctrl Pts',(-16.4562523864159,18.1726376448454,
-2.54351613362869));
#110853=CARTESIAN_POINT('Ctrl Pts',(-16.6280000106062,20.564179464316,-2.41634032694724));
#110854=CARTESIAN_POINT('Ctrl Pts',(-18.731871915622,21.7142630277803,-2.28916452026582));
#110855=CARTESIAN_POINT('Ctrl Pts',(-20.5383022256027,20.7307617397078,
-2.18006983762423));
#110856=CARTESIAN_POINT('Ctrl Pts',(-20.8463944855641,19.6158003448226,
-2.11336709054312));
#110857=CARTESIAN_POINT('Ctrl Pts',(-20.8478239987731,19.2101685861784,
-2.0890562790225));
#110858=CARTESIAN_POINT('Ctrl Pts',(-20.8509998750783,19.2102727321581,
-2.08722602201616));
#110859=CARTESIAN_POINT('Ctrl Pts',(-20.850932996752,19.0155969878683,-2.07601666321716));
#110860=CARTESIAN_POINT('Ctrl Pts',(-20.8240164305583,18.8218628606765,
-2.06573534679094));
#110861=CARTESIAN_POINT('Ctrl Pts',(-20.7567162189418,18.584055871884,-2.05215244185046));
#110862=CARTESIAN_POINT('Ctrl Pts',(-20.7405653205142,18.5341439975041,
-2.04923747298217));
#110863=CARTESIAN_POINT('Ctrl Pts',(-20.7225806143688,18.484889719012,-2.04625075898636));
#110864=CARTESIAN_POINT('Origin',(-18.734,19.211,0.));
#110865=CARTESIAN_POINT('',(-20.7225806756344,18.4848898867987,-1.24458630806144));
#110866=CARTESIAN_POINT('',(-20.7225806136401,18.4848897170162,-1.46829797183507));
#110867=CARTESIAN_POINT('',(-20.7225806137986,18.4848897174502,0.));
#110868=CARTESIAN_POINT('Ctrl Pts',(-20.7225806136401,18.4848897170162,
-1.46829797183507));
#110869=CARTESIAN_POINT('Ctrl Pts',(-20.772093170878,18.6204885561492,-1.4767475415403));
#110870=CARTESIAN_POINT('Ctrl Pts',(-20.8076106590459,18.7608045197434,
-1.48469153836204));
#110871=CARTESIAN_POINT('Ctrl Pts',(-20.8435716232105,19.0058873147326,
-1.49816093193042));
#110872=CARTESIAN_POINT('Ctrl Pts',(-20.8510665768484,19.1090662014719,
-1.5037241301894));
#110873=CARTESIAN_POINT('Ctrl Pts',(-20.8509605930383,19.2724280292508,
-1.5128625274986));
#110874=CARTESIAN_POINT('Ctrl Pts',(-20.848366219973,19.3324481090795,-1.51629225644068));
#110875=CARTESIAN_POINT('Ctrl Pts',(-20.8424571662823,19.4012045864611,
-1.52038549800654));
#110876=CARTESIAN_POINT('Ctrl Pts',(-20.84163261838,19.4101334885926,-1.52092026133344));
#110877=CARTESIAN_POINT('Ctrl Pts',(-20.8403055953013,19.423570727867,-1.52173022272583));
#110878=CARTESIAN_POINT('Ctrl Pts',(-20.8398453012565,19.4280832592346,
-1.52200310844775));
#110879=CARTESIAN_POINT('Ctrl Pts',(-20.8389970518347,19.4361424913529,
-1.52249210538345));
#110880=CARTESIAN_POINT('Ctrl Pts',(-20.8386146299038,19.4396897220715,
-1.52270790270283));
#110881=CARTESIAN_POINT('Ctrl Pts',(-20.837768977974,19.4473519291442,-1.5231752774535));
#110882=CARTESIAN_POINT('Ctrl Pts',(-20.8373026477048,19.4514664603963,
-1.52342702188824));
#110883=CARTESIAN_POINT('Ctrl Pts',(-20.8359714187376,19.4629119818602,
-1.52412939672326));
#110884=CARTESIAN_POINT('Ctrl Pts',(-20.8350802526499,19.4702397732347,
-1.5245814667027));
#110885=CARTESIAN_POINT('Ctrl Pts',(-20.8297855229006,19.5119550389898,
-1.5271680133266));
#110886=CARTESIAN_POINT('Ctrl Pts',(-20.8245763666059,19.5462327957154,
-1.52934381699349));
#110887=CARTESIAN_POINT('Ctrl Pts',(-20.8054071890936,19.6544149896487,
-1.53633891098771));
#110888=CARTESIAN_POINT('Ctrl Pts',(-20.7883503424776,19.7277085403984,
-1.54126752850267));
#110889=CARTESIAN_POINT('Ctrl Pts',(-20.7136651524747,19.9855767263582,
-1.55897626805703));
#110890=CARTESIAN_POINT('Ctrl Pts',(-20.6347144920359,20.1630288020327,
-1.57174491669585));
#110891=CARTESIAN_POINT('Ctrl Pts',(-20.52155967755,20.3453590042295,-1.58493000273531));
#110892=CARTESIAN_POINT('Ctrl Pts',(-20.5100907630276,20.3632333115886,
-1.58622485581085));
#110893=CARTESIAN_POINT('Ctrl Pts',(-20.4937578174105,20.3878647368295,
-1.58801298157456));
#110894=CARTESIAN_POINT('Ctrl Pts',(-20.4891202632915,20.3947698463815,
-1.58851468253942));
#110895=CARTESIAN_POINT('Ctrl Pts',(-20.4810444645849,20.4066425607041,
-1.58937810281685));
#110896=CARTESIAN_POINT('Ctrl Pts',(-20.4776254564377,20.4116230728427,
-1.58974054362169));
#110897=CARTESIAN_POINT('Ctrl Pts',(-20.4705005819946,20.4219073417681,
-1.59048948289309));
#110898=CARTESIAN_POINT('Ctrl Pts',(-20.4667916223787,20.4272088868545,
-1.59087585834058));
#110899=CARTESIAN_POINT('Ctrl Pts',(-20.4580472064134,20.4395868545563,
-1.5917787065444));
#110900=CARTESIAN_POINT('Ctrl Pts',(-20.4529923688728,20.4466494924997,
-1.59229442933029));
#110901=CARTESIAN_POINT('Ctrl Pts',(-20.4364321481621,20.4694891976478,
-1.59396426284884));
#110902=CARTESIAN_POINT('Ctrl Pts',(-20.4247517069832,20.4851385257338,
-1.59511159306344));
#110903=CARTESIAN_POINT('Ctrl Pts',(-20.3638544262758,20.5644156951665,
-1.6009440405323));
#110904=CARTESIAN_POINT('Ctrl Pts',(-20.3112538404237,20.6253662372658,
-1.60549253391176));
#110905=CARTESIAN_POINT('Ctrl Pts',(-20.1384830030225,20.8039024264036,
-1.61926738115335));
#110906=CARTESIAN_POINT('Ctrl Pts',(-20.0077164891844,20.9102791333806,
-1.62810924859928));
#110907=CARTESIAN_POINT('Ctrl Pts',(-19.8645527343082,21.0008440070415,
-1.63762177446481));
#110908=CARTESIAN_POINT('Ctrl Pts',(-19.8633406036649,21.001609073889,-1.63770230688805));
#110909=CARTESIAN_POINT('Ctrl Pts',(-19.8165544504403,21.0310729309989,
-1.64081045970006));
#110910=CARTESIAN_POINT('Ctrl Pts',(-19.7699065971989,21.0580208684212,
-1.64389973656495));
#110911=CARTESIAN_POINT('Ctrl Pts',(-19.7145584032438,21.087238414556,-1.64761367364294));
#110912=CARTESIAN_POINT('Ctrl Pts',(-19.7068050584584,21.0912701089764,
-1.64813501313869));
#110913=CARTESIAN_POINT('Ctrl Pts',(-19.6950331591432,21.0972991287085,
-1.64892852740314));
#110914=CARTESIAN_POINT('Ctrl Pts',(-19.6910327410687,21.0993319272865,
-1.649198526796));
#110915=CARTESIAN_POINT('Ctrl Pts',(-19.683843252723,21.1029565268024,-1.64968443062165));
#110916=CARTESIAN_POINT('Ctrl Pts',(-19.6806566008649,21.1045530052785,
-1.6499000375978));
#110917=CARTESIAN_POINT('Ctrl Pts',(-19.6737268085872,21.108002891657,-1.65036942735312));
#110918=CARTESIAN_POINT('Ctrl Pts',(-19.6699822597049,21.1098532472402,
-1.65062339025646));
#110919=CARTESIAN_POINT('Ctrl Pts',(-19.6594568308272,21.1150156524095,
-1.65133810705894));
#110920=CARTESIAN_POINT('Ctrl Pts',(-19.6526637603123,21.1183025040342,
-1.6518003822164));
#110921=CARTESIAN_POINT('Ctrl Pts',(-19.6121136771161,21.1376559227571,
-1.65456514608512));
#110922=CARTESIAN_POINT('Ctrl Pts',(-19.577955653816,21.1528612546117,-1.65691576629389));
#110923=CARTESIAN_POINT('Ctrl Pts',(-19.4646081386315,21.1997621018972,
-1.66474457719752));
#110924=CARTESIAN_POINT('Ctrl Pts',(-19.3839070776935,21.2275767701418,
-1.67036055457777));
#110925=CARTESIAN_POINT('Ctrl Pts',(-19.1303549397287,21.2981622714081,
-1.68774770695599));
#110926=CARTESIAN_POINT('Ctrl Pts',(-18.9535869921731,21.3240900494598,
-1.69943901710199));
#110927=CARTESIAN_POINT('Ctrl Pts',(-18.7528396253182,21.3280389508183,
-1.71179546537254));
#110928=CARTESIAN_POINT('Ctrl Pts',(-18.7300373791083,21.3281190831423,
-1.71318717086491));
#110929=CARTESIAN_POINT('Ctrl Pts',(-18.6977235695387,21.3277105496945,
-1.71514332857322));
#110930=CARTESIAN_POINT('Ctrl Pts',(-18.6882103733659,21.3275261267726,
-1.71571725069181));
#110931=CARTESIAN_POINT('Ctrl Pts',(-18.6727395335275,21.3271218514576,
-1.71664746726135));
#110932=CARTESIAN_POINT('Ctrl Pts',(-18.666781083937,21.3269409617051,-1.71700497755867));
#110933=CARTESIAN_POINT('Ctrl Pts',(-18.6542978150237,21.3265092049677,
-1.71775243060923));
#110934=CARTESIAN_POINT('Ctrl Pts',(-18.6477732235398,21.3262533132198,
-1.71814221190239));
#110935=CARTESIAN_POINT('Ctrl Pts',(-18.6322313311064,21.3255717363993,
-1.71906862383351));
#110936=CARTESIAN_POINT('Ctrl Pts',(-18.6232153165642,21.3251185511004,
-1.7196043871257));
#110937=CARTESIAN_POINT('Ctrl Pts',(-18.5927419619009,21.3233913451983,
-1.72140982004915));
#110938=CARTESIAN_POINT('Ctrl Pts',(-18.5713007730654,21.321848180288,-1.72267105502257));
#110939=CARTESIAN_POINT('Ctrl Pts',(-18.37109355362,21.3043700943778,-1.73437218530679));
#110940=CARTESIAN_POINT('Ctrl Pts',(-18.1950140076912,21.2660913668851,
-1.74401510710511));
#110941=CARTESIAN_POINT('Ctrl Pts',(-17.9123263109276,21.1657520524479,
-1.76034028089886));
#110942=CARTESIAN_POINT('Ctrl Pts',(-17.8024542251927,21.1158404754064,
-1.76694993789784));
#110943=CARTESIAN_POINT('Ctrl Pts',(-17.6891590166171,21.0522187560071,
-1.77465079425141));
#110944=CARTESIAN_POINT('Ctrl Pts',(-17.680910115097,21.0475132383796,-1.77521686369375));
#110945=CARTESIAN_POINT('Ctrl Pts',(-17.6687297401433,21.0404560003738,
-1.77606114966729));
#110946=CARTESIAN_POINT('Ctrl Pts',(-17.664773660047,21.0381466872926,-1.7763366940007));
#110947=CARTESIAN_POINT('Ctrl Pts',(-17.6577462647211,21.0340138933654,
-1.77682858204549));
#110948=CARTESIAN_POINT('Ctrl Pts',(-17.6546720386063,21.0321954616757,
-1.7770445967854));
#110949=CARTESIAN_POINT('Ctrl Pts',(-17.6480700897573,21.0282677632469,
-1.77751029947401));
#110950=CARTESIAN_POINT('Ctrl Pts',(-17.6445439550583,21.0261560315225,
-1.77776014303231));
#110951=CARTESIAN_POINT('Ctrl Pts',(-17.6348221353206,21.0202952947674,
-1.77845200097139));
#110952=CARTESIAN_POINT('Ctrl Pts',(-17.6286395709653,21.0165247880609,
-1.77889538694874));
#110953=CARTESIAN_POINT('Ctrl Pts',(-17.5947837336046,20.9956383573915,
-1.78134158865437));
#110954=CARTESIAN_POINT('Ctrl Pts',(-17.5674901691052,20.9779188757617,
-1.78338075026793));
#110955=CARTESIAN_POINT('Ctrl Pts',(-17.4062312191767,20.8678617196679,
-1.79578677801862));
#110956=CARTESIAN_POINT('Ctrl Pts',(-17.2828694487212,20.760961530764,-1.80674351524227));
#110957=CARTESIAN_POINT('Ctrl Pts',(-17.0940656621517,20.5548559903665,
-1.82500098322813));
#110958=CARTESIAN_POINT('Ctrl Pts',(-17.0224172982632,20.4623296992898,
-1.8324417104591));
#110959=CARTESIAN_POINT('Ctrl Pts',(-16.9509757770334,20.3523666389927,
-1.84044866088052));
#110960=CARTESIAN_POINT('Ctrl Pts',(-16.9433122852977,20.3403054097198,
-1.84131663452484));
#110961=CARTESIAN_POINT('Ctrl Pts',(-16.9313098083461,20.3209858338611,
-1.84269093951051));
#110962=CARTESIAN_POINT('Ctrl Pts',(-16.9268912772551,20.3137776502433,
-1.84320019890914));
#110963=CARTESIAN_POINT('Ctrl Pts',(-16.9191746638351,20.3010182054698,
-1.84409557502407));
#110964=CARTESIAN_POINT('Ctrl Pts',(-16.9158585973788,20.2954779991077,
-1.84448234786525));
#110965=CARTESIAN_POINT('Ctrl Pts',(-16.9090523326695,20.2839876954241,
-1.84528041501967));
#110966=CARTESIAN_POINT('Ctrl Pts',(-16.9055657621033,20.2780355300763,
-1.84569157395204));
#110967=CARTESIAN_POINT('Ctrl Pts',(-16.8966908943633,20.262713400558,-1.8467442818472));
#110968=CARTESIAN_POINT('Ctrl Pts',(-16.8913451090216,20.2533189463313,
-1.84738428951001));
#110969=CARTESIAN_POINT('Ctrl Pts',(-16.8693339854494,20.2139389280165,
-1.8500449507682));
#110970=CARTESIAN_POINT('Ctrl Pts',(-16.853326234936,20.1835904714479,-1.85204207564392));
#110971=CARTESIAN_POINT('Ctrl Pts',(-16.8135459453665,20.1035143011146,
-1.85718614484259));
#110972=CARTESIAN_POINT('Ctrl Pts',(-16.790964549502,20.0532229141713,-1.86029370021906));
#110973=CARTESIAN_POINT('Ctrl Pts',(-16.7295083369658,19.9006802098619,
-1.86943810277065));
#110974=CARTESIAN_POINT('Ctrl Pts',(-16.6965650202614,19.7962394433127,
-1.87532622032092));
#110975=CARTESIAN_POINT('Ctrl Pts',(-16.6614979198788,19.6451828366451,
-1.88376907075576));
#110976=CARTESIAN_POINT('Ctrl Pts',(-16.6526043735314,19.6003219961865,
-1.88626911846589));
#110977=CARTESIAN_POINT('Ctrl Pts',(-16.6414625464269,19.5327080713401,
-1.89006889938615));
#110978=CARTESIAN_POINT('Ctrl Pts',(-16.6381185040672,19.5101484261164,
-1.89134199193598));
#110979=CARTESIAN_POINT('Ctrl Pts',(-16.6349997254098,19.4864777571354,
-1.89268722023571));
#110980=CARTESIAN_POINT('Ctrl Pts',(-16.6348606066572,19.4854156604791,
-1.89274760014244));
#110981=CARTESIAN_POINT('Ctrl Pts',(-16.6322661713896,19.4654911271904,
-1.89388068451132));
#110982=CARTESIAN_POINT('Ctrl Pts',(-16.6300644480917,19.4465970583556,
-1.89496155260961));
#110983=CARTESIAN_POINT('Ctrl Pts',(-16.6247547778914,19.3949922707455,
-1.89793716880863));
#110984=CARTESIAN_POINT('Ctrl Pts',(-16.6221534413677,19.3622362653008,
-1.89985157408718));
#110985=CARTESIAN_POINT('Ctrl Pts',(-16.6199303411559,19.3225610941034,
-1.90221548195122));
#110986=CARTESIAN_POINT('Ctrl Pts',(-16.6195787148595,19.3156853674982,
-1.90262678473982));
#110987=CARTESIAN_POINT('Ctrl Pts',(-16.6190558028044,19.3043793296246,
-1.90330597445504));
#110988=CARTESIAN_POINT('Ctrl Pts',(-16.618864881926,19.2999499180403,-1.90357278659488));
#110989=CARTESIAN_POINT('Ctrl Pts',(-16.6185457019116,19.2919616848831,
-1.9040553258584));
#110990=CARTESIAN_POINT('Ctrl Pts',(-16.6184125073555,19.2884031158922,
-1.90427077371997));
#110991=CARTESIAN_POINT('Ctrl Pts',(-16.6181411073559,19.2806272278032,
-1.9047426280809));
#110992=CARTESIAN_POINT('Ctrl Pts',(-16.6180065331723,19.276409877377,-1.904999230178));
#110993=CARTESIAN_POINT('Ctrl Pts',(-16.6176607291121,19.2644514682656,
-1.90572872268441));
#110994=CARTESIAN_POINT('Ctrl Pts',(-16.6174793676046,19.2567097074783,
-1.90620323481775));
#110995=CARTESIAN_POINT('Ctrl Pts',(-16.6166052469029,19.20797783466,-1.90920352792312));
#110996=CARTESIAN_POINT('Ctrl Pts',(-16.6170608681158,19.1669787141585,
-1.91178725615409));
#110997=CARTESIAN_POINT('Ctrl Pts',(-16.6260552817034,18.943087572951,-1.92613099367957));
#110998=CARTESIAN_POINT('Ctrl Pts',(-16.6571021423828,18.7618768183812,
-1.93851336704575));
#110999=CARTESIAN_POINT('Ctrl Pts',(-16.7370944515095,18.5025908417339,
-1.95601438523293));
#111000=CARTESIAN_POINT('Ctrl Pts',(-16.7683562975834,18.4199730547995,
-1.96157153686915));
#111001=CARTESIAN_POINT('Ctrl Pts',(-16.8103162345117,18.3270788052049,
-1.96779041290174));
#111002=CARTESIAN_POINT('Ctrl Pts',(-16.8160647347727,18.3146740323007,
-1.96862036383626));
#111003=CARTESIAN_POINT('Ctrl Pts',(-16.8254845392132,18.2948525254036,
-1.9699459384234));
#111004=CARTESIAN_POINT('Ctrl Pts',(-16.8290797910932,18.2874002706771,
-1.97044417575424));
#111005=CARTESIAN_POINT('Ctrl Pts',(-16.8355458639991,18.2741957411976,
-1.97132681299776));
#111006=CARTESIAN_POINT('Ctrl Pts',(-16.8383993534999,18.2684351395203,
-1.97171181019933));
#111007=CARTESIAN_POINT('Ctrl Pts',(-16.8444044030833,18.2564497613088,
-1.97251273631025));
#111008=CARTESIAN_POINT('Ctrl Pts',(-16.8475605890665,18.2502273792721,
-1.97292849744536));
#111009=CARTESIAN_POINT('Ctrl Pts',(-16.8558480976322,18.2340869402244,
-1.97400688831941));
#111010=CARTESIAN_POINT('Ctrl Pts',(-16.8610272763885,18.2241935962108,
-1.97466782663415));
#111011=CARTESIAN_POINT('Ctrl Pts',(-16.8839668193809,18.1812054106382,
-1.97753995334988));
#111012=CARTESIAN_POINT('Ctrl Pts',(-16.9025284906629,18.1485443389106,
-1.97972257113581));
#111013=CARTESIAN_POINT('Ctrl Pts',(-16.9542722721378,18.0628859284714,
-1.98546413999428));
#111014=CARTESIAN_POINT('Ctrl Pts',(-16.9889498675745,18.0108343342411,
-1.98897057598798));
#111015=CARTESIAN_POINT('Ctrl Pts',(-17.0946125412111,17.8665172824652,
-1.998860473838));
#111016=CARTESIAN_POINT('Ctrl Pts',(-17.1709627413942,17.778470936924,-2.00509548245638));
#111017=CARTESIAN_POINT('Ctrl Pts',(-17.3255285815601,17.6273782381556,
-2.01692457769316));
#111018=CARTESIAN_POINT('Ctrl Pts',(-17.4017323359465,17.5627563211379,
-2.02247378546111));
#111019=CARTESIAN_POINT('Ctrl Pts',(-17.4900147963413,17.4980248685897,
-2.02895931383772));
#111020=CARTESIAN_POINT('Ctrl Pts',(-17.4978721726306,17.4923461738664,
-2.02953703118549));
#111021=CARTESIAN_POINT('Ctrl Pts',(-17.5095306305389,17.484041661526,-2.03039538901899));
#111022=CARTESIAN_POINT('Ctrl Pts',(-17.5133018765579,17.4813739045473,
-2.03067322641621));
#111023=CARTESIAN_POINT('Ctrl Pts',(-17.5200076965833,17.4766631027844,
-2.03116763491802));
#111024=CARTESIAN_POINT('Ctrl Pts',(-17.5229387469449,17.4746151270706,
-2.03138386406435));
#111025=CARTESIAN_POINT('Ctrl Pts',(-17.5292296625561,17.4702432327415,
-2.03184824767471));
#111026=CARTESIAN_POINT('Ctrl Pts',(-17.5325910193304,17.4679216456925,
-2.03209654840715));
#111027=CARTESIAN_POINT('Ctrl Pts',(-17.541836086478,17.4615758043646,-2.03277989674342));
#111028=CARTESIAN_POINT('Ctrl Pts',(-17.5477333727836,17.4575715586888,
-2.03321626197525));
#111029=CARTESIAN_POINT('Ctrl Pts',(-17.5793230731723,17.4363545204237,
-2.03555571816893));
#111030=CARTESIAN_POINT('Ctrl Pts',(-17.6053686935918,17.4196774370775,
-2.03749158792104));
#111031=CARTESIAN_POINT('Ctrl Pts',(-17.6853024591858,17.3709309344064,
-2.04343173718327));
#111032=CARTESIAN_POINT('Ctrl Pts',(-17.7402568165067,17.340680753308,-2.04751346858103));
#111033=CARTESIAN_POINT('Ctrl Pts',(-17.9272150449388,17.2483353736808,
-2.06121640637012));
#111034=CARTESIAN_POINT('Ctrl Pts',(-18.0643009772396,17.1974296987275,
-2.07093960091191));
#111035=CARTESIAN_POINT('Ctrl Pts',(-18.2780045266389,17.1423391488082,
-2.08506738200193));
#111036=CARTESIAN_POINT('Ctrl Pts',(-18.3514180325007,17.1275118696366,
-2.08975426356528));
#111037=CARTESIAN_POINT('Ctrl Pts',(-18.438452373882,17.1146906740026,-2.09511762195096));
#111038=CARTESIAN_POINT('Ctrl Pts',(-18.451452095435,17.112898981609,-2.09591379190503));
#111039=CARTESIAN_POINT('Ctrl Pts',(-18.4726000748713,17.1101843723045,
-2.09720120544719));
#111040=CARTESIAN_POINT('Ctrl Pts',(-18.4807383632071,17.1091877418027,
-2.09769476491574));
#111041=CARTESIAN_POINT('Ctrl Pts',(-18.495239242451,17.1074973828996,-2.0985709262653));
#111042=CARTESIAN_POINT('Ctrl Pts',(-18.5015995392823,17.1067851852185,
-2.09895410615008));
#111043=CARTESIAN_POINT('Ctrl Pts',(-18.5150065447146,17.1053454580934,
-2.09975950511818));
#111044=CARTESIAN_POINT('Ctrl Pts',(-18.5220538836354,17.1046244330745,
-2.10018151485112));
#111045=CARTESIAN_POINT('Ctrl Pts',(-18.5407000552306,17.1028112387086,
-2.1012946051871));
#111046=CARTESIAN_POINT('Ctrl Pts',(-18.5523046151238,17.1017794052805,
-2.10198378334474));
#111047=CARTESIAN_POINT('Ctrl Pts',(-18.6062150455316,17.0974341198738,
-2.105169574526));
#111048=CARTESIAN_POINT('Ctrl Pts',(-18.6486076683341,17.0952972237828,
-2.10762913198384));
#111049=CARTESIAN_POINT('Ctrl Pts',(-18.7655036106586,17.0929244791949,
-2.11431062805601));
#111050=CARTESIAN_POINT('Ctrl Pts',(-18.8400009351297,17.0953437149919,
-2.1184545985267));
#111051=CARTESIAN_POINT('Ctrl Pts',(-19.0801363246528,17.1158609224158,
-2.13168202061258));
#111052=CARTESIAN_POINT('Ctrl Pts',(-19.2437801056489,17.1495610455256,
-2.14046030295509));
#111053=CARTESIAN_POINT('Ctrl Pts',(-19.4349847888982,17.2131174368166,
-2.15199060397981));
#111054=CARTESIAN_POINT('Ctrl Pts',(-19.4679224323766,17.2249808776535,
-2.15402679701654));
#111055=CARTESIAN_POINT('Ctrl Pts',(-19.5071002780485,17.2401995633245,
-2.15652622605923));
#111056=CARTESIAN_POINT('Ctrl Pts',(-19.5136391089855,17.2427771320967,
-2.15694601087442));
#111057=CARTESIAN_POINT('Ctrl Pts',(-19.5243224062948,17.2470500148479,
-2.15763636305506));
#111058=CARTESIAN_POINT('Ctrl Pts',(-19.5284746031473,17.2487260246904,
-2.15790579442479));
#111059=CARTESIAN_POINT('Ctrl Pts',(-19.535921727548,17.2517595241352,-2.15839109267274));
#111060=CARTESIAN_POINT('Ctrl Pts',(-19.5392185696694,17.2531121701846,
-2.15860666532094));
#111061=CARTESIAN_POINT('Ctrl Pts',(-19.5463789673075,17.2560711214286,
-2.15907646932416));
#111062=CARTESIAN_POINT('Ctrl Pts',(-19.5502411304838,17.257680537392,-2.15933088347273));
#111063=CARTESIAN_POINT('Ctrl Pts',(-19.5609462500667,17.2621787995516,
-2.1600388273396));
#111064=CARTESIAN_POINT('Ctrl Pts',(-19.5677787346432,17.2650921939319,
-2.16049380715666));
#111065=CARTESIAN_POINT('Ctrl Pts',(-19.607532075362,17.2822909572066,-2.16315874751795));
#111066=CARTESIAN_POINT('Ctrl Pts',(-19.6400986699825,17.2973747219567,
-2.16541301610423));
#111067=CARTESIAN_POINT('Ctrl Pts',(-19.7438174942051,17.3486549461156,
-2.17278807546737));
#111068=CARTESIAN_POINT('Ctrl Pts',(-19.8133083911187,17.3880485025383,
-2.17803105458147));
#111069=CARTESIAN_POINT('Ctrl Pts',(-19.9532651082704,17.4782008180299,
-2.18902178704521));
#111070=CARTESIAN_POINT('Ctrl Pts',(-20.0231781449331,17.5295657222382,
-2.19476299579208));
#111071=CARTESIAN_POINT('Ctrl Pts',(-20.1737010323259,17.6550762826311,
-2.20752739975055));
#111072=CARTESIAN_POINT('Ctrl Pts',(-20.2521166851698,17.7314845843767,
-2.21446963224926));
#111073=CARTESIAN_POINT('Ctrl Pts',(-20.3336379992466,17.824259982578,-2.22200948829987));
#111074=CARTESIAN_POINT('Ctrl Pts',(-20.3428801360305,17.834993340225,-2.2228697172755));
#111075=CARTESIAN_POINT('Ctrl Pts',(-20.3574425044958,17.8522526736318,
-2.22423411278676));
#111076=CARTESIAN_POINT('Ctrl Pts',(-20.3628326070596,17.8587188888056,
-2.224741142035));
#111077=CARTESIAN_POINT('Ctrl Pts',(-20.3722848375392,17.8701967319361,
-2.22563392778639));
#111078=CARTESIAN_POINT('Ctrl Pts',(-20.3763628695648,17.8751950671355,
-2.22602032845939));
#111079=CARTESIAN_POINT('Ctrl Pts',(-20.3847637490828,17.8855884277285,
-2.22681890836706));
#111080=CARTESIAN_POINT('Ctrl Pts',(-20.3890831490421,17.8909861505662,
-2.22723094589812));
#111081=CARTESIAN_POINT('Ctrl Pts',(-20.4001304916741,17.9049308984128,
-2.22828856940508));
#111082=CARTESIAN_POINT('Ctrl Pts',(-20.4068191954625,17.9135088596134,
-2.2289325857393));
#111083=CARTESIAN_POINT('Ctrl Pts',(-20.4346932866237,17.9498299801156,
-2.23163248749914));
#111084=CARTESIAN_POINT('Ctrl Pts',(-20.4552576598895,17.9780443036075,
-2.2336639492588));
#111085=CARTESIAN_POINT('Ctrl Pts',(-20.5324401683793,18.089636002645,-2.24146597766943));
#111086=CARTESIAN_POINT('Ctrl Pts',(-20.5837764500916,18.1765077105203,
-2.24704183883486));
#111087=CARTESIAN_POINT('Ctrl Pts',(-20.6636064468633,18.3366885048602,
-2.25681069373311));
#111088=CARTESIAN_POINT('Ctrl Pts',(-20.6945765374082,18.4085405953949,
-2.26102810748162));
#111089=CARTESIAN_POINT('Ctrl Pts',(-20.7218617307922,18.4829231940916,
-2.26535938548301));
#111090=CARTESIAN_POINT('Ctrl Pts',(-20.7222215396299,18.4839063297364,
-2.26541662762247));
#111091=CARTESIAN_POINT('Ctrl Pts',(-20.7225806137756,18.4848897173872,
-2.26547387919804));
#111092=CARTESIAN_POINT('Ctrl Pts',(-20.7225806143688,18.484889719012,-2.04625075898636));
#111093=CARTESIAN_POINT('Ctrl Pts',(-20.7190678452871,18.4752693835319,
-2.0456673946269));
#111094=CARTESIAN_POINT('Ctrl Pts',(-20.7154851171429,18.4656741356815,
-2.04508128329489));
#111095=CARTESIAN_POINT('Ctrl Pts',(-20.7008063082509,18.4272155179506,
-2.04271348048677));
#111096=CARTESIAN_POINT('Ctrl Pts',(-20.6891489412846,18.3985730439432,
-2.04090771294304));
#111097=CARTESIAN_POINT('Ctrl Pts',(-20.6740381885879,18.3636561288022,
-2.03864182751629));
#111098=CARTESIAN_POINT('Ctrl Pts',(-20.6711741840977,18.3571288232929,
-2.03821543231835));
#111099=CARTESIAN_POINT('Ctrl Pts',(-20.6666170559015,18.3468836863867,
-2.03754154370128));
#111100=CARTESIAN_POINT('Ctrl Pts',(-20.6649460109763,18.3431560104146,
-2.03729538221779));
#111101=CARTESIAN_POINT('Ctrl Pts',(-20.6617920753989,18.3361745888825,
-2.03683249527082));
#111102=CARTESIAN_POINT('Ctrl Pts',(-20.6603117270573,18.3329197557002,
-2.03661592599276));
#111103=CARTESIAN_POINT('Ctrl Pts',(-20.6568999795337,18.3254685161816,
-2.03611839220421));
#111104=CARTESIAN_POINT('Ctrl Pts',(-20.6549630915615,18.3212746828098,
-2.03583709280961));
#111105=CARTESIAN_POINT('Ctrl Pts',(-20.6489187114161,18.3082988735045,
-2.03496288620491));
#111106=CARTESIAN_POINT('Ctrl Pts',(-20.6447646742806,18.2995388947276,
-2.03436721312599));
#111107=CARTESIAN_POINT('Ctrl Pts',(-20.5974955275657,18.2016017030713,
-2.02764827948139));
#111108=CARTESIAN_POINT('Ctrl Pts',(-20.5482373920097,18.115537297651,-2.021195611675));
#111109=CARTESIAN_POINT('Ctrl Pts',(-20.399449731234,17.8933013163034,-2.0035776289607));
#111110=CARTESIAN_POINT('Ctrl Pts',(-20.2893723145285,17.765010224037,-1.99238949452662));
#111111=CARTESIAN_POINT('Ctrl Pts',(-20.1423767404648,17.6301373120347,
-1.9798625993034));
#111112=CARTESIAN_POINT('Ctrl Pts',(-20.1190530915225,17.6096630672868,
-1.97793392486713));
#111113=CARTESIAN_POINT('Ctrl Pts',(-20.0836920553102,17.5799728486222,
-1.97509534439942));
#111114=CARTESIAN_POINT('Ctrl Pts',(-20.0719930233165,17.5703620445284,
-1.97416961807476));
#111115=CARTESIAN_POINT('Ctrl Pts',(-20.0530918684216,17.5551713226938,
-1.9726950683028));
#111116=CARTESIAN_POINT('Ctrl Pts',(-20.04595524529,17.5495110881048,-1.9721430324799));
#111117=CARTESIAN_POINT('Ctrl Pts',(-20.0322741886686,17.5388034115547,
-1.97109364827273));
#111118=CARTESIAN_POINT('Ctrl Pts',(-20.0257363115092,17.5337479009031,
-1.97059598362392));
#111119=CARTESIAN_POINT('Ctrl Pts',(-20.0142087486863,17.52494142388,-1.96972510511618));
#111120=CARTESIAN_POINT('Ctrl Pts',(-20.0092317974269,17.5211740248042,
-1.96935124475302));
#111121=CARTESIAN_POINT('Ctrl Pts',(-19.9993762615517,17.513782025418,-1.96861508121863));
#111122=CARTESIAN_POINT('Ctrl Pts',(-19.9944985893209,17.5101563140465,
-1.96825273668805));
#111123=CARTESIAN_POINT('Ctrl Pts',(-19.9827961448665,17.5015355474121,
-1.96738812041314));
#111124=CARTESIAN_POINT('Ctrl Pts',(-19.9759568870928,17.496560260653,-1.96688661920639));
#111125=CARTESIAN_POINT('Ctrl Pts',(-19.9511416912045,17.4787346163345,
-1.96508050613971));
#111126=CARTESIAN_POINT('Ctrl Pts',(-19.9329942545738,17.4661246211756,
-1.96378511870904));
#111127=CARTESIAN_POINT('Ctrl Pts',(-19.7605673997803,17.3502719999949,
-1.95170323482904));
#111128=CARTESIAN_POINT('Ctrl Pts',(-19.5935406163916,17.2674606365657,
-1.94177388522409));
#111129=CARTESIAN_POINT('Ctrl Pts',(-19.3420213280998,17.1816115205769,
-1.92728568526151));
#111130=CARTESIAN_POINT('Ctrl Pts',(-19.2647982366149,17.1600590543207,
-1.92287977218364));
#111131=CARTESIAN_POINT('Ctrl Pts',(-19.1513562354283,17.1352349761077,
-1.91623718674218));
#111132=CARTESIAN_POINT('Ctrl Pts',(-19.1159773718957,17.1284343706335,
-1.91414184751537));
#111133=CARTESIAN_POINT('Ctrl Pts',(-19.0730795303477,17.1213182513299,
-1.91155406408531));
#111134=CARTESIAN_POINT('Ctrl Pts',(-19.0657080621816,17.1201354667644,
-1.91110771450358));
#111135=CARTESIAN_POINT('Ctrl Pts',(-19.0542204789755,17.1183545106463,
-1.91040931555447));
#111136=CARTESIAN_POINT('Ctrl Pts',(-19.0501085126652,17.117729423413,-1.91015876392219));
#111137=CARTESIAN_POINT('Ctrl Pts',(-19.0424677606854,17.1165909290181,
-1.90969211006112));
#111138=CARTESIAN_POINT('Ctrl Pts',(-19.0389395103124,17.1160743186361,
-1.90947619137495));
#111139=CARTESIAN_POINT('Ctrl Pts',(-19.0309451845286,17.114924403995,-1.90898598685904));
#111140=CARTESIAN_POINT('Ctrl Pts',(-19.0264784026677,17.114296461136,-1.90871140344036));
#111141=CARTESIAN_POINT('Ctrl Pts',(-19.0149395420422,17.1127119112403,
-1.90800037643951));
#111142=CARTESIAN_POINT('Ctrl Pts',(-19.007864638088,17.1117767897605,-1.90756276579224));
#111143=CARTESIAN_POINT('Ctrl Pts',(-18.9643760245005,17.1062522925866,
-1.90486323660953));
#111144=CARTESIAN_POINT('Ctrl Pts',(-18.9278551237891,17.1025750331161,
-1.9025550410228));
#111145=CARTESIAN_POINT('Ctrl Pts',(-18.7213642553807,17.0871935138433,
-1.88934038092808));
#111146=CARTESIAN_POINT('Ctrl Pts',(-18.5505639565763,17.0950916986026,
-1.87784520490375));
#111147=CARTESIAN_POINT('Ctrl Pts',(-18.2884010190126,17.1392262784515,
-1.86056765255793));
#111148=CARTESIAN_POINT('Ctrl Pts',(-18.1954197599543,17.1614292173261,
-1.85450128655694));
#111149=CARTESIAN_POINT('Ctrl Pts',(-18.0838103250555,17.1962046114691,
-1.84732045803713));
#111150=CARTESIAN_POINT('Ctrl Pts',(-18.0634738039575,17.2028810432982,
-1.84601587830353));
#111151=CARTESIAN_POINT('Ctrl Pts',(-18.034722933616,17.2128053660157,-1.84417642340332));
#111152=CARTESIAN_POINT('Ctrl Pts',(-18.026223205722,17.2158002044253,-1.84363323020972));
#111153=CARTESIAN_POINT('Ctrl Pts',(-18.0116009287435,17.2210574932488,
-1.84269974419708));
#111154=CARTESIAN_POINT('Ctrl Pts',(-18.0054692935604,17.2232941340372,
-1.84230859983062));
#111155=CARTESIAN_POINT('Ctrl Pts',(-17.9937543168371,17.2276289045175,
-1.84156182444511));
#111156=CARTESIAN_POINT('Ctrl Pts',(-17.9881693159729,17.2297223400741,
-1.84120604126877));
#111157=CARTESIAN_POINT('Ctrl Pts',(-17.9736813109815,17.2352228463991,
-1.8402836761945));
#111158=CARTESIAN_POINT('Ctrl Pts',(-17.9647922757975,17.2386665213237,
-1.8397183250998));
#111159=CARTESIAN_POINT('Ctrl Pts',(-17.9346218912784,17.2505897309601,
-1.8378011256372));
#111160=CARTESIAN_POINT('Ctrl Pts',(-17.9134545780258,17.259354782647,-1.836458887937));
#111161=CARTESIAN_POINT('Ctrl Pts',(-17.7304096863751,17.3386554305616,
-1.82486619276819));
#111162=CARTESIAN_POINT('Ctrl Pts',(-17.5778061498537,17.428841159686,-1.81537759335669));
#111163=CARTESIAN_POINT('Ctrl Pts',(-17.3699643020394,17.5897248764056,
-1.80107399983594));
#111164=CARTESIAN_POINT('Ctrl Pts',(-17.3050623933915,17.6466274812604,
-1.79635040402545));
#111165=CARTESIAN_POINT('Ctrl Pts',(-17.2170891575077,17.7338113009417,
-1.78927749720031));
#111166=CARTESIAN_POINT('Ctrl Pts',(-17.1910744509895,17.7610050643575,
-1.78709140170358));
#111167=CARTESIAN_POINT('Ctrl Pts',(-17.1607210687907,17.7944762382524,
-1.78440297493004));
#111168=CARTESIAN_POINT('Ctrl Pts',(-17.155672242358,17.8001039554484,-1.78395102770745));
#111169=CARTESIAN_POINT('Ctrl Pts',(-17.1478792023388,17.8088847099593,
-1.78324576055274));
#111170=CARTESIAN_POINT('Ctrl Pts',(-17.1451139405222,17.8120190992573,
-1.78299398637949));
#111171=CARTESIAN_POINT('Ctrl Pts',(-17.1400081157992,17.8178411522909,
-1.7825262378712));
#111172=CARTESIAN_POINT('Ctrl Pts',(-17.1376650504122,17.8205265446659,
-1.78231045455948));
#111173=CARTESIAN_POINT('Ctrl Pts',(-17.132389860561,17.826603358792,-1.78182207696554));
#111174=CARTESIAN_POINT('Ctrl Pts',(-17.1294617383689,17.8299981661678,
-1.78154919457091));
#111175=CARTESIAN_POINT('Ctrl Pts',(-17.120869946294,17.8400235334818,-1.7807432512955));
#111176=CARTESIAN_POINT('Ctrl Pts',(-17.1152365164015,17.8466797223251,
-1.78020805361927));
#111177=CARTESIAN_POINT('Ctrl Pts',(-17.075428506715,17.8943085894367,-1.77637885816132));
#111178=CARTESIAN_POINT('Ctrl Pts',(-17.0427753817604,17.9365220978506,
-1.77298776242021));
#111179=CARTESIAN_POINT('Ctrl Pts',(-17.0014688792481,17.9943086844479,
-1.76839701273352));
#111180=CARTESIAN_POINT('Ctrl Pts',(-16.9913642515662,18.0088259421183,
-1.76724780278229));
#111181=CARTESIAN_POINT('Ctrl Pts',(-16.9542796703162,18.0635552758287,
-1.76293490378192));
#111182=CARTESIAN_POINT('Ctrl Pts',(-16.9285005056758,18.1045619374357,
-1.75974265646073));
#111183=CARTESIAN_POINT('Ctrl Pts',(-16.8491452090389,18.2409608759958,
-1.74931858448016));
#111184=CARTESIAN_POINT('Ctrl Pts',(-16.8015456967016,18.3396347972161,
-1.74208581379438));
#111185=CARTESIAN_POINT('Ctrl Pts',(-16.741756468379,18.4928838200185,-1.73151221537489));
#111186=CARTESIAN_POINT('Ctrl Pts',(-16.7237398247873,18.5449819925373,
-1.7280230083582));
#111187=CARTESIAN_POINT('Ctrl Pts',(-16.697838083891,18.630560181972,-1.72246534820155));
#111188=CARTESIAN_POINT('Ctrl Pts',(-16.6886997835665,18.6636308631711,
-1.72035845383858));
#111189=CARTESIAN_POINT('Ctrl Pts',(-16.6777441101147,18.7073954565616,
-1.71762190105163));
#111190=CARTESIAN_POINT('Ctrl Pts',(-16.6751997173642,18.7179003915396,
-1.71696890022378));
#111191=CARTESIAN_POINT('Ctrl Pts',(-16.6711634515564,18.7351408236112,
-1.71590340947858));
#111192=CARTESIAN_POINT('Ctrl Pts',(-16.669623873787,18.7418648461031,-1.71548939009587));
#111193=CARTESIAN_POINT('Ctrl Pts',(-16.6667068922995,18.7548970567613,
-1.71468988721327));
#111194=CARTESIAN_POINT('Ctrl Pts',(-16.6653254310474,18.7612042494961,
-1.71430427736103));
#111195=CARTESIAN_POINT('Ctrl Pts',(-16.6622017480666,18.7757845583152,
-1.71341587634844));
#111196=CARTESIAN_POINT('Ctrl Pts',(-16.6604801797879,18.7840620235377,
-1.71291375121927));
#111197=CARTESIAN_POINT('Ctrl Pts',(-16.6559824231989,18.8063567809199,
-1.71156718170263));
#111198=CARTESIAN_POINT('Ctrl Pts',(-16.6532984614739,18.8203923877775,
-1.71072567854518));
#111199=CARTESIAN_POINT('Ctrl Pts',(-16.6299799312036,18.9494024324239,
-1.70304537508105));
#111200=CARTESIAN_POINT('Ctrl Pts',(-16.6187508089804,19.0658798497603,
-1.69652311331571));
#111201=CARTESIAN_POINT('Ctrl Pts',(-16.6150144979993,19.3453779252748,
-1.68122065926736));
#111202=CARTESIAN_POINT('Ctrl Pts',(-16.6315990743005,19.5077414717001,
-1.67262337881141));
#111203=CARTESIAN_POINT('Ctrl Pts',(-16.6736115328653,19.6983901181167,
-1.66141475394752));
#111204=CARTESIAN_POINT('Ctrl Pts',(-16.6813531724137,19.7300284204965,
-1.65951524838366));
#111205=CARTESIAN_POINT('Ctrl Pts',(-16.6917045230492,19.7684680761476,
-1.65714500416665));
#111206=CARTESIAN_POINT('Ctrl Pts',(-16.693623922798,19.7754527714791,-1.65671177622824));
#111207=CARTESIAN_POINT('Ctrl Pts',(-16.6966886322803,19.7863853383506,
-1.65602949294841));
#111208=CARTESIAN_POINT('Ctrl Pts',(-16.6978096797495,19.7903400345965,
-1.65578182540814));
#111209=CARTESIAN_POINT('Ctrl Pts',(-16.6999263418473,19.7977249019883,
-1.65531768475457));
#111210=CARTESIAN_POINT('Ctrl Pts',(-16.7009191219703,19.8011558269973,
-1.65510137735003));
#111211=CARTESIAN_POINT('Ctrl Pts',(-16.7032047709694,19.8089805301996,
-1.65460652994716));
#111212=CARTESIAN_POINT('Ctrl Pts',(-16.7045032144444,19.8133726199457,
-1.65432766855632));
#111213=CARTESIAN_POINT('Ctrl Pts',(-16.7085367007406,19.8268551290962,
-1.65346833805376));
#111214=CARTESIAN_POINT('Ctrl Pts',(-16.7113186002461,19.8359312474635,
-1.652885234344));
#111215=CARTESIAN_POINT('Ctrl Pts',(-16.7367835368353,19.9170606218719,
-1.64763344775525));
#111216=CARTESIAN_POINT('Ctrl Pts',(-16.7632447056273,19.9878630869451,
-1.64277153447652));
#111217=CARTESIAN_POINT('Ctrl Pts',(-16.8475448761804,20.1812114853825,
-1.62897837287824));
#111218=CARTESIAN_POINT('Ctrl Pts',(-16.9134494627898,20.2998630218719,
-1.61992773292954));
#111219=CARTESIAN_POINT('Ctrl Pts',(-17.0412259322724,20.4854769435079,
-1.60532414890131));
#111220=CARTESIAN_POINT('Ctrl Pts',(-17.0968888214295,20.5562308769006,
-1.59962552812818));
#111221=CARTESIAN_POINT('Ctrl Pts',(-17.1707195242886,20.6386809476795,
-1.59283182932643));
#111222=CARTESIAN_POINT('Ctrl Pts',(-17.1847748556969,20.6539207304438,
-1.59156881984961));
#111223=CARTESIAN_POINT('Ctrl Pts',(-17.2051793221326,20.6754027754882,
-1.58977737081244));
#111224=CARTESIAN_POINT('Ctrl Pts',(-17.2113471489855,20.681814894202,-1.58924119213932));
#111225=CARTESIAN_POINT('Ctrl Pts',(-17.2220950721111,20.6928484464511,
-1.58831596558539));
#111226=CARTESIAN_POINT('Ctrl Pts',(-17.2266563535593,20.6974879623549,
-1.58792610574032));
#111227=CARTESIAN_POINT('Ctrl Pts',(-17.2354573882277,20.7063577865244,
-1.58717917307284));
#111228=CARTESIAN_POINT('Ctrl Pts',(-17.2396938407051,20.7105912684611,
-1.58682196062898));
#111229=CARTESIAN_POINT('Ctrl Pts',(-17.250815938143,20.7216116345574,-1.58589018190079));
#111230=CARTESIAN_POINT('Ctrl Pts',(-17.2577302605293,20.7283694780248,
-1.58531689756478));
#111231=CARTESIAN_POINT('Ctrl Pts',(-17.2817714603034,20.7515467143845,
-1.58334382810852));
#111232=CARTESIAN_POINT('Ctrl Pts',(-17.2991282910977,20.7677257807722,
-1.5819544402883));
#111233=CARTESIAN_POINT('Ctrl Pts',(-17.4372178387847,20.8921729389442,
-1.57116043397875));
#111234=CARTESIAN_POINT('Ctrl Pts',(-17.5697566900678,20.9865367991548,
-1.56238143124986));
#111235=CARTESIAN_POINT('Ctrl Pts',(-17.8259908979364,21.1278249193074,
-1.54648533972015));
#111236=CARTESIAN_POINT('Ctrl Pts',(-17.9457581808062,21.1801021444401,
-1.53939274147877));
#111237=CARTESIAN_POINT('Ctrl Pts',(-18.0808430655757,21.2247567998446,
-1.53099669199578));
#111238=CARTESIAN_POINT('Ctrl Pts',(-18.0921655107044,21.2283940873398,
-1.53028995139147));
#111239=CARTESIAN_POINT('Ctrl Pts',(-18.1083098766694,21.2334307329601,
-1.52927717034302));
#111240=CARTESIAN_POINT('Ctrl Pts',(-18.1131072948517,21.234908705344,-1.52897558269147));
#111241=CARTESIAN_POINT('Ctrl Pts',(-18.1213857646729,21.2374269042973,
-1.52845399910139));
#111242=CARTESIAN_POINT('Ctrl Pts',(-18.1248643571753,21.2384752694612,
-1.52823447783377));
#111243=CARTESIAN_POINT('Ctrl Pts',(-18.1316159470946,21.2404910941323,
-1.52780769857028));
#111244=CARTESIAN_POINT('Ctrl Pts',(-18.1348885920772,21.2414595954786,
-1.52760050881988));
#111245=CARTESIAN_POINT('Ctrl Pts',(-18.1437278408755,21.2440522382063,
-1.52704006298681));
#111246=CARTESIAN_POINT('Ctrl Pts',(-18.1492987512022,21.2456614148179,
-1.5266859493317));
#111247=CARTESIAN_POINT('Ctrl Pts',(-18.170019326319,21.2515544994108,-1.52536571578831));
#111248=CARTESIAN_POINT('Ctrl Pts',(-18.1852095920935,21.2556921332941,
-1.52439164039854));
#111249=CARTESIAN_POINT('Ctrl Pts',(-18.32787796054,21.2928488899631,-1.51519416206896));
#111250=CARTESIAN_POINT('Ctrl Pts',(-18.4581190231792,21.3140723916972,
-1.50645220198235));
#111251=CARTESIAN_POINT('Ctrl Pts',(-18.7483780155742,21.3339345601522,
-1.48723402036962));
#111252=CARTESIAN_POINT('Ctrl Pts',(-18.9080304619821,21.3268424909805,
-1.47686494019605));
#111253=CARTESIAN_POINT('Ctrl Pts',(-19.0864174680456,21.2985688712288,
-1.46577189765157));
#111254=CARTESIAN_POINT('Ctrl Pts',(-19.1073848533288,21.29492074396,-1.46447486056233));
#111255=CARTESIAN_POINT('Ctrl Pts',(-19.137128302477,21.2892823234735,-1.46264408471769));
#111256=CARTESIAN_POINT('Ctrl Pts',(-19.1459516656374,21.2875513895393,
-1.46210213502894));
#111257=CARTESIAN_POINT('Ctrl Pts',(-19.1611569950002,21.2844677366788,
-1.46117009979723));
#111258=CARTESIAN_POINT('Ctrl Pts',(-19.1675441768289,21.2831416461337,
-1.46077916987309));
#111259=CARTESIAN_POINT('Ctrl Pts',(-19.17976391058,21.2805456422496,-1.46003233689425));
#111260=CARTESIAN_POINT('Ctrl Pts',(-19.185597411166,21.2792805439983,-1.45967628392075));
#111261=CARTESIAN_POINT('Ctrl Pts',(-19.2007567509899,21.2759257786496,
-1.45875220920336));
#111262=CARTESIAN_POINT('Ctrl Pts',(-19.2100739958683,21.2737975884552,
-1.45818542731458));
#111263=CARTESIAN_POINT('Ctrl Pts',(-19.2418174444575,21.2663204067912,
-1.45625818626532));
#111264=CARTESIAN_POINT('Ctrl Pts',(-19.264171028183,21.2606680886822,-1.45490747644726));
#111265=CARTESIAN_POINT('Ctrl Pts',(-19.4549968071667,21.2090851292604,
-1.44342161133107));
#111266=CARTESIAN_POINT('Ctrl Pts',(-19.6172786135118,21.1428401096183,
-1.43402871203011));
#111267=CARTESIAN_POINT('Ctrl Pts',(-19.846006883766,21.0145535142479,-1.41976145696229));
#111268=CARTESIAN_POINT('Ctrl Pts',(-19.9196792641771,20.9669973918359,
-1.41496702939098));
#111269=CARTESIAN_POINT('Ctrl Pts',(-20.0207558050714,20.8924846767388,
-1.40779861654817));
#111270=CARTESIAN_POINT('Ctrl Pts',(-20.0507099584124,20.8691331978145,
-1.40559291803075));
#111271=CARTESIAN_POINT('Ctrl Pts',(-20.0858687956549,20.8401707167837,
-1.4028827589211));
#111272=CARTESIAN_POINT('Ctrl Pts',(-20.0916937734104,20.8353195740972,
-1.40242963365393));
#111273=CARTESIAN_POINT('Ctrl Pts',(-20.1006932920051,20.8277423893667,
-1.40172291874549));
#111274=CARTESIAN_POINT('Ctrl Pts',(-20.1038860843742,20.8250379868916,
-1.40147088500506));
#111275=CARTESIAN_POINT('Ctrl Pts',(-20.1097830276902,20.8200129764703,
-1.40100291356065));
#111276=CARTESIAN_POINT('Ctrl Pts',(-20.1124893449939,20.817694999959,-1.40078716852823));
#111277=CARTESIAN_POINT('Ctrl Pts',(-20.1185827513068,20.812449233957,-1.40029920425895));
#111278=CARTESIAN_POINT('Ctrl Pts',(-20.1219663921994,20.809517543673,-1.40002669898897));
#111279=CARTESIAN_POINT('Ctrl Pts',(-20.1318927159867,20.8008617948016,
-1.39922279338479));
#111280=CARTESIAN_POINT('Ctrl Pts',(-20.1384093776285,20.7951082242273,
-1.39868927156008));
#111281=CARTESIAN_POINT('Ctrl Pts',(-20.1842710770323,20.7541114430327,
-1.39489478221264));
#111282=CARTESIAN_POINT('Ctrl Pts',(-20.2223171047442,20.7174495705688,
-1.39153861526006));
#111283=CARTESIAN_POINT('Ctrl Pts',(-20.2724917413791,20.6653429351066,
-1.38686514685341));
#111284=CARTESIAN_POINT('Ctrl Pts',(-20.2858390408807,20.651092278134,-1.38559624224201));
#111285=CARTESIAN_POINT('Ctrl Pts',(-20.3975968402582,20.5284125485089,
-1.37476366487907));
#111286=CARTESIAN_POINT('Ctrl Pts',(-20.4847193863943,20.4102152054933,
-1.36495843767335));
#111287=CARTESIAN_POINT('Ctrl Pts',(-20.5902290357467,20.2307612337731,
-1.35150939859198));
#111288=CARTESIAN_POINT('Ctrl Pts',(-20.6191743012523,20.1762037026442,
-1.347583287487));
#111289=CARTESIAN_POINT('Ctrl Pts',(-20.6616864783605,20.0868420836187,
-1.34141728728218));
#111290=CARTESIAN_POINT('Ctrl Pts',(-20.6767885689105,20.0528119545064,
-1.33912762571612));
#111291=CARTESIAN_POINT('Ctrl Pts',(-20.6952311505789,20.0081105667389,
-1.33619305310821));
#111292=CARTESIAN_POINT('Ctrl Pts',(-20.6993949396811,19.9977881672321,
-1.33552036370463));
#111293=CARTESIAN_POINT('Ctrl Pts',(-20.7060329042927,19.980950506244,-1.33443100152554));
#111294=CARTESIAN_POINT('Ctrl Pts',(-20.7085566179745,19.9744551210768,
-1.33401266450816));
#111295=CARTESIAN_POINT('Ctrl Pts',(-20.7133473849458,19.9619422592231,
-1.3332103758235));
#111296=CARTESIAN_POINT('Ctrl Pts',(-20.7156191794287,19.9559266917677,
-1.33282626855246));
#111297=CARTESIAN_POINT('Ctrl Pts',(-20.7207568627085,19.9421326041437,
-1.33194908268649));
#111298=CARTESIAN_POINT('Ctrl Pts',(-20.7236045542558,19.9343473833711,
-1.33145661645791));
#111299=CARTESIAN_POINT('Ctrl Pts',(-20.7310458706766,19.9136273509501,
-1.33015272451114));
#111300=CARTESIAN_POINT('Ctrl Pts',(-20.7355595981026,19.9006641156193,
-1.32934395282688));
#111301=CARTESIAN_POINT('Ctrl Pts',(-20.7688588159741,19.8019488125391,
-1.32323618964279));
#111302=CARTESIAN_POINT('Ctrl Pts',(-20.7922498000777,19.7144695028033,
-1.31812049820499));
#111303=CARTESIAN_POINT('Ctrl Pts',(-20.8373639130496,19.4886586124642,
-1.3053742556948));
#111304=CARTESIAN_POINT('Ctrl Pts',(-20.8511051845503,19.3491947094905,
-1.29793919539568));
#111305=CARTESIAN_POINT('Ctrl Pts',(-20.8509840406832,19.1891096026292,
-1.28909428040406));
#111306=CARTESIAN_POINT('Ctrl Pts',(-20.8506770365379,19.1688228885415,
-1.28796720666155));
#111307=CARTESIAN_POINT('Ctrl Pts',(-20.8483264336703,19.0891816749561,
-1.28350793907996));
#111308=CARTESIAN_POINT('Ctrl Pts',(-20.8440773401239,19.029924794281,-1.28011469178611));
#111309=CARTESIAN_POINT('Ctrl Pts',(-20.8363297207849,18.9620447043256,
-1.27606213717897));
#111310=CARTESIAN_POINT('Ctrl Pts',(-20.8352591883989,18.9531651479409,
-1.27552872938984));
#111311=CARTESIAN_POINT('Ctrl Pts',(-20.8335616374147,18.9397981216427,
-1.27472044424236));
#111312=CARTESIAN_POINT('Ctrl Pts',(-20.8329764096806,18.9353053158733,
-1.2744478656179));
#111313=CARTESIAN_POINT('Ctrl Pts',(-20.8319046586927,18.9272787151137,
-1.27395921812067));
#111314=CARTESIAN_POINT('Ctrl Pts',(-20.831423622613,18.9237442402599,-1.27374346151846));
#111315=CARTESIAN_POINT('Ctrl Pts',(-20.8303644473174,18.9161063311495,
-1.2732759425222));
#111316=CARTESIAN_POINT('Ctrl Pts',(-20.8297832003396,18.9120034307911,
-1.2730240118858));
#111317=CARTESIAN_POINT('Ctrl Pts',(-20.8281309513191,18.9005821117377,
-1.27232055547921));
#111318=CARTESIAN_POINT('Ctrl Pts',(-20.827033648108,18.8932676428192,-1.2718675827939));
#111319=CARTESIAN_POINT('Ctrl Pts',(-20.8205389576268,18.8514691043742,
-1.26926555580998));
#111320=CARTESIAN_POINT('Ctrl Pts',(-20.8143280450887,18.817119074259,-1.26707459920712));
#111321=CARTESIAN_POINT('Ctrl Pts',(-20.7918958078795,18.7084703106017,
-1.26000962832172));
#111322=CARTESIAN_POINT('Ctrl Pts',(-20.7725200131397,18.634887319593,-1.25502398948114));
#111323=CARTESIAN_POINT('Ctrl Pts',(-20.7408447834904,18.5364539837809,
-1.2482018376817));
#111324=CARTESIAN_POINT('Ctrl Pts',(-20.7319594999981,18.5105754523218,
-1.24639321905346));
#111325=CARTESIAN_POINT('Ctrl Pts',(-20.7225806756345,18.4848898867987,
-1.24458630806144));
#111326=CARTESIAN_POINT('Origin',(-18.734,19.211,0.));
#111327=CARTESIAN_POINT('',(-20.7225806137986,18.4848897174502,-0.444429630404752));
#111328=CARTESIAN_POINT('',(-20.7225806137986,18.4848897174502,-0.666446459697765));
#111329=CARTESIAN_POINT('',(-20.7225806137986,18.4848897174502,0.));
#111330=CARTESIAN_POINT('',(-17.1140743056112,20.5739122292573,0.));
#111331=CARTESIAN_POINT('Ctrl Pts',(-20.7225806137986,18.4848897174502,
-0.444429630404752));
#111332=CARTESIAN_POINT('Ctrl Pts',(-20.6978891218494,18.4172677275186,
-0.44011526652472));
#111333=CARTESIAN_POINT('Ctrl Pts',(-20.6697399412968,18.3508947277507,
-0.435800902644688));
#111334=CARTESIAN_POINT('Ctrl Pts',(-20.6382938060541,18.2861464439036,
-0.431486538764656));
#111335=CARTESIAN_POINT('Ctrl Pts',(-20.6068209811841,18.2213432055274,
-0.427168513106713));
#111336=CARTESIAN_POINT('Ctrl Pts',(-20.5720458283503,18.1581678859396,
-0.422850487448771));
#111337=CARTESIAN_POINT('Ctrl Pts',(-20.5341758800126,18.0969731596496,
-0.418532461790828));
#111338=CARTESIAN_POINT('Ctrl Pts',(-20.496290462457,18.0357534363742,-0.414212672294214));
#111339=CARTESIAN_POINT('Ctrl Pts',(-20.4553080152584,17.9765163262865,
-0.4098928827976));
#111340=CARTESIAN_POINT('Ctrl Pts',(-20.4114788156669,17.9195845660715,
-0.405573093300986));
#111341=CARTESIAN_POINT('Ctrl Pts',(-20.3675728424278,17.8625530810398,
-0.401245737022412));
#111342=CARTESIAN_POINT('Ctrl Pts',(-20.3208104807034,17.8078353893813,
-0.396918380743837));
#111343=CARTESIAN_POINT('Ctrl Pts',(-20.2714811519989,17.7557197152273,
-0.392591024465263));
#111344=CARTESIAN_POINT('Ctrl Pts',(-20.2294416137679,17.7113055921575,
-0.388903156324941));
#111345=CARTESIAN_POINT('Ctrl Pts',(-20.1855385022242,17.6687807601312,
-0.385215288184619));
#111346=CARTESIAN_POINT('Ctrl Pts',(-20.139969531998,17.6283001942588,-0.381527420044297));
#111347=CARTESIAN_POINT('Ctrl Pts',(-20.0856806361702,17.5800734028086,
-0.377133853801673));
#111348=CARTESIAN_POINT('Ctrl Pts',(-20.028804456646,17.534551575879,-0.372740287559049));
#111349=CARTESIAN_POINT('Ctrl Pts',(-19.9696413059749,17.4920236874905,
-0.368346721316425));
#111350=CARTESIAN_POINT('Ctrl Pts',(-19.9105644543723,17.4495578329375,
-0.36395956380406));
#111351=CARTESIAN_POINT('Ctrl Pts',(-19.8492076419246,17.4100775251571,
-0.359572406291694));
#111352=CARTESIAN_POINT('Ctrl Pts',(-19.7859055363078,17.3738326851686,
-0.355185248779329));
#111353=CARTESIAN_POINT('Ctrl Pts',(-19.7226758978493,17.3376293376475,
-0.350803113609185));
#111354=CARTESIAN_POINT('Ctrl Pts',(-19.6575058056517,17.3046543374869,
-0.346420978439041));
#111355=CARTESIAN_POINT('Ctrl Pts',(-19.5907589079217,17.2751143696755,
-0.342038843268897));
#111356=CARTESIAN_POINT('Ctrl Pts',(-19.5240531514201,17.2455926096102,
-0.33765940914449));
#111357=CARTESIAN_POINT('Ctrl Pts',(-19.4557729567064,17.2195018746871,
-0.333279975020084));
#111358=CARTESIAN_POINT('Ctrl Pts',(-19.3863053176006,17.1970022908082,
-0.328900540895677));
#111359=CARTESIAN_POINT('Ctrl Pts',(-19.3168577535507,17.1745092089554,
-0.324522372358906));
#111360=CARTESIAN_POINT('Ctrl Pts',(-19.2462238836977,17.1556053656812,
-0.320144203822134));
#111361=CARTESIAN_POINT('Ctrl Pts',(-19.1748077989579,17.1404016602977,
-0.315766035285363));
#111362=CARTESIAN_POINT('Ctrl Pts',(-19.1033889720517,17.1251973711369,
-0.311387698639869));
#111363=CARTESIAN_POINT('Ctrl Pts',(-19.0311883413904,17.1136936001516,
-0.307009361994375));
#111364=CARTESIAN_POINT('Ctrl Pts',(-18.9586205452228,17.1059502118326,
-0.302631025348881));
#111365=CARTESIAN_POINT('Ctrl Pts',(-18.8859767969382,17.0981987189992,
-0.298248106175667));
#111366=CARTESIAN_POINT('Ctrl Pts',(-18.8129655950942,17.0942155178377,
-0.293865187002452));
#111367=CARTESIAN_POINT('Ctrl Pts',(-18.740006248305,17.0940085203333,-0.289482267829238));
#111368=CARTESIAN_POINT('Ctrl Pts',(-18.6670065469439,17.0938014083365,
-0.285096924417943));
#111369=CARTESIAN_POINT('Ctrl Pts',(-18.5940592383891,17.0973746352134,
-0.280711581006648));
#111370=CARTESIAN_POINT('Ctrl Pts',(-18.5215804684087,17.1046840354309,
-0.276326237595353));
#111371=CARTESIAN_POINT('Ctrl Pts',(-18.4489736078896,17.1120063534313,
-0.271933144038736));
#111372=CARTESIAN_POINT('Ctrl Pts',(-18.3768374152679,17.1230779575914,
-0.267540050482118));
#111373=CARTESIAN_POINT('Ctrl Pts',(-18.3055792094826,17.1378032832718,
-0.263146956925501));
#111374=CARTESIAN_POINT('Ctrl Pts',(-18.2580242315412,17.1476303976399,
-0.260215175737955));
#111375=CARTESIAN_POINT('Ctrl Pts',(-18.2108600441032,17.159083715391,-0.25728339455041));
#111376=CARTESIAN_POINT('Ctrl Pts',(-18.1642034381997,17.1721226426878,
-0.254351613362864));
#111377=CARTESIAN_POINT('Ctrl Pts',(-18.0951058972849,17.1914330446111,
-0.250009701502006));
#111378=CARTESIAN_POINT('Ctrl Pts',(-18.0268399854881,17.2143024101294,
-0.245667789641149));
#111379=CARTESIAN_POINT('Ctrl Pts',(-17.9598043906283,17.2406421242755,
-0.241325877780291));
#111380=CARTESIAN_POINT('Ctrl Pts',(-17.8928697395248,17.266942175468,-0.236990504071195));
#111381=CARTESIAN_POINT('Ctrl Pts',(-17.8271621848895,17.29670202984,-0.232655130362099));
#111382=CARTESIAN_POINT('Ctrl Pts',(-17.7630669345952,17.3297828454685,
-0.228319756653002));
#111383=CARTESIAN_POINT('Ctrl Pts',(-17.6990453506666,17.3628256404409,
-0.223989365703525));
#111384=CARTESIAN_POINT('Ctrl Pts',(-17.6366328289126,17.3991815955316,
-0.219658974754049));
#111385=CARTESIAN_POINT('Ctrl Pts',(-17.5761945067698,17.4386638468265,
-0.215328583804572));
#111386=CARTESIAN_POINT('Ctrl Pts',(-17.5157933283169,17.4781218334421,
-0.211000854191362));
#111387=CARTESIAN_POINT('Ctrl Pts',(-17.4573643561352,17.5207020380533,
-0.206673124578153));
#111388=CARTESIAN_POINT('Ctrl Pts',(-17.4012466091921,17.5661725320599,
-0.202345394964943));
#111389=CARTESIAN_POINT('Ctrl Pts',(-17.3451439091011,17.6116308340625,
-0.19801882574592));
#111390=CARTESIAN_POINT('Ctrl Pts',(-17.2913515880726,17.6599775776503,
-0.193692256526897));
#111391=CARTESIAN_POINT('Ctrl Pts',(-17.2401767514858,17.7109396338152,
-0.189365687307874));
#111392=CARTESIAN_POINT('Ctrl Pts',(-17.1889979072006,17.7619056810149,
-0.185038779258564));
#111393=CARTESIAN_POINT('Ctrl Pts',(-17.1404373022758,17.8154870975619,
-0.180711871209254));
#111394=CARTESIAN_POINT('Ctrl Pts',(-17.0947649174399,17.8713741775764,
-0.176384963159944));
#111395=CARTESIAN_POINT('Ctrl Pts',(-17.0490377231869,17.9273283252136,
-0.172052862578908));
#111396=CARTESIAN_POINT('Ctrl Pts',(-17.0062059805783,17.9855932764931,
-0.167720761997871));
#111397=CARTESIAN_POINT('Ctrl Pts',(-16.9664985330235,18.0458272384595,
-0.163388661416834));
#111398=CARTESIAN_POINT('Ctrl Pts',(-16.9267665792056,18.1060983750471,
-0.159053887191346));
#111399=CARTESIAN_POINT('Ctrl Pts',(-16.8901630045679,18.1683405133195,
-0.154719112965857));
#111400=CARTESIAN_POINT('Ctrl Pts',(-16.8568710208891,18.2321865367793,
-0.150384338740368));
#111401=CARTESIAN_POINT('Ctrl Pts',(-16.8235119906461,18.2961611394355,
-0.146040834734123));
#111402=CARTESIAN_POINT('Ctrl Pts',(-16.7934780711976,18.3617456271075,
-0.141697330727878));
#111403=CARTESIAN_POINT('Ctrl Pts',(-16.7669043702654,18.4285526960369,
-0.137353826721632));
#111404=CARTESIAN_POINT('Ctrl Pts',(-16.7461478827044,18.4807351187547,
-0.133961153374898));
#111405=CARTESIAN_POINT('Ctrl Pts',(-16.7275015133356,18.5336630097784,
-0.130568480028163));
#111406=CARTESIAN_POINT('Ctrl Pts',(-16.7110080390405,18.5871470318309,
-0.127175806681429));
#111407=CARTESIAN_POINT('Ctrl Pts',(-16.6890808417458,18.6582511959801,
-0.122665427818863));
#111408=CARTESIAN_POINT('Ctrl Pts',(-16.6708715522275,18.7306260888239,
-0.118155048956298));
#111409=CARTESIAN_POINT('Ctrl Pts',(-16.6565194459451,18.8038593025457,
-0.113644670093733));
#111410=CARTESIAN_POINT('Ctrl Pts',(-16.6414519720022,18.8807427590775,
-0.108909475506494));
#111411=CARTESIAN_POINT('Ctrl Pts',(-16.6306364414031,18.9585718864235,
-0.104174280919255));
#111412=CARTESIAN_POINT('Ctrl Pts',(-16.624175177866,19.0368500074442,-0.0994390863320157));
#111413=CARTESIAN_POINT('Ctrl Pts',(-16.6180411415214,19.1111637754199,
-0.094943703110145));
#111414=CARTESIAN_POINT('Ctrl Pts',(-16.6158311470803,19.18588164953,-0.0904483198882744));
#111415=CARTESIAN_POINT('Ctrl Pts',(-16.6175803959886,19.2605687376906,
-0.0859529366664038));
#111416=CARTESIAN_POINT('Ctrl Pts',(-16.6193280001048,19.3351855987192,
-0.0814617803849424));
#111417=CARTESIAN_POINT('Ctrl Pts',(-16.6250274372589,19.4097712832384,
-0.076970624103481));
#111418=CARTESIAN_POINT('Ctrl Pts',(-16.6346618981062,19.4838892338239,
-0.0724794678220196));
#111419=CARTESIAN_POINT('Ctrl Pts',(-16.6442898170097,19.5579568572063,
-0.0679913611032213));
#111420=CARTESIAN_POINT('Ctrl Pts',(-16.6578473889511,19.6315569329051,
-0.0635032543844231));
#111421=CARTESIAN_POINT('Ctrl Pts',(-16.6752659458499,19.7042576347942,
-0.0590151476656248));
#111422=CARTESIAN_POINT('Ctrl Pts',(-16.6926772219334,19.7769279483805,
-0.054528916938974));
#111423=CARTESIAN_POINT('Ctrl Pts',(-16.7139461674509,19.8486991989659,
-0.0500426862123233));
#111424=CARTESIAN_POINT('Ctrl Pts',(-16.7389532085404,19.9191506194918,
-0.0455564554856726));
#111425=CARTESIAN_POINT('Ctrl Pts',(-16.7639633583527,19.9896107981086,
-0.0410696670581851));
#111426=CARTESIAN_POINT('Ctrl Pts',(-16.7927123885946,20.0587503922126,
-0.0365828786306977));
#111427=CARTESIAN_POINT('Ctrl Pts',(-16.8250314087851,20.1261655138581,
-0.0320960902032102));
#111428=CARTESIAN_POINT('Ctrl Pts',(-16.8573519842581,20.1935838797095,
-0.0276090858587984));
#111429=CARTESIAN_POINT('Ctrl Pts',(-16.8932426902261,20.2592772053156,
-0.0231220815143867));
#111430=CARTESIAN_POINT('Ctrl Pts',(-16.9324879501579,20.3228648003574,
-0.0186350771699749));
#111431=CARTESIAN_POINT('Ctrl Pts',(-16.9717602972259,20.3864962836508,
-0.0141449758885697));
#111432=CARTESIAN_POINT('Ctrl Pts',(-17.0143915779344,20.4480187554703,
-0.00965487460716451));
#111433=CARTESIAN_POINT('Ctrl Pts',(-17.0601224600125,20.5070798513692,
-0.00516477332575931));
#111434=CARTESIAN_POINT('Ctrl Pts',(-17.0776565589201,20.5297250103958,
-0.0034431822171712));
#111435=CARTESIAN_POINT('Ctrl Pts',(-17.0956458992255,20.5520086551532,
-0.00172159110858308));
#111436=CARTESIAN_POINT('Ctrl Pts',(-17.1140743056112,20.5739122292573,
5.04250086090388E-15));
#111437=CARTESIAN_POINT('',(-20.3539402423909,20.5738949376539,-2.19221144982933E-7));
#111438=CARTESIAN_POINT('Origin',(-18.734,19.211,0.));
#111439=CARTESIAN_POINT('Ctrl Pts',(-20.3539402423909,20.5738949376539,
-2.19221144982933E-7));
#111440=CARTESIAN_POINT('Ctrl Pts',(-20.307293457224,20.6293394201171,-0.00438523054252598));
#111441=CARTESIAN_POINT('Ctrl Pts',(-20.2577052453279,20.6824952398001,
-0.00877024186390698));
#111442=CARTESIAN_POINT('Ctrl Pts',(-20.2054289850318,20.7330334234202,
-0.013155253185288));
#111443=CARTESIAN_POINT('Ctrl Pts',(-20.1532303457042,20.7834965668072,
-0.0175337535431148));
#111444=CARTESIAN_POINT('Ctrl Pts',(-20.0983519254295,20.8313494565076,
-0.0219122539009416));
#111445=CARTESIAN_POINT('Ctrl Pts',(-20.0410868627427,20.8762966502235,
-0.0262907542587684));
#111446=CARTESIAN_POINT('Ctrl Pts',(-19.9838891952347,20.9211909456447,
-0.0306641015651428));
#111447=CARTESIAN_POINT('Ctrl Pts',(-19.9243108432099,20.9631860414448,
-0.0350374488715171));
#111448=CARTESIAN_POINT('Ctrl Pts',(-19.8626799780619,21.0020249878553,
-0.0394107961778915));
#111449=CARTESIAN_POINT('Ctrl Pts',(-19.8010881104923,21.0408393585139,
-0.0437813762027535));
#111450=CARTESIAN_POINT('Ctrl Pts',(-19.7374467144136,21.0765012852422,
-0.0481519562276155));
#111451=CARTESIAN_POINT('Ctrl Pts',(-19.6721138966917,21.1087964371433,
-0.0525225362524776));
#111452=CARTESIAN_POINT('Ctrl Pts',(-19.606800782292,21.1410818493484,-0.0568917981810183));
#111453=CARTESIAN_POINT('Ctrl Pts',(-19.5397976918716,21.170002288633,-0.061261060109559));
#111454=CARTESIAN_POINT('Ctrl Pts',(-19.4714868524903,21.1953896145677,
-0.0656303220380997));
#111455=CARTESIAN_POINT('Ctrl Pts',(-19.4031739921601,21.2207776915762,
-0.069999713229504));
#111456=CARTESIAN_POINT('Ctrl Pts',(-19.3335537597041,21.2426322814668,
-0.0743691044209083));
#111457=CARTESIAN_POINT('Ctrl Pts',(-19.2630262593489,21.2608341925432,
-0.0787384956123125));
#111458=CARTESIAN_POINT('Ctrl Pts',(-19.1924269638888,21.2790546326772,
-0.0831123347268293));
#111459=CARTESIAN_POINT('Ctrl Pts',(-19.1209190256059,21.2936148503493,
-0.087486173841346));
#111460=CARTESIAN_POINT('Ctrl Pts',(-19.0489146836732,21.3044463790618,
-0.0918600129558628));
#111461=CARTESIAN_POINT('Ctrl Pts',(-18.9768705191302,21.3152838982429,
-0.0962362710591022));
#111462=CARTESIAN_POINT('Ctrl Pts',(-18.9043298854537,21.3223885760892,
-0.100612529162342));
#111463=CARTESIAN_POINT('Ctrl Pts',(-18.8317094286016,21.3257439248198,
-0.104988787265581));
#111464=CARTESIAN_POINT('Ctrl Pts',(-18.7589648320258,21.3291050092905,
-0.109372526283915));
#111465=CARTESIAN_POINT('Ctrl Pts',(-18.6861406230803,21.3287039714963,
-0.113756265302249));
#111466=CARTESIAN_POINT('Ctrl Pts',(-18.6136520423462,21.324576440323,-0.118140004320582));
#111467=CARTESIAN_POINT('Ctrl Pts',(-18.5716442693833,21.3221844995419,
-0.120680419811489));
#111468=CARTESIAN_POINT('Ctrl Pts',(-18.5297491060652,21.3185420587999,
-0.123220835302396));
#111469=CARTESIAN_POINT('Ctrl Pts',(-18.4880458562809,21.3136639196951,
-0.125761250793303));
#111470=CARTESIAN_POINT('Ctrl Pts',(-18.415885212538,21.3052230988983,-0.13015702374017));
#111471=CARTESIAN_POINT('Ctrl Pts',(-18.3440242467257,21.2930474771355,
-0.134552796687037));
#111472=CARTESIAN_POINT('Ctrl Pts',(-18.2728788054799,21.2771694615796,
-0.138948569633904));
#111473=CARTESIAN_POINT('Ctrl Pts',(-18.2018361910671,21.2613143945926,
-0.143337989349932));
#111474=CARTESIAN_POINT('Ctrl Pts',(-18.1315075132682,21.2417676616992,
-0.147727409065961));
#111475=CARTESIAN_POINT('Ctrl Pts',(-18.0623022558515,21.2186132945629,
-0.152116828781989));
#111476=CARTESIAN_POINT('Ctrl Pts',(-17.9931750162608,21.1954850302612,
-0.156501300131427));
#111477=CARTESIAN_POINT('Ctrl Pts',(-17.9251691345195,21.168757363137,-0.160885771480865));
#111478=CARTESIAN_POINT('Ctrl Pts',(-17.8586810464526,21.138564714753,-0.165270242830304));
#111479=CARTESIAN_POINT('Ctrl Pts',(-17.7922332423914,21.1083903595828,
-0.16965205770286));
#111480=CARTESIAN_POINT('Ctrl Pts',(-17.727301843592,21.0747553873415,-0.174033872575416));
#111481=CARTESIAN_POINT('Ctrl Pts',(-17.6642640090407,21.0378426066978,
-0.178415687447972));
#111482=CARTESIAN_POINT('Ctrl Pts',(-17.6012437811929,21.0009401359321,
-0.182796278463204));
#111483=CARTESIAN_POINT('Ctrl Pts',(-17.5401164818006,20.960761917242,-0.187176869478435));
#111484=CARTESIAN_POINT('Ctrl Pts',(-17.4812338530685,20.9175362525016,
-0.191557460493667));
#111485=CARTESIAN_POINT('Ctrl Pts',(-17.4223484413193,20.8743085447519,
-0.195938258552297));
#111486=CARTESIAN_POINT('Ctrl Pts',(-17.3657082969836,20.8280333908517,
-0.200319056610927));
#111487=CARTESIAN_POINT('Ctrl Pts',(-17.3116340465776,20.7789808973788,
-0.204699854669557));
#111488=CARTESIAN_POINT('Ctrl Pts',(-17.2575026772118,20.7298765894584,
-0.20908528019184));
#111489=CARTESIAN_POINT('Ctrl Pts',(-17.205942969612,20.6779894082539,-0.213470705714123));
#111490=CARTESIAN_POINT('Ctrl Pts',(-17.1572398491782,20.6236274904518,
-0.217856131236407));
#111491=CARTESIAN_POINT('Ctrl Pts',(-17.1085094838157,20.5692351621432,
-0.222244010002017));
#111492=CARTESIAN_POINT('Ctrl Pts',(-17.0626391892087,20.5123657149588,
-0.226631888767627));
#111493=CARTESIAN_POINT('Ctrl Pts',(-17.0198728898629,20.4533595495238,
-0.231019767533237));
#111494=CARTESIAN_POINT('Ctrl Pts',(-16.977030854158,20.3942488879739,-0.235415416949259));
#111495=CARTESIAN_POINT('Ctrl Pts',(-16.9373040526506,20.3329943550554,
-0.239811066365281));
#111496=CARTESIAN_POINT('Ctrl Pts',(-16.9008921528455,20.2699639373939,
-0.244206715781303));
#111497=CARTESIAN_POINT('Ctrl Pts',(-16.876785868281,20.2282350193066,-0.247116829679114));
#111498=CARTESIAN_POINT('Ctrl Pts',(-16.8541315650652,20.1857282478032,
-0.250026943576926));
#111499=CARTESIAN_POINT('Ctrl Pts',(-16.8329755574333,20.1425551882545,
-0.252937057474737));
#111500=CARTESIAN_POINT('Ctrl Pts',(-16.8011149178839,20.0775371889959,
-0.257319646645567));
#111501=CARTESIAN_POINT('Ctrl Pts',(-16.7725299917263,20.0107527148536,
-0.261702235816397));
#111502=CARTESIAN_POINT('Ctrl Pts',(-16.7474198406578,19.9425656296656,
-0.266084824987227));
#111503=CARTESIAN_POINT('Ctrl Pts',(-16.7223474688912,19.8744811348786,
-0.27046082036424));
#111504=CARTESIAN_POINT('Ctrl Pts',(-16.7007396607462,19.804998667962,-0.274836815741254));
#111505=CARTESIAN_POINT('Ctrl Pts',(-16.6827487993224,19.7345050254952,
-0.279212811118268));
#111506=CARTESIAN_POINT('Ctrl Pts',(-16.6647794915184,19.664095836637,-0.283583563914705));
#111507=CARTESIAN_POINT('Ctrl Pts',(-16.6504186420449,19.5926783449243,
-0.287954316711142));
#111508=CARTESIAN_POINT('Ctrl Pts',(-16.6397693071744,19.5206559465391,
-0.292325069507579));
#111509=CARTESIAN_POINT('Ctrl Pts',(-16.6291268685744,19.4486801882446,
-0.296692991902482));
#111510=CARTESIAN_POINT('Ctrl Pts',(-16.6221912467961,19.3761007777963,
-0.301060914297385));
#111511=CARTESIAN_POINT('Ctrl Pts',(-16.6190144407725,19.3033313828498,
-0.305428836692288));
#111512=CARTESIAN_POINT('Ctrl Pts',(-16.6158386365901,19.2305849365467,
-0.309795381613959));
#111513=CARTESIAN_POINT('Ctrl Pts',(-16.6164193161497,19.1576491077123,
-0.314161926535629));
#111514=CARTESIAN_POINT('Ctrl Pts',(-16.6207564869952,19.0849410663896,
-0.3185284714573));
#111515=CARTESIAN_POINT('Ctrl Pts',(-16.6250937309155,19.0122318000445,
-0.322895089948766));
#111516=CARTESIAN_POINT('Ctrl Pts',(-16.6331875609615,18.9397508116576,
-0.327261708440232));
#111517=CARTESIAN_POINT('Ctrl Pts',(-16.6449859783168,18.8679119395679,
-0.331628326931697));
#111518=CARTESIAN_POINT('Ctrl Pts',(-16.6567966078099,18.7959987095216,
-0.335999465160445));
#111519=CARTESIAN_POINT('Ctrl Pts',(-16.6723194019262,18.724729401209,-0.340370603389193));
#111520=CARTESIAN_POINT('Ctrl Pts',(-16.6914510303897,18.65450857442,-0.344741741617941));
#111521=CARTESIAN_POINT('Ctrl Pts',(-16.7105930357156,18.5842496603425,
-0.349115250721693));
#111522=CARTESIAN_POINT('Ctrl Pts',(-16.7333476210311,18.5150408198692,
-0.353488759825446));
#111523=CARTESIAN_POINT('Ctrl Pts',(-16.7595620940047,18.4472697103238,
-0.357862268929199));
#111524=CARTESIAN_POINT('Ctrl Pts',(-16.7858233028864,18.3793777765166,
-0.362243575249389));
#111525=CARTESIAN_POINT('Ctrl Pts',(-16.8155565194802,18.3129291342218,
-0.36662488156958));
#111526=CARTESIAN_POINT('Ctrl Pts',(-16.8485618556778,18.24828924181,-0.37100618788977));
#111527=CARTESIAN_POINT('Ctrl Pts',(-16.8714293819245,18.2035039250521,
-0.374041746645237));
#111528=CARTESIAN_POINT('Ctrl Pts',(-16.895866654182,18.1595863577281,-0.377077305400704));
#111529=CARTESIAN_POINT('Ctrl Pts',(-16.9217951530525,18.1166496937908,
-0.380112864156171));
#111530=CARTESIAN_POINT('Ctrl Pts',(-16.9592870771133,18.0545644125798,
-0.384502201884909));
#111531=CARTESIAN_POINT('Ctrl Pts',(-17.000046146169,17.9942872611044,-0.388891539613648));
#111532=CARTESIAN_POINT('Ctrl Pts',(-17.043872573219,17.9361830401024,-0.393280877342386));
#111533=CARTESIAN_POINT('Ctrl Pts',(-17.0876340137246,17.8781649769917,
-0.397663706489194));
#111534=CARTESIAN_POINT('Ctrl Pts',(-17.1344534950993,17.8223138297408,
-0.402046535636003));
#111535=CARTESIAN_POINT('Ctrl Pts',(-17.1840867641359,17.7689674201693,
-0.406429364782811));
#111536=CARTESIAN_POINT('Ctrl Pts',(-17.2336617334564,17.7156836718046,
-0.410807045816267));
#111537=CARTESIAN_POINT('Ctrl Pts',(-17.2860435979521,17.6648991677451,
-0.415184726849724));
#111538=CARTESIAN_POINT('Ctrl Pts',(-17.3409475304282,17.6169191309661,
-0.41956240788318));
#111539=CARTESIAN_POINT('Ctrl Pts',(-17.3958166506481,17.5689695162945,
-0.423937313214652));
#111540=CARTESIAN_POINT('Ctrl Pts',(-17.4532043037707,17.5238211571202,
-0.428312218546124));
#111541=CARTESIAN_POINT('Ctrl Pts',(-17.512789475476,17.4817418195099,-0.432687123877597));
#111542=CARTESIAN_POINT('Ctrl Pts',(-17.5723564947757,17.4396753012167,
-0.437060696410096));
#111543=CARTESIAN_POINT('Ctrl Pts',(-17.6341193099784,17.4006762261877,
-0.441434268942594));
#111544=CARTESIAN_POINT('Ctrl Pts',(-17.697725898141,17.3649704807842,-0.445807841475093));
#111545=CARTESIAN_POINT('Ctrl Pts',(-17.7613340609316,17.3292638514586,
-0.450181522278611));
#111546=CARTESIAN_POINT('Ctrl Pts',(-17.8267856659411,17.29685094787,-0.454555203082129));
#111547=CARTESIAN_POINT('Ctrl Pts',(-17.8937034068912,17.2679120875242,
-0.458928883885646));
#111548=CARTESIAN_POINT('Ctrl Pts',(-17.9606903750841,17.2389432895641,
-0.463307089316843));
#111549=CARTESIAN_POINT('Ctrl Pts',(-18.0291460640641,17.2134559021899,
-0.46768529474804));
#111550=CARTESIAN_POINT('Ctrl Pts',(-18.0986732370017,17.1915820382551,
-0.472063500179237));
#111551=CARTESIAN_POINT('Ctrl Pts',(-18.1682382801081,17.1696962600299,
-0.476444090338188));
#111552=CARTESIAN_POINT('Ctrl Pts',(-18.2388755021191,17.1514280448653,
-0.480824680497139));
#111553=CARTESIAN_POINT('Ctrl Pts',(-18.3101751880181,17.1368588455102,
-0.48520527065609));
#111554=CARTESIAN_POINT('Ctrl Pts',(-18.3816008664645,17.1222639011532,
-0.489593601686642));
#111555=CARTESIAN_POINT('Ctrl Pts',(-18.4536908693965,17.1113810977932,
-0.493981932717193));
#111556=CARTESIAN_POINT('Ctrl Pts',(-18.5260286230796,17.1042401877808,
-0.498370263747745));
#111557=CARTESIAN_POINT('Ctrl Pts',(-18.5750326393233,17.0994026962577,
-0.501343066111032));
#111558=CARTESIAN_POINT('Ctrl Pts',(-18.624150260615,17.0962813311373,-0.504315868474319));
#111559=CARTESIAN_POINT('Ctrl Pts',(-18.6732524681258,17.0948717578154,
-0.507288670837606));
#111560=CARTESIAN_POINT('Ctrl Pts',(-18.7457477325719,17.0927906417942,
-0.511677762579042));
#111561=CARTESIAN_POINT('Ctrl Pts',(-18.818490899314,17.0944351534906,-0.516066854320478));
#111562=CARTESIAN_POINT('Ctrl Pts',(-18.8910671105736,17.0998347002719,
-0.520455946061914));
#111563=CARTESIAN_POINT('Ctrl Pts',(-18.9635359557306,17.1052262591976,
-0.524838544771178));
#111564=CARTESIAN_POINT('Ctrl Pts',(-19.035837858837,17.1143617900503,-0.529221143480442));
#111565=CARTESIAN_POINT('Ctrl Pts',(-19.1075565880863,17.1272187073742,
-0.533603742189706));
#111566=CARTESIAN_POINT('Ctrl Pts',(-19.1791914726444,17.1400605939763,
-0.537981217305189));
#111567=CARTESIAN_POINT('Ctrl Pts',(-19.2502440654555,17.1566151398615,
-0.542358692420672));
#111568=CARTESIAN_POINT('Ctrl Pts',(-19.320303591177,17.1768079984984,-0.546736167536156));
#111569=CARTESIAN_POINT('Ctrl Pts',(-19.3903189366748,17.1969881233207,
-0.55111088217292));
#111570=CARTESIAN_POINT('Ctrl Pts',(-19.4593419954755,17.2208018753163,
-0.555485596809685));
#111571=CARTESIAN_POINT('Ctrl Pts',(-19.5269739113634,17.2481242077255,
-0.55986031144645));
#111572=CARTESIAN_POINT('Ctrl Pts',(-19.5945854628885,17.2754383132218,
-0.564233708831224));
#111573=CARTESIAN_POINT('Ctrl Pts',(-19.6608062563393,17.3062587212117,
-0.568607106215997));
#111574=CARTESIAN_POINT('Ctrl Pts',(-19.725255876789,17.3404116469059,-0.572980503600771));
#111575=CARTESIAN_POINT('Ctrl Pts',(-19.7897073269138,17.3745655421753,
-0.577354025142924));
#111576=CARTESIAN_POINT('Ctrl Pts',(-19.8523870791116,17.4120519154598,
-0.581727546685077));
#111577=CARTESIAN_POINT('Ctrl Pts',(-19.9129393606857,17.4526510631203,
-0.58610106822723));
#111578=CARTESIAN_POINT('Ctrl Pts',(-19.973554643469,17.4932924518876,-0.590479140170093));
#111579=CARTESIAN_POINT('Ctrl Pts',(-20.0320376349008,17.5370528121332,
-0.594857212112955));
#111580=CARTESIAN_POINT('Ctrl Pts',(-20.0880623158587,17.5836695956963,
-0.599235284055817));
#111581=CARTESIAN_POINT('Ctrl Pts',(-20.1441176953746,17.6303119227879,
-0.60361575495024));
#111582=CARTESIAN_POINT('Ctrl Pts',(-20.1977117280629,17.6798134620823,
-0.607996225844662));
#111583=CARTESIAN_POINT('Ctrl Pts',(-20.2485542488445,17.731873762214,-0.612376696739084));
#111584=CARTESIAN_POINT('Ctrl Pts',(-20.2994868988124,17.7840263503049,
-0.616764932950229));
#111585=CARTESIAN_POINT('Ctrl Pts',(-20.3476579775569,17.8387463951233,
-0.621153169161374));
#111586=CARTESIAN_POINT('Ctrl Pts',(-20.392817087906,17.8956997039189,-0.625541405372519));
#111587=CARTESIAN_POINT('Ctrl Pts',(-20.4234260448481,17.9343027978054,
-0.628515762754692));
#111588=CARTESIAN_POINT('Ctrl Pts',(-20.4526521208593,17.9739312228937,
-0.631490120136865));
#111589=CARTESIAN_POINT('Ctrl Pts',(-20.4804290546179,18.0144739630136,
-0.634464477519039));
#111590=CARTESIAN_POINT('Ctrl Pts',(-20.5219934548532,18.0751406547235,
-0.638915198457137));
#111591=CARTESIAN_POINT('Ctrl Pts',(-20.5604706098725,18.1380885636268,
-0.643365919395235));
#111592=CARTESIAN_POINT('Ctrl Pts',(-20.5956058248693,18.2029758173473,
-0.647816640333333));
#111593=CARTESIAN_POINT('Ctrl Pts',(-20.630675943178,18.2677428513588,-0.652259115208526));
#111594=CARTESIAN_POINT('Ctrl Pts',(-20.6624162095655,18.3344416830545,
-0.656701590083719));
#111595=CARTESIAN_POINT('Ctrl Pts',(-20.6906150240255,18.4027013870123,
-0.661144064958911));
#111596=CARTESIAN_POINT('Ctrl Pts',(-20.7018340891964,18.4298589140898,
-0.662911529871862));
#111597=CARTESIAN_POINT('Ctrl Pts',(-20.7124930667491,18.4572631970918,
-0.664678994784814));
#111598=CARTESIAN_POINT('Ctrl Pts',(-20.7225806137986,18.4848897174502,
-0.666446459697765));
#111599=CARTESIAN_POINT('Origin',(-18.734,19.211,0.));
#111600=CARTESIAN_POINT('',(-20.8509997094738,19.2121090932814,-0.710943720977507));
#111601=CARTESIAN_POINT('Ctrl Pts',(-20.7225806137986,18.4848897174502,
-0.666446459697765));
#111602=CARTESIAN_POINT('Ctrl Pts',(-20.7478890253796,18.5542012502099,
-0.6708808112059));
#111603=CARTESIAN_POINT('Ctrl Pts',(-20.7695972005712,18.6249130163545,
-0.675315162714036));
#111604=CARTESIAN_POINT('Ctrl Pts',(-20.7875591148731,18.696622743775,-0.679749514222171));
#111605=CARTESIAN_POINT('Ctrl Pts',(-20.8055066444181,18.7682750426286,
-0.684180314490311));
#111606=CARTESIAN_POINT('Ctrl Pts',(-20.819713760552,18.8409232657494,-0.688611114758451));
#111607=CARTESIAN_POINT('Ctrl Pts',(-20.8300842049517,18.914149859774,-0.69304191502659));
#111608=CARTESIAN_POINT('Ctrl Pts',(-20.8404495516885,18.987340458766,-0.697470537304587));
#111609=CARTESIAN_POINT('Ctrl Pts',(-20.8469819094182,19.0611084042472,
-0.701899159582584));
#111610=CARTESIAN_POINT('Ctrl Pts',(-20.8496363438536,19.135027238001,-0.70632778186058));
#111611=CARTESIAN_POINT('Ctrl Pts',(-20.8505585800838,19.1607090275647,
-0.707866428232889));
#111612=CARTESIAN_POINT('Ctrl Pts',(-20.8510131737292,19.1864089784392,
-0.709405074605198));
#111613=CARTESIAN_POINT('Ctrl Pts',(-20.8509997094738,19.2121090932814,
-0.710943720977507));
#111614=CARTESIAN_POINT('Ctrl Pts',(-20.8509997571974,19.2120139161396,
-0.712619133284185));
#111615=CARTESIAN_POINT('Ctrl Pts',(-20.8509644874188,19.2856552261446,
-0.716802597200607));
#111616=CARTESIAN_POINT('Ctrl Pts',(-20.847086770126,19.3592496595573,-0.720880559931813));
#111617=CARTESIAN_POINT('Ctrl Pts',(-20.8222620020048,19.595214125847,-0.733864837499567));
#111618=CARTESIAN_POINT('Ctrl Pts',(-20.7863401949605,19.7553767871956,
-0.742508191233821));
#111619=CARTESIAN_POINT('Ctrl Pts',(-20.7220379866568,19.9392645428959,
-0.753708987400108));
#111620=CARTESIAN_POINT('Ctrl Pts',(-20.7110792378879,19.9685102205914,
-0.75553220632609));
#111621=CARTESIAN_POINT('Ctrl Pts',(-20.6968237939304,20.0041347978913,
-0.757817282440839));
#111622=CARTESIAN_POINT('Ctrl Pts',(-20.6941357135984,20.0107549841072,
-0.758244682239247));
#111623=CARTESIAN_POINT('Ctrl Pts',(-20.6898577693182,20.0211395457907,
-0.758919647536638));
#111624=CARTESIAN_POINT('Ctrl Pts',(-20.6882904028546,20.0249132128897,
-0.759165870600361));
#111625=CARTESIAN_POINT('Ctrl Pts',(-20.6853317611769,20.0319787634579,
-0.75962869952792));
#111626=CARTESIAN_POINT('Ctrl Pts',(-20.6839430718721,20.0352716712264,
-0.759845148210268));
#111627=CARTESIAN_POINT('Ctrl Pts',(-20.6807434917007,20.042805290023,-0.760342046420319));
#111628=CARTESIAN_POINT('Ctrl Pts',(-20.6789270824204,20.0470436030065,
-0.760622828751681));
#111629=CARTESIAN_POINT('Ctrl Pts',(-20.6732663761397,20.0601337089901,
-0.761493774946246));
#111630=CARTESIAN_POINT('Ctrl Pts',(-20.6693754502033,20.0689650296054,
-0.762086675123137));
#111631=CARTESIAN_POINT('Ctrl Pts',(-20.6287967220064,20.1593867246904,
-0.768209612911351));
#111632=CARTESIAN_POINT('Ctrl Pts',(-20.5870364700279,20.2385914074892,
-0.7740093348254));
#111633=CARTESIAN_POINT('Ctrl Pts',(-20.4754719849046,20.4211519047305,
-0.788069021307969));
#111634=CARTESIAN_POINT('Ctrl Pts',(-20.4012933161308,20.5214689210608,
-0.796363873212959));
#111635=CARTESIAN_POINT('Ctrl Pts',(-20.276280420012,20.6626053145,-0.808564248865147));
#111636=CARTESIAN_POINT('Ctrl Pts',(-20.2316806753148,20.708578286057,-0.812641832944686));
#111637=CARTESIAN_POINT('Ctrl Pts',(-20.1666557738227,20.7697897404679,
-0.818210628129412));
#111638=CARTESIAN_POINT('Ctrl Pts',(-20.147939876371,20.7867861952464,-0.819773459131753));
#111639=CARTESIAN_POINT('Ctrl Pts',(-20.1190927133919,20.8120552684204,
-0.822123071126478));
#111640=CARTESIAN_POINT('Ctrl Pts',(-20.1091823322634,20.820575522391,-0.822920016855451));
#111641=CARTESIAN_POINT('Ctrl Pts',(-20.0907767487775,20.8361052671643,
-0.824381527496059));
#111642=CARTESIAN_POINT('Ctrl Pts',(-20.0823045815443,20.8431412432604,
-0.825047164872525));
#111643=CARTESIAN_POINT('Ctrl Pts',(-20.0684848163721,20.8544372539313,
-0.826121634120932));
#111644=CARTESIAN_POINT('Ctrl Pts',(-20.0631708905226,20.8587379883434,
-0.82653211244437));
#111645=CARTESIAN_POINT('Ctrl Pts',(-20.0528357104379,20.8670200573879,
-0.827325344376364));
#111646=CARTESIAN_POINT('Ctrl Pts',(-20.0478170344389,20.871004476804,-0.827708219487189));
#111647=CARTESIAN_POINT('Ctrl Pts',(-20.0362987645331,20.8800640874097,
-0.82858172565631));
#111648=CARTESIAN_POINT('Ctrl Pts',(-20.0297874270979,20.885124232755,-0.829071754163217));
#111649=CARTESIAN_POINT('Ctrl Pts',(-20.0127186575559,20.8982296149092,
-0.830346638840626));
#111650=CARTESIAN_POINT('Ctrl Pts',(-20.0021147343949,20.9062139130508,
-0.831129096273738));
#111651=CARTESIAN_POINT('Ctrl Pts',(-19.9282389158269,20.9607581179443,
-0.83651618177468));
#111652=CARTESIAN_POINT('Ctrl Pts',(-19.8624894643728,21.003867420594,-0.840984804573554));
#111653=CARTESIAN_POINT('Ctrl Pts',(-19.6590188628693,21.1216359093979,
-0.854082781571101));
#111654=CARTESIAN_POINT('Ctrl Pts',(-19.5152783900345,21.1847757490113,
-0.862369425581119));
#111655=CARTESIAN_POINT('Ctrl Pts',(-19.3162813833807,21.2470107542544,
-0.873917128287804));
#111656=CARTESIAN_POINT('Ctrl Pts',(-19.2661150801762,21.2606936873164,
-0.876838311748348));
#111657=CARTESIAN_POINT('Ctrl Pts',(-19.188878892102,21.2787334268187,-0.881419646854493));
#111658=CARTESIAN_POINT('Ctrl Pts',(-19.1621414977169,21.2844345971685,
-0.883020721231884));
#111659=CARTESIAN_POINT('Ctrl Pts',(-19.1285733413727,21.2909153468698,
-0.885058118865585));
#111660=CARTESIAN_POINT('Ctrl Pts',(-19.1218378389243,21.2921818228192,
-0.885468292525569));
#111661=CARTESIAN_POINT('Ctrl Pts',(-19.1111362675934,21.294140284196,-0.886122326229782));
#111662=CARTESIAN_POINT('Ctrl Pts',(-19.1071741028785,21.2948537127864,
-0.886364984222708));
#111663=CARTESIAN_POINT('Ctrl Pts',(-19.099675739095,21.2961817993719,-0.886825213188938));
#111664=CARTESIAN_POINT('Ctrl Pts',(-19.0961400036328,21.2967987677715,
-0.887042651213709));
#111665=CARTESIAN_POINT('Ctrl Pts',(-19.0880231761644,21.2981938536432,
-0.887542773090114));
#111666=CARTESIAN_POINT('Ctrl Pts',(-19.0834410843493,21.2989658808437,
-0.887825798261902));
#111667=CARTESIAN_POINT('Ctrl Pts',(-19.071206252694,21.3009859007711,-0.888583307904103));
#111668=CARTESIAN_POINT('Ctrl Pts',(-19.0635492186102,21.3022069315537,
-0.889059256198721));
#111669=CARTESIAN_POINT('Ctrl Pts',(-19.0080358175804,21.3107469313232,
-0.892522552686661));
#111670=CARTESIAN_POINT('Ctrl Pts',(-18.9599513418803,21.3164638435916,
-0.895590319796249));
#111671=CARTESIAN_POINT('Ctrl Pts',(-18.9040180682394,21.3211759547509,
-0.899205847696877));
#111672=CARTESIAN_POINT('Ctrl Pts',(-18.896315118878,21.3217824386576,-0.899704802798105));
#111673=CARTESIAN_POINT('Ctrl Pts',(-18.7362031820373,21.3335070701645,
-0.910095381370922));
#111674=CARTESIAN_POINT('Ctrl Pts',(-18.5830358157563,21.3281335954217,
-0.920358116998048));
#111675=CARTESIAN_POINT('Ctrl Pts',(-18.3399050110413,21.2930647988216,
-0.936301292287723));
#111676=CARTESIAN_POINT('Ctrl Pts',(-18.2489969350588,21.2737846834032,
-0.942191496674143));
#111677=CARTESIAN_POINT('Ctrl Pts',(-18.1393445762057,21.242875597218,-0.949187253272218));
#111678=CARTESIAN_POINT('Ctrl Pts',(-18.119137872333,21.2368524452801,-0.950472112144795));
#111679=CARTESIAN_POINT('Ctrl Pts',(-18.0904786757538,21.227841477502,-0.952288825887074));
#111680=CARTESIAN_POINT('Ctrl Pts',(-18.0819504618521,21.2251004552375,
-0.952828721196307));
#111681=CARTESIAN_POINT('Ctrl Pts',(-18.0672480883332,21.2202718483831,
-0.953758328574996));
#111682=CARTESIAN_POINT('Ctrl Pts',(-18.0610657480937,21.2182097465142,
-0.954148873460335));
#111683=CARTESIAN_POINT('Ctrl Pts',(-18.0492328464613,21.2142021009902,
-0.954895725948036));
#111684=CARTESIAN_POINT('Ctrl Pts',(-18.0435808167235,21.2122611185121,
-0.955252179838339));
#111685=CARTESIAN_POINT('Ctrl Pts',(-18.0288748718741,21.2071411850671,
-0.956178936265384));
#111686=CARTESIAN_POINT('Ctrl Pts',(-18.0198341521834,21.2039245403315,
-0.956747984307098));
#111687=CARTESIAN_POINT('Ctrl Pts',(-17.9889263123131,21.1926903483604,
-0.958691292278482));
#111688=CARTESIAN_POINT('Ctrl Pts',(-17.9671693056927,21.1843733013344,
-0.960055577346037));
#111689=CARTESIAN_POINT('Ctrl Pts',(-17.7867477354959,21.1119689216963,
-0.971348978071564));
#111690=CARTESIAN_POINT('Ctrl Pts',(-17.6362548081601,21.0292222243391,
-0.980569978519324));
#111691=CARTESIAN_POINT('Ctrl Pts',(-17.4241948340607,20.8766001513782,
-0.994776638331962));
#111692=CARTESIAN_POINT('Ctrl Pts',(-17.3544796360186,20.8193328079773,
-0.999701344985896));
#111693=CARTESIAN_POINT('Ctrl Pts',(-17.2604243215597,20.7314453644377,
-1.00704506081657));
#111694=CARTESIAN_POINT('Ctrl Pts',(-17.2329451248067,20.7043228804672,
-1.00928622953275));
#111695=CARTESIAN_POINT('Ctrl Pts',(-17.2009530100053,20.670970520954,-1.01203567414906));
#111696=CARTESIAN_POINT('Ctrl Pts',(-17.1957110727717,20.665446344133,-1.01249086182849));
#111697=CARTESIAN_POINT('Ctrl Pts',(-17.1876303834867,20.6568380194722,
-1.01320009247586));
#111698=CARTESIAN_POINT('Ctrl Pts',(-17.1847707323466,20.6537734558738,
-1.01345256142014));
#111699=CARTESIAN_POINT('Ctrl Pts',(-17.1794973944048,20.6480884947147,
-1.01392092107518));
#111700=CARTESIAN_POINT('Ctrl Pts',(-17.1770812137249,20.6454704893504,
-1.01413661643034));
#111701=CARTESIAN_POINT('Ctrl Pts',(-17.1716502496337,20.6395559888072,
-1.01462392428141));
#111702=CARTESIAN_POINT('Ctrl Pts',(-17.1686393037645,20.6362560631204,
-1.01489581947224));
#111703=CARTESIAN_POINT('Ctrl Pts',(-17.1598306450122,20.6265403976705,
-1.01569629081882));
#111704=CARTESIAN_POINT('Ctrl Pts',(-17.1540618521074,20.6200987256406,
-1.01622696190097));
#111705=CARTESIAN_POINT('Ctrl Pts',(-17.1140894207959,20.5749098063458,
-1.01994813811215));
#111706=CARTESIAN_POINT('Ctrl Pts',(-17.081278129716,20.5349598601349,-1.02322979657745));
#111707=CARTESIAN_POINT('Ctrl Pts',(-17.036605646116,20.476317108393,-1.02798904859693));
#111708=CARTESIAN_POINT('Ctrl Pts',(-17.0235219917822,20.4585736105255,
-1.02942192098114));
#111709=CARTESIAN_POINT('Ctrl Pts',(-16.9840406604591,20.4032419330316,
-1.03386143163218));
#111710=CARTESIAN_POINT('Ctrl Pts',(-16.958587554632,20.3649969545664,-1.03688966893136));
#111711=CARTESIAN_POINT('Ctrl Pts',(-16.8768044647256,20.2329944378632,
-1.0471474763071));
#111712=CARTESIAN_POINT('Ctrl Pts',(-16.8264950004093,20.1357032123579,
-1.05437846374188));
#111713=CARTESIAN_POINT('Ctrl Pts',(-16.7624917997307,19.984225277447,-1.06494833635042));
#111714=CARTESIAN_POINT('Ctrl Pts',(-16.7430437086544,19.9326756746082,
-1.06843562985732));
#111715=CARTESIAN_POINT('Ctrl Pts',(-16.7147841280757,19.8478924823877,
-1.07399054196894));
#111716=CARTESIAN_POINT('Ctrl Pts',(-16.704732821792,19.8151023978544,-1.07609656105327));
#111717=CARTESIAN_POINT('Ctrl Pts',(-16.6925670134059,19.7716756027844,
-1.07883211206632));
#111718=CARTESIAN_POINT('Ctrl Pts',(-16.6897316546778,19.761247861793,-1.07948496914327));
#111719=CARTESIAN_POINT('Ctrl Pts',(-16.6852176273085,19.7441297747803,
-1.08055025475023));
#111720=CARTESIAN_POINT('Ctrl Pts',(-16.6834916170951,19.7374522208109,
-1.08096421211433));
#111721=CARTESIAN_POINT('Ctrl Pts',(-16.680213173264,19.7245078873784,-1.08176361527494));
#111722=CARTESIAN_POINT('Ctrl Pts',(-16.6786567155513,19.7182422148946,
-1.08214918730627));
#111723=CARTESIAN_POINT('Ctrl Pts',(-16.6751283415835,19.7037554830237,
-1.08303752944692));
#111724=CARTESIAN_POINT('Ctrl Pts',(-16.6731769512605,19.6955295004719,
-1.08353963339714));
#111725=CARTESIAN_POINT('Ctrl Pts',(-16.6680598863212,19.6733685164413,
-1.08488620753554));
#111726=CARTESIAN_POINT('Ctrl Pts',(-16.664985905864,19.659412635284,-1.08572773572183));
#111727=CARTESIAN_POINT('Ctrl Pts',(-16.6380608209679,19.5309965610869,
-1.09341431787822));
#111728=CARTESIAN_POINT('Ctrl Pts',(-16.6235871599688,19.4147688836979,
-1.09994216807236));
#111729=CARTESIAN_POINT('Ctrl Pts',(-16.6120973758036,19.1351849122773,
-1.11526010212648));
#111730=CARTESIAN_POINT('Ctrl Pts',(-16.6242137323605,18.972235145299,-1.12386691866123));
#111731=CARTESIAN_POINT('Ctrl Pts',(-16.6609680655026,18.7805676774271,
-1.13507496762888));
#111732=CARTESIAN_POINT('Ctrl Pts',(-16.6677798930822,18.7489744611762,
-1.13696011689814));
#111733=CARTESIAN_POINT('Ctrl Pts',(-16.6769959440115,18.7105246992441,
-1.13931436159752));
#111734=CARTESIAN_POINT('Ctrl Pts',(-16.6787161466169,18.7035066585481,
-1.13974653461169));
#111735=CARTESIAN_POINT('Ctrl Pts',(-16.6814701959169,18.6925144501394,
-1.14042750463657));
#111736=CARTESIAN_POINT('Ctrl Pts',(-16.6824797534705,18.6885341738594,
-1.14067492227184));
#111737=CARTESIAN_POINT('Ctrl Pts',(-16.6843891984449,18.6810968739097,
-1.14113884384032));
#111738=CARTESIAN_POINT('Ctrl Pts',(-16.6852862576736,18.6776391819487,
-1.14135518358945));
#111739=CARTESIAN_POINT('Ctrl Pts',(-16.6873549154763,18.6697478147095,
-1.14185041999644));
#111740=CARTESIAN_POINT('Ctrl Pts',(-16.6885321679357,18.6653156799367,
-1.14212964011229));
#111741=CARTESIAN_POINT('Ctrl Pts',(-16.6921981560382,18.6516924817732,
-1.14299111899549));
#111742=CARTESIAN_POINT('Ctrl Pts',(-16.6947344695324,18.6425145046581,
-1.14357603093432));
#111743=CARTESIAN_POINT('Ctrl Pts',(-16.7185345291006,18.5586001020669,
-1.1489634870136));
#111744=CARTESIAN_POINT('Ctrl Pts',(-16.743833883568,18.4850779475505,-1.15397035239638));
#111745=CARTESIAN_POINT('Ctrl Pts',(-16.7885262290105,18.3752408746039,
-1.16173151612132));
#111746=CARTESIAN_POINT('Ctrl Pts',(-16.8050338382097,18.3378156385795,
-1.16442854162162));
#111747=CARTESIAN_POINT('Ctrl Pts',(-16.8696062210673,18.2022022690548,
-1.17435060277607));
#111748=CARTESIAN_POINT('Ctrl Pts',(-16.9241744305047,18.1072917502362,
-1.18157790916052));
#111749=CARTESIAN_POINT('Ctrl Pts',(-17.0168586192068,17.9715885596055,
-1.19214010318181));
#111750=CARTESIAN_POINT('Ctrl Pts',(-17.0496456235718,17.9273854191799,
-1.19562339839137));
#111751=CARTESIAN_POINT('Ctrl Pts',(-17.1055890508072,17.8578034999957,
-1.20117279033525));
#111752=CARTESIAN_POINT('Ctrl Pts',(-17.1277042788828,17.8316243227604,
-1.20327718171052));
#111753=CARTESIAN_POINT('Ctrl Pts',(-17.1576168939423,17.7979104643993,
-1.20601104221214));
#111754=CARTESIAN_POINT('Ctrl Pts',(-17.1648493365256,17.7898835604415,
-1.206663793652));
#111755=CARTESIAN_POINT('Ctrl Pts',(-17.1767991192414,17.7768235844802,
-1.20772900343561));
#111756=CARTESIAN_POINT('Ctrl Pts',(-17.1814801023337,17.7717576496746,
-1.20814298933927));
#111757=CARTESIAN_POINT('Ctrl Pts',(-17.190591363699,17.7619932775971,-1.20894251483392));
#111758=CARTESIAN_POINT('Ctrl Pts',(-17.1950185401579,17.7572920623917,
-1.20932818032899));
#111759=CARTESIAN_POINT('Ctrl Pts',(-17.2052937035856,17.7464804224071,
-1.21021683459015));
#111760=CARTESIAN_POINT('Ctrl Pts',(-17.2111569614164,17.7403846128733,
-1.21071915639667));
#111761=CARTESIAN_POINT('Ctrl Pts',(-17.2270311478431,17.7240775543239,
-1.21206653225809));
#111762=CARTESIAN_POINT('Ctrl Pts',(-17.2371093742525,17.713932215858,-1.21290864003686));
#111763=CARTESIAN_POINT('Ctrl Pts',(-17.3310033182662,17.6213092191099,
-1.22063513862648));
#111764=CARTESIAN_POINT('Ctrl Pts',(-17.4214564833862,17.5458419534176,
-1.22719844412912));
#111765=CARTESIAN_POINT('Ctrl Pts',(-17.6516587521603,17.3842528929774,
-1.24259191487288));
#111766=CARTESIAN_POINT('Ctrl Pts',(-17.7960287792519,17.3060944366576,
-1.25123873227028));
#111767=CARTESIAN_POINT('Ctrl Pts',(-17.9767198091943,17.2338362009708,
-1.26243143158562));
#111768=CARTESIAN_POINT('Ctrl Pts',(-18.0057508762016,17.2229600203372,
-1.26424162530969));
#111769=CARTESIAN_POINT('Ctrl Pts',(-18.0417424947828,17.2103702386494,
-1.26651246501864));
#111770=CARTESIAN_POINT('Ctrl Pts',(-18.0484882642279,17.2080487893232,
-1.26693921807486));
#111771=CARTESIAN_POINT('Ctrl Pts',(-18.0591164756236,17.2044512391706,
-1.2676135606256));
#111772=CARTESIAN_POINT('Ctrl Pts',(-18.0629911707342,17.2031521841886,
-1.26785981548969));
#111773=CARTESIAN_POINT('Ctrl Pts',(-18.0702630935823,17.2007375532514,
-1.26832279388764));
#111774=CARTESIAN_POINT('Ctrl Pts',(-18.0736593943947,17.1996193623134,
-1.26853936072229));
#111775=CARTESIAN_POINT('Ctrl Pts',(-18.0814483277144,17.1970768040885,
-1.2690367849795));
#111776=CARTESIAN_POINT('Ctrl Pts',(-18.0858427856537,17.1956582055167,
-1.26931797660527));
#111777=CARTESIAN_POINT('Ctrl Pts',(-18.0994689238567,17.191308655185,-1.27019150285857));
#111778=CARTESIAN_POINT('Ctrl Pts',(-18.1087159515204,17.1884267218595,
-1.27078659716504));
#111779=CARTESIAN_POINT('Ctrl Pts',(-18.2199199388366,17.154604307949,-1.27796792724048));
#111780=CARTESIAN_POINT('Ctrl Pts',(-18.3240413118227,17.1313437695978,
-1.28493417481822));
#111781=CARTESIAN_POINT('Ctrl Pts',(-18.5377573258039,17.1002762461415,
-1.29918061398552));
#111782=CARTESIAN_POINT('Ctrl Pts',(-18.6471234135829,17.0929534442292,
-1.3064404179305));
#111783=CARTESIAN_POINT('Ctrl Pts',(-18.8191816468751,17.0947878546033,
-1.31756393534099));
#111784=CARTESIAN_POINT('Ctrl Pts',(-18.881737767282,17.0982329799035,-1.32154887540623));
#111785=CARTESIAN_POINT('Ctrl Pts',(-18.968826740589,17.1069170190539,-1.32700390271539));
#111786=CARTESIAN_POINT('Ctrl Pts',(-18.9935547201064,17.1098240868105,
-1.32854246794858));
#111787=CARTESIAN_POINT('Ctrl Pts',(-19.0367600611059,17.1156777949324,
-1.33121312760618));
#111788=CARTESIAN_POINT('Ctrl Pts',(-19.0552599654708,17.1184343815603,
-1.33235100316907));
#111789=CARTESIAN_POINT('Ctrl Pts',(-19.0821458078013,17.1228054824148,
-1.33399684596642));
#111790=CARTESIAN_POINT('Ctrl Pts',(-19.0905619617199,17.1242260741639,
-1.33451092929524));
#111791=CARTESIAN_POINT('Ctrl Pts',(-19.1053191105548,17.1268088686221,
-1.3354104383561));
#111792=CARTESIAN_POINT('Ctrl Pts',(-19.1116637739917,17.1279492014793,
-1.33579655352527));
#111793=CARTESIAN_POINT('Ctrl Pts',(-19.1239855686781,17.1302219573573,
-1.33654525053515));
#111794=CARTESIAN_POINT('Ctrl Pts',(-19.1299632158707,17.1313511980657,
-1.33690792949389));
#111795=CARTESIAN_POINT('Ctrl Pts',(-19.1442608149774,17.1341160459722,
-1.33777416058269));
#111796=CARTESIAN_POINT('Ctrl Pts',(-19.1525760123578,17.1357759109289,
-1.33827693555516));
#111797=CARTESIAN_POINT('Ctrl Pts',(-19.1826607657826,17.141969556595,-1.34009252945942));
#111798=CARTESIAN_POINT('Ctrl Pts',(-19.2043690043141,17.1467963972756,
-1.34139599484094));
#111799=CARTESIAN_POINT('Ctrl Pts',(-19.4052505677662,17.1947961940575,
-1.35340661079202));
#111800=CARTESIAN_POINT('Ctrl Pts',(-19.578138660735,17.2608484261107,-1.36327116938842));
#111801=CARTESIAN_POINT('Ctrl Pts',(-19.8115611527497,17.3869628521163,
-1.3777304877114));
#111802=CARTESIAN_POINT('Ctrl Pts',(-19.8805489176555,17.429519413392,-1.38218222351613));
#111803=CARTESIAN_POINT('Ctrl Pts',(-19.9766417376677,17.4966939345755,
-1.38888709278125));
#111804=CARTESIAN_POINT('Ctrl Pts',(-20.005819439317,17.5182275010892,-1.39099582174232));
#111805=CARTESIAN_POINT('Ctrl Pts',(-20.0403302155074,17.5450929441108,
-1.39359845490154));
#111806=CARTESIAN_POINT('Ctrl Pts',(-20.0462081306796,17.5497189374463,
-1.39404564302806));
#111807=CARTESIAN_POINT('Ctrl Pts',(-20.0553184366203,17.5569673782921,
-1.3947450683031));
#111808=CARTESIAN_POINT('Ctrl Pts',(-20.058567884312,17.5595684259435,-1.39499580052242));
#111809=CARTESIAN_POINT('Ctrl Pts',(-20.0645866224007,17.5644153670785,
-1.39546260918367));
#111810=CARTESIAN_POINT('Ctrl Pts',(-20.0673579172715,17.5666586799171,
-1.39567850094296));
#111811=CARTESIAN_POINT('Ctrl Pts',(-20.0736189729604,17.571753125808,-1.39616840971934));
#111812=CARTESIAN_POINT('Ctrl Pts',(-20.0771052872768,17.5746083923203,
-1.39644272284676));
#111813=CARTESIAN_POINT('Ctrl Pts',(-20.0873944228759,17.5830901522574,
-1.39725674035497));
#111814=CARTESIAN_POINT('Ctrl Pts',(-20.0941710972335,17.5887480108595,
-1.39779864466668));
#111815=CARTESIAN_POINT('Ctrl Pts',(-20.1437891457519,17.630703671618,-1.40180783895269));
#111816=CARTESIAN_POINT('Ctrl Pts',(-20.1852029484385,17.6686476611607,
-1.4053826159621));
#111817=CARTESIAN_POINT('Ctrl Pts',(-20.2694058430704,17.7521918859532,
-1.41306229560888));
#111818=CARTESIAN_POINT('Ctrl Pts',(-20.311784641918,17.7981350999428,-1.41717759412954));
#111819=CARTESIAN_POINT('Ctrl Pts',(-20.4227518524972,17.9296641046729,
-1.42854454226548));
#111820=CARTESIAN_POINT('Ctrl Pts',(-20.4868272563151,18.0188152136544,
-1.43579415293509));
#111821=CARTESIAN_POINT('Ctrl Pts',(-20.5724488815152,18.1598759155566,
-1.44640315108994));
#111822=CARTESIAN_POINT('Ctrl Pts',(-20.5993182114281,18.2083310946217,
-1.44991079691162));
#111823=CARTESIAN_POINT('Ctrl Pts',(-20.6397608263552,18.2885304252743,
-1.45549437506563));
#111824=CARTESIAN_POINT('Ctrl Pts',(-20.6545119656725,18.3196479640476,
-1.45760919717485));
#111825=CARTESIAN_POINT('Ctrl Pts',(-20.6728942765733,18.3610028708258,
-1.46035438236236));
#111826=CARTESIAN_POINT('Ctrl Pts',(-20.677214501923,18.3709264665149,-1.46100827245335));
#111827=CARTESIAN_POINT('Ctrl Pts',(-20.6841645614341,18.3872313378617,
-1.46207484230072));
#111828=CARTESIAN_POINT('Ctrl Pts',(-20.6868395896257,18.3935930240452,
-1.46248905750794));
#111829=CARTESIAN_POINT('Ctrl Pts',(-20.6919565570171,18.4059305668096,
-1.46328868198003));
#111830=CARTESIAN_POINT('Ctrl Pts',(-20.6944023615243,18.4119047279714,
-1.46367421894243));
#111831=CARTESIAN_POINT('Ctrl Pts',(-20.6999852446905,18.4257214744577,
-1.4645620858008));
#111832=CARTESIAN_POINT('Ctrl Pts',(-20.7031028026407,18.4335718677551,
-1.46506375223575));
#111833=CARTESIAN_POINT('Ctrl Pts',(-20.7113578706468,18.4547273875365,
-1.46640827990993));
#111834=CARTESIAN_POINT('Ctrl Pts',(-20.7164081046749,18.4680662651916,
-1.46724821401887));
#111835=CARTESIAN_POINT('Ctrl Pts',(-20.7217433674324,18.4825998411213,
-1.46815522842632));
#111836=CARTESIAN_POINT('Ctrl Pts',(-20.7221624896271,18.4837446109271,
-1.46822661684574));
#111837=CARTESIAN_POINT('Ctrl Pts',(-20.7225806136401,18.4848897170162,
-1.46829797183507));
#111838=CARTESIAN_POINT('',(-20.8509993841467,19.2126147825168,-0.48905627896718));
#111839=CARTESIAN_POINT('Ctrl Pts',(-20.7225806756345,18.4848898867987,
-1.24458630806144));
#111840=CARTESIAN_POINT('Ctrl Pts',(-20.6661824054662,18.3304332718076,
-1.23372069736793));
#111841=CARTESIAN_POINT('Ctrl Pts',(-20.5919348586647,18.1829508307763,
-1.22298094813775));
#111842=CARTESIAN_POINT('Ctrl Pts',(-20.4894887237695,18.0276123060087,
-1.21154561110675));
#111843=CARTESIAN_POINT('Ctrl Pts',(-20.4774345686897,18.0099242109399,
-1.21024038985349));
#111844=CARTESIAN_POINT('Ctrl Pts',(-20.4603099945566,17.9855970243815,
-1.20844033487475));
#111845=CARTESIAN_POINT('Ctrl Pts',(-20.4554657382646,17.9788010042766,
-1.20793692583058));
#111846=CARTESIAN_POINT('Ctrl Pts',(-20.4470415660747,17.9671293572218,
-1.20707135210583));
#111847=CARTESIAN_POINT('Ctrl Pts',(-20.443480736494,17.9622401368551,-1.20670845761028));
#111848=CARTESIAN_POINT('Ctrl Pts',(-20.4360700664556,17.9521559683733,
-1.2059593064324));
#111849=CARTESIAN_POINT('Ctrl Pts',(-20.432217277546,17.9469632573528,-1.2055731695855));
#111850=CARTESIAN_POINT('Ctrl Pts',(-20.4231497435379,17.9348585065408,
-1.20467212634334));
#111851=CARTESIAN_POINT('Ctrl Pts',(-20.4179162397047,17.9279606130451,
-1.2041579608589));
#111852=CARTESIAN_POINT('Ctrl Pts',(-20.4008334404141,17.9057296134496,
-1.20249840406264));
#111853=CARTESIAN_POINT('Ctrl Pts',(-20.3888156884135,17.8905267612099,
-1.201359675248));
#111854=CARTESIAN_POINT('Ctrl Pts',(-20.3265598744795,17.813956113538,-1.19560103161039));
#111855=CARTESIAN_POINT('Ctrl Pts',(-20.2731079112592,17.7552777134216,
-1.19111372096945));
#111856=CARTESIAN_POINT('Ctrl Pts',(-20.1000689467924,17.5855344376121,
-1.17766518008992));
#111857=CARTESIAN_POINT('Ctrl Pts',(-19.9708586354561,17.4851791348537,
-1.16906415688845));
#111858=CARTESIAN_POINT('Ctrl Pts',(-19.779177507349,17.3689833967405,-1.15653489955564));
#111859=CARTESIAN_POINT('Ctrl Pts',(-19.7255937634343,17.3395937027378,
-1.1530484463857));
#111860=CARTESIAN_POINT('Ctrl Pts',(-19.6626471361593,17.3085314559998,
-1.14888528194358));
#111861=CARTESIAN_POINT('Ctrl Pts',(-19.6544483243733,17.3045512228687,
-1.14834174356928));
#111862=CARTESIAN_POINT('Ctrl Pts',(-19.6421586674782,17.2986827845872,
-1.14752471290199));
#111863=CARTESIAN_POINT('Ctrl Pts',(-19.6380869564036,17.2967544378846,
-1.14725364736495));
#111864=CARTESIAN_POINT('Ctrl Pts',(-19.6307808095641,17.2933227849416,
-1.14676653356237));
#111865=CARTESIAN_POINT('Ctrl Pts',(-19.6275487043282,17.2918146430695,
-1.14655078837474));
#111866=CARTESIAN_POINT('Ctrl Pts',(-19.6205325734518,17.2885623920429,
-1.14608189277962));
#111867=CARTESIAN_POINT('Ctrl Pts',(-19.6167472553636,17.2868213069632,
-1.14582856644096));
#111868=CARTESIAN_POINT('Ctrl Pts',(-19.6061409649053,17.2819807491722,
-1.14511783251206));
#111869=CARTESIAN_POINT('Ctrl Pts',(-19.5993087209995,17.2789063308839,
-1.14465893236172));
#111870=CARTESIAN_POINT('Ctrl Pts',(-19.5591798241623,17.2611044057851,
-1.14195798477386));
#111871=CARTESIAN_POINT('Ctrl Pts',(-19.525526141534,17.2472025131218,-1.1396703469668));
#111872=CARTESIAN_POINT('Ctrl Pts',(-19.4153877701052,17.2049966891448,
-1.13214940977712));
#111873=CARTESIAN_POINT('Ctrl Pts',(-19.3376248017066,17.1802430185681,
-1.12678928356071));
#111874=CARTESIAN_POINT('Ctrl Pts',(-19.0810914400379,17.1146220679987,
-1.10930521312209));
#111875=CARTESIAN_POINT('Ctrl Pts',(-18.89836296349,17.0924428681064,-1.09724057977298));
#111876=CARTESIAN_POINT('Ctrl Pts',(-18.6927243429773,17.0942847882105,
-1.08459114743813));
#111877=CARTESIAN_POINT('Ctrl Pts',(-18.6704139674967,17.0948374722266,
-1.08322948011463));
#111878=CARTESIAN_POINT('Ctrl Pts',(-18.6396296031995,17.096087386524,-1.08136478133196));
#111879=CARTESIAN_POINT('Ctrl Pts',(-18.6311454516231,17.0964830150604,
-1.08085235508817));
#111880=CARTESIAN_POINT('Ctrl Pts',(-18.6165836652113,17.0972499024122,
-1.07997533804089));
#111881=CARTESIAN_POINT('Ctrl Pts',(-18.6105048786102,17.0975963407516,
-1.07960997350805));
#111882=CARTESIAN_POINT('Ctrl Pts',(-18.5979923136674,17.0983636190374,
-1.07885940979585));
#111883=CARTESIAN_POINT('Ctrl Pts',(-18.5915587881476,17.0987876357967,
-1.07847431431837));
#111884=CARTESIAN_POINT('Ctrl Pts',(-18.5766192677292,17.0998408277616,
-1.0775819258605));
#111885=CARTESIAN_POINT('Ctrl Pts',(-18.5681149000994,17.1004920321651,
-1.07707532954861));
#111886=CARTESIAN_POINT('Ctrl Pts',(-18.5410181716267,17.1027317049662,
-1.07546550415896));
#111887=CARTESIAN_POINT('Ctrl Pts',(-18.5224424531343,17.1045146268516,
-1.07436838052141));
#111888=CARTESIAN_POINT('Ctrl Pts',(-18.3441708847962,17.1240073808989,
-1.06389542661839));
#111889=CARTESIAN_POINT('Ctrl Pts',(-18.1869536833619,17.1595972059036,
-1.05514807854796));
#111890=CARTESIAN_POINT('Ctrl Pts',(-17.908489155771,17.2569640080484,-1.0391283317762));
#111891=CARTESIAN_POINT('Ctrl Pts',(-17.7862402686981,17.3132470157437,
-1.03186578695907));
#111892=CARTESIAN_POINT('Ctrl Pts',(-17.6566074513414,17.3885949576223,
-1.0230744383104));
#111893=CARTESIAN_POINT('Ctrl Pts',(-17.6431400224009,17.3966242618457,
-1.02214692552163));
#111894=CARTESIAN_POINT('Ctrl Pts',(-17.6248243605882,17.4078217188635,
-1.02086420744213));
#111895=CARTESIAN_POINT('Ctrl Pts',(-17.6198977230591,17.4108614977312,
-1.02051703991936));
#111896=CARTESIAN_POINT('Ctrl Pts',(-17.6120880690931,17.415724462686,-1.0199632086467));
#111897=CARTESIAN_POINT('Ctrl Pts',(-17.6091968426527,17.4175345020241,
-1.01975740602113));
#111898=CARTESIAN_POINT('Ctrl Pts',(-17.6032369544812,17.4212857434948,
-1.01933155605172));
#111899=CARTESIAN_POINT('Ctrl Pts',(-17.600168920238,17.4232278481787,-1.0191114457333));
#111900=CARTESIAN_POINT('Ctrl Pts',(-17.5928702715098,17.4278743300661,
-1.01858571433786));
#111901=CARTESIAN_POINT('Ctrl Pts',(-17.5886442674297,17.4305858749448,
-1.01827962018844));
#111902=CARTESIAN_POINT('Ctrl Pts',(-17.5744201016722,17.439784174264,-1.01724374439948));
#111903=CARTESIAN_POINT('Ctrl Pts',(-17.5644672952418,17.4463401802521,
-1.01650955102563));
#111904=CARTESIAN_POINT('Ctrl Pts',(-17.540688822463,17.4622927997074,-1.01473383619391));
#111905=CARTESIAN_POINT('Ctrl Pts',(-17.5269182498908,17.4717696959647,
-1.01368766859242));
#111906=CARTESIAN_POINT('Ctrl Pts',(-17.4756936471639,17.5079237954973,
-1.00973299998004));
#111907=CARTESIAN_POINT('Ctrl Pts',(-17.4390016859435,17.5356545857966,
-1.0067721880836));
#111908=CARTESIAN_POINT('Ctrl Pts',(-17.345430048465,17.6112848533801,-0.998936010096704));
#111909=CARTESIAN_POINT('Ctrl Pts',(-17.2901188588802,17.6610252389756,
-0.994012843500479));
#111910=CARTESIAN_POINT('Ctrl Pts',(-17.1277334247407,17.8233055054867,
-0.978845963952766));
#111911=CARTESIAN_POINT('Ctrl Pts',(-17.030311472297,17.9448047966296,-0.968729742295685));
#111912=CARTESIAN_POINT('Ctrl Pts',(-16.9342093851213,18.0960938136812,
-0.957687436261378));
#111913=CARTESIAN_POINT('Ctrl Pts',(-16.9217169768475,18.1165173004625,
-0.95622518042325));
#111914=CARTESIAN_POINT('Ctrl Pts',(-16.9046536568069,18.1455071477022,
-0.954188351445424));
#111915=CARTESIAN_POINT('Ctrl Pts',(-16.8997914923099,18.1538991453648,
-0.953603205203594));
#111916=CARTESIAN_POINT('Ctrl Pts',(-16.8920195688184,18.167528400318,-0.952660008442099));
#111917=CARTESIAN_POINT('Ctrl Pts',(-16.8890741112461,18.172745043666,-0.952300670527777));
#111918=CARTESIAN_POINT('Ctrl Pts',(-16.8829818529425,18.1836427135349,
-0.951553456524428));
#111919=CARTESIAN_POINT('Ctrl Pts',(-16.8798389663413,18.1893258653065,
-0.951165723964566));
#111920=CARTESIAN_POINT('Ctrl Pts',(-16.8724720934962,18.2027930352354,
-0.950251454980925));
#111921=CARTESIAN_POINT('Ctrl Pts',(-16.8682706810135,18.2105893131313,
-0.949725728885034));
#111922=CARTESIAN_POINT('Ctrl Pts',(-16.8544954966124,18.2365396177502,
-0.947987380311746));
#111923=CARTESIAN_POINT('Ctrl Pts',(-16.8451366114532,18.2548068406588,
-0.946782362737516));
#111924=CARTESIAN_POINT('Ctrl Pts',(-16.7969195895766,18.3523910957784,
-0.940438786218297));
#111925=CARTESIAN_POINT('Ctrl Pts',(-16.7627857120895,18.4339500893872,
-0.935466697220141));
#111926=CARTESIAN_POINT('Ctrl Pts',(-16.6909608146935,18.6410770511559,
-0.923366002619506));
#111927=CARTESIAN_POINT('Ctrl Pts',(-16.6596403026142,18.7684487036692,
-0.916388592646102));
#111928=CARTESIAN_POINT('Ctrl Pts',(-16.6347040122347,18.935195888883,-0.907088387874391));
#111929=CARTESIAN_POINT('Ctrl Pts',(-16.6301237574798,18.9726387674235,
-0.904988041061026));
#111930=CARTESIAN_POINT('Ctrl Pts',(-16.6221951274404,19.0558447166839,
-0.900256665875105));
#111931=CARTESIAN_POINT('Ctrl Pts',(-16.6193295473621,19.1016328096204,
-0.89761039489276));
#111932=CARTESIAN_POINT('Ctrl Pts',(-16.6177244726638,19.1550977082651,
-0.894433886191191));
#111933=CARTESIAN_POINT('Ctrl Pts',(-16.6175368056639,19.1627225013456,
-0.893978822287519));
#111934=CARTESIAN_POINT('Ctrl Pts',(-16.6173018807339,19.1749542369422,
-0.893245278152376));
#111935=CARTESIAN_POINT('Ctrl Pts',(-16.6172284502246,19.1795606889306,
-0.892968224132206));
#111936=CARTESIAN_POINT('Ctrl Pts',(-16.6171246645964,19.1877483284721,
-0.89247429639216));
#111937=CARTESIAN_POINT('Ctrl Pts',(-16.6170883596882,19.1913293927005,
-0.892257758631505));
#111938=CARTESIAN_POINT('Ctrl Pts',(-16.6170304167432,19.1989531423377,
-0.891795673294241));
#111939=CARTESIAN_POINT('Ctrl Pts',(-16.6170112720165,19.2029957403879,
-0.891549994801778));
#111940=CARTESIAN_POINT('Ctrl Pts',(-16.6169907240015,19.2139759740558,
-0.890880975854258));
#111941=CARTESIAN_POINT('Ctrl Pts',(-16.6170118446434,19.2209135304453,
-0.890456406001248));
#111942=CARTESIAN_POINT('Ctrl Pts',(-16.6172932451306,19.2562654351253,
-0.888283820471431));
#111943=CARTESIAN_POINT('Ctrl Pts',(-16.6180914884379,19.2846711116209,
-0.88650820891694));
#111944=CARTESIAN_POINT('Ctrl Pts',(-16.6221165596621,19.368072710525,-0.881223467570355));
#111945=CARTESIAN_POINT('Ctrl Pts',(-16.6269184270536,19.422966778176,-0.877654128152968));
#111946=CARTESIAN_POINT('Ctrl Pts',(-16.6514759837071,19.6164141724189,
-0.864883257524241));
#111947=CARTESIAN_POINT('Ctrl Pts',(-16.6828174660238,19.7531458382776,
-0.855531879975794));
#111948=CARTESIAN_POINT('Ctrl Pts',(-16.75623907893,19.9714761807052,-0.840658246436459));
#111949=CARTESIAN_POINT('Ctrl Pts',(-16.7905179086766,20.0552413071479,
-0.83495965037874));
#111950=CARTESIAN_POINT('Ctrl Pts',(-16.8360572771144,20.1489184453406,
-0.828604162730233));
#111951=CARTESIAN_POINT('Ctrl Pts',(-16.8421814937466,20.161210683379,-0.827770418694047));
#111952=CARTESIAN_POINT('Ctrl Pts',(-16.8521957805494,20.1808302295515,
-0.826439833355268));
#111953=CARTESIAN_POINT('Ctrl Pts',(-16.8560099818797,20.1881956249345,
-0.825940349688879));
#111954=CARTESIAN_POINT('Ctrl Pts',(-16.8628597152704,20.2012345346307,
-0.825056113301347));
#111955=CARTESIAN_POINT('Ctrl Pts',(-16.8658779937436,20.2069169492838,
-0.824670757756287));
#111956=CARTESIAN_POINT('Ctrl Pts',(-16.8722212273066,20.2187288451307,
-0.823869686996268));
#111957=CARTESIAN_POINT('Ctrl Pts',(-16.8755506590548,20.2248558441353,
-0.823454136657031));
#111958=CARTESIAN_POINT('Ctrl Pts',(-16.8842769218857,20.2407269561538,
-0.822377583909497));
#111959=CARTESIAN_POINT('Ctrl Pts',(-16.8897205356042,20.2504452050555,
-0.821718259363182));
#111960=CARTESIAN_POINT('Ctrl Pts',(-16.9137060550737,20.292483856465,-0.818865114800046));
#111961=CARTESIAN_POINT('Ctrl Pts',(-16.9330234058495,20.3243557089529,
-0.816699363238438));
#111962=CARTESIAN_POINT('Ctrl Pts',(-16.9865976866517,20.4077018411699,
-0.811013100648686));
#111963=CARTESIAN_POINT('Ctrl Pts',(-17.0222854735611,20.458214648653,-0.807543735795336));
#111964=CARTESIAN_POINT('Ctrl Pts',(-17.1467825047545,20.618998401745,-0.796293123111812));
#111965=CARTESIAN_POINT('Ctrl Pts',(-17.2444281536335,20.7219243089349,
-0.788770462594634));
#111966=CARTESIAN_POINT('Ctrl Pts',(-17.409019288528,20.8638342901307,-0.776740250899853));
#111967=CARTESIAN_POINT('Ctrl Pts',(-17.4690404527405,20.9102085893253,
-0.772457516937216));
#111968=CARTESIAN_POINT('Ctrl Pts',(-17.5392367700206,20.958661364388,-0.767402546046644));
#111969=CARTESIAN_POINT('Ctrl Pts',(-17.5470986426051,20.9640101484255,
-0.766835764205138));
#111970=CARTESIAN_POINT('Ctrl Pts',(-17.5588058980946,20.9718602622615,
-0.765990401295918));
#111971=CARTESIAN_POINT('Ctrl Pts',(-17.5626239318698,20.974402434633,-0.765714494738421));
#111972=CARTESIAN_POINT('Ctrl Pts',(-17.5694371352572,20.9789069987217,
-0.765221710979636));
#111973=CARTESIAN_POINT('Ctrl Pts',(-17.5724290490476,20.9808742180346,
-0.765005161598151));
#111974=CARTESIAN_POINT('Ctrl Pts',(-17.5788815519957,20.9850934072501,
-0.764537805093699));
#111975=CARTESIAN_POINT('Ctrl Pts',(-17.5823436982332,20.987342818405,-0.764286838985219));
#111976=CARTESIAN_POINT('Ctrl Pts',(-17.5919269215151,20.9935293973991,
-0.763591657213845));
#111977=CARTESIAN_POINT('Ctrl Pts',(-17.5980616885217,20.9974451064006,
-0.76314606220414));
#111978=CARTESIAN_POINT('Ctrl Pts',(-17.6319343511103,21.0188203827484,
-0.760683153329686));
#111979=CARTESIAN_POINT('Ctrl Pts',(-17.6600530322491,21.0356645905723,
-0.758629155280327));
#111980=CARTESIAN_POINT('Ctrl Pts',(-17.8308675921068,21.1326732237587,
-0.746147031498064));
#111981=CARTESIAN_POINT('Ctrl Pts',(-17.9820744812969,21.1967201331268,
-0.735129536852101));
#111982=CARTESIAN_POINT('Ctrl Pts',(-18.2489484650775,21.274856427027,-0.716988808393646));
#111983=CARTESIAN_POINT('Ctrl Pts',(-18.3611862289954,21.2980542769874,
-0.709709002545072));
#111984=CARTESIAN_POINT('Ctrl Pts',(-18.4889250262089,21.3138149699519,
-0.701850632073147));
#111985=CARTESIAN_POINT('Ctrl Pts',(-18.5031019853212,21.3154188421148,
-0.700984062011824));
#111986=CARTESIAN_POINT('Ctrl Pts',(-18.525708393466,21.3177451560251,-0.699610903005511));
#111987=CARTESIAN_POINT('Ctrl Pts',(-18.5341276420099,21.318560577904,-0.699101409450835));
#111988=CARTESIAN_POINT('Ctrl Pts',(-18.548995169212,21.3199106367754,-0.698204998522658));
#111989=CARTESIAN_POINT('Ctrl Pts',(-18.5554413934681,21.3204662089711,
-0.6978174289666));
#111990=CARTESIAN_POINT('Ctrl Pts',(-18.5687896234043,21.3215550102637,
-0.697017111803055));
#111991=CARTESIAN_POINT('Ctrl Pts',(-18.5756919082355,21.3220839561022,
-0.696604502964991));
#111992=CARTESIAN_POINT('Ctrl Pts',(-18.5934372164303,21.3233563203803,
-0.695546808775368));
#111993=CARTESIAN_POINT('Ctrl Pts',(-18.604283679647,21.3240501184931,-0.694903282781177));
#111994=CARTESIAN_POINT('Ctrl Pts',(-18.6497615255562,21.3266076329172,
-0.692217031230371));
#111995=CARTESIAN_POINT('Ctrl Pts',(-18.6844318494821,21.3277038002833,
-0.690198340680983));
#111996=CARTESIAN_POINT('Ctrl Pts',(-18.7749971102932,21.3283405967756,
-0.684989197299901));
#111997=CARTESIAN_POINT('Ctrl Pts',(-18.8308754223719,21.326520689323,-0.681839342417253));
#111998=CARTESIAN_POINT('Ctrl Pts',(-19.0845510728595,21.30818490816,-0.66770526995044));
#111999=CARTESIAN_POINT('Ctrl Pts',(-19.2794566785421,21.2661224384763,
-0.657394742607753));
#112000=CARTESIAN_POINT('Ctrl Pts',(-19.4955732415967,21.1865286229346,
-0.644170573043048));
#112001=CARTESIAN_POINT('Ctrl Pts',(-19.5252605407747,21.1748262786256,
-0.642310020563612));
#112002=CARTESIAN_POINT('Ctrl Pts',(-19.560955550427,21.1598150271161,-0.640006098716338));
#112003=CARTESIAN_POINT('Ctrl Pts',(-19.5672279888995,21.157141466583,-0.639598706187977));
#112004=CARTESIAN_POINT('Ctrl Pts',(-19.5775392164593,21.152687428939,-0.638924629426782));
#112005=CARTESIAN_POINT('Ctrl Pts',(-19.5815856015658,21.1509245162147,
-0.638658991695032));
#112006=CARTESIAN_POINT('Ctrl Pts',(-19.5888765445898,21.1477208617822,
-0.638178292201905));
#112007=CARTESIAN_POINT('Ctrl Pts',(-19.5921230212778,21.1462846000402,
-0.637963506611658));
#112008=CARTESIAN_POINT('Ctrl Pts',(-19.5984346187881,21.1434733051312,
-0.637544468857211));
#112009=CARTESIAN_POINT('Ctrl Pts',(-19.6015000361135,21.1420991616646,
-0.63734027919467));
#112010=CARTESIAN_POINT('Ctrl Pts',(-19.6105436869147,21.1380192592625,
-0.636735918907484));
#112011=CARTESIAN_POINT('Ctrl Pts',(-19.6165125589159,21.1352930237778,
-0.636334506879658));
#112012=CARTESIAN_POINT('Ctrl Pts',(-19.6448686053524,21.1221819423287,
-0.634415809423085));
#112013=CARTESIAN_POINT('Ctrl Pts',(-19.6670847067223,21.1114343816403,
-0.632877663218519));
#112014=CARTESIAN_POINT('Ctrl Pts',(-19.7292835658204,21.0799907256176,
-0.628482435917448));
#112015=CARTESIAN_POINT('Ctrl Pts',(-19.768799843259,21.0584047930099,-0.625584594246166));
#112016=CARTESIAN_POINT('Ctrl Pts',(-19.8895240320114,20.987369750416,-0.616462819794181));
#112017=CARTESIAN_POINT('Ctrl Pts',(-19.9681110295935,20.9336998229802,
-0.610137699519105));
#112018=CARTESIAN_POINT('Ctrl Pts',(-20.1606341990481,20.7822639581417,
-0.593981499477576));
#112019=CARTESIAN_POINT('Ctrl Pts',(-20.2682894328901,20.6773313239393,
-0.58430710599027));
#112020=CARTESIAN_POINT('Ctrl Pts',(-20.3729857963497,20.5510053032042,
-0.574291057872095));
#112021=CARTESIAN_POINT('Ctrl Pts',(-20.3818932676913,20.5400359087893,
-0.573432938594564));
#112022=CARTESIAN_POINT('Ctrl Pts',(-20.3959065203289,20.5224213336995,
-0.572073108101216));
#112023=CARTESIAN_POINT('Ctrl Pts',(-20.4010837091802,20.5158337467101,
-0.571568520633174));
#112024=CARTESIAN_POINT('Ctrl Pts',(-20.4101516393898,20.5041534135766,
-0.570680753598069));
#112025=CARTESIAN_POINT('Ctrl Pts',(-20.414058593238,20.4990734427706,-0.570296928178713));
#112026=CARTESIAN_POINT('Ctrl Pts',(-20.4220974030441,20.4885222745632,
-0.569504380690207));
#112027=CARTESIAN_POINT('Ctrl Pts',(-20.4262258736835,20.483048583316,-0.569095795672346));
#112028=CARTESIAN_POINT('Ctrl Pts',(-20.436766166414,20.4689317132398,-0.56804855313326));
#112029=CARTESIAN_POINT('Ctrl Pts',(-20.4431388558035,20.4602594569402,
-0.567411436815932));
#112030=CARTESIAN_POINT('Ctrl Pts',(-20.469546928276,20.4237417762547,-0.564754091978195));
#112031=CARTESIAN_POINT('Ctrl Pts',(-20.4889707980334,20.3954591389648,
-0.562757557265251));
#112032=CARTESIAN_POINT('Ctrl Pts',(-20.5378441393409,20.3204522608832,
-0.557608779161852));
#112033=CARTESIAN_POINT('Ctrl Pts',(-20.5661685036933,20.2730250583122,
-0.554496407991956));
#112034=CARTESIAN_POINT('Ctrl Pts',(-20.6274494475575,20.1606495983284,
-0.547383443430525));
#112035=CARTESIAN_POINT('Ctrl Pts',(-20.6589746514456,20.0950013682202,
-0.543420670502669));
#112036=CARTESIAN_POINT('Ctrl Pts',(-20.7006456271119,19.9953686608852,
-0.537557063547991));
#112037=CARTESIAN_POINT('Ctrl Pts',(-20.7134213668993,19.9625452447437,
-0.535648164490024));
#112038=CARTESIAN_POINT('Ctrl Pts',(-20.7392650272067,19.8909096373497,
-0.531505467693999));
#112039=CARTESIAN_POINT('Ctrl Pts',(-20.752037460671,19.8520067039789,-0.529270205292095));
#112040=CARTESIAN_POINT('Ctrl Pts',(-20.7690474666544,19.7946336295599,
-0.525964916082148));
#112041=CARTESIAN_POINT('Ctrl Pts',(-20.7741781414794,19.7764374674583,
-0.524915331532082));
#112042=CARTESIAN_POINT('Ctrl Pts',(-20.7946963209701,19.6997509089702,
-0.520477600405977));
#112043=CARTESIAN_POINT('Ctrl Pts',(-20.8078159804839,19.6406889783358,
-0.517025262311643));
#112044=CARTESIAN_POINT('Ctrl Pts',(-20.8199723679835,19.5722344460836,
-0.512901190397606));
#112045=CARTESIAN_POINT('Ctrl Pts',(-20.821498830832,19.5633062157223,-0.512360924112629));
#112046=CARTESIAN_POINT('Ctrl Pts',(-20.823694281759,19.5499496480819,-0.51154876385499));
#112047=CARTESIAN_POINT('Ctrl Pts',(-20.8244066116757,19.5455284026217,
-0.511279283813246));
#112048=CARTESIAN_POINT('Ctrl Pts',(-20.8256595644647,19.5375913647195,
-0.510794307785514));
#112049=CARTESIAN_POINT('Ctrl Pts',(-20.8262053588607,19.5340764444796,
-0.510579109141631));
#112050=CARTESIAN_POINT('Ctrl Pts',(-20.827252000903,19.5272221728641,-0.510158628847916));
#112051=CARTESIAN_POINT('Ctrl Pts',(-20.8277537164576,19.5238830074441,
-0.509953403503997));
#112052=CARTESIAN_POINT('Ctrl Pts',(-20.8288494591856,19.5164696311133,
-0.509496951442346));
#112053=CARTESIAN_POINT('Ctrl Pts',(-20.8294395919548,19.5123948705603,
-0.509245509884245));
#112054=CARTESIAN_POINT('Ctrl Pts',(-20.8308794508217,19.5022442397548,
-0.508617812015502));
#112055=CARTESIAN_POINT('Ctrl Pts',(-20.8317146529024,19.496166392462,-0.508240780882291));
#112056=CARTESIAN_POINT('Ctrl Pts',(-20.8356021105131,19.4669354473259,
-0.506422052246403));
#112057=CARTESIAN_POINT('Ctrl Pts',(-20.8382973967367,19.443737509715,-0.504962354972492));
#112058=CARTESIAN_POINT('Ctrl Pts',(-20.8474812586133,19.3513903947303,
-0.499099088402688));
#112059=CARTESIAN_POINT('Ctrl Pts',(-20.8509485244656,19.2819899972872,
-0.494577406431323));
#112060=CARTESIAN_POINT('Ctrl Pts',(-20.8509994310879,19.2125520223715,
-0.490010528127494));
#112061=CARTESIAN_POINT('Ctrl Pts',(-20.8509993841467,19.2126147825168,
-0.48905627896718));
#112062=CARTESIAN_POINT('Ctrl Pts',(-20.8510540322183,19.1409705004862,
-0.484732818607042));
#112063=CARTESIAN_POINT('Ctrl Pts',(-20.8474675455063,19.0691917009212,
-0.480409358246904));
#112064=CARTESIAN_POINT('Ctrl Pts',(-20.8402254628036,18.9976849751246,
-0.476085897886766));
#112065=CARTESIAN_POINT('Ctrl Pts',(-20.8329909785512,18.9262532747475,
-0.471766973735264));
#112066=CARTESIAN_POINT('Ctrl Pts',(-20.8221085499717,18.8550935731786,
-0.467448049583762));
#112067=CARTESIAN_POINT('Ctrl Pts',(-20.80761573801,18.7846119477787,-0.463129125432261));
#112068=CARTESIAN_POINT('Ctrl Pts',(-20.79313335316,18.714181031639,-0.458813308607625));
#112069=CARTESIAN_POINT('Ctrl Pts',(-20.7750458368668,18.6444277090544,
-0.454497491782989));
#112070=CARTESIAN_POINT('Ctrl Pts',(-20.7534422764624,18.5757505277167,
-0.450181674958354));
#112071=CARTESIAN_POINT('Ctrl Pts',(-20.7438446616878,18.5452399489996,
-0.44826432677382));
#112072=CARTESIAN_POINT('Ctrl Pts',(-20.7335537696515,18.514941633152,-0.446346978589286));
#112073=CARTESIAN_POINT('Ctrl Pts',(-20.7225806137986,18.4848897174502,
-0.444429630404752));
#112074=CARTESIAN_POINT('Origin',(18.734,19.211,0.));
#112075=CARTESIAN_POINT('',(16.6170002905278,19.2121090962232,-0.710943720977502));
#112076=CARTESIAN_POINT('Ctrl Pts',(16.7454194503191,18.4848895418526,-0.666446447912836));
#112077=CARTESIAN_POINT('Ctrl Pts',(16.7201110306304,18.55420107782,-0.670880799794245));
#112078=CARTESIAN_POINT('Ctrl Pts',(16.698402847815,18.6249128475929,-0.675315151675655));
#112079=CARTESIAN_POINT('Ctrl Pts',(16.680440926398,18.6966225790074,-0.679749503557064));
#112080=CARTESIAN_POINT('Ctrl Pts',(16.662493389734,18.7682748818904,-0.684180304200555));
#112081=CARTESIAN_POINT('Ctrl Pts',(16.6482862669931,18.8409231094069,-0.688611104844046));
#112082=CARTESIAN_POINT('Ctrl Pts',(16.6379158165232,18.9141497081386,-0.693041905487537));
#112083=CARTESIAN_POINT('Ctrl Pts',(16.6275504637139,18.9873403118716,-0.697470528142895));
#112084=CARTESIAN_POINT('Ctrl Pts',(16.6210181004519,19.0611082624056,-0.701899150798253));
#112085=CARTESIAN_POINT('Ctrl Pts',(16.6183636610493,19.1350271014677,-0.706327773453611));
#112086=CARTESIAN_POINT('Ctrl Pts',(16.6174414214923,19.1607089374613,-0.707866422628241));
#112087=CARTESIAN_POINT('Ctrl Pts',(16.6169868262123,19.1864089348596,-0.709405071802872));
#112088=CARTESIAN_POINT('Ctrl Pts',(16.6170002905278,19.2121090962232,-0.710943720977502));
#112089=CARTESIAN_POINT('Ctrl Pts',(16.6170002428046,19.2120139203676,-0.712619110604606));
#112090=CARTESIAN_POINT('Ctrl Pts',(16.6170721755735,19.3622048615904,-0.721151256465651));
#112091=CARTESIAN_POINT('Ctrl Pts',(16.6331258766371,19.5119663956388,-0.729201744036881));
#112092=CARTESIAN_POINT('Ctrl Pts',(16.6820965468833,19.7382498276167,-0.741816400252578));
#112093=CARTESIAN_POINT('Ctrl Pts',(16.7038575484408,19.8166564320282,-0.746283827984639));
#112094=CARTESIAN_POINT('Ctrl Pts',(16.7417875619102,19.9280069665996,-0.75300998471601));
#112095=CARTESIAN_POINT('Ctrl Pts',(16.7543870689087,19.9620936521435,-0.755123005876484));
#112096=CARTESIAN_POINT('Ctrl Pts',(16.7706293840764,20.0027832821349,-0.757730146936945));
#112097=CARTESIAN_POINT('Ctrl Pts',(16.7734389713608,20.0097148368039,-0.758177289893332));
#112098=CARTESIAN_POINT('Ctrl Pts',(16.7778681013996,20.0204777927027,-0.75887650288154));
#112099=CARTESIAN_POINT('Ctrl Pts',(16.7794623375713,20.0243196340088,-0.759127065838273));
#112100=CARTESIAN_POINT('Ctrl Pts',(16.7824436436943,20.0314446914402,-0.759593622265121));
#112101=CARTESIAN_POINT('Ctrl Pts',(16.7838276867843,20.0347291130496,-0.75980943151961));
#112102=CARTESIAN_POINT('Ctrl Pts',(16.7869797398919,20.0421566627409,-0.760299146739663));
#112103=CARTESIAN_POINT('Ctrl Pts',(16.7887526763491,20.0462976357273,-0.760573349045485));
#112104=CARTESIAN_POINT('Ctrl Pts',(16.794151598636,20.0587972605664,-0.761404532062207));
#112105=CARTESIAN_POINT('Ctrl Pts',(16.7978182879772,20.0671380650843,-0.761963907066338));
#112106=CARTESIAN_POINT('Ctrl Pts',(16.8264545300996,20.13115348135,-0.766292207608628));
#112107=CARTESIAN_POINT('Ctrl Pts',(16.853764529941,20.1857436858668,-0.770187814146948));
#112108=CARTESIAN_POINT('Ctrl Pts',(16.9113896732437,20.2894733572407,-0.777892465160095));
#112109=CARTESIAN_POINT('Ctrl Pts',(16.9414352247186,20.3387075234899,-0.781691412437072));
#112110=CARTESIAN_POINT('Ctrl Pts',(17.034267564791,20.4777246916938,-0.792733422523316));
#112111=CARTESIAN_POINT('Ctrl Pts',(17.1020634321017,20.5639480019873,-0.799975476567422));
#112112=CARTESIAN_POINT('Ctrl Pts',(17.2136539678244,20.6852086621884,-0.81056922548381));
#112113=CARTESIAN_POINT('Ctrl Pts',(17.2526575030984,20.7243963366687,-0.814069183085821));
#112114=CARTESIAN_POINT('Ctrl Pts',(17.309882590848,20.7775567411757,-0.818924447556188));
#112115=CARTESIAN_POINT('Ctrl Pts',(17.3268631398915,20.7928268991362,-0.820332738954798));
#112116=CARTESIAN_POINT('Ctrl Pts',(17.3532541641535,20.8157983089728,-0.822472985443773));
#112117=CARTESIAN_POINT('Ctrl Pts',(17.3624890431794,20.8236978578387,-0.823213077882509));
#112118=CARTESIAN_POINT('Ctrl Pts',(17.3797349967899,20.838194820665,-0.824579076934076));
#112119=CARTESIAN_POINT('Ctrl Pts',(17.3877275052182,20.8448136549541,-0.825205849827082));
#112120=CARTESIAN_POINT('Ctrl Pts',(17.4009524691374,20.8556026997506,-0.826232775485803));
#112121=CARTESIAN_POINT('Ctrl Pts',(17.4061565314278,20.8598072913878,-0.826634317755328));
#112122=CARTESIAN_POINT('Ctrl Pts',(17.4164195138048,20.8680191038776,-0.827421239841784));
#112123=CARTESIAN_POINT('Ctrl Pts',(17.4214769952318,20.872027998438,-0.827806684392119));
#112124=CARTESIAN_POINT('Ctrl Pts',(17.4331770167175,20.8812154065039,-0.828693042407577));
#112125=CARTESIAN_POINT('Ctrl Pts',(17.4398323152578,20.8863775529277,-0.8291933012266));
#112126=CARTESIAN_POINT('Ctrl Pts',(17.4577691339486,20.9001194909548,-0.830531204646337));
#112127=CARTESIAN_POINT('Ctrl Pts',(17.4691064243091,20.9086260291679,-0.831365970496308));
#112128=CARTESIAN_POINT('Ctrl Pts',(17.5673788772651,20.980830251459,-0.838511190985972));
#112129=CARTESIAN_POINT('Ctrl Pts',(17.658980633666,21.0379213769114,-0.844555606789997));
#112130=CARTESIAN_POINT('Ctrl Pts',(17.9003338187212,21.1638782901066,-0.859509511383662));
#112131=CARTESIAN_POINT('Ctrl Pts',(18.0544765438377,21.2227082675158,-0.868183303358356));
#112132=CARTESIAN_POINT('Ctrl Pts',(18.2518193841745,21.2727285920438,-0.879791342789503));
#112133=CARTESIAN_POINT('Ctrl Pts',(18.2900413229699,21.28129543473,-0.882064101689193));
#112134=CARTESIAN_POINT('Ctrl Pts',(18.3359843080636,21.2902621362035,-0.884848709101056));
#112135=CARTESIAN_POINT('Ctrl Pts',(18.3435003741053,21.2916868001242,-0.885305933870731));
#112136=CARTESIAN_POINT('Ctrl Pts',(18.3551553850479,21.2938306231413,-0.886017766370994));
#112137=CARTESIAN_POINT('Ctrl Pts',(18.3592891154542,21.2945782680939,-0.886270783978306));
#112138=CARTESIAN_POINT('Ctrl Pts',(18.3669338506184,21.2959374434686,-0.886739763218027));
#112139=CARTESIAN_POINT('Ctrl Pts',(18.3704441847306,21.29655241359,-0.88695552682346));
#112140=CARTESIAN_POINT('Ctrl Pts',(18.3783518622324,21.2979171762964,-0.887442508573786));
#112141=CARTESIAN_POINT('Ctrl Pts',(18.3827500025938,21.2986619307488,-0.887714006478885));
#112142=CARTESIAN_POINT('Ctrl Pts',(18.3940282459288,21.3005350716878,-0.888411809653817));
#112143=CARTESIAN_POINT('Ctrl Pts',(18.4009115669748,21.3016433703701,-0.888839211734882));
#112144=CARTESIAN_POINT('Ctrl Pts',(18.4415321412924,21.3079780811404,-0.891369892077375));
#112145=CARTESIAN_POINT('Ctrl Pts',(18.4753843176729,21.3124214579499,-0.893513182270694));
#112146=CARTESIAN_POINT('Ctrl Pts',(18.5262581163844,21.3178512632335,-0.896770859022912));
#112147=CARTESIAN_POINT('Ctrl Pts',(18.5432102147203,21.3194539748645,-0.897862463120768));
#112148=CARTESIAN_POINT('Ctrl Pts',(18.5665359734006,21.3213756728581,-0.899371291000689));
#112149=CARTESIAN_POINT('Ctrl Pts',(18.5728948702985,21.3218706300148,-0.899783310766908));
#112150=CARTESIAN_POINT('Ctrl Pts',(18.731701388198,21.3335098807761,-0.910088948362018));
#112151=CARTESIAN_POINT('Ctrl Pts',(18.8849097070059,21.328140398447,-0.920354509541062));
#112152=CARTESIAN_POINT('Ctrl Pts',(19.1280848751859,21.2930668979692,-0.936300611875996));
#112153=CARTESIAN_POINT('Ctrl Pts',(19.2189970957486,21.2737862735516,-0.942191090915608));
#112154=CARTESIAN_POINT('Ctrl Pts',(19.3286539598942,21.2428760308616,-0.949187136634125));
#112155=CARTESIAN_POINT('Ctrl Pts',(19.3488611490825,21.2368527475187,-0.95047202656592));
#112156=CARTESIAN_POINT('Ctrl Pts',(19.3775209093902,21.2278416102537,-0.95228877618808));
#112157=CARTESIAN_POINT('Ctrl Pts',(19.3860492057119,21.2251005632437,-0.952828676750796));
#112158=CARTESIAN_POINT('Ctrl Pts',(19.4007516765177,21.2202719264654,-0.953758290330705));
#112159=CARTESIAN_POINT('Ctrl Pts',(19.406934031911,21.2182098203206,-0.954148836193282));
#112160=CARTESIAN_POINT('Ctrl Pts',(19.4187669317587,21.2142021767488,-0.95489568860466));
#112161=CARTESIAN_POINT('Ctrl Pts',(19.424418944651,21.2122612007821,-0.955252141450639));
#112162=CARTESIAN_POINT('Ctrl Pts',(19.4391247784187,21.2071413081171,-0.956178890925988));
#112163=CARTESIAN_POINT('Ctrl Pts',(19.4481654042787,21.2039246987908,-0.956747933098307));
#112164=CARTESIAN_POINT('Ctrl Pts',(19.4790725825043,21.1926907567521,-0.958691199611591));
#112165=CARTESIAN_POINT('Ctrl Pts',(19.5008290278612,21.1843739417313,-0.96005544967437));
#112166=CARTESIAN_POINT('Ctrl Pts',(19.6812591892358,21.111966351105,-0.971349389867178));
#112167=CARTESIAN_POINT('Ctrl Pts',(19.8317602969987,21.0292140245565,-0.980570870939259));
#112168=CARTESIAN_POINT('Ctrl Pts',(20.0438205499428,20.8765876721058,-0.99477769771984));
#112169=CARTESIAN_POINT('Ctrl Pts',(20.1135298459832,20.8193242800664,-0.999702041086007));
#112170=CARTESIAN_POINT('Ctrl Pts',(20.2075785076758,20.7314425783718,-1.00704526893611));
#112171=CARTESIAN_POINT('Ctrl Pts',(20.2350564296684,20.7043212731197,-1.00928633988184));
#112172=CARTESIAN_POINT('Ctrl Pts',(20.2670472697989,20.6709702266446,-1.0120356762018));
#112173=CARTESIAN_POINT('Ctrl Pts',(20.2722891401027,20.6654461184853,-1.0124908582202));
#112174=CARTESIAN_POINT('Ctrl Pts',(20.2803697489133,20.656837877807,-1.01320008194604));
#112175=CARTESIAN_POINT('Ctrl Pts',(20.283229385846,20.6537733289009,-1.01345254967954));
#112176=CARTESIAN_POINT('Ctrl Pts',(20.2885027108963,20.6480883808154,-1.01392090825715));
#112177=CARTESIAN_POINT('Ctrl Pts',(20.2909188927957,20.6454703737422,-1.01413660375317));
#112178=CARTESIAN_POINT('Ctrl Pts',(20.2963498763317,20.6395558511298,-1.01462391342197));
#112179=CARTESIAN_POINT('Ctrl Pts',(20.2993608403056,20.6362559049736,-1.01489581029872));
#112180=CARTESIAN_POINT('Ctrl Pts',(20.3081696001938,20.6265401257491,-1.01569629101565));
#112181=CARTESIAN_POINT('Ctrl Pts',(20.3139384751181,20.6200983595085,-1.01622696985406));
#112182=CARTESIAN_POINT('Ctrl Pts',(20.3539129043045,20.5749071551173,-1.01994833415176));
#112183=CARTESIAN_POINT('Ctrl Pts',(20.3867259501602,20.5349548807027,-1.0232301831665));
#112184=CARTESIAN_POINT('Ctrl Pts',(20.4313964331169,20.4763142183867,-1.02798925885708));
#112185=CARTESIAN_POINT('Ctrl Pts',(20.4444766487415,20.4585753722496,-1.02942175511493));
#112186=CARTESIAN_POINT('Ctrl Pts',(20.4839563367759,20.4032464403743,-1.03386105231835));
#112187=CARTESIAN_POINT('Ctrl Pts',(20.5094109551861,20.3649993504169,-1.03688946022074));
#112188=CARTESIAN_POINT('Ctrl Pts',(20.5911954386698,20.2329946161385,-1.04714744045571));
#112189=CARTESIAN_POINT('Ctrl Pts',(20.6415049234467,20.1357033724387,-1.05437842966978));
#112190=CARTESIAN_POINT('Ctrl Pts',(20.7055081559617,19.9842253924476,-1.06494830594674));
#112191=CARTESIAN_POINT('Ctrl Pts',(20.7249562597562,19.9326757639309,-1.06843560131803));
#112192=CARTESIAN_POINT('Ctrl Pts',(20.7532158563074,19.847892532634,-1.07399051610733));
#112193=CARTESIAN_POINT('Ctrl Pts',(20.7632671672991,19.8151024352732,-1.07609653604523));
#112194=CARTESIAN_POINT('Ctrl Pts',(20.7754329805161,19.7716756249597,-1.07883208803829));
#112195=CARTESIAN_POINT('Ctrl Pts',(20.7782683399662,19.7612478817376,-1.07948494525895));
#112196=CARTESIAN_POINT('Ctrl Pts',(20.7827823683459,19.7441297914933,-1.08055023107254));
#112197=CARTESIAN_POINT('Ctrl Pts',(20.7845083788725,19.7374522365306,-1.08096418850021));
#112198=CARTESIAN_POINT('Ctrl Pts',(20.7877868232135,19.7245079014751,-1.08176359176459));
#112199=CARTESIAN_POINT('Ctrl Pts',(20.7893432811271,19.7182422283619,-1.08214916383628));
#112200=CARTESIAN_POINT('Ctrl Pts',(20.7928716554397,19.7037554954688,-1.08303750604323));
#112201=CARTESIAN_POINT('Ctrl Pts',(20.7948230459075,19.6955295125245,-1.08353961001947));
#112202=CARTESIAN_POINT('Ctrl Pts',(20.7999401110022,19.6733685283922,-1.08488618416961));
#112203=CARTESIAN_POINT('Ctrl Pts',(20.8030140914805,19.6594126475277,-1.08572771234218));
#112204=CARTESIAN_POINT('Ctrl Pts',(20.8299391557904,19.5309966753832,-1.09341428843042));
#112205=CARTESIAN_POINT('Ctrl Pts',(20.844412813131,19.4147691027026,-1.09994213320598));
#112206=CARTESIAN_POINT('Ctrl Pts',(20.8559026263753,19.1351854659258,-1.11526004969816));
#112207=CARTESIAN_POINT('Ctrl Pts',(20.8437863383083,18.9722359259568,-1.12386685462392));
#112208=CARTESIAN_POINT('Ctrl Pts',(20.8070320844516,18.7805683776233,-1.13507490368345));
#112209=CARTESIAN_POINT('Ctrl Pts',(20.8002202035693,18.7489748729143,-1.1369600696242));
#112210=CARTESIAN_POINT('Ctrl Pts',(20.7910040818629,18.7105248052916,-1.13931433290164));
#112211=CARTESIAN_POINT('Ctrl Pts',(20.7892838746561,18.7035067444061,-1.13974650713986));
#112212=CARTESIAN_POINT('Ctrl Pts',(20.7865298195019,18.6925145111395,-1.14042747868541));
#112213=CARTESIAN_POINT('Ctrl Pts',(20.7855202608741,18.6885342301473,-1.14067489660744));
#112214=CARTESIAN_POINT('Ctrl Pts',(20.783610814994,18.6810969258929,-1.14113881843456));
#112215=CARTESIAN_POINT('Ctrl Pts',(20.7827137559631,18.6776392343322,-1.14135515815387));
#112216=CARTESIAN_POINT('Ctrl Pts',(20.7806451001205,18.6697478737409,-1.14185039413272));
#112217=CARTESIAN_POINT('Ctrl Pts',(20.7794678494619,18.6653157452054,-1.142129613848));
#112218=CARTESIAN_POINT('Ctrl Pts',(20.7758018722212,18.6516925855068,-1.14299109027105));
#112219=CARTESIAN_POINT('Ctrl Pts',(20.7732655681816,18.6425146405063,-1.14357600012887));
#112220=CARTESIAN_POINT('Ctrl Pts',(20.7494659901649,18.5586019094306,-1.14896334844942));
#112221=CARTESIAN_POINT('Ctrl Pts',(20.7241672868575,18.4850813388748,-1.15397009932529));
#112222=CARTESIAN_POINT('Ctrl Pts',(20.6794752132422,18.3752441480921,-1.16173125821361));
#112223=CARTESIAN_POINT('Ctrl Pts',(20.6629669607468,18.3378173233877,-1.16442839640459));
#112224=CARTESIAN_POINT('Ctrl Pts',(20.5983938453691,18.2022023902509,-1.17435057158121));
#112225=CARTESIAN_POINT('Ctrl Pts',(20.5438256344561,18.1072918553061,-1.18157787902276));
#112226=CARTESIAN_POINT('Ctrl Pts',(20.4511414351924,17.9715886342431,-1.19214007518589));
#112227=CARTESIAN_POINT('Ctrl Pts',(20.418354422777,17.9273854792938,-1.19562337147695));
#112228=CARTESIAN_POINT('Ctrl Pts',(20.3624109825724,17.8578035399774,-1.20117276493636));
#112229=CARTESIAN_POINT('Ctrl Pts',(20.3402957503356,17.8316243566024,-1.20327715677248));
#112230=CARTESIAN_POINT('Ctrl Pts',(20.3103831304053,17.7979104915539,-1.20601101777612));
#112231=CARTESIAN_POINT('Ctrl Pts',(20.3031506873816,17.7898835868325,-1.2066637692684));
#112232=CARTESIAN_POINT('Ctrl Pts',(20.2912009041653,17.7768236098939,-1.20772897911582));
#112233=CARTESIAN_POINT('Ctrl Pts',(20.2865199210203,17.7717576748657,-1.20814296503141));
#112234=CARTESIAN_POINT('Ctrl Pts',(20.2774086597171,17.7619933025391,-1.20894249053427));
#112235=CARTESIAN_POINT('Ctrl Pts',(20.2729814833772,17.7572920873077,-1.20932815602549));
#112236=CARTESIAN_POINT('Ctrl Pts',(20.2627063204704,17.74648044752,-1.2102168102565));
#112237=CARTESIAN_POINT('Ctrl Pts',(20.256843063044,17.7403846382049,-1.21071913203689));
#112238=CARTESIAN_POINT('Ctrl Pts',(20.2409688782791,17.7240775808132,-1.2120665077803));
#112239=CARTESIAN_POINT('Ctrl Pts',(20.2308906531443,17.7139322432663,-1.21290861546797));
#112240=CARTESIAN_POINT('Ctrl Pts',(20.1369968128611,17.6213093453177,-1.22063510567093));
#112241=CARTESIAN_POINT('Ctrl Pts',(20.0465437660938,17.5458421600769,-1.22719840370218));
#112242=CARTESIAN_POINT('Ctrl Pts',(19.8163415546447,17.3842530644563,-1.24259187359711));
#112243=CARTESIAN_POINT('Ctrl Pts',(19.6719714362308,17.3060945328849,-1.25123869641716));
#112244=CARTESIAN_POINT('Ctrl Pts',(19.4912802674861,17.2338362297299,-1.26243140406671));
#112245=CARTESIAN_POINT('Ctrl Pts',(19.4622491643232,17.222960034575,-1.26424160000635));
#112246=CARTESIAN_POINT('Ctrl Pts',(19.4262575064435,17.2103702390641,-1.26651244218093));
#112247=CARTESIAN_POINT('Ctrl Pts',(19.4195117344216,17.2080487888513,-1.26693919539804));
#112248=CARTESIAN_POINT('Ctrl Pts',(19.4088835199112,17.2044512376676,-1.26761353814391));
#112249=CARTESIAN_POINT('Ctrl Pts',(19.4050088242724,17.2031521825187,-1.26785979304073));
#112250=CARTESIAN_POINT('Ctrl Pts',(19.397736900938,17.2007375514422,-1.26832277146825));
#112251=CARTESIAN_POINT('Ctrl Pts',(19.3943406001685,17.1996193605286,-1.26853933829952));
#112252=CARTESIAN_POINT('Ctrl Pts',(19.3865516676927,17.1970768026022,-1.26903676250137));
#112253=CARTESIAN_POINT('Ctrl Pts',(19.3821572105583,17.1956582043003,-1.26931795407472));
#112254=CARTESIAN_POINT('Ctrl Pts',(19.3685310777802,17.1913086557225,-1.27019147997714));
#112255=CARTESIAN_POINT('Ctrl Pts',(19.3592840547534,17.1884267238223,-1.270786573982));
#112256=CARTESIAN_POINT('Ctrl Pts',(19.2481012735029,17.1546107590281,-1.27796653456379));
#112257=CARTESIAN_POINT('Ctrl Pts',(19.144001982154,17.1313534392421,-1.28493125873903));
#112258=CARTESIAN_POINT('Ctrl Pts',(18.9302864243071,17.1002791382127,-1.29917768219238));
#112259=CARTESIAN_POINT('Ctrl Pts',(18.8208977152644,17.0929531387274,-1.30643903080193));
#112260=CARTESIAN_POINT('Ctrl Pts',(18.6488171391698,17.0947879134385,-1.31756399007033));
#112261=CARTESIAN_POINT('Ctrl Pts',(18.5862613574716,17.0982330510975,-1.32154890782154));
#112262=CARTESIAN_POINT('Ctrl Pts',(18.4991728130932,17.106917069951,-1.32700390776245));
#112263=CARTESIAN_POINT('Ctrl Pts',(18.474444925285,17.1098241317021,-1.32854246718625));
#112264=CARTESIAN_POINT('Ctrl Pts',(18.4312397297831,17.1156778256324,-1.33121311773824));
#112265=CARTESIAN_POINT('Ctrl Pts',(18.4127398793921,17.1184344058632,-1.33235098995107));
#112266=CARTESIAN_POINT('Ctrl Pts',(18.3858541005302,17.1228054977378,-1.33399682884304));
#112267=CARTESIAN_POINT('Ctrl Pts',(18.3774379562992,17.1242260882117,-1.33451091157527));
#112268=CARTESIAN_POINT('Ctrl Pts',(18.3626808183819,17.1268088812865,-1.33541041996459));
#112269=CARTESIAN_POINT('Ctrl Pts',(18.3563361561911,17.1279492141412,-1.33579653505552));
#112270=CARTESIAN_POINT('Ctrl Pts',(18.3440143594684,17.1302219708145,-1.33654523218482));
#112271=CARTESIAN_POINT('Ctrl Pts',(18.3380367089998,17.1313512123604,-1.33690791134002));
#112272=CARTESIAN_POINT('Ctrl Pts',(18.3237390948993,17.1341160637259,-1.33777414333123));
#112273=CARTESIAN_POINT('Ctrl Pts',(18.3154238858244,17.1357759314167,-1.33827691900606));
#112274=CARTESIAN_POINT('Ctrl Pts',(18.2853390465207,17.1419695964793,-1.34009251807192));
#112275=CARTESIAN_POINT('Ctrl Pts',(18.2636307342855,17.1467964560217,-1.34139598784263));
#112276=CARTESIAN_POINT('Ctrl Pts',(18.0627498736254,17.1947961193728,-1.35340656131926));
#112277=CARTESIAN_POINT('Ctrl Pts',(17.8898625021901,17.2608479974272,-1.36327108162538));
#112278=CARTESIAN_POINT('Ctrl Pts',(17.6564401292847,17.3869620717287,-1.37773038284321));
#112279=CARTESIAN_POINT('Ctrl Pts',(17.587451897218,17.4295188653848,-1.38218214560317));
#112280=CARTESIAN_POINT('Ctrl Pts',(17.4913585237652,17.4966937421309,-1.38888705149075));
#112281=CARTESIAN_POINT('Ctrl Pts',(17.4621807076068,17.5182273877247,-1.39099578831577));
#112282=CARTESIAN_POINT('Ctrl Pts',(17.4276698142784,17.5450929207151,-1.39359843021575));
#112283=CARTESIAN_POINT('Ctrl Pts',(17.4217918922038,17.5497189193321,-1.39404561885559));
#112284=CARTESIAN_POINT('Ctrl Pts',(17.4126815777818,17.5569673667819,-1.39474504477035));
#112285=CARTESIAN_POINT('Ctrl Pts',(17.4094321284608,17.5595684156936,-1.39499577711186));
#112286=CARTESIAN_POINT('Ctrl Pts',(17.4034133886956,17.5644153581116,-1.39546258589766));
#112287=CARTESIAN_POINT('Ctrl Pts',(17.4006420937703,17.5666586709635,-1.39567847765864));
#112288=CARTESIAN_POINT('Ctrl Pts',(17.394381039644,17.5717531155132,-1.39616838630699));
#112289=CARTESIAN_POINT('Ctrl Pts',(17.3908947269368,17.57460838066,-1.39644269930387));
#112290=CARTESIAN_POINT('Ctrl Pts',(17.3806056010608,17.5830901324146,-1.39725671602911));
#112291=CARTESIAN_POINT('Ctrl Pts',(17.3738289347408,17.5887479841084,-1.39779861968202));
#112292=CARTESIAN_POINT('Ctrl Pts',(17.3242111151522,17.6307034491885,-1.40180779530323));
#112293=CARTESIAN_POINT('Ctrl Pts',(17.2827975181789,17.6686472326923,-1.4053825531971));
#112294=CARTESIAN_POINT('Ctrl Pts',(17.1985945891666,17.7521914187054,-1.4130622312626));
#112295=CARTESIAN_POINT('Ctrl Pts',(17.156215584395,17.7981348345008,-1.41717754863527));
#112296=CARTESIAN_POINT('Ctrl Pts',(17.045248180235,17.9296640609522,-1.42854451615834));
#112297=CARTESIAN_POINT('Ctrl Pts',(16.9811727702815,18.018815173926,-1.43579412729792));
#112298=CARTESIAN_POINT('Ctrl Pts',(16.8955511350191,18.1598758862508,-1.44640312640984));
#112299=CARTESIAN_POINT('Ctrl Pts',(16.8686818008557,18.2083310713638,-1.44991077271153));
#112300=CARTESIAN_POINT('Ctrl Pts',(16.8282391802368,18.2885304115173,-1.45549435156725));
#112301=CARTESIAN_POINT('Ctrl Pts',(16.8134880391355,18.3196479535453,-1.45760917390799));
#112302=CARTESIAN_POINT('Ctrl Pts',(16.7951057262466,18.3610028643832,-1.46035435937222));
#112303=CARTESIAN_POINT('Ctrl Pts',(16.7907855005412,18.3709264608044,-1.46100824951286));
#112304=CARTESIAN_POINT('Ctrl Pts',(16.7838354404969,18.3872313332866,-1.46207481943634));
#112305=CARTESIAN_POINT('Ctrl Pts',(16.7811604121196,18.393593019872,-1.46248903467034));
#112306=CARTESIAN_POINT('Ctrl Pts',(16.7760434443961,18.4059305633697,-1.46328865919097));
#112307=CARTESIAN_POINT('Ctrl Pts',(16.773597639742,18.4119047248618,-1.46367419617511));
#112308=CARTESIAN_POINT('Ctrl Pts',(16.7680147562702,18.4257214720483,-1.46456206307928));
#112309=CARTESIAN_POINT('Ctrl Pts',(16.7648971981634,18.4335718657141,-1.46506372953812));
#112310=CARTESIAN_POINT('Ctrl Pts',(16.7566421298026,18.4547273863516,-1.46640825726746));
#112311=CARTESIAN_POINT('Ctrl Pts',(16.7515918955811,18.4680662644982,-1.46724819140767));
#112312=CARTESIAN_POINT('Ctrl Pts',(16.7462566540906,18.4825997824912,-1.46815520219957));
#112313=CARTESIAN_POINT('Ctrl Pts',(16.7458375532442,18.4837444938304,-1.46822658697579));
#112314=CARTESIAN_POINT('Ctrl Pts',(16.7454194504776,18.4848895414187,-1.46829793832533));
#112315=CARTESIAN_POINT('',(16.617000615792,19.2126147021618,-0.489056278967189));
#112316=CARTESIAN_POINT('Ctrl Pts',(16.7454193884829,18.4848897112021,-1.2445862186816));
#112317=CARTESIAN_POINT('Ctrl Pts',(16.8018177025919,18.3304330182041,-1.23372060137579));
#112318=CARTESIAN_POINT('Ctrl Pts',(16.8760653119355,18.1829505081514,-1.22298084578471));
#112319=CARTESIAN_POINT('Ctrl Pts',(16.9785115262827,18.027611935167,-1.21154550356326));
#112320=CARTESIAN_POINT('Ctrl Pts',(16.9905656820716,18.0099238470398,-1.21024028263197));
#112321=CARTESIAN_POINT('Ctrl Pts',(17.0076902571063,17.9855966698589,-1.20844022807956));
#112322=CARTESIAN_POINT('Ctrl Pts',(17.0125345137391,17.9788006522226,-1.20793681914285));
#112323=CARTESIAN_POINT('Ctrl Pts',(17.020958686521,17.9671290093565,-1.20707124559801));
#112324=CARTESIAN_POINT('Ctrl Pts',(17.0245195163649,17.9622397907119,-1.20670835117514));
#112325=CARTESIAN_POINT('Ctrl Pts',(17.0319301869605,17.9521556257385,-1.20595920014336));
#112326=CARTESIAN_POINT('Ctrl Pts',(17.0357829761629,17.9469629165046,-1.20557306336987));
#112327=CARTESIAN_POINT('Ctrl Pts',(17.0448505108803,17.934858169794,-1.20467202029334));
#112328=CARTESIAN_POINT('Ctrl Pts',(17.0500840151204,17.9279602786125,-1.20415785490094));
#112329=CARTESIAN_POINT('Ctrl Pts',(17.0671668158501,17.905729286248,-1.20249829838223));
#112330=CARTESIAN_POINT('Ctrl Pts',(17.0791845688017,17.8905264389161,-1.20135956975118));
#112331=CARTESIAN_POINT('Ctrl Pts',(17.1414403898606,17.8139558127088,-1.19560092677479));
#112332=CARTESIAN_POINT('Ctrl Pts',(17.1948923580414,17.7552774291804,-1.19111361657809));
#112333=CARTESIAN_POINT('Ctrl Pts',(17.3679313906468,17.5855341478621,-1.17766507248548));
#112334=CARTESIAN_POINT('Ctrl Pts',(17.4971417734192,17.4851788360257,-1.1690640459197));
#112335=CARTESIAN_POINT('Ctrl Pts',(17.6888228829003,17.368983179271,-1.15653479048417));
#112336=CARTESIAN_POINT('Ctrl Pts',(17.7424065273263,17.339593552571,-1.15304834380677));
#112337=CARTESIAN_POINT('Ctrl Pts',(17.8053530477427,17.3085313662473,-1.14888518660732));
#112338=CARTESIAN_POINT('Ctrl Pts',(17.8135518570711,17.304551135281,-1.14834164841957));
#112339=CARTESIAN_POINT('Ctrl Pts',(17.8258415114177,17.2986826996303,-1.14752461795865));
#112340=CARTESIAN_POINT('Ctrl Pts',(17.8299132224218,17.296754353427,-1.14725355243867));
#112341=CARTESIAN_POINT('Ctrl Pts',(17.8372193709518,17.2933227005219,-1.14676643854585));
#112342=CARTESIAN_POINT('Ctrl Pts',(17.8404514779532,17.2918145581983,-1.14655069325011));
#112343=CARTESIAN_POINT('Ctrl Pts',(17.8474676156369,17.288562304833,-1.14608179722227));
#112344=CARTESIAN_POINT('Ctrl Pts',(17.8512529387803,17.2868212178851,-1.14582847055763));
#112345=CARTESIAN_POINT('Ctrl Pts',(17.8618592457823,17.2819806538693,-1.14511773555571));
#112346=CARTESIAN_POINT('Ctrl Pts',(17.8686915012149,17.2789062313153,-1.14465883465491));
#112347=CARTESIAN_POINT('Ctrl Pts',(17.9088205167704,17.261104259353,-1.1419578792227));
#112348=CARTESIAN_POINT('Ctrl Pts',(17.9424743087865,17.2472023294799,-1.13967023409614));
#112349=CARTESIAN_POINT('Ctrl Pts',(18.0526131915964,17.2049963454243,-1.1321492625559));
#112350=CARTESIAN_POINT('Ctrl Pts',(18.1303765751753,17.1802425924568,-1.12678910835977));
#112351=CARTESIAN_POINT('Ctrl Pts',(18.3869095020089,17.11462199314,-1.10930507321492));
#112352=CARTESIAN_POINT('Ctrl Pts',(18.5696370501885,17.0924429474123,-1.0972405059824));
#112353=CARTESIAN_POINT('Ctrl Pts',(18.7752748015699,17.0942847709101,-1.08459112651074));
#112354=CARTESIAN_POINT('Ctrl Pts',(18.7975852360155,17.0948374476744,-1.0832294555494));
#112355=CARTESIAN_POINT('Ctrl Pts',(18.8283696716387,17.0960873541174,-1.08136475242817));
#112356=CARTESIAN_POINT('Ctrl Pts',(18.8368538355264,17.096482980337,-1.08085232543775));
#112357=CARTESIAN_POINT('Ctrl Pts',(18.8514156400355,17.0972498638032,-1.07997530729859));
#112358=CARTESIAN_POINT('Ctrl Pts',(18.8574944324195,17.0975963004759,-1.07960994241799));
#112359=CARTESIAN_POINT('Ctrl Pts',(18.87000700651,17.0983635752619,-1.07885937815799));
#112360=CARTESIAN_POINT('Ctrl Pts',(18.8764405353957,17.0987875901687,-1.07847428247985));
#112361=CARTESIAN_POINT('Ctrl Pts',(18.8913800590137,17.0998407775738,-1.07758189383363));
#112362=CARTESIAN_POINT('Ctrl Pts',(18.899884426487,17.1004919792367,-1.07707529753252));
#112363=CARTESIAN_POINT('Ctrl Pts',(18.9269811360591,17.1027316417658,-1.07546547327035));
#112364=CARTESIAN_POINT('Ctrl Pts',(18.9455568359123,17.1045145556207,-1.07436835073024));
#112365=CARTESIAN_POINT('Ctrl Pts',(19.1238252816247,17.1240069056998,-1.06389558019926));
#112366=CARTESIAN_POINT('Ctrl Pts',(19.2810394936595,17.159595631502,-1.05514838677631));
#112367=CARTESIAN_POINT('Ctrl Pts',(19.559504417885,17.2569610830505,-1.03912864398778));
#112368=CARTESIAN_POINT('Ctrl Pts',(19.6817562466483,17.3132450592697,-1.03186594805774));
#112369=CARTESIAN_POINT('Ctrl Pts',(19.8113918692138,17.388594554649,-1.02307441343735));
#112370=CARTESIAN_POINT('Ctrl Pts',(19.8248594297125,17.396623931143,-1.02214689192185));
#112371=CARTESIAN_POINT('Ctrl Pts',(19.843175241912,17.4078214742779,-1.02086416357804));
#112372=CARTESIAN_POINT('Ctrl Pts',(19.8481018998733,17.4108612642901,-1.02051699468056));
#112373=CARTESIAN_POINT('Ctrl Pts',(19.8559115786694,17.4157242425549,-1.01996316173835));
#112374=CARTESIAN_POINT('Ctrl Pts',(19.8588028095931,17.4175342839147,-1.01975735882682));
#112375=CARTESIAN_POINT('Ctrl Pts',(19.8647626966768,17.4212855231065,-1.01933150900215));
#112376=CARTESIAN_POINT('Ctrl Pts',(19.8678307253766,17.4232276234367,-1.0191113991178));
#112377=CARTESIAN_POINT('Ctrl Pts',(19.8751293491352,17.4278740873608,-1.0185856696097));
#112378=CARTESIAN_POINT('Ctrl Pts',(19.879355333859,17.4305856185173,-1.01827957692072));
#112379=CARTESIAN_POINT('Ctrl Pts',(19.8935793862848,17.4397838398057,-1.01724370960489));
#112380=CARTESIAN_POINT('Ctrl Pts',(19.9035320997178,17.4463397800289,-1.01650952332952));
#112381=CARTESIAN_POINT('Ctrl Pts',(19.9273103183535,17.4622922153143,-1.0147338282345));
#112382=CARTESIAN_POINT('Ctrl Pts',(19.9410807314051,17.471768990872,-1.0136876733919));
#112383=CARTESIAN_POINT('Ctrl Pts',(19.9923045517757,17.5079224860696,-1.0097330682375));
#112384=CARTESIAN_POINT('Ctrl Pts',(20.0289959183228,17.5356527555774,-1.00677230862063));
#112385=CARTESIAN_POINT('Ctrl Pts',(20.1225742910843,17.6112881892137,-0.998935581656554));
#112386=CARTESIAN_POINT('Ctrl Pts',(20.177892152827,17.6610350522653,-0.994011792116405));
#112387=CARTESIAN_POINT('Ctrl Pts',(20.3402764466694,17.8233178585506,-0.97884485441687));
#112388=CARTESIAN_POINT('Ctrl Pts',(20.4376925012312,17.9448111597473,-0.968729204076044));
#112389=CARTESIAN_POINT('Ctrl Pts',(20.5337902901492,18.0960932858598,-0.957687396619167));
#112390=CARTESIAN_POINT('Ctrl Pts',(20.5462827913781,18.1165169130028,-0.956225130372346));
#112391=CARTESIAN_POINT('Ctrl Pts',(20.563346210817,18.1455069202426,-0.954188289951838));
#112392=CARTESIAN_POINT('Ctrl Pts',(20.5682083863896,18.1538989347082,-0.953603142493229));
#112393=CARTESIAN_POINT('Ctrl Pts',(20.5759803200287,18.1675282041206,-0.95265994467836));
#112394=CARTESIAN_POINT('Ctrl Pts',(20.5789257769284,18.1727448449722,-0.952300606916462));
#112395=CARTESIAN_POINT('Ctrl Pts',(20.5850180281273,18.1836424993465,-0.951553393936105));
#112396=CARTESIAN_POINT('Ctrl Pts',(20.5881609083949,18.1893256380664,-0.951165662243415));
#112397=CARTESIAN_POINT('Ctrl Pts',(20.5955277563842,18.202792758418,-0.950251396564215));
#112398=CARTESIAN_POINT('Ctrl Pts',(20.5997291506798,18.2105889996081,-0.949725672894765));
#112399=CARTESIAN_POINT('Ctrl Pts',(20.6135042310877,18.2365390965757,-0.947987338027659));
#112400=CARTESIAN_POINT('Ctrl Pts',(20.622863034932,18.2548061462338,-0.946782331584998));
#112401=CARTESIAN_POINT('Ctrl Pts',(20.671079376451,18.3523889117711,-0.940438849605809));
#112402=CARTESIAN_POINT('Ctrl Pts',(20.7052128150041,18.4339465173116,-0.935466838502114));
#112403=CARTESIAN_POINT('Ctrl Pts',(20.7770356875938,18.6410659637741,-0.923366564920433));
#112404=CARTESIAN_POINT('Ctrl Pts',(20.8083555698789,18.768431224881,-0.9163894775598));
#112405=CARTESIAN_POINT('Ctrl Pts',(20.8332930771479,18.9351735100264,-0.90708957052538));
#112406=CARTESIAN_POINT('Ctrl Pts',(20.8378739167237,18.972617979004,-0.904989142915688));
#112407=CARTESIAN_POINT('Ctrl Pts',(20.8458040228046,19.0558313986986,-0.900257365177248));
#112408=CARTESIAN_POINT('Ctrl Pts',(20.8486701978349,19.1016253978506,-0.897610763853716));
#112409=CARTESIAN_POINT('Ctrl Pts',(20.8502754963556,19.1550964974429,-0.894433888659794));
#112410=CARTESIAN_POINT('Ctrl Pts',(20.8504631740708,19.1627215689269,-0.893978808345923));
#112411=CARTESIAN_POINT('Ctrl Pts',(20.8506981096336,19.1749536612913,-0.893245243016827));
#112412=CARTESIAN_POINT('Ctrl Pts',(20.8507715425591,19.179560191593,-0.892968184348993));
#112413=CARTESIAN_POINT('Ctrl Pts',(20.8508753308635,19.1877479143726,-0.892474251672583));
#112414=CARTESIAN_POINT('Ctrl Pts',(20.8509116365179,19.1913289835225,-0.892257713650956));
#112415=CARTESIAN_POINT('Ctrl Pts',(20.8509695805185,19.1989526804795,-0.891795631580296));
#112416=CARTESIAN_POINT('Ctrl Pts',(20.8509887259094,19.2029952209265,-0.891549956635076));
#112417=CARTESIAN_POINT('Ctrl Pts',(20.8510092763564,19.2139751548644,-0.890880956095523));
#112418=CARTESIAN_POINT('Ctrl Pts',(20.8509881595329,19.2209124691406,-0.890456401210897));
#112419=CARTESIAN_POINT('Ctrl Pts',(20.8507068063256,19.2562611684461,-0.888284013714216));
#112420=CARTESIAN_POINT('Ctrl Pts',(20.8499087234104,19.2846638841337,-0.886508591043632));
#112421=CARTESIAN_POINT('Ctrl Pts',(20.8458846131126,19.3680539103531,-0.881224599527745));
#112422=CARTESIAN_POINT('Ctrl Pts',(20.8410840999099,19.4229394116035,-0.87765583949491));
#112423=CARTESIAN_POINT('Ctrl Pts',(20.8165298326325,19.6163873043886,-0.864885018400925));
#112424=CARTESIAN_POINT('Ctrl Pts',(20.7851878762934,19.7531278766494,-0.855533026123477));
#112425=CARTESIAN_POINT('Ctrl Pts',(20.7117632783027,19.9714705117818,-0.840658547782599));
#112426=CARTESIAN_POINT('Ctrl Pts',(20.6774831392652,20.0552393107478,-0.834959697909745));
#112427=CARTESIAN_POINT('Ctrl Pts',(20.6319419562892,20.1489199980843,-0.828603966027766));
#112428=CARTESIAN_POINT('Ctrl Pts',(20.6258176840833,20.1612123217394,-0.827770215727556));
#112429=CARTESIAN_POINT('Ctrl Pts',(20.6158033200141,20.1808319750147,-0.826439622383354));
#112430=CARTESIAN_POINT('Ctrl Pts',(20.6119890984143,20.1881973926852,-0.825940136924066));
#112431=CARTESIAN_POINT('Ctrl Pts',(20.60513933745,20.2012363246238,-0.825055898523691));
#112432=CARTESIAN_POINT('Ctrl Pts',(20.60212105194,20.2069187393921,-0.824670542748864));
#112433=CARTESIAN_POINT('Ctrl Pts',(20.5957778127672,20.2187306184847,-0.823869472659096));
#112434=CARTESIAN_POINT('Ctrl Pts',(20.5924483826109,20.2248576007023,-0.823453923214118));
#112435=CARTESIAN_POINT('Ctrl Pts',(20.583722144385,20.2407286327134,-0.822377375254052));
#112436=CARTESIAN_POINT('Ctrl Pts',(20.5782785544882,20.2504468187836,-0.82171805457273));
#112437=CARTESIAN_POINT('Ctrl Pts',(20.5542933360813,20.2924848601319,-0.818864949670978));
#112438=CARTESIAN_POINT('Ctrl Pts',(20.5349762899705,20.3243561804899,-0.816699232909909));
#112439=CARTESIAN_POINT('Ctrl Pts',(20.4814031028342,20.4077006157434,-0.811013082972562));
#112440=CARTESIAN_POINT('Ctrl Pts',(20.4457161800394,20.4582123094883,-0.807543793289486));
#112441=CARTESIAN_POINT('Ctrl Pts',(20.3211982712216,20.6190236951154,-0.79629125185731));
#112442=CARTESIAN_POINT('Ctrl Pts',(20.223525225247,20.7219736439583,-0.788766768521985));
#112443=CARTESIAN_POINT('Ctrl Pts',(20.0589248347197,20.8638775702418,-0.776736150204603));
#112444=CARTESIAN_POINT('Ctrl Pts',(19.9989286229428,20.9102301408278,-0.772455181743465));
#112445=CARTESIAN_POINT('Ctrl Pts',(19.9287599899443,20.958663574936,-0.767402204384557));
#112446=CARTESIAN_POINT('Ctrl Pts',(19.9208987847652,20.9640118858235,-0.766835470671899));
#112447=CARTESIAN_POINT('Ctrl Pts',(19.9091923300918,20.9718614443569,-0.765990165713417));
#112448=CARTESIAN_POINT('Ctrl Pts',(19.9053744241163,20.9744035262946,-0.765714268437201));
#112449=CARTESIAN_POINT('Ctrl Pts',(19.8985613494388,20.9789079968831,-0.76522149408285));
#112450=CARTESIAN_POINT('Ctrl Pts',(19.895569436007,20.9808752122895,-0.765004944767182));
#112451=CARTESIAN_POINT('Ctrl Pts',(19.889116818243,20.9850944687073,-0.764537580042762));
#112452=CARTESIAN_POINT('Ctrl Pts',(19.8856545563741,20.9873439503088,-0.764286605602603));
#112453=CARTESIAN_POINT('Ctrl Pts',(19.876070753523,20.9935308892412,-0.763591381927055));
#112454=CARTESIAN_POINT('Ctrl Pts',(19.8699355199932,20.9974468836334,-0.763145753095967));
#112455=CARTESIAN_POINT('Ctrl Pts',(19.8360559128462,21.0188264560479,-0.760682339576365));
#112456=CARTESIAN_POINT('Ctrl Pts',(19.8079305722278,21.035674377244,-0.75862785368423));
#112457=CARTESIAN_POINT('Ctrl Pts',(19.63711232465,21.1326822547788,-0.746145465528185));
#112458=CARTESIAN_POINT('Ctrl Pts',(19.4859092909409,21.1967258840482,-0.73512831277251));
#112459=CARTESIAN_POINT('Ctrl Pts',(19.2190444171249,21.2748578121306,-0.71698827893012));
#112460=CARTESIAN_POINT('Ctrl Pts',(19.1068117116188,21.2980543600943,-0.70970881956078));
#112461=CARTESIAN_POINT('Ctrl Pts',(18.9790781526786,21.3138145990478,-0.701850770658219));
#112462=CARTESIAN_POINT('Ctrl Pts',(18.9649012567325,21.3154184859781,-0.700984204352974));
#112463=CARTESIAN_POINT('Ctrl Pts',(18.9422949152857,21.3177448288807,-0.699611049189376));
#112464=CARTESIAN_POINT('Ctrl Pts',(18.9338756702896,21.3185602637674,-0.699101555770226));
#112465=CARTESIAN_POINT('Ctrl Pts',(18.9190081292988,21.319910347466,-0.698205143869056));
#112466=CARTESIAN_POINT('Ctrl Pts',(18.9125618877204,21.3204659312839,-0.697817573212883));
#112467=CARTESIAN_POINT('Ctrl Pts',(18.8992136022336,21.3215547578927,-0.697017252603145));
#112468=CARTESIAN_POINT('Ctrl Pts',(18.8923112791487,21.3220837172095,-0.69660464142529));
#112469=CARTESIAN_POINT('Ctrl Pts',(18.8745658310052,21.3233561181224,-0.695546938774859));
#112470=CARTESIAN_POINT('Ctrl Pts',(18.8637192659353,21.3240499381971,-0.69490340669241));
#112471=CARTESIAN_POINT('Ctrl Pts',(18.8182406329857,21.3266075582578,-0.692217108573733));
#112472=CARTESIAN_POINT('Ctrl Pts',(18.7835696213021,21.3277037771271,-0.69019837849321));
#112473=CARTESIAN_POINT('Ctrl Pts',(18.6930022215074,21.3283406221209,-0.684989114463495));
#112474=CARTESIAN_POINT('Ctrl Pts',(18.6371224591221,21.3265206306365,-0.681839180758607));
#112475=CARTESIAN_POINT('Ctrl Pts',(18.3834475168122,21.3081844708893,-0.667705160538776));
#112476=CARTESIAN_POINT('Ctrl Pts',(18.1885440302935,21.2661224211238,-0.657394732740525));
#112477=CARTESIAN_POINT('Ctrl Pts',(17.9724290328685,21.1865295053752,-0.644170670349927));
#112478=CARTESIAN_POINT('Ctrl Pts',(17.9427413969282,21.1748270650188,-0.642310098073312));
#112479=CARTESIAN_POINT('Ctrl Pts',(17.9070460265398,21.1598156963852,-0.640006153946296));
#112480=CARTESIAN_POINT('Ctrl Pts',(17.9007735587118,21.1571421292857,-0.639598759682576));
#112481=CARTESIAN_POINT('Ctrl Pts',(17.8904622900824,21.1526880834603,-0.63892468050851));
#112482=CARTESIAN_POINT('Ctrl Pts',(17.8864158931916,21.1509251693245,-0.638659042109389));
#112483=CARTESIAN_POINT('Ctrl Pts',(17.8791249403602,21.1477215172384,-0.638178342160083));
#112484=CARTESIAN_POINT('Ctrl Pts',(17.8758784656039,21.1462852593304,-0.637963556785933));
#112485=CARTESIAN_POINT('Ctrl Pts',(17.8695668896892,21.1434739798637,-0.637544520634806));
#112486=CARTESIAN_POINT('Ctrl Pts',(17.8665014919915,21.1420998480889,-0.637340332364547));
#112487=CARTESIAN_POINT('Ctrl Pts',(17.8574579143111,21.1380199874035,-0.636735977221489));
#112488=CARTESIAN_POINT('Ctrl Pts',(17.8514890956,21.1352937823569,-0.636334568963541));
#112489=CARTESIAN_POINT('Ctrl Pts',(17.8231334432058,21.1221829136873,-0.634415899126147));
#112490=CARTESIAN_POINT('Ctrl Pts',(17.8009176767315,21.1114355468693,-0.632877777299931));
#112491=CARTESIAN_POINT('Ctrl Pts',(17.738719949441,21.0799925751033,-0.628482634339698));
#112492=CARTESIAN_POINT('Ctrl Pts',(17.6992044461274,21.0584071729178,-0.625584854015875));
#112493=CARTESIAN_POINT('Ctrl Pts',(17.578480504402,20.9873727237562,-0.616463116042292));
#112494=CARTESIAN_POINT('Ctrl Pts',(17.4998930277222,20.9337027526604,-0.610137964857277));
#112495=CARTESIAN_POINT('Ctrl Pts',(17.3073680120026,20.7822661100353,-0.593981625990813));
#112496=CARTESIAN_POINT('Ctrl Pts',(17.1997115698409,20.6773325280377,-0.584307127283576));
#112497=CARTESIAN_POINT('Ctrl Pts',(17.0950142907436,20.5510054088362,-0.574290993645261));
#112498=CARTESIAN_POINT('Ctrl Pts',(17.0861068718918,20.5400360809597,-0.573432879666373));
#112499=CARTESIAN_POINT('Ctrl Pts',(17.0720937011992,20.5224216141066,-0.572073057614107));
#112500=CARTESIAN_POINT('Ctrl Pts',(17.0669165426599,20.515834068139,-0.571568473305881));
#112501=CARTESIAN_POINT('Ctrl Pts',(17.057848665583,20.5041538086771,-0.570680711877575));
#112502=CARTESIAN_POINT('Ctrl Pts',(17.0539417347495,20.4990738703728,-0.570296888909056));
#112503=CARTESIAN_POINT('Ctrl Pts',(17.0459029725944,20.4885227706918,-0.569504346541635));
#112504=CARTESIAN_POINT('Ctrl Pts',(17.0417745265418,20.4830491155068,-0.569095764192877));
#112505=CARTESIAN_POINT('Ctrl Pts',(17.0312342977279,20.4689323409043,-0.56804852865523));
#112506=CARTESIAN_POINT('Ctrl Pts',(17.0248616471264,20.4602601443962,-0.567411416658005));
#112507=CARTESIAN_POINT('Ctrl Pts',(16.9984537533301,20.4237427443155,-0.564754091846726));
#112508=CARTESIAN_POINT('Ctrl Pts',(16.9790300138077,20.3954603342814,-0.562757572607046));
#112509=CARTESIAN_POINT('Ctrl Pts',(16.9301570205903,20.3204541225425,-0.557608838260007));
#112510=CARTESIAN_POINT('Ctrl Pts',(16.9018328518384,20.2730273714807,-0.5544964948555));
#112511=CARTESIAN_POINT('Ctrl Pts',(16.8405517695375,20.1606520576168,-0.547383534944862));
#112512=CARTESIAN_POINT('Ctrl Pts',(16.809026302663,20.0950034808887,-0.543420741127947));
#112513=CARTESIAN_POINT('Ctrl Pts',(16.7673555757298,19.9953716183546,-0.537557186073658));
#112514=CARTESIAN_POINT('Ctrl Pts',(16.7545802484305,19.9625494382349,-0.535648358953803));
#112515=CARTESIAN_POINT('Ctrl Pts',(16.7287365187993,19.8909142528261,-0.531505687115641));
#112516=CARTESIAN_POINT('Ctrl Pts',(16.7159637149578,19.8520104643433,-0.529270377031467));
#112517=CARTESIAN_POINT('Ctrl Pts',(16.6989489234478,19.7946215484291,-0.52596417755349));
#112518=CARTESIAN_POINT('Ctrl Pts',(16.6938141846103,19.7764103006376,-0.524913722589127));
#112519=CARTESIAN_POINT('Ctrl Pts',(16.6732971358612,19.699721606859,-0.520475847901493));
#112520=CARTESIAN_POINT('Ctrl Pts',(16.660181126937,19.640673069453,-0.51702426761041));
#112521=CARTESIAN_POINT('Ctrl Pts',(16.6480273223415,19.5722326453611,-0.512901042489556));
#112522=CARTESIAN_POINT('Ctrl Pts',(16.6465009500222,19.5633049044344,-0.512360805496219));
#112523=CARTESIAN_POINT('Ctrl Pts',(16.644305604138,19.5499489430587,-0.511548681784569));
#112524=CARTESIAN_POINT('Ctrl Pts',(16.6435932942977,19.5455278134918,-0.511279208710169));
#112525=CARTESIAN_POINT('Ctrl Pts',(16.6423403665007,19.537590922247,-0.510794241488942));
#112526=CARTESIAN_POINT('Ctrl Pts',(16.6417945776022,19.5340760326778,-0.510579044653354));
#112527=CARTESIAN_POINT('Ctrl Pts',(16.640747943493,19.52722180465,-0.510158566898103));
#112528=CARTESIAN_POINT('Ctrl Pts',(16.640246230466,19.5238826521244,-0.509953342278624));
#112529=CARTESIAN_POINT('Ctrl Pts',(16.6391504869416,19.5164692620266,-0.509496889213461));
#112530=CARTESIAN_POINT('Ctrl Pts',(16.6385603510653,19.5123944747754,-0.509245445913275));
#112531=CARTESIAN_POINT('Ctrl Pts',(16.6371204772028,19.5022437235401,-0.508617740339853));
#112532=CARTESIAN_POINT('Ctrl Pts',(16.6362852638928,19.4961657824301,-0.508240703202683));
#112533=CARTESIAN_POINT('Ctrl Pts',(16.6323977852852,19.4669346043774,-0.50642195905365));
#112534=CARTESIAN_POINT('Ctrl Pts',(16.6297024930675,19.4437365273374,-0.504962251941544));
#112535=CARTESIAN_POINT('Ctrl Pts',(16.6205187012968,19.351389617802,-0.499098993300709));
#112536=CARTESIAN_POINT('Ctrl Pts',(16.6170514727118,19.2819895701451,-0.494577329568077));
#112537=CARTESIAN_POINT('Ctrl Pts',(16.617000568856,19.2125519458626,-0.490010468414517));
#112538=CARTESIAN_POINT('Ctrl Pts',(16.617000615792,19.2126147021618,-0.489056278967189));
#112539=CARTESIAN_POINT('Ctrl Pts',(16.6169459704489,19.1409704320946,-0.484732818395265));
#112540=CARTESIAN_POINT('Ctrl Pts',(16.6205324586778,19.0691916432072,-0.480409357823342));
#112541=CARTESIAN_POINT('Ctrl Pts',(16.6277745421012,18.9976849266948,-0.476085897251419));
#112542=CARTESIAN_POINT('Ctrl Pts',(16.6350090269828,18.9262532364906,-0.471766972942677));
#112543=CARTESIAN_POINT('Ctrl Pts',(16.645891455306,18.8550935436973,-0.467448048633935));
#112544=CARTESIAN_POINT('Ctrl Pts',(16.6603842665429,18.7846119256369,-0.463129124325193));
#112545=CARTESIAN_POINT('Ctrl Pts',(16.6748666504054,18.714181018112,-0.4588133074219));
#112546=CARTESIAN_POINT('Ctrl Pts',(16.6929541651129,18.6444277026836,-0.454497490518607));
#112547=CARTESIAN_POINT('Ctrl Pts',(16.7145577237428,18.5757505270643,-0.450181673615314));
#112548=CARTESIAN_POINT('Ctrl Pts',(16.7241553570749,18.545239889388,-0.448264321531073));
#112549=CARTESIAN_POINT('Ctrl Pts',(16.7344462704266,18.5149415151545,-0.446346969446833));
#112550=CARTESIAN_POINT('Ctrl Pts',(16.7454194503191,18.4848895418526,-0.444429617362593));
#112551=CARTESIAN_POINT('Origin',(18.734,-18.952,0.));
#112552=CARTESIAN_POINT('',(16.6170002905271,-18.9508909049916,-0.710943720977502));
#112553=CARTESIAN_POINT('Ctrl Pts',(16.7454194499637,-19.6781104571739,
-0.666446448202515));
#112554=CARTESIAN_POINT('Ctrl Pts',(16.7201110311403,-19.6087989234712,
-0.670880799931208));
#112555=CARTESIAN_POINT('Ctrl Pts',(16.6984028489342,-19.5380871560008,
-0.675315151659902));
#112556=CARTESIAN_POINT('Ctrl Pts',(16.6804409278771,-19.4663774268974,
-0.679749503388595));
#112557=CARTESIAN_POINT('Ctrl Pts',(16.6624933915782,-19.3947251263463,
-0.684180303878107));
#112558=CARTESIAN_POINT('Ctrl Pts',(16.6482862689509,-19.3220769011711,
-0.688611104367619));
#112559=CARTESIAN_POINT('Ctrl Pts',(16.6379158183503,-19.2488503047633,
-0.693041904857131));
#112560=CARTESIAN_POINT('Ctrl Pts',(16.6275504654133,-19.1756597033728,
-0.697470527357381));
#112561=CARTESIAN_POINT('Ctrl Pts',(16.6210181017774,-19.1018917551645,
-0.701899149857632));
#112562=CARTESIAN_POINT('Ctrl Pts',(16.6183636617623,-19.0279729183858,
-0.706327772357882));
#112563=CARTESIAN_POINT('Ctrl Pts',(16.6174414217412,-19.0022910761897,
-0.707866421897756));
#112564=CARTESIAN_POINT('Ctrl Pts',(16.6169868262232,-18.976591072574,-0.709405071437629));
#112565=CARTESIAN_POINT('Ctrl Pts',(16.6170002905271,-18.9508909049916,
-0.710943720977502));
#112566=CARTESIAN_POINT('Ctrl Pts',(16.6170002428037,-18.9509860813785,
-0.71261911997228));
#112567=CARTESIAN_POINT('Ctrl Pts',(16.6170355426432,-18.8772821863969,
-0.71680613931656));
#112568=CARTESIAN_POINT('Ctrl Pts',(16.6209198238468,-18.8036252920842,
-0.720887471493913));
#112569=CARTESIAN_POINT('Ctrl Pts',(16.6457836173313,-18.5674910391913,
-0.733880950583028));
#112570=CARTESIAN_POINT('Ctrl Pts',(16.6817565015368,-18.4072256903138,
-0.742529972060711));
#112571=CARTESIAN_POINT('Ctrl Pts',(16.7460896191493,-18.2233937368426,
-0.753730253773707));
#112572=CARTESIAN_POINT('Ctrl Pts',(16.7569987507012,-18.1942925374262,
-0.755544779403702));
#112573=CARTESIAN_POINT('Ctrl Pts',(16.7711944231595,-18.1588202190053,
-0.757820171089045));
#112574=CARTESIAN_POINT('Ctrl Pts',(16.7738785229288,-18.1522102218227,
-0.75824692452464));
#112575=CARTESIAN_POINT('Ctrl Pts',(16.7781515132025,-18.1418380566543,
-0.758921095400191));
#112576=CARTESIAN_POINT('Ctrl Pts',(16.7797179957211,-18.1380666336509,
-0.75916717565633));
#112577=CARTESIAN_POINT('Ctrl Pts',(16.7826759254017,-18.1310029653032,
-0.759629887068448));
#112578=CARTESIAN_POINT('Ctrl Pts',(16.7840648014493,-18.1277097017187,
-0.759846361949575));
#112579=CARTESIAN_POINT('Ctrl Pts',(16.7872660989969,-18.1201722433198,
-0.760343519957725));
#112580=CARTESIAN_POINT('Ctrl Pts',(16.7890840600327,-18.1159304552678,
-0.7606245371859));
#112581=CARTESIAN_POINT('Ctrl Pts',(16.7947542407714,-18.102818984733,-0.761496922286903));
#112582=CARTESIAN_POINT('Ctrl Pts',(16.7986533115283,-18.0939698731072,
-0.762091039278325));
#112583=CARTESIAN_POINT('Ctrl Pts',(16.8403369192543,-18.00109682771,-0.768380309550798));
#112584=CARTESIAN_POINT('Ctrl Pts',(16.8835033415036,-17.9196072284535,
-0.774361178149046));
#112585=CARTESIAN_POINT('Ctrl Pts',(16.9959657519195,-17.7371479806969,
-0.788456678379995));
#112586=CARTESIAN_POINT('Ctrl Pts',(17.0689947662275,-17.6388399003217,
-0.796593907650438));
#112587=CARTESIAN_POINT('Ctrl Pts',(17.1923918239987,-17.4996928903399,
-0.808626273526529));
#112588=CARTESIAN_POINT('Ctrl Pts',(17.2368175647855,-17.453935350144,-0.812685605840463));
#112589=CARTESIAN_POINT('Ctrl Pts',(17.3015997566456,-17.3929766520606,
-0.818232054003031));
#112590=CARTESIAN_POINT('Ctrl Pts',(17.3202629042825,-17.3760330695435,
-0.81979016167976));
#112591=CARTESIAN_POINT('Ctrl Pts',(17.3490355213559,-17.3508340284309,
-0.82213340014388));
#112592=CARTESIAN_POINT('Ctrl Pts',(17.3589255684514,-17.3423325202814,
-0.822928630515614));
#112593=CARTESIAN_POINT('Ctrl Pts',(17.3772963109687,-17.326833868013,-0.82438726746762));
#112594=CARTESIAN_POINT('Ctrl Pts',(17.3857541133686,-17.3198103992765,
-0.825051739970025));
#112595=CARTESIAN_POINT('Ctrl Pts',(17.3995560471391,-17.3085295836163,
-0.826124784077197));
#112596=CARTESIAN_POINT('Ctrl Pts',(17.4048666696862,-17.3042317320671,
-0.826534994193013));
#112597=CARTESIAN_POINT('Ctrl Pts',(17.4149606219979,-17.2961433136996,
-0.827309690418029));
#112598=CARTESIAN_POINT('Ctrl Pts',(17.4197397094547,-17.2923475857319,
-0.827674381729845));
#112599=CARTESIAN_POINT('Ctrl Pts',(17.4308937937994,-17.2835669917952,
-0.828520726216034));
#112600=CARTESIAN_POINT('Ctrl Pts',(17.4372811196317,-17.2785978858684,
-0.82900174839417));
#112601=CARTESIAN_POINT('Ctrl Pts',(17.4538175285942,-17.2658846989307,
-0.830237875951687));
#112602=CARTESIAN_POINT('Ctrl Pts',(17.4640085401947,-17.2581955038162,
-0.830990818829536));
#112603=CARTESIAN_POINT('Ctrl Pts',(17.5289624618929,-17.2101030885643,
-0.835735356583544));
#112604=CARTESIAN_POINT('Ctrl Pts',(17.5855804178744,-17.1722657100199,
-0.839626364752976));
#112605=CARTESIAN_POINT('Ctrl Pts',(17.7838167681934,-17.0531924166677,
-0.852592511231799));
#112606=CARTESIAN_POINT('Ctrl Pts',(17.9329436580573,-16.9856264318967,
-0.861226753026156));
#112607=CARTESIAN_POINT('Ctrl Pts',(18.1411303138149,-16.9189564153889,
-0.873301274503703));
#112608=CARTESIAN_POINT('Ctrl Pts',(18.1945524665604,-16.9041337479739,
-0.876406525842522));
#112609=CARTESIAN_POINT('Ctrl Pts',(18.2762612297136,-16.884881656752,-0.881248542072119));
#112610=CARTESIAN_POINT('Ctrl Pts',(18.3041598476546,-16.8789008008341,
-0.882917908553437));
#112611=CARTESIAN_POINT('Ctrl Pts',(18.3389930273685,-16.8721666421691,
-0.885031716162564));
#112612=CARTESIAN_POINT('Ctrl Pts',(18.3458231882031,-16.8708810546962,
-0.885447598510661));
#112613=CARTESIAN_POINT('Ctrl Pts',(18.3566405913668,-16.8689000845491,
-0.886108654377235));
#112614=CARTESIAN_POINT('Ctrl Pts',(18.3606237796473,-16.8681824507699,
-0.886352581239698));
#112615=CARTESIAN_POINT('Ctrl Pts',(18.3681384624805,-16.8668508005615,
-0.886813781301725));
#112616=CARTESIAN_POINT('Ctrl Pts',(18.3716694666074,-16.8662343294563,
-0.887030913233596));
#112617=CARTESIAN_POINT('Ctrl Pts',(18.3797450055537,-16.8648455619696,
-0.887528456116828));
#112618=CARTESIAN_POINT('Ctrl Pts',(18.3842905010985,-16.8640791406926,
-0.887809196000663));
#112619=CARTESIAN_POINT('Ctrl Pts',(18.3963642288273,-16.8620839082306,
-0.888556652553524));
#112620=CARTESIAN_POINT('Ctrl Pts',(18.4038965813485,-16.8608809422738,
-0.889024773657226));
#112621=CARTESIAN_POINT('Ctrl Pts',(18.4566786031498,-16.8527435920211,
-0.892316956169591));
#112622=CARTESIAN_POINT('Ctrl Pts',(18.5021328400444,-16.8472383611177,
-0.895212973041072));
#112623=CARTESIAN_POINT('Ctrl Pts',(18.551351529235,-16.8428907603699,-0.898389467614695));
#112624=CARTESIAN_POINT('Ctrl Pts',(18.5549780714355,-16.8425798433235,
-0.8986237573938));
#112625=CARTESIAN_POINT('Ctrl Pts',(18.565504661746,-16.841704700739,-0.899304479954829));
#112626=CARTESIAN_POINT('Ctrl Pts',(18.572406655665,-16.8411649712813,-0.89975163445017));
#112627=CARTESIAN_POINT('Ctrl Pts',(18.7317404347313,-16.8294912688356,
-0.910091580626856));
#112628=CARTESIAN_POINT('Ctrl Pts',(18.8849319967157,-16.8348623850344,
-0.920355985649072));
#112629=CARTESIAN_POINT('Ctrl Pts',(19.1280890125997,-16.869933960768,-0.936300890317911));
#112630=CARTESIAN_POINT('Ctrl Pts',(19.2189995374875,-16.8892143769221,
-0.942191256988144));
#112631=CARTESIAN_POINT('Ctrl Pts',(19.3286545583813,-16.9201241464266,
-0.949187184418303));
#112632=CARTESIAN_POINT('Ctrl Pts',(19.3488615490117,-16.9261473760029,
-0.950472061642716));
#112633=CARTESIAN_POINT('Ctrl Pts',(19.3775210786797,-16.9351584439184,
-0.952288796585128));
#112634=CARTESIAN_POINT('Ctrl Pts',(19.3860493412802,-16.937899480802,-0.952828694998408));
#112635=CARTESIAN_POINT('Ctrl Pts',(19.4007517722814,-16.9427281053334,
-0.953758306041049));
#112636=CARTESIAN_POINT('Ctrl Pts',(19.4069341214739,-16.944790209727,-0.954148851503725));
#112637=CARTESIAN_POINT('Ctrl Pts',(19.4187670220499,-16.948797854094,-0.95489570394616));
#112638=CARTESIAN_POINT('Ctrl Pts',(19.4244190418326,-16.9507388327227,
-0.955252157219276));
#112639=CARTESIAN_POINT('Ctrl Pts',(19.4391249210422,-16.9558587420666,
-0.956178909538389));
#112640=CARTESIAN_POINT('Ctrl Pts',(19.4481655852883,-16.9590753658766,
-0.956747954111838));
#112641=CARTESIAN_POINT('Ctrl Pts',(19.479073034196,-16.970309410156,-0.95869123758568));
#112642=CARTESIAN_POINT('Ctrl Pts',(19.5008297091688,-16.9786263200856,
-0.96005550196899));
#112643=CARTESIAN_POINT('Ctrl Pts',(19.681256356536,-17.0510325973115,-0.971349221504955));
#112644=CARTESIAN_POINT('Ctrl Pts',(19.8317541182695,-17.1337826213133,
-0.980570505987134));
#112645=CARTESIAN_POINT('Ctrl Pts',(20.0438142572456,-17.2864072233282,
-0.994777264474122));
#112646=CARTESIAN_POINT('Ctrl Pts',(20.1135259674386,-17.3436722316453,
-0.999701756439865));
#112647=CARTESIAN_POINT('Ctrl Pts',(20.2075773503907,-17.4315562820003,
-1.00704518389461));
#112648=CARTESIAN_POINT('Ctrl Pts',(20.2350557938208,-17.4586780694052,
-1.00928629483316));
#112649=CARTESIAN_POINT('Ctrl Pts',(20.2670471553504,-17.4920296529738,
-1.01203567545134));
#112650=CARTESIAN_POINT('Ctrl Pts',(20.2722890530305,-17.4975537892179,
-1.01249085978528));
#112651=CARTESIAN_POINT('Ctrl Pts',(20.2803696947564,-17.5061620642462,
-1.01320008634213));
#112652=CARTESIAN_POINT('Ctrl Pts',(20.2832293374995,-17.509226619161,-1.0134525545708));
#112653=CARTESIAN_POINT('Ctrl Pts',(20.2885026678211,-17.5149115725923,
-1.01392091358897));
#112654=CARTESIAN_POINT('Ctrl Pts',(20.290918849221,-17.5175295789655,-1.0141366090273));
#112655=CARTESIAN_POINT('Ctrl Pts',(20.2963498247981,-17.5234440925452,
-1.01462391795212));
#112656=CARTESIAN_POINT('Ctrl Pts',(20.2993607813639,-17.5267440303257,
-1.01489581413903));
#112657=CARTESIAN_POINT('Ctrl Pts',(20.3081694998761,-17.5364597630036,
-1.01569629102243));
#112658=CARTESIAN_POINT('Ctrl Pts',(20.3139383412456,-17.5429014907017,
-1.01622696668769));
#112659=CARTESIAN_POINT('Ctrl Pts',(20.3539119531124,-17.5880917602718,
-1.01994825404022));
#112660=CARTESIAN_POINT('Ctrl Pts',(20.3867242811015,-17.6280430822312,
-1.02323002510233));
#112661=CARTESIAN_POINT('Ctrl Pts',(20.4313955828887,-17.6866845998212,
-1.02798917296889));
#112662=CARTESIAN_POINT('Ctrl Pts',(20.4444772056338,-17.7044253494656,
-1.02942182313896));
#112663=CARTESIAN_POINT('Ctrl Pts',(20.4839575658919,-17.7597554046055,
-1.03386120766503));
#112664=CARTESIAN_POINT('Ctrl Pts',(20.5094115651562,-17.7980016302671,
-1.03688954573458));
#112665=CARTESIAN_POINT('Ctrl Pts',(20.5911954782104,-17.9300054568297,
-1.04714745521377));
#112666=CARTESIAN_POINT('Ctrl Pts',(20.6415049546145,-18.0272966930861,
-1.05437844370008));
#112667=CARTESIAN_POINT('Ctrl Pts',(20.7055081741047,-18.1787746546412,
-1.06494831847687));
#112668=CARTESIAN_POINT('Ctrl Pts',(20.7249562726974,-18.2303242726602,
-1.06843561308593));
#112669=CARTESIAN_POINT('Ctrl Pts',(20.7532158627143,-18.3151074879787,
-1.07399052678027));
#112670=CARTESIAN_POINT('Ctrl Pts',(20.763267171779,-18.3478975800922,-1.07609654636897));
#112671=CARTESIAN_POINT('Ctrl Pts',(20.7754329830177,-18.391324384167,-1.07883209796092));
#112672=CARTESIAN_POINT('Ctrl Pts',(20.7782683421713,-18.4017521264737,
-1.07948495512259));
#112673=CARTESIAN_POINT('Ctrl Pts',(20.7827823701362,-18.418870215392,-1.08055024085139));
#112674=CARTESIAN_POINT('Ctrl Pts',(20.7845083805336,-18.425547769945,-1.08096419825283));
#112675=CARTESIAN_POINT('Ctrl Pts',(20.7877868246637,-18.4384921043285,
-1.08176360147426));
#112676=CARTESIAN_POINT('Ctrl Pts',(20.7893432824945,-18.4447577771819,
-1.08214917352929));
#112677=CARTESIAN_POINT('Ctrl Pts',(20.7928716566639,-18.4592445096494,
-1.08303751570866));
#112678=CARTESIAN_POINT('Ctrl Pts',(20.7948230470711,-18.4674704924275,
-1.08353961967391));
#112679=CARTESIAN_POINT('Ctrl Pts',(20.7999401120983,-18.4896314765021,
-1.08488619381826));
#112680=CARTESIAN_POINT('Ctrl Pts',(20.8030140925656,-18.5035873574756,
-1.08572772199579));
#112681=CARTESIAN_POINT('Ctrl Pts',(20.8299391651873,-18.6320033708402,
-1.09341430053484));
#112682=CARTESIAN_POINT('Ctrl Pts',(20.8444128240033,-18.7482309858231,
-1.0999421474991));
#112683=CARTESIAN_POINT('Ctrl Pts',(20.8559026254581,-19.0278147569397,
-1.11526007103807));
#112684=CARTESIAN_POINT('Ctrl Pts',(20.8437863098804,-19.1907643877648,
-1.12386688060966));
#112685=CARTESIAN_POINT('Ctrl Pts',(20.8070320242304,-19.3824319035813,
-1.13507492961851));
#112686=CARTESIAN_POINT('Ctrl Pts',(20.800220164733,-19.4140252925404,-1.13696008886946));
#112687=CARTESIAN_POINT('Ctrl Pts',(20.7910040714245,-19.4524752374912,
-1.13931434469167));
#112688=CARTESIAN_POINT('Ctrl Pts',(20.7892838660647,-19.4594932902695,
-1.13974651843837));
#112689=CARTESIAN_POINT('Ctrl Pts',(20.7865298132606,-19.4704855135526,
-1.14042748937319));
#112690=CARTESIAN_POINT('Ctrl Pts',(20.7855202550648,-19.4744657926485,
-1.14067490717982));
#112691=CARTESIAN_POINT('Ctrl Pts',(20.7836108095494,-19.4819030951674,
-1.14113882890266));
#112692=CARTESIAN_POINT('Ctrl Pts',(20.7827137504395,-19.4853607868861,
-1.14135516863377));
#112693=CARTESIAN_POINT('Ctrl Pts',(20.7806450938112,-19.4932521501384,
-1.14185040478401));
#112694=CARTESIAN_POINT('Ctrl Pts',(20.7794678424307,-19.4976842811726,
-1.14212962465978));
#112695=CARTESIAN_POINT('Ctrl Pts',(20.7758018608328,-19.5113074562963,
-1.1429911020694));
#112696=CARTESIAN_POINT('Ctrl Pts',(20.7732655530011,-19.5204854141741,
-1.14357601276167));
#112697=CARTESIAN_POINT('Ctrl Pts',(20.7494657818614,-19.6043988155693,
-1.14896340429626));
#112698=CARTESIAN_POINT('Ctrl Pts',(20.7241668174136,-19.6779200213361,
-1.15397020109261));
#112699=CARTESIAN_POINT('Ctrl Pts',(20.6794746347646,-19.7877571648899,
-1.16173136192276));
#112700=CARTESIAN_POINT('Ctrl Pts',(20.6629666402308,-19.8251833525167,
-1.16442845492379));
#112701=CARTESIAN_POINT('Ctrl Pts',(20.5983938185803,-19.9607976586218,
-1.1743505843766));
#112702=CARTESIAN_POINT('Ctrl Pts',(20.5438256082449,-20.0557081870924,
-1.18157789139431));
#112703=CARTESIAN_POINT('Ctrl Pts',(20.4511414131881,-20.1914113959507,
-1.1921400866996));
#112704=CARTESIAN_POINT('Ctrl Pts',(20.4183544039852,-20.2356145450826,
-1.19562338255792));
#112705=CARTESIAN_POINT('Ctrl Pts',(20.362410968956,-20.3051964763336,-1.20117277541098));
#112706=CARTESIAN_POINT('Ctrl Pts',(20.3402957383787,-20.3313756572483,
-1.20327716706276));
#112707=CARTESIAN_POINT('Ctrl Pts',(20.3103831203905,-20.3650895196156,
-1.20601102786557));
#112708=CARTESIAN_POINT('Ctrl Pts',(20.3031506775416,-20.3731164240299,
-1.20666377933687));
#112709=CARTESIAN_POINT('Ctrl Pts',(20.2912008945218,-20.3861764005765,
-1.20772898915887));
#112710=CARTESIAN_POINT('Ctrl Pts',(20.2865199113978,-20.3912423355137,
-1.20814297506961));
#112711=CARTESIAN_POINT('Ctrl Pts',(20.2774086500694,-20.4010067077372,
-1.20894250056905));
#112712=CARTESIAN_POINT('Ctrl Pts',(20.272981473681,-20.4057079229574,-1.20932816606182));
#112713=CARTESIAN_POINT('Ctrl Pts',(20.2627063105642,-20.4165195628214,
-1.21021682030486));
#112714=CARTESIAN_POINT('Ctrl Pts',(20.2568430529755,-20.4226153722222,
-1.21071914209565));
#112715=CARTESIAN_POINT('Ctrl Pts',(20.240968867543,-20.4389224300737,-1.21206651788627));
#112716=CARTESIAN_POINT('Ctrl Pts',(20.230890641896,-20.4490677679866,-1.21290862561043));
#112717=CARTESIAN_POINT('Ctrl Pts',(20.1369967599727,-20.5416907055649,
-1.22063511917889));
#112718=CARTESIAN_POINT('Ctrl Pts',(20.0465436656997,-20.6171579230743,
-1.22719842020855));
#112719=CARTESIAN_POINT('Ctrl Pts',(19.8163414313007,-20.7787470044817,
-1.24259189043989));
#112720=CARTESIAN_POINT('Ctrl Pts',(19.6719713496131,-20.8569055057939,
-1.2512387110801));
#112721=CARTESIAN_POINT('Ctrl Pts',(19.4912802367099,-20.9291637818119,
-1.26243141537735));
#112722=CARTESIAN_POINT('Ctrl Pts',(19.462249148109,-20.94003997112,-1.26424161042471));
#112723=CARTESIAN_POINT('Ctrl Pts',(19.4262575060555,-20.9526297610663,
-1.26651245160639));
#112724=CARTESIAN_POINT('Ctrl Pts',(19.4195117350713,-20.9549512109224,
-1.26693920475872));
#112725=CARTESIAN_POINT('Ctrl Pts',(19.4088835218168,-20.958548761691,-1.26761354742592));
#112726=CARTESIAN_POINT('Ctrl Pts',(19.4050088263892,-20.9598478167734,
-1.26785980230966));
#112727=CARTESIAN_POINT('Ctrl Pts',(19.3977369032497,-20.9622624477946,
-1.26832278072534));
#112728=CARTESIAN_POINT('Ctrl Pts',(19.3943406024634,-20.963380638718,-1.26853934755794));
#112729=CARTESIAN_POINT('Ctrl Pts',(19.3865516696503,-20.9659231967643,
-1.26903677178193));
#112730=CARTESIAN_POINT('Ctrl Pts',(19.3821572121935,-20.9673417951746,
-1.26931796337629));
#112731=CARTESIAN_POINT('Ctrl Pts',(19.3685310772336,-20.9716913444586,
-1.27019148941984));
#112732=CARTESIAN_POINT('Ctrl Pts',(19.3592840523413,-20.9745732769327,
-1.27078658354604));
#112733=CARTESIAN_POINT('Ctrl Pts',(19.2480925145358,-21.0083919047543,
-1.27796710962819));
#112734=CARTESIAN_POINT('Ctrl Pts',(19.1439841050508,-21.0316505536747,
-1.28493246285752));
#112735=CARTESIAN_POINT('Ctrl Pts',(18.9302683587808,-21.0627220560751,
-1.29917889280898));
#112736=CARTESIAN_POINT('Ctrl Pts',(18.8208889906715,-21.0700467351152,
-1.30643960358215));
#112737=CARTESIAN_POINT('Ctrl Pts',(18.6488176405106,-21.0682121108594,
-1.31756396746955));
#112738=CARTESIAN_POINT('Ctrl Pts',(18.5862617189313,-21.0647669783043,
-1.32154889443608));
#112739=CARTESIAN_POINT('Ctrl Pts',(18.4991729974121,-21.0560829510683,
-1.32700390567964));
#112740=CARTESIAN_POINT('Ctrl Pts',(18.4744450717296,-21.053175886837,-1.32854246750262));
#112741=CARTESIAN_POINT('Ctrl Pts',(18.4312398161399,-21.0473221870459,
-1.33121312181506));
#112742=CARTESIAN_POINT('Ctrl Pts',(18.4127399434587,-21.0445656041731,
-1.3323509954114));
#112743=CARTESIAN_POINT('Ctrl Pts',(18.3858541383861,-21.04019450859,-1.33399683591618));
#112744=CARTESIAN_POINT('Ctrl Pts',(18.3774379901541,-21.0387739175895,
-1.3345109188948));
#112745=CARTESIAN_POINT('Ctrl Pts',(18.3626808477277,-21.0361911239433,
-1.33541042756147));
#112746=CARTESIAN_POINT('Ctrl Pts',(18.3563361850225,-21.0350507910876,
-1.33579654268471));
#112747=CARTESIAN_POINT('Ctrl Pts',(18.3440143891395,-21.0327780347425,
-1.33654523976477));
#112748=CARTESIAN_POINT('Ctrl Pts',(18.3380367400237,-21.0316487935424,
-1.33690791883884));
#112749=CARTESIAN_POINT('Ctrl Pts',(18.3237391321155,-21.0288839436055,
-1.33777415045736));
#112750=CARTESIAN_POINT('Ctrl Pts',(18.3154239278694,-21.0272240770436,
-1.33827692584218));
#112751=CARTESIAN_POINT('Ctrl Pts',(18.2853391240321,-21.0210304199913,
-1.34009252277639));
#112752=CARTESIAN_POINT('Ctrl Pts',(18.2636308422363,-21.0162035682387,
-1.34139599073438));
#112753=CARTESIAN_POINT('Ctrl Pts',(18.0627496913366,-20.9682038497831,
-1.35340658175214));
#112754=CARTESIAN_POINT('Ctrl Pts',(17.8898620219208,-20.9021518255334,
-1.36327111787147));
#112755=CARTESIAN_POINT('Ctrl Pts',(17.6564395998259,-20.7760376059843,
-1.3777304261534));
#112756=CARTESIAN_POINT('Ctrl Pts',(17.5874515606887,-20.7334809082973,
-1.38218217778131));
#112757=CARTESIAN_POINT('Ctrl Pts',(17.4913584157976,-20.6663061783925,
-1.38888706854443));
#112758=CARTESIAN_POINT('Ctrl Pts',(17.4621806469295,-20.6447725654575,
-1.39099580212177));
#112759=CARTESIAN_POINT('Ctrl Pts',(17.4276698019771,-20.6179070696227,
-1.39359844041197));
#112760=CARTESIAN_POINT('Ctrl Pts',(17.4217918827532,-20.6132810731869,
-1.39404562883981));
#112761=CARTESIAN_POINT('Ctrl Pts',(17.4126815718345,-20.606032628465,-1.39474505449033));
#112762=CARTESIAN_POINT('Ctrl Pts',(17.4094321231862,-20.6034315800736,
-1.39499578678139));
#112763=CARTESIAN_POINT('Ctrl Pts',(17.4034133841137,-20.5985846381858,
-1.39546259551572));
#112764=CARTESIAN_POINT('Ctrl Pts',(17.4006420892115,-20.5963413253399,
-1.39567848727596));
#112765=CARTESIAN_POINT('Ctrl Pts',(17.394381034439,-20.5912468802355,-1.39616839597726));
#112766=CARTESIAN_POINT('Ctrl Pts',(17.3908947210674,-20.588391614525,-1.39644270902803));
#112767=CARTESIAN_POINT('Ctrl Pts',(17.3806055911754,-20.5799098593907,
-1.39725672607667));
#112768=CARTESIAN_POINT('Ctrl Pts',(17.3738289215356,-20.5742520048436,
-1.39779863000167));
#112769=CARTESIAN_POINT('Ctrl Pts',(17.3242110073926,-20.5322964589429,
-1.40180781333197));
#112770=CARTESIAN_POINT('Ctrl Pts',(17.282797325454,-20.4943525903393,-1.40538257912108));
#112771=CARTESIAN_POINT('Ctrl Pts',(17.1985944106414,-20.4108083883091,
-1.41306225783972));
#112772=CARTESIAN_POINT('Ctrl Pts',(17.1562154909218,-20.3648650558648,
-1.41717756742601));
#112773=CARTESIAN_POINT('Ctrl Pts',(17.0452481667157,-20.23333592099,-1.42854452694169));
#112774=CARTESIAN_POINT('Ctrl Pts',(16.9811727592963,-20.1441848096651,
-1.43579413788716));
#112775=CARTESIAN_POINT('Ctrl Pts',(16.8955511281902,-20.0031241016455,
-1.44640313660375));
#112776=CARTESIAN_POINT('Ctrl Pts',(16.8686817957824,-19.9546689190305,
-1.44991078270719));
#112777=CARTESIAN_POINT('Ctrl Pts',(16.8282391775142,-19.874469582801,-1.45549436127309));
#112778=CARTESIAN_POINT('Ctrl Pts',(16.8134880371499,-19.8433520421174,
-1.4576091835182));
#112779=CARTESIAN_POINT('Ctrl Pts',(16.795105725082,-19.8019971329562,-1.46035436886814));
#112780=CARTESIAN_POINT('Ctrl Pts',(16.7907854995237,-19.7920735368376,
-1.46100825898826));
#112781=CARTESIAN_POINT('Ctrl Pts',(16.7838354397002,-19.7757686648256,
-1.46207482888022));
#112782=CARTESIAN_POINT('Ctrl Pts',(16.7811604113993,-19.7694069784057,
-1.46248904410319));
#112783=CARTESIAN_POINT('Ctrl Pts',(16.7760434438126,-19.7570694352098,
-1.46328866860384));
#112784=CARTESIAN_POINT('Ctrl Pts',(16.7735976392193,-19.7510952738546,
-1.46367420557897));
#112785=CARTESIAN_POINT('Ctrl Pts',(16.7680147558737,-19.7372785269574,
-1.46456207246422));
#112786=CARTESIAN_POINT('Ctrl Pts',(16.7648971978317,-19.7294281334439,
-1.46506373891318));
#112787=CARTESIAN_POINT('Ctrl Pts',(16.7566421296176,-19.7082726131605,
-1.4664082666197));
#112788=CARTESIAN_POINT('Ctrl Pts',(16.7515918954761,-19.6949337352172,
-1.46724820074698));
#112789=CARTESIAN_POINT('Ctrl Pts',(16.7462566539521,-19.6804002171314,
-1.4681552115446));
#112790=CARTESIAN_POINT('Ctrl Pts',(16.745837552997,-19.6792555054942,-1.46822659633938));
#112791=CARTESIAN_POINT('Ctrl Pts',(16.7454194501222,-19.6781104576079,
-1.46829794770746));
#112792=CARTESIAN_POINT('',(16.6170006157907,-18.95038529957,-0.489056278967188));
#112793=CARTESIAN_POINT('Ctrl Pts',(16.7454193881274,-19.6781102878244,
-1.24458621709267));
#112794=CARTESIAN_POINT('Ctrl Pts',(16.8018177033943,-19.832566984228,-1.23372059953188));
#112795=CARTESIAN_POINT('Ctrl Pts',(16.8760653146766,-19.9800494973809,
-1.22298084368604));
#112796=CARTESIAN_POINT('Ctrl Pts',(16.9785115316654,-20.1353880728159,
-1.21154550124883));
#112797=CARTESIAN_POINT('Ctrl Pts',(16.9905656874721,-20.1530761607974,
-1.21024028032419));
#112798=CARTESIAN_POINT('Ctrl Pts',(17.0076902625298,-20.1774033377812,
-1.20844022578061));
#112799=CARTESIAN_POINT('Ctrl Pts',(17.0125345191703,-20.1841993553649,
-1.20793681684617));
#112800=CARTESIAN_POINT('Ctrl Pts',(17.0209586919664,-20.1958709981426,
-1.20707124330506));
#112801=CARTESIAN_POINT('Ctrl Pts',(17.0245195218161,-20.2007602167504,
-1.20670834888374));
#112802=CARTESIAN_POINT('Ctrl Pts',(17.0319301924233,-20.2108443816476,
-1.20595919785515));
#112803=CARTESIAN_POINT('Ctrl Pts',(17.0357829816325,-20.2160370908435,
-1.2055730610832));
#112804=CARTESIAN_POINT('Ctrl Pts',(17.0448505163654,-20.228141837466,-1.20467201801022));
#112805=CARTESIAN_POINT('Ctrl Pts',(17.0500840206145,-20.2350397285979,
-1.20415785261978));
#112806=CARTESIAN_POINT('Ctrl Pts',(17.0671668213754,-20.2572707208069,
-1.20249829610703));
#112807=CARTESIAN_POINT('Ctrl Pts',(17.0791845743477,-20.2724735680331,
-1.20135956747992));
#112808=CARTESIAN_POINT('Ctrl Pts',(17.1414403955605,-20.3490441937779,
-1.19560092451776));
#112809=CARTESIAN_POINT('Ctrl Pts',(17.1948923638484,-20.4077225769487,
-1.19111361433064));
#112810=CARTESIAN_POINT('Ctrl Pts',(17.3679313979148,-20.5774658583777,
-1.17766507016939));
#112811=CARTESIAN_POINT('Ctrl Pts',(17.4971417822176,-20.6778211704038,
-1.16906404353162));
#112812=CARTESIAN_POINT('Ctrl Pts',(17.6888228912938,-20.7940168254065,
-1.1565347881372));
#112813=CARTESIAN_POINT('Ctrl Pts',(17.742406533583,-20.8234064506605,-1.15304834159926));
#112814=CARTESIAN_POINT('Ctrl Pts',(17.8053530517049,-20.8544686356864,
-1.14888518455534));
#112815=CARTESIAN_POINT('Ctrl Pts',(17.813551860981,-20.8584488666064,-1.14834164637157));
#112816=CARTESIAN_POINT('Ctrl Pts',(17.8258415152737,-20.8643173022009,
-1.14752461591503));
#112817=CARTESIAN_POINT('Ctrl Pts',(17.8299132262763,-20.8662456483934,
-1.14725355039542));
#112818=CARTESIAN_POINT('Ctrl Pts',(17.837219374842,-20.8696773012974,-1.1467664365007));
#112819=CARTESIAN_POINT('Ctrl Pts',(17.8404514818805,-20.8711854436304,
-1.14655069120268));
#112820=CARTESIAN_POINT('Ctrl Pts',(17.8474676197136,-20.8744376970473,
-1.14608179516534));
#112821=CARTESIAN_POINT('Ctrl Pts',(17.8512529429665,-20.8761787840357,
-1.14582846849364));
#112822=CARTESIAN_POINT('Ctrl Pts',(17.861859250324,-20.8810193481851,-1.14511773346867));
#112823=CARTESIAN_POINT('Ctrl Pts',(17.868691506005,-20.8840937708311,-1.1446588325517));
#112824=CARTESIAN_POINT('Ctrl Pts',(17.9088205241138,-20.9018957438009,
-1.14195787695079));
#112825=CARTESIAN_POINT('Ctrl Pts',(17.9424743184824,-20.915797674474,-1.13967023166682));
#112826=CARTESIAN_POINT('Ctrl Pts',(18.0526132122882,-20.9580036619708,
-1.13214925938801));
#112827=CARTESIAN_POINT('Ctrl Pts',(18.1303766047942,-20.9827574167094,
-1.12678910459031));
#112828=CARTESIAN_POINT('Ctrl Pts',(18.3869095222611,-21.0483780084675,
-1.10930507020568));
#112829=CARTESIAN_POINT('Ctrl Pts',(18.5696370504609,-21.0705570508792,
-1.09724050439611));
#112830=CARTESIAN_POINT('Ctrl Pts',(18.7752747831385,-21.0687152294627,
-1.08459112606208));
#112831=CARTESIAN_POINT('Ctrl Pts',(18.7975852188531,-21.0681625528546,
-1.08322945502247));
#112832=CARTESIAN_POINT('Ctrl Pts',(18.8283696560096,-21.066912646581,-1.08136475180797));
#112833=CARTESIAN_POINT('Ctrl Pts',(18.8368538201628,-21.0665170204114,
-1.08085232480144));
#112834=CARTESIAN_POINT('Ctrl Pts',(18.8514156250629,-21.0657501370288,
-1.07997530663869));
#112835=CARTESIAN_POINT('Ctrl Pts',(18.85749441757,-21.0654037003922,-1.07960994175069));
#112836=CARTESIAN_POINT('Ctrl Pts',(18.8700069918549,-21.0646364256818,
-1.07885937747905));
#112837=CARTESIAN_POINT('Ctrl Pts',(18.8764405208141,-21.0642124108148,
-1.07847428179653));
#112838=CARTESIAN_POINT('Ctrl Pts',(18.8913800445021,-21.0631592235079,
-1.07758189314619));
#112839=CARTESIAN_POINT('Ctrl Pts',(18.899884411973,-21.0625080219041,-1.07707529684525));
#112840=CARTESIAN_POINT('Ctrl Pts',(18.9269811211416,-21.060268359596,-1.07546547260716));
#112841=CARTESIAN_POINT('Ctrl Pts',(18.945556820596,-21.0584854459138,-1.07436835009053));
#112842=CARTESIAN_POINT('Ctrl Pts',(19.1238251993047,-21.0389931045081,
-1.06389558349427));
#112843=CARTESIAN_POINT('Ctrl Pts',(19.2810393471936,-21.0034044022969,
-1.05514839338973));
#112844=CARTESIAN_POINT('Ctrl Pts',(19.5595042799313,-20.9060389797379,
-1.03912865068673));
#112845=CARTESIAN_POINT('Ctrl Pts',(19.6817561718178,-20.8497549827405,
-1.03186595151421));
#112846=CARTESIAN_POINT('Ctrl Pts',(19.8113918545858,-20.7744054540267,
-1.02307441290294));
#112847=CARTESIAN_POINT('Ctrl Pts',(19.8248594179145,-20.7663760759782,
-1.02214689119972));
#112848=CARTESIAN_POINT('Ctrl Pts',(19.8431752333489,-20.7551785309911,
-1.02086416263513));
#112849=CARTESIAN_POINT('Ctrl Pts',(19.8481018917498,-20.7521387407391,
-1.02051699370807));
#112850=CARTESIAN_POINT('Ctrl Pts',(19.8559115710803,-20.7472757621879,
-1.01996316072993));
#112851=CARTESIAN_POINT('Ctrl Pts',(19.8588028021005,-20.7454657207846,
-1.01975735781224));
#112852=CARTESIAN_POINT('Ctrl Pts',(19.8647626891617,-20.7417144816413,
-1.01933150799062));
#112853=CARTESIAN_POINT('Ctrl Pts',(19.8678307177431,-20.7397723814043,
-1.01911139811555));
#112854=CARTESIAN_POINT('Ctrl Pts',(19.8751293409624,-20.7351259178681,
-1.01858566864822));
#112855=CARTESIAN_POINT('Ctrl Pts',(19.8793553252695,-20.732414387007,-1.01827957599067));
#112856=CARTESIAN_POINT('Ctrl Pts',(19.8935793752587,-20.7232161673964,
-1.01724370885702));
#112857=CARTESIAN_POINT('Ctrl Pts',(19.9035320866917,-20.7166602285876,
-1.01650952273431));
#112858=CARTESIAN_POINT('Ctrl Pts',(19.9273102998622,-20.700707797263,-1.01473382806373));
#112859=CARTESIAN_POINT('Ctrl Pts',(19.9410807094834,-20.691231024301,-1.0136876734955));
#112860=CARTESIAN_POINT('Ctrl Pts',(19.9923045130314,-20.655077542099,-1.00973306970564));
#112861=CARTESIAN_POINT('Ctrl Pts',(20.0289958667914,-20.6273472837901,
-1.00677231121293));
#112862=CARTESIAN_POINT('Ctrl Pts',(20.1225743842928,-20.5517117391419,
-0.998935572451693));
#112863=CARTESIAN_POINT('Ctrl Pts',(20.1778923894249,-20.5019647368871,
-0.994011769524073));
#112864=CARTESIAN_POINT('Ctrl Pts',(20.3402766587832,-20.3396818760092,
-0.978844830573222));
#112865=CARTESIAN_POINT('Ctrl Pts',(20.4376925866136,-20.2181887035235,
-0.968729192508623));
#112866=CARTESIAN_POINT('Ctrl Pts',(20.5337902831701,-20.0669067254841,
-0.957687395765254));
#112867=CARTESIAN_POINT('Ctrl Pts',(20.5462827863953,-20.0464830953269,
-0.956225129294907));
#112868=CARTESIAN_POINT('Ctrl Pts',(20.563346207969,-20.017493084651,-0.954188288628662));
#112869=CARTESIAN_POINT('Ctrl Pts',(20.5682083837791,-20.0091010698254,
-0.953603141143982));
#112870=CARTESIAN_POINT('Ctrl Pts',(20.5759803176351,-19.9954718001044,
-0.952659943306616));
#112871=CARTESIAN_POINT('Ctrl Pts',(20.5789257745204,-19.9902551593064,
-0.952300605547992));
#112872=CARTESIAN_POINT('Ctrl Pts',(20.5850180255667,-19.979357505265,-0.951553392589612));
#112873=CARTESIAN_POINT('Ctrl Pts',(20.5881609056978,-19.9736743668263,
-0.951165660915609));
#112874=CARTESIAN_POINT('Ctrl Pts',(20.5955277531521,-19.9602072475418,
-0.950251395307535));
#112875=CARTESIAN_POINT('Ctrl Pts',(20.5997291470569,-19.9524110071407,
-0.949725671690242));
#112876=CARTESIAN_POINT('Ctrl Pts',(20.6135042252298,-19.9264609146362,
-0.947987337117727));
#112877=CARTESIAN_POINT('Ctrl Pts',(20.6228630273264,-19.908193868702,-0.946782330914329));
#112878=CARTESIAN_POINT('Ctrl Pts',(20.6710793542249,-19.8106111351768,
-0.940438850966872));
#112879=CARTESIAN_POINT('Ctrl Pts',(20.7052127833459,-19.7290535594662,
-0.935466841537171));
#112880=CARTESIAN_POINT('Ctrl Pts',(20.7770356124094,-19.5219342745485,
-0.923366577005673));
#112881=CARTESIAN_POINT('Ctrl Pts',(20.8083554811537,-19.3945691508358,
-0.916389496580278));
#112882=CARTESIAN_POINT('Ctrl Pts',(20.8332930141252,-19.2278269740611,
-0.907089596115496));
#112883=CARTESIAN_POINT('Ctrl Pts',(20.8378738659814,-19.1903824739513,
-0.904989166941394));
#112884=CARTESIAN_POINT('Ctrl Pts',(20.845804004131,-19.1071688939514,-0.900257380576004));
#112885=CARTESIAN_POINT('Ctrl Pts',(20.8486701922348,-19.0613747650289,
-0.897610771994247));
#112886=CARTESIAN_POINT('Ctrl Pts',(20.8502754956742,-19.0079035291881,
-0.894433888747696));
#112887=CARTESIAN_POINT('Ctrl Pts',(20.850463173625,-19.0002784515828,-0.893978808073013));
#112888=CARTESIAN_POINT('Ctrl Pts',(20.8506981094217,-18.9880463513708,
-0.893245242277728));
#112889=CARTESIAN_POINT('Ctrl Pts',(20.8507715424004,-18.9834398193474,
-0.89296818350772));
#112890=CARTESIAN_POINT('Ctrl Pts',(20.8508753307636,-18.9752520947348,
-0.892474250722606));
#112891=CARTESIAN_POINT('Ctrl Pts',(20.8509116364345,-18.9716710254737,
-0.892257712695064));
#112892=CARTESIAN_POINT('Ctrl Pts',(20.8509695804583,-18.9640473296703,
-0.891795630695948));
#112893=CARTESIAN_POINT('Ctrl Pts',(20.8509887258639,-18.9600047904858,
-0.891549955828478));
#112894=CARTESIAN_POINT('Ctrl Pts',(20.8510092763643,-18.9490248631197,
-0.890880955692545));
#112895=CARTESIAN_POINT('Ctrl Pts',(20.8509881596246,-18.942087554154,-0.890456401136245));
#112896=CARTESIAN_POINT('Ctrl Pts',(20.8507068074548,-18.9067389251845,
-0.88828401798507));
#112897=CARTESIAN_POINT('Ctrl Pts',(20.849908728059,-18.8783362744689,-0.886508599459404));
#112898=CARTESIAN_POINT('Ctrl Pts',(20.8458846388466,-18.7949465021971,
-0.881224624397769));
#112899=CARTESIAN_POINT('Ctrl Pts',(20.8410841553577,-18.7400611889243,
-0.877655877078888));
#112900=CARTESIAN_POINT('Ctrl Pts',(20.8165299602159,-18.546613284839,-0.864885057049364));
#112901=CARTESIAN_POINT('Ctrl Pts',(20.7851879933606,-18.4098725167902,
-0.855533051259325));
#112902=CARTESIAN_POINT('Ctrl Pts',(20.7117633298357,-18.1915296121857,
-0.840658554401902));
#112903=CARTESIAN_POINT('Ctrl Pts',(20.6774831622946,-18.1077607332038,
-0.834959698999613));
#112904=CARTESIAN_POINT('Ctrl Pts',(20.6319419398103,-18.0140799685371,
-0.828603961796962));
#112905=CARTESIAN_POINT('Ctrl Pts',(20.6258176663965,-18.0017876430153,
-0.827770211360294));
#112906=CARTESIAN_POINT('Ctrl Pts',(20.6158033006481,-17.9821679874033,
-0.826439617841622));
#112907=CARTESIAN_POINT('Ctrl Pts',(20.6119890786087,-17.9748025692469,
-0.825940132343313));
#112908=CARTESIAN_POINT('Ctrl Pts',(20.605139317047,-17.9617636368225,-0.82505589389912));
#112909=CARTESIAN_POINT('Ctrl Pts',(20.6021210313848,-17.9560812220505,
-0.824670538119259));
#112910=CARTESIAN_POINT('Ctrl Pts',(20.5957777920921,-17.9442693433204,
-0.82386946804403));
#112911=CARTESIAN_POINT('Ctrl Pts',(20.5924483619717,-17.9381423614674,
-0.823453918618515));
#112912=CARTESIAN_POINT('Ctrl Pts',(20.5837221242851,-17.9222713311964,
-0.822377370762704));
#112913=CARTESIAN_POINT('Ctrl Pts',(20.578278534909,-17.9125531464928,-0.821718050165515));
#112914=CARTESIAN_POINT('Ctrl Pts',(20.5542933230677,-17.870515118424,-0.818864946127468));
#112915=CARTESIAN_POINT('Ctrl Pts',(20.5349762835991,-17.8386438096503,
-0.8166992301243));
#112916=CARTESIAN_POINT('Ctrl Pts',(20.481403120302,-17.7552994113448,-0.811013082640622));
#112917=CARTESIAN_POINT('Ctrl Pts',(20.4457162163399,-17.7047877418501,
-0.807543794594892));
#112918=CARTESIAN_POINT('Ctrl Pts',(20.3211978524967,-17.5439757539065,
-0.796291211123318));
#112919=CARTESIAN_POINT('Ctrl Pts',(20.2235242093855,-17.4410252810488,
-0.788766688059283));
#112920=CARTESIAN_POINT('Ctrl Pts',(20.0589236171188,-17.2991214866803,
-0.77673606087605));
#112921=CARTESIAN_POINT('Ctrl Pts',(19.998927949183,-17.2527693896341,-0.772455130894074));
#112922=CARTESIAN_POINT('Ctrl Pts',(19.9287599195456,-17.204336377034,-0.767402196982563));
#112923=CARTESIAN_POINT('Ctrl Pts',(19.9208987289038,-17.1989880764515,
-0.766835464318208));
#112924=CARTESIAN_POINT('Ctrl Pts',(19.9091922916748,-17.1911385300126,
-0.765990160622017));
#112925=CARTESIAN_POINT('Ctrl Pts',(19.905374388484,-17.1885964500448,-0.765714263548012));
#112926=CARTESIAN_POINT('Ctrl Pts',(19.8985613166124,-17.1840919814935,
-0.765221489398647));
#112927=CARTESIAN_POINT('Ctrl Pts',(19.8955694031899,-17.1821247661727,
-0.765004940084503));
#112928=CARTESIAN_POINT('Ctrl Pts',(19.8891167829349,-17.1779055082966,
-0.764537575181715));
#112929=CARTESIAN_POINT('Ctrl Pts',(19.885654518553,-17.1756560251639,-0.764286600560479));
#112930=CARTESIAN_POINT('Ctrl Pts',(19.8760707030928,-17.1694690783995,
-0.763591375973212));
#112931=CARTESIAN_POINT('Ctrl Pts',(19.869935459412,-17.1655530777967,-0.76314574640617));
#112932=CARTESIAN_POINT('Ctrl Pts',(19.8360557010601,-17.1441734118384,
-0.76068232189865));
#112933=CARTESIAN_POINT('Ctrl Pts',(19.8079302154371,-17.1273254097837,
-0.758627825383906));
#112934=CARTESIAN_POINT('Ctrl Pts',(19.637111887861,-17.0303175488475,-0.746145431491577));
#112935=CARTESIAN_POINT('Ctrl Pts',(19.4859089384337,-16.9662739910768,
-0.735128286201479));
#112936=CARTESIAN_POINT('Ctrl Pts',(19.2190442627122,-16.8881421578079,
-0.716988267455996));
#112937=CARTESIAN_POINT('Ctrl Pts',(19.1068116667028,-16.8649456380465,
-0.709708815586819));
#112938=CARTESIAN_POINT('Ctrl Pts',(18.9790782211547,-16.8491854089419,
-0.701850773645383));
#112939=CARTESIAN_POINT('Ctrl Pts',(18.9649013265773,-16.8475815216944,
-0.700984207421549));
#112940=CARTESIAN_POINT('Ctrl Pts',(18.9422949865791,-16.8452551781684,
-0.699611052341453));
#112941=CARTESIAN_POINT('Ctrl Pts',(18.9338757416618,-16.8444397430016,
-0.699101558925369));
#112942=CARTESIAN_POINT('Ctrl Pts',(18.9190082003776,-16.8430896587684,
-0.69820514700346));
#112943=CARTESIAN_POINT('Ctrl Pts',(18.9125619584257,-16.8425340746999,
-0.69781757632356));
#112944=CARTESIAN_POINT('Ctrl Pts',(18.8992136717395,-16.8414452475454,
-0.69701725563942));
#112945=CARTESIAN_POINT('Ctrl Pts',(18.8923113478295,-16.8409162879381,
-0.6966046444111));
#112946=CARTESIAN_POINT('Ctrl Pts',(18.8745658966637,-16.8396438862354,
-0.695546941577965));
#112947=CARTESIAN_POINT('Ctrl Pts',(18.8637193293942,-16.8389500656871,
-0.694903409364044));
#112948=CARTESIAN_POINT('Ctrl Pts',(18.8182406794367,-16.8363924433478,
-0.692217110239066));
#112949=CARTESIAN_POINT('Ctrl Pts',(18.7835696528897,-16.8352962233687,
-0.69019837930424));
#112950=CARTESIAN_POINT('Ctrl Pts',(18.693002206864,-16.8346593773351,-0.684989112666923));
#112951=CARTESIAN_POINT('Ctrl Pts',(18.6371224131308,-16.8364793706412,
-0.681839177258327));
#112952=CARTESIAN_POINT('Ctrl Pts',(18.3834474860446,-16.8548155386015,
-0.667705158163168));
#112953=CARTESIAN_POINT('Ctrl Pts',(18.1885440452532,-16.896877579339,-0.657394732512601));
#112954=CARTESIAN_POINT('Ctrl Pts',(17.9724290817017,-16.9764704756795,
-0.644170672438002));
#112955=CARTESIAN_POINT('Ctrl Pts',(17.9427414385785,-16.9881729180789,
-0.642310099739248));
#112956=CARTESIAN_POINT('Ctrl Pts',(17.9070460604945,-17.0031842892043,
-0.640006155137102));
#112957=CARTESIAN_POINT('Ctrl Pts',(17.90077359204,-17.0058578564428,-0.63959876083637));
#112958=CARTESIAN_POINT('Ctrl Pts',(17.8904623225333,-17.0103119024413,
-0.638924681610809));
#112959=CARTESIAN_POINT('Ctrl Pts',(17.8864159253901,-17.0120748166069,
-0.638659043197406));
#112960=CARTESIAN_POINT('Ctrl Pts',(17.879124972349,-17.0152784686418,-0.638178343238376));
#112961=CARTESIAN_POINT('Ctrl Pts',(17.8758784976345,-17.0167147264671,
-0.637963557868887));
#112962=CARTESIAN_POINT('Ctrl Pts',(17.8695669221827,-17.0195260056022,
-0.63754452175214));
#112963=CARTESIAN_POINT('Ctrl Pts',(17.866501524906,-17.0209001371259,-0.637340333511754));
#112964=CARTESIAN_POINT('Ctrl Pts',(17.8574579487995,-17.0249799969133,
-0.636735978479423));
#112965=CARTESIAN_POINT('Ctrl Pts',(17.8514891312339,-17.0277062013054,
-0.636334570302513));
#112966=CARTESIAN_POINT('Ctrl Pts',(17.8231334872806,-17.0408170654135,
-0.63441590105685));
#112967=CARTESIAN_POINT('Ctrl Pts',(17.8009177279784,-17.0515644280766,
-0.632877779752791));
#112968=CARTESIAN_POINT('Ctrl Pts',(17.738720024919,-17.0830073851841,-0.628482638598404));
#112969=CARTESIAN_POINT('Ctrl Pts',(17.699204538176,-17.1045927760092,-0.625584859587855));
#112970=CARTESIAN_POINT('Ctrl Pts',(17.5784806017701,-17.1756272124288,
-0.616463122397769));
#112971=CARTESIAN_POINT('Ctrl Pts',(17.4998931148633,-17.2292971844216,
-0.610137970553651));
#112972=CARTESIAN_POINT('Ctrl Pts',(17.307368059534,-17.3807338437067,-0.593981628709136));
#112973=CARTESIAN_POINT('Ctrl Pts',(17.199711591409,-17.4856674460666,-0.584307127741038));
#112974=CARTESIAN_POINT('Ctrl Pts',(17.0950142926375,-17.6119945888665,
-0.574290992265421));
#112975=CARTESIAN_POINT('Ctrl Pts',(17.086106874914,-17.6229639153124,-0.573432878400448));
#112976=CARTESIAN_POINT('Ctrl Pts',(17.072093705984,-17.6405783798368,-0.572073056529783));
#112977=CARTESIAN_POINT('Ctrl Pts',(17.0669165480973,-17.6471659249212,
-0.571568472289585));
#112978=CARTESIAN_POINT('Ctrl Pts',(17.0578486721638,-17.6588461827973,
-0.570680710981957));
#112979=CARTESIAN_POINT('Ctrl Pts',(17.0539417418264,-17.6639261204009,
-0.570296888066272));
#112980=CARTESIAN_POINT('Ctrl Pts',(17.0459029806981,-17.6744772186052,
-0.569504345809204));
#112981=CARTESIAN_POINT('Ctrl Pts',(17.0417745351756,-17.6799508730127,
-0.569095763517996));
#112982=CARTESIAN_POINT('Ctrl Pts',(17.0312343077408,-17.6940676455551,
-0.568048528131414));
#112983=CARTESIAN_POINT('Ctrl Pts',(17.0248616579755,-17.7027398407741,
-0.56741141622733));
#112984=CARTESIAN_POINT('Ctrl Pts',(16.9984537680377,-17.739257234796,-0.564754091848449));
#112985=CARTESIAN_POINT('Ctrl Pts',(16.979030031329,-17.7675396399212,-0.562757572942994));
#112986=CARTESIAN_POINT('Ctrl Pts',(16.9301570456348,-17.8425458372623,
-0.55760883954137));
#112987=CARTESIAN_POINT('Ctrl Pts',(16.9018328811112,-17.8899725785667,
-0.554496496736844));
#112988=CARTESIAN_POINT('Ctrl Pts',(16.8405517958169,-18.0023478892813,
-0.547383536926009));
#112989=CARTESIAN_POINT('Ctrl Pts',(16.8090263232568,-18.067996473509,-0.543420742657022));
#112990=CARTESIAN_POINT('Ctrl Pts',(16.7673556016827,-18.1676283178345,
-0.537557188721337));
#112991=CARTESIAN_POINT('Ctrl Pts',(16.7545802832847,-18.2004504712821,
-0.535648363153797));
#112992=CARTESIAN_POINT('Ctrl Pts',(16.7287365521522,-18.2720856476005,
-0.531505691853217));
#112993=CARTESIAN_POINT('Ctrl Pts',(16.7159637403136,-18.3109894545521,
-0.529270380739138));
#112994=CARTESIAN_POINT('Ctrl Pts',(16.6989488456493,-18.3683787119344,
-0.525964161640086));
#112995=CARTESIAN_POINT('Ctrl Pts',(16.6938140192241,-18.3865902848655,
-0.524913687915817));
#112996=CARTESIAN_POINT('Ctrl Pts',(16.6732969948426,-18.4632790246769,
-0.520475810133252));
#112997=CARTESIAN_POINT('Ctrl Pts',(16.6601810645928,-18.5223272734326,
-0.517024246174424));
#112998=CARTESIAN_POINT('Ctrl Pts',(16.6480273156646,-18.5907673934646,
-0.512901039303712));
#112999=CARTESIAN_POINT('Ctrl Pts',(16.6465009452968,-18.5996951238406,
-0.51236080294181));
#113000=CARTESIAN_POINT('Ctrl Pts',(16.644305601677,-18.6130510721475,-0.511548680017965));
#113001=CARTESIAN_POINT('Ctrl Pts',(16.6435932922695,-18.6174721992162,
-0.511279207093751));
#113002=CARTESIAN_POINT('Ctrl Pts',(16.6423403650114,-18.625409087299,-0.510794240062401));
#113003=CARTESIAN_POINT('Ctrl Pts',(16.6417945762315,-18.6289239762063,
-0.510579043265837));
#113004=CARTESIAN_POINT('Ctrl Pts',(16.6407479422931,-18.6357782032962,
-0.510158565565197));
#113005=CARTESIAN_POINT('Ctrl Pts',(16.6402462293206,-18.6391173555435,
-0.509953340961359));
#113006=CARTESIAN_POINT('Ctrl Pts',(16.6391504857787,-18.6465307459401,
-0.509496887874436));
#113007=CARTESIAN_POINT('Ctrl Pts',(16.6385603498353,-18.6506055337683,
-0.50924544453661));
#113008=CARTESIAN_POINT('Ctrl Pts',(16.6371204756496,-18.6607562875997,
-0.508617738797099));
#113009=CARTESIAN_POINT('Ctrl Pts',(16.6362852620975,-18.6668342307324,
-0.508240701530483));
#113010=CARTESIAN_POINT('Ctrl Pts',(16.6323977830372,-18.6960654138083,
-0.5064219570469));
#113011=CARTESIAN_POINT('Ctrl Pts',(16.6297024906904,-18.7192634938548,
-0.504962249722664));
#113012=CARTESIAN_POINT('Ctrl Pts',(16.6205187004321,-18.8116103989568,
-0.499098991253069));
#113013=CARTESIAN_POINT('Ctrl Pts',(16.6170514726509,-18.881010439068,-0.494577327914004));
#113014=CARTESIAN_POINT('Ctrl Pts',(16.6170005688548,-18.9504480557866,
-0.49001046713057));
#113015=CARTESIAN_POINT('Ctrl Pts',(16.6170006157907,-18.95038529957,-0.489056278967188));
#113016=CARTESIAN_POINT('Ctrl Pts',(16.6169459705064,-19.0220295693798,
-0.484732818390677));
#113017=CARTESIAN_POINT('Ctrl Pts',(16.620532458768,-19.0938083580375,-0.480409357814167));
#113018=CARTESIAN_POINT('Ctrl Pts',(16.6277745422071,-19.1653150743503,
-0.476085897237656));
#113019=CARTESIAN_POINT('Ctrl Pts',(16.6350090271023,-19.2367467643357,
-0.471766972925506));
#113020=CARTESIAN_POINT('Ctrl Pts',(16.6458914554201,-19.3079064569402,
-0.467448048613356));
#113021=CARTESIAN_POINT('Ctrl Pts',(16.6603842666415,-19.3783880748427,
-0.463129124301205));
#113022=CARTESIAN_POINT('Ctrl Pts',(16.6748666504828,-19.4488189821819,
-0.458813307396227));
#113023=CARTESIAN_POINT('Ctrl Pts',(16.6929541651561,-19.5185722974559,
-0.454497490491248));
#113024=CARTESIAN_POINT('Ctrl Pts',(16.7145577237479,-19.5872494729519,
-0.45018167358627));
#113025=CARTESIAN_POINT('Ctrl Pts',(16.7241553569732,-19.6177601102879,
-0.448264321519214));
#113026=CARTESIAN_POINT('Ctrl Pts',(16.7344462702044,-19.6480584841912,
-0.446346969452159));
#113027=CARTESIAN_POINT('Ctrl Pts',(16.7454194499637,-19.6781104571739,
-0.444429617385103));
#113028=CARTESIAN_POINT('Origin',(-18.734,-18.952,0.));
#113029=CARTESIAN_POINT('',(-20.8509997094775,-18.9508909138291,-0.710943720977502));
#113030=CARTESIAN_POINT('Ctrl Pts',(-20.7225805821191,-19.6781103693095,
-0.666446455478431));
#113031=CARTESIAN_POINT('Ctrl Pts',(-20.7478889918429,-19.6087988510222,
-0.670880806094382));
#113032=CARTESIAN_POINT('Ctrl Pts',(-20.7695971667487,-19.5380870993955,
-0.675315156710334));
#113033=CARTESIAN_POINT('Ctrl Pts',(-20.7875590822766,-19.4663773863607,
-0.679749507326285));
#113034=CARTESIAN_POINT('Ctrl Pts',(-20.8055066130117,-19.3947251020211,
-0.684180306694308));
#113035=CARTESIAN_POINT('Ctrl Pts',(-20.8197137318595,-19.3220768932863,
-0.68861110606233));
#113036=CARTESIAN_POINT('Ctrl Pts',(-20.8300841804326,-19.2488503133574,
-0.693041905430352));
#113037=CARTESIAN_POINT('Ctrl Pts',(-20.8404495313235,-19.175659728576,
-0.697470526801298));
#113038=CARTESIAN_POINT('Ctrl Pts',(-20.8469818946778,-19.1018917970174,
-0.701899148172244));
#113039=CARTESIAN_POINT('Ctrl Pts',(-20.8496363361419,-19.0279729767482,
-0.70632776954319));
#113040=CARTESIAN_POINT('Ctrl Pts',(-20.8505585774639,-19.0022911180789,
-0.707866420021294));
#113041=CARTESIAN_POINT('Ctrl Pts',(-20.8510131736829,-18.9765910979418,
-0.709405070499398));
#113042=CARTESIAN_POINT('Ctrl Pts',(-20.8509997094775,-18.9508909138291,
-0.710943720977502));
#113043=CARTESIAN_POINT('Ctrl Pts',(-20.8509997572023,-18.9509860940746,
-0.712619188017889));
#113044=CARTESIAN_POINT('Ctrl Pts',(-20.850964631018,-18.8776438618634,
-0.716785661483279));
#113045=CARTESIAN_POINT('Ctrl Pts',(-20.8471182042979,-18.8043479163262,
-0.720847520086871));
#113046=CARTESIAN_POINT('Ctrl Pts',(-20.8225250941853,-18.5696299416392,
-0.733763884425625));
#113047=CARTESIAN_POINT('Ctrl Pts',(-20.7869923924286,-18.4103781101525,
-0.742358139260776));
#113048=CARTESIAN_POINT('Ctrl Pts',(-20.7229676898254,-18.2262294227371,
-0.753553850662875));
#113049=CARTESIAN_POINT('Ctrl Pts',(-20.7116463931708,-18.1959246812705,
-0.755440714754925));
#113050=CARTESIAN_POINT('Ctrl Pts',(-20.6969536994598,-18.1591860537959,
-0.757796644379626));
#113051=CARTESIAN_POINT('Ctrl Pts',(-20.6942371115394,-18.1524928751802,
-0.758228674046915));
#113052=CARTESIAN_POINT('Ctrl Pts',(-20.6899236894109,-18.1420195311309,
-0.758909328814416));
#113053=CARTESIAN_POINT('Ctrl Pts',(-20.6883499983137,-18.1382298099701,
-0.75915657360869));
#113054=CARTESIAN_POINT('Ctrl Pts',(-20.6853861958599,-18.1311506425931,
-0.75962025348826));
#113055=CARTESIAN_POINT('Ctrl Pts',(-20.6839987756849,-18.1278601289272,
-0.759836524939919));
#113056=CARTESIAN_POINT('Ctrl Pts',(-20.6808111784495,-18.1203532880343,
-0.760331610884589));
#113057=CARTESIAN_POINT('Ctrl Pts',(-20.6790056308094,-18.1161392979295,
-0.760610749093168));
#113058=CARTESIAN_POINT('Ctrl Pts',(-20.6734109853909,-18.1031981677212,
-0.761471662144984));
#113059=CARTESIAN_POINT('Ctrl Pts',(-20.6695767924482,-18.0944908201619,
-0.762056084851175));
#113060=CARTESIAN_POINT('Ctrl Pts',(-20.6165813810053,-17.9763061593527,
-0.77005598901314));
#113061=CARTESIAN_POINT('Ctrl Pts',(-20.5582617224411,-17.871188441333,
-0.777951515509893));
#113062=CARTESIAN_POINT('Ctrl Pts',(-20.4306702152987,-17.6812337367286,
-0.793068874262596));
#113063=CARTESIAN_POINT('Ctrl Pts',(-20.363095503531,-17.5956858642857,
-0.800262887893773));
#113064=CARTESIAN_POINT('Ctrl Pts',(-20.252283159863,-17.4756965346801,
-0.810755849071076));
#113065=CARTESIAN_POINT('Ctrl Pts',(-20.2137969225058,-17.4371212794387,
-0.814203379954689));
#113066=CARTESIAN_POINT('Ctrl Pts',(-20.1572924335114,-17.3846970365266,
-0.818993217678231));
#113067=CARTESIAN_POINT('Ctrl Pts',(-20.1404764348063,-17.3695891713637,
-0.820386945875824));
#113068=CARTESIAN_POINT('Ctrl Pts',(-20.114318725804,-17.3468349724094,
-0.822507372087951));
#113069=CARTESIAN_POINT('Ctrl Pts',(-20.1051486143512,-17.3389947187231,
-0.823242027532029));
#113070=CARTESIAN_POINT('Ctrl Pts',(-20.0880140846261,-17.3245967695061,
-0.824598863731232));
#113071=CARTESIAN_POINT('Ctrl Pts',(-20.0800678308926,-17.3180181101005,
-0.825221892191775));
#113072=CARTESIAN_POINT('Ctrl Pts',(-20.0669001276875,-17.307277889046,
-0.826244239948318));
#113073=CARTESIAN_POINT('Ctrl Pts',(-20.0617065809242,-17.3030825341428,
-0.826644924850156));
#113074=CARTESIAN_POINT('Ctrl Pts',(-20.0514495199719,-17.2948767448298,
-0.827431313417878));
#113075=CARTESIAN_POINT('Ctrl Pts',(-20.0463873291951,-17.2908647797079,
-0.827817076068002));
#113076=CARTESIAN_POINT('Ctrl Pts',(-20.0346550516866,-17.281653642031,
-0.828705779615124));
#113077=CARTESIAN_POINT('Ctrl Pts',(-20.0279719855212,-17.2764711214339,
-0.82920805457678));
#113078=CARTESIAN_POINT('Ctrl Pts',(-20.0099118661412,-17.2626385338318,
-0.830554923825369));
#113079=CARTESIAN_POINT('Ctrl Pts',(-19.9984778539664,-17.2540633035146,
-0.831396577707444));
#113080=CARTESIAN_POINT('Ctrl Pts',(-19.8930995769677,-17.1766870392063,
-0.839055562750339));
#113081=CARTESIAN_POINT('Ctrl Pts',(-19.7937099858338,-17.1156264259946,
-0.845558675082553));
#113082=CARTESIAN_POINT('Ctrl Pts',(-19.5445352122423,-16.9895467831458,
-0.860849606959898));
#113083=CARTESIAN_POINT('Ctrl Pts',(-19.39130540912,-16.933057766199,-0.869452606281301));
#113084=CARTESIAN_POINT('Ctrl Pts',(-19.2014072603363,-16.8869853199322,
-0.880671120996706));
#113085=CARTESIAN_POINT('Ctrl Pts',(-19.1695035487123,-16.8800223045043,
-0.882575372180294));
#113086=CARTESIAN_POINT('Ctrl Pts',(-19.1303340925041,-16.8724180984619,
-0.884951048685638));
#113087=CARTESIAN_POINT('Ctrl Pts',(-19.1232076227952,-16.8710725574915,
-0.885384795887963));
#113088=CARTESIAN_POINT('Ctrl Pts',(-19.1120279494661,-16.8690211726241,
-0.886067813576971));
#113089=CARTESIAN_POINT('Ctrl Pts',(-19.1079792850815,-16.8682904666097,
-0.886315693419612));
#113090=CARTESIAN_POINT('Ctrl Pts',(-19.1004106025692,-16.8669472342115,
-0.88678011651294));
#113091=CARTESIAN_POINT('Ctrl Pts',(-19.0968911554678,-16.8663318158353,
-0.886996493281382));
#113092=CARTESIAN_POINT('Ctrl Pts',(-19.0888568438837,-16.8649478696211,
-0.887491394053295));
#113093=CARTESIAN_POINT('Ctrl Pts',(-19.0843410509844,-16.8641850844352,
-0.887770238752649));
#113094=CARTESIAN_POINT('Ctrl Pts',(-19.0704611381452,-16.8618868577665,
-0.888629316287147));
#113095=CARTESIAN_POINT('Ctrl Pts',(-19.0610892909,-16.8603997435232,-0.889212180646249));
#113096=CARTESIAN_POINT('Ctrl Pts',(-18.9323061362925,-16.8408512679557,
-0.897257144669816));
#113097=CARTESIAN_POINT('Ctrl Pts',(-18.8115857524508,-16.8329794704031,
-0.905205339547631));
#113098=CARTESIAN_POINT('Ctrl Pts',(-18.5117666877223,-16.8390891261654,
-0.925017373247488));
#113099=CARTESIAN_POINT('Ctrl Pts',(-18.3338128414782,-16.8654584894827,
-0.936778359655229));
#113100=CARTESIAN_POINT('Ctrl Pts',(-18.1406018114183,-16.919752677353,
-0.949107327055617));
#113101=CARTESIAN_POINT('Ctrl Pts',(-18.1200073978207,-16.9258796362289,
-0.950416984134922));
#113102=CARTESIAN_POINT('Ctrl Pts',(-18.0908984537672,-16.9350243273827,
-0.952262298924337));
#113103=CARTESIAN_POINT('Ctrl Pts',(-18.0823049836019,-16.9377845020349,
-0.952806346304224));
#113104=CARTESIAN_POINT('Ctrl Pts',(-18.067525618235,-16.9426360380585,
-0.953740848063025));
#113105=CARTESIAN_POINT('Ctrl Pts',(-18.0613313149609,-16.9447011994352,
-0.95413215877235));
#113106=CARTESIAN_POINT('Ctrl Pts',(-18.0494997399287,-16.9487067274606,
-0.954878945147));
#113107=CARTESIAN_POINT('Ctrl Pts',(-18.0438609256574,-16.9506423105741,
-0.955234574450041));
#113108=CARTESIAN_POINT('Ctrl Pts',(-18.0292418495597,-16.9557295960538,
-0.956155880435101));
#113109=CARTESIAN_POINT('Ctrl Pts',(-18.0202744665804,-16.9589181041099,
-0.9567203321157));
#113110=CARTESIAN_POINT('Ctrl Pts',(-17.9898855188329,-16.9699548183433,
-0.958631094151841));
#113111=CARTESIAN_POINT('Ctrl Pts',(-17.9685689674468,-16.978088943957,
-0.95996788295131));
#113112=CARTESIAN_POINT('Ctrl Pts',(-17.7822653249788,-17.0526520215882,
-0.971630642283501));
#113113=CARTESIAN_POINT('Ctrl Pts',(-17.6261311732976,-17.1392797013109,
-0.981181748730143));
#113114=CARTESIAN_POINT('Ctrl Pts',(-17.413782395421,-17.2948923701231,
-0.995511430765395));
#113115=CARTESIAN_POINT('Ctrl Pts',(-17.3480296005977,-17.3494819905999,
-1.0001909121203));
#113116=CARTESIAN_POINT('Ctrl Pts',(-17.2584705224172,-17.4334805280647,
-1.00720431964912));
#113117=CARTESIAN_POINT('Ctrl Pts',(-17.2318680831641,-17.4597909184569,
-1.00937813157564));
#113118=CARTESIAN_POINT('Ctrl Pts',(-17.2007546230231,-17.4922381763028,
-1.01205292551249));
#113119=CARTESIAN_POINT('Ctrl Pts',(-17.1955599921347,-17.4977138155592,
-1.01250411152458));
#113120=CARTESIAN_POINT('Ctrl Pts',(-17.1875363651409,-17.5062625852512,
-1.01320843434943));
#113121=CARTESIAN_POINT('Ctrl Pts',(-17.184686936081,-17.5093165712382,
-1.01346003182036));
#113122=CARTESIAN_POINT('Ctrl Pts',(-17.179423070408,-17.5149919029403,
-1.01392759838447));
#113123=CARTESIAN_POINT('Ctrl Pts',(-17.1770062080904,-17.5176109201461,
-1.01414337740842));
#113124=CARTESIAN_POINT('Ctrl Pts',(-17.1715619136192,-17.5235405670129,
-1.01463193342264));
#113125=CARTESIAN_POINT('Ctrl Pts',(-17.168538402035,-17.5268547056869,
-1.0149049996497));
#113126=CARTESIAN_POINT('Ctrl Pts',(-17.1596586959676,-17.5366503035713,
-1.01571205547905));
#113127=CARTESIAN_POINT('Ctrl Pts',(-17.1538321408568,-17.543158335492,
-1.01624819093665));
#113128=CARTESIAN_POINT('Ctrl Pts',(-17.1124198293643,-17.5899943291057,
-1.02010494607336));
#113129=CARTESIAN_POINT('Ctrl Pts',(-17.0783450568244,-17.6316260577086,
-1.02352424029672));
#113130=CARTESIAN_POINT('Ctrl Pts',(-16.9526015051071,-17.79778590453,-1.03699530452035));
#113131=CARTESIAN_POINT('Ctrl Pts',(-16.8730915694235,-17.9309151274526,
-1.04738335034069));
#113132=CARTESIAN_POINT('Ctrl Pts',(-16.770102185504,-18.1561071343316,
-1.06345670520847));
#113133=CARTESIAN_POINT('Ctrl Pts',(-16.7370305857035,-18.2431578468464,
-1.06935955476122));
#113134=CARTESIAN_POINT('Ctrl Pts',(-16.7036093562023,-18.3522931717415,
-1.07636851192662));
#113135=CARTESIAN_POINT('Ctrl Pts',(-16.6977313051731,-18.3725655348653,
-1.07765472999939));
#113136=CARTESIAN_POINT('Ctrl Pts',(-16.6897908267291,-18.4015654913221,
-1.079472958303));
#113137=CARTESIAN_POINT('Ctrl Pts',(-16.68747929468,-18.4102230172991,-1.08001302979415));
#113138=CARTESIAN_POINT('Ctrl Pts',(-16.6835816992291,-18.4252018784276,
-1.0809427958372));
#113139=CARTESIAN_POINT('Ctrl Pts',(-16.6819697422263,-18.431516290664,
-1.0813333245803));
#113140=CARTESIAN_POINT('Ctrl Pts',(-16.6789360176397,-18.4436332841626,
-1.0820800471102));
#113141=CARTESIAN_POINT('Ctrl Pts',(-16.6775096067372,-18.449434628222,
-1.08243638763739));
#113142=CARTESIAN_POINT('Ctrl Pts',(-16.6738576842075,-18.4645632476118,
-1.08336263296591));
#113143=CARTESIAN_POINT('Ctrl Pts',(-16.6716709374437,-18.4738998104669,
-1.08393128542887));
#113144=CARTESIAN_POINT('Ctrl Pts',(-16.6643984342844,-18.505929184234,
-1.08587214324255));
#113145=CARTESIAN_POINT('Ctrl Pts',(-16.659623081995,-18.528691272768,-1.08723440551242));
#113146=CARTESIAN_POINT('Ctrl Pts',(-16.622759356728,-18.7200441334948,
-1.09855503281612));
#113147=CARTESIAN_POINT('Ctrl Pts',(-16.6109048184111,-18.8918811289625,
-1.1078004019157));
#113148=CARTESIAN_POINT('Ctrl Pts',(-16.6246444007161,-19.1529064185535,
-1.12201427758092));
#113149=CARTESIAN_POINT('Ctrl Pts',(-16.6350568150434,-19.2421368322252,
-1.12691916895212));
#113150=CARTESIAN_POINT('Ctrl Pts',(-16.6579819809965,-19.3683185976219,
-1.13423619678522));
#113151=CARTESIAN_POINT('Ctrl Pts',(-16.6658979423526,-19.4060104066427,
-1.13647194471781));
#113152=CARTESIAN_POINT('Ctrl Pts',(-16.6766033184645,-19.4508645143586,
-1.1392153657923));
#113153=CARTESIAN_POINT('Ctrl Pts',(-16.678409801845,-19.4582566959017,
-1.13967021507414));
#113154=CARTESIAN_POINT('Ctrl Pts',(-16.6812727194323,-19.4697038432969,
-1.14037902080438));
#113155=CARTESIAN_POINT('Ctrl Pts',(-16.6823014258713,-19.4737657692599,
-1.14063140598727));
#113156=CARTESIAN_POINT('Ctrl Pts',(-16.6842271484725,-19.4812758749446,
-1.14109970022834));
#113157=CARTESIAN_POINT('Ctrl Pts',(-16.6851208128819,-19.4847248545684,
-1.14131541449824));
#113158=CARTESIAN_POINT('Ctrl Pts',(-16.6871551199814,-19.4924951543287,
-1.14180287078307));
#113159=CARTESIAN_POINT('Ctrl Pts',(-16.6883007361917,-19.4968151025053,
-1.14207489622946));
#113160=CARTESIAN_POINT('Ctrl Pts',(-16.6917051437054,-19.50949048039,-1.14287599382586));
#113161=CARTESIAN_POINT('Ctrl Pts',(-16.6940014761971,-19.5178356057865,
-1.14340716516022));
#113162=CARTESIAN_POINT('Ctrl Pts',(-16.7104124668958,-19.576076357016,
-1.14713933633344));
#113163=CARTESIAN_POINT('Ctrl Pts',(-16.7263038615,-19.6254486306065,-1.1504320728655));
#113164=CARTESIAN_POINT('Ctrl Pts',(-16.7513457188333,-19.6944526689545,
-1.15517165026876));
#113165=CARTESIAN_POINT('Ctrl Pts',(-16.7590107151941,-19.7146081857888,
-1.15657311590473));
#113166=CARTESIAN_POINT('Ctrl Pts',(-16.7840719944143,-19.7775947722123,
-1.16099997778447));
#113167=CARTESIAN_POINT('Ctrl Pts',(-16.8025638202033,-19.8199746764711,
-1.16404776532646));
#113168=CARTESIAN_POINT('Ctrl Pts',(-16.8694205396727,-19.9604599662169,
-1.17432515973072));
#113169=CARTESIAN_POINT('Ctrl Pts',(-16.9239979012258,-20.0554237337135,
-1.18155611709649));
#113170=CARTESIAN_POINT('Ctrl Pts',(-17.0167265964488,-20.1912312064795,
-1.19212597824787));
#113171=CARTESIAN_POINT('Ctrl Pts',(-17.0495457919176,-20.2354861769175,
-1.19561326428979));
#113172=CARTESIAN_POINT('Ctrl Pts',(-17.1055411522579,-20.3051395539879,
-1.20116826928217));
#113173=CARTESIAN_POINT('Ctrl Pts',(-17.1276733761538,-20.3313403731348,
-1.2032743795307));
#113174=CARTESIAN_POINT('Ctrl Pts',(-17.1576060241161,-20.3650774337534,
-1.20601011230233));
#113175=CARTESIAN_POINT('Ctrl Pts',(-17.164840526552,-20.3731067358428,
-1.20666305704469));
#113176=CARTESIAN_POINT('Ctrl Pts',(-17.1767928496026,-20.3861696113741,
-1.20772850138904));
#113177=CARTESIAN_POINT('Ctrl Pts',(-17.1814742821618,-20.3912360753681,
-1.20814252985013));
#113178=CARTESIAN_POINT('Ctrl Pts',(-17.190585789053,-20.4010007832985,
-1.20894208165084));
#113179=CARTESIAN_POINT('Ctrl Pts',(-17.1950127547054,-20.4057018115139,
-1.20932773118715));
#113180=CARTESIAN_POINT('Ctrl Pts',(-17.2052865024455,-20.4165120509319,
-1.21021626879744));
#113181=CARTESIAN_POINT('Ctrl Pts',(-17.2111485424769,-20.4226066593126,
-1.21071849047337));
#113182=CARTESIAN_POINT('Ctrl Pts',(-17.2270173142075,-20.4389083686787,
-1.21206542043532));
#113183=CARTESIAN_POINT('Ctrl Pts',(-17.2370912734195,-20.4490496288815,
-1.21290718553109));
#113184=CARTESIAN_POINT('Ctrl Pts',(-17.3306416150942,-20.5413364240546,
-1.22060558191524));
#113185=CARTESIAN_POINT('Ctrl Pts',(-17.4207019398818,-20.6165295191162,
-1.22714391961088));
#113186=CARTESIAN_POINT('Ctrl Pts',(-17.6505928968053,-20.7781358035061,
-1.24252640308231));
#113187=CARTESIAN_POINT('Ctrl Pts',(-17.7951262372743,-20.8564806741519,
-1.25118391531412));
#113188=CARTESIAN_POINT('Ctrl Pts',(-17.976214436349,-20.9289737140594,
-1.26239998728148));
#113189=CARTESIAN_POINT('Ctrl Pts',(-18.0054548048088,-20.9399350321059,
-1.26422304119466));
#113190=CARTESIAN_POINT('Ctrl Pts',(-18.0416743067521,-20.952606223557,
-1.26650820836094));
#113191=CARTESIAN_POINT('Ctrl Pts',(-18.0484353456044,-20.9549331562959,
-1.26693592008741));
#113192=CARTESIAN_POINT('Ctrl Pts',(-18.0590822442749,-20.958537254408,
-1.26761144098931));
#113193=CARTESIAN_POINT('Ctrl Pts',(-18.0629603109275,-20.9598375097001,
-1.26785790775429));
#113194=CARTESIAN_POINT('Ctrl Pts',(-18.0702350407491,-20.9622531831667,
-1.26832106102532));
#113195=CARTESIAN_POINT('Ctrl Pts',(-18.0736307693733,-20.9633712387644,
-1.26853758948812));
#113196=CARTESIAN_POINT('Ctrl Pts',(-18.0814137343029,-20.965911973664,
-1.26903462827884));
#113197=CARTESIAN_POINT('Ctrl Pts',(-18.0858027851299,-20.9673289164672,
-1.26931547087678));
#113198=CARTESIAN_POINT('Ctrl Pts',(-18.0993957276365,-20.9716682078382,
-1.27018685796167));
#113199=CARTESIAN_POINT('Ctrl Pts',(-18.1086148598757,-20.9745418835357,
-1.2707801430648));
#113200=CARTESIAN_POINT('Ctrl Pts',(-18.2198831369804,-21.0083915995844,
-1.27796539504898));
#113201=CARTESIAN_POINT('Ctrl Pts',(-18.3241012098868,-21.031673084689,
-1.28493824032067));
#113202=CARTESIAN_POINT('Ctrl Pts',(-18.5378628955064,-21.0627307298022,
-1.29918768837418));
#113203=CARTESIAN_POINT('Ctrl Pts',(-18.6471743992129,-21.0700458188569,
-1.30644376519846));
#113204=CARTESIAN_POINT('Ctrl Pts',(-18.8191787198025,-21.0682122872552,
-1.31756380342891));
#113205=CARTESIAN_POINT('Ctrl Pts',(-18.8817356568463,-21.0647671917594,
-1.32154879729399));
#113206=CARTESIAN_POINT('Ctrl Pts',(-18.9688256643133,-21.0560831036814,
-1.32700389058882));
#113207=CARTESIAN_POINT('Ctrl Pts',(-18.9935538649445,-21.0531760214477,
-1.32854246982863));
#113208=CARTESIAN_POINT('Ctrl Pts',(-19.0367595567446,-21.0473222791134,
-1.33121315144019));
#113209=CARTESIAN_POINT('Ctrl Pts',(-19.0552595912429,-21.0445656770634,
-1.33235103508021));
#113210=CARTESIAN_POINT('Ctrl Pts',(-19.0821455865989,-21.0401945545604,
-1.33399688729359));
#113211=CARTESIAN_POINT('Ctrl Pts',(-19.0905617638768,-21.0387739597373,
-1.33451097206093));
#113212=CARTESIAN_POINT('Ctrl Pts',(-19.1053189390384,-21.0361911619444,
-1.33541048274113));
#113213=CARTESIAN_POINT('Ctrl Pts',(-19.1116636054813,-21.0350508290813,
-1.33579659809905));
#113214=CARTESIAN_POINT('Ctrl Pts',(-19.1239853952597,-21.0327780751215,
-1.33654529482105));
#113215=CARTESIAN_POINT('Ctrl Pts',(-19.1299630345564,-21.0316488364326,
-1.33690797330629));
#113216=CARTESIAN_POINT('Ctrl Pts',(-19.1442605975167,-21.0288839968661,
-1.33777420221956));
#113217=CARTESIAN_POINT('Ctrl Pts',(-19.1525757667027,-21.0272241385019,
-1.33827697549871));
#113218=CARTESIAN_POINT('Ctrl Pts',(-19.1826603130865,-21.0210305396005,
-1.34009255695913));
#113219=CARTESIAN_POINT('Ctrl Pts',(-19.2043683739302,-21.0162037443949,
-1.34139601175898));
#113220=CARTESIAN_POINT('Ctrl Pts',(-19.4052516317385,-20.9682036259441,
-1.35340673011112));
#113221=CARTESIAN_POINT('Ctrl Pts',(-19.5781414642451,-20.9021505404539,
-1.36327138102053));
#113222=CARTESIAN_POINT('Ctrl Pts',(-19.8115642434693,-20.7760352665265,
-1.37773074058416));
#113223=CARTESIAN_POINT('Ctrl Pts',(-19.8805508821496,-20.7334792654729,
-1.38218241140538));
#113224=CARTESIAN_POINT('Ctrl Pts',(-19.9766423679338,-20.6663056014761,
-1.38888719238138));
#113225=CARTESIAN_POINT('Ctrl Pts',(-20.0058197935248,-20.6447722256088,
-1.39099590238403));
#113226=CARTESIAN_POINT('Ctrl Pts',(-20.0403302873196,-20.6179069994832,
-1.39359851447107));
#113227=CARTESIAN_POINT('Ctrl Pts',(-20.0462081858515,-20.6132810188803,
-1.3940457013601));
#113228=CARTESIAN_POINT('Ctrl Pts',(-20.0553184713441,-20.6060325939564,
-1.3947451250928));
#113229=CARTESIAN_POINT('Ctrl Pts',(-20.0585679151092,-20.6034315493424,
-1.39499585701764));
#113230=CARTESIAN_POINT('Ctrl Pts',(-20.0645866491574,-20.5985846112994,
-1.39546266537871));
#113231=CARTESIAN_POINT('Ctrl Pts',(-20.0673579438965,-20.596341298493,
-1.39567855713391));
#113232=CARTESIAN_POINT('Ctrl Pts',(-20.0736190033552,-20.5912468493669,
-1.39616846621913));
#113233=CARTESIAN_POINT('Ctrl Pts',(-20.0771053215513,-20.5883915795621,
-1.39644277966131));
#113234=CARTESIAN_POINT('Ctrl Pts',(-20.0873944805958,-20.5799097998947,
-1.39725679905749));
#113235=CARTESIAN_POINT('Ctrl Pts',(-20.0941711743339,-20.574251924635,
-1.39779870495772));
#113236=CARTESIAN_POINT('Ctrl Pts',(-20.1437897748362,-20.5322957920663,
-1.40180794424738));
#113237=CARTESIAN_POINT('Ctrl Pts',(-20.1852040735271,-20.4943513057331,
-1.40538276734724));
#113238=CARTESIAN_POINT('Ctrl Pts',(-20.2694068852616,-20.4108069874383,
-1.41306245080667));
#113239=CARTESIAN_POINT('Ctrl Pts',(-20.3117851875953,-20.3648642600338,
-1.41717770387232));
#113240=CARTESIAN_POINT('Ctrl Pts',(-20.4227519314223,-20.2333357899058,
-1.4285446052632));
#113241=CARTESIAN_POINT('Ctrl Pts',(-20.4868273204476,-20.1441846905486,
-1.43579421479988));
#113242=CARTESIAN_POINT('Ctrl Pts',(-20.5724489213871,-20.0031240137737,
-1.44640321064745));
#113243=CARTESIAN_POINT('Ctrl Pts',(-20.5993182410521,-19.9546688492893,
-1.4499108553119));
#113244=CARTESIAN_POINT('Ctrl Pts',(-20.6397608422569,-19.8744695415408,
-1.45549443177426));
#113245=CARTESIAN_POINT('Ctrl Pts',(-20.6545119772732,-19.8433520106125,
-1.45760925332541));
#113246=CARTESIAN_POINT('Ctrl Pts',(-20.6728942833821,-19.8019971136178,
-1.46035443784606));
#113247=CARTESIAN_POINT('Ctrl Pts',(-20.6772145078748,-19.7920735196925,
-1.46100832781741));
#113248=CARTESIAN_POINT('Ctrl Pts',(-20.6841645660995,-19.7757686510845,
-1.46207489748118));
#113249=CARTESIAN_POINT('Ctrl Pts',(-20.6868395938445,-19.7694069658667,
-1.46248911262404));
#113250=CARTESIAN_POINT('Ctrl Pts',(-20.6919565604378,-19.7570694248642,
-1.4632887369795));
#113251=CARTESIAN_POINT('Ctrl Pts',(-20.6944023645908,-19.7510952644985,
-1.46367427388952));
#113252=CARTESIAN_POINT('Ctrl Pts',(-20.6999852470215,-19.7372785196961,
-1.46456214063773));
#113253=CARTESIAN_POINT('Ctrl Pts',(-20.7031028045932,-19.7294281272891,
-1.46506380701488));
#113254=CARTESIAN_POINT('Ctrl Pts',(-20.7113578717422,-19.7082726095752,
-1.46640833455584));
#113255=CARTESIAN_POINT('Ctrl Pts',(-20.7164081053056,-19.6949337331012,
-1.46724826858965));
#113256=CARTESIAN_POINT('Ctrl Pts',(-20.7217433569485,-19.6804001874366,
-1.46815528110785));
#113257=CARTESIAN_POINT('Ctrl Pts',(-20.72216246852,-19.6792554467231,-1.46822666771441));
#113258=CARTESIAN_POINT('Ctrl Pts',(-20.7225805819607,-19.6781103697434,
-1.46829802089257));
#113259=CARTESIAN_POINT('',(-20.8509993841888,-18.9503852727442,-0.489056278967187));
#113260=CARTESIAN_POINT('Ctrl Pts',(-20.7225806439552,-19.6781101999604,
-1.24458624895942));
#113261=CARTESIAN_POINT('Ctrl Pts',(-20.6661823420556,-19.8325668809376,
-1.23372063291377));
#113262=CARTESIAN_POINT('Ctrl Pts',(-20.5919347480107,-19.9800493809754,
-1.22298087846725));
#113263=CARTESIAN_POINT('Ctrl Pts',(-20.4894885518365,-20.1353879489779,
-1.21154553712518));
#113264=CARTESIAN_POINT('Ctrl Pts',(-20.4774343962679,-20.1530760392754,
-1.21024031609317));
#113265=CARTESIAN_POINT('Ctrl Pts',(-20.4603098215144,-20.1774032193866,
-1.20844026140752));
#113266=CARTESIAN_POINT('Ctrl Pts',(-20.4554655649895,-20.1841992377921,
-1.20793685243739));
#113267=CARTESIAN_POINT('Ctrl Pts',(-20.4470413923941,-20.1958708819646,
-1.20707127883651));
#113268=CARTESIAN_POINT('Ctrl Pts',(-20.4434805626339,-20.2007601011453,
-1.20670838439107));
#113269=CARTESIAN_POINT('Ctrl Pts',(-20.4360698922163,-20.2108442672094,
-1.20595923331404));
#113270=CARTESIAN_POINT('Ctrl Pts',(-20.4322171031056,-20.2160369770011,
-1.20557309651764));
#113271=CARTESIAN_POINT('Ctrl Pts',(-20.4231495686122,-20.2281417249901,
-1.20467205338959));
#113272=CARTESIAN_POINT('Ctrl Pts',(-20.4179160645021,-20.2350396168909,
-1.20415788796871));
#113273=CARTESIAN_POINT('Ctrl Pts',(-20.400833264236,-20.2572706114968,
-1.20249833136461));
#113274=CARTESIAN_POINT('Ctrl Pts',(-20.3888155115931,-20.272473460348,
-1.20135960267726));
#113275=CARTESIAN_POINT('Ctrl Pts',(-20.3265596928535,-20.349044093152,
-1.19560095950256));
#113276=CARTESIAN_POINT('Ctrl Pts',(-20.2731077263145,-20.4077224817765,
-1.19111364917385));
#113277=CARTESIAN_POINT('Ctrl Pts',(-20.1000687157715,-20.5774657606864,
-1.17766510614145));
#113278=CARTESIAN_POINT('Ctrl Pts',(-19.9708583561275,-20.6778210692345,
-1.16906408067147));
#113279=CARTESIAN_POINT('Ctrl Pts',(-19.7791772409136,-20.794016751747,
-1.15653482464692));
#113280=CARTESIAN_POINT('Ctrl Pts',(-19.7255935645414,-20.823406400002,
-1.15304837588591));
#113281=CARTESIAN_POINT('Ctrl Pts',(-19.6626470098079,-20.8544686056655,
-1.14888521636218));
#113282=CARTESIAN_POINT('Ctrl Pts',(-19.6544481996829,-20.8584488373225,
-1.14834167811425));
#113283=CARTESIAN_POINT('Ctrl Pts',(-19.6421585445052,-20.8643172738121,
-1.14752464758654));
#113284=CARTESIAN_POINT('Ctrl Pts',(-19.6380868334741,-20.8662456201739,
-1.1472535820609));
#113285=CARTESIAN_POINT('Ctrl Pts',(-19.6307806854683,-20.8696772730928,
-1.14676646819602));
#113286=CARTESIAN_POINT('Ctrl Pts',(-19.6275485790196,-20.8711854152749,
-1.14655072293413));
#113287=CARTESIAN_POINT('Ctrl Pts',(-19.6205324434656,-20.8744376679082,
-1.14608182704168));
#113288=CARTESIAN_POINT('Ctrl Pts',(-19.6167471219066,-20.8761787542702,
-1.14582850047923));
#113289=CARTESIAN_POINT('Ctrl Pts',(-19.6061408201004,-20.8810193163291,
-1.14511776581438));
#113290=CARTESIAN_POINT('Ctrl Pts',(-19.599308568291,-20.8840937375409,
-1.14465886514953));
#113291=CARTESIAN_POINT('Ctrl Pts',(-19.5591795902109,-20.9018956946936,
-1.14195791219407));
#113292=CARTESIAN_POINT('Ctrl Pts',(-19.5255258327402,-20.9157976128018,
-1.13967026937973));
#113293=CARTESIAN_POINT('Ctrl Pts',(-19.4153871114746,-20.9580035462417,
-1.13214930869362));
#113294=CARTESIAN_POINT('Ctrl Pts',(-19.3376238590628,-20.9827572731476,
-1.12678916334));
#113295=CARTESIAN_POINT('Ctrl Pts',(-19.0810907958565,-21.0483779830773,
-1.10930511712457));
#113296=CARTESIAN_POINT('Ctrl Pts',(-18.8983629554454,-21.0705570774497,
-1.09724052908153));
#113297=CARTESIAN_POINT('Ctrl Pts',(-18.692724930536,-21.0687152236704,
-1.08459113297433));
#113298=CARTESIAN_POINT('Ctrl Pts',(-18.6704145147232,-21.0681625446401,
-1.08322946316258));
#113299=CARTESIAN_POINT('Ctrl Pts',(-18.6396301016288,-21.0669126357501,
-1.08136476141177));
#113300=CARTESIAN_POINT('Ctrl Pts',(-18.63114594162,-21.0665170088076,-1.0808523346566));
#113301=CARTESIAN_POINT('Ctrl Pts',(-18.6165841428066,-21.0657501241288,
-1.07997531686111));
#113302=CARTESIAN_POINT('Ctrl Pts',(-18.6105053522402,-21.0654036869358,
-1.07960995208983));
#113303=CARTESIAN_POINT('Ctrl Pts',(-18.597992781016,-21.0646364110564,
-1.0788593880015));
#113304=CARTESIAN_POINT('Ctrl Pts',(-18.5915592531782,-21.0642123955703,
-1.07847429238584));
#113305=CARTESIAN_POINT('Ctrl Pts',(-18.5766197305293,-21.0631592067378,
-1.07758190379666));
#113306=CARTESIAN_POINT('Ctrl Pts',(-18.5681153629804,-21.0625080042162,
-1.07707530749062));
#113307=CARTESIAN_POINT('Ctrl Pts',(-18.5410186473279,-21.0602683384612,
-1.07546548286585));
#113308=CARTESIAN_POINT('Ctrl Pts',(-18.5224429415029,-21.0584854220796,
-1.07436835997421));
#113309=CARTESIAN_POINT('Ctrl Pts',(-18.3441735034812,-21.0389929439099,
-1.06389553117215));
#113310=CARTESIAN_POINT('Ctrl Pts',(-18.1869583414912,-21.003403869076,
-1.05514828860677));
#113311=CARTESIAN_POINT('Ctrl Pts',(-17.9084935426492,-20.9060379886269,
-1.03912854452344));
#113312=CARTESIAN_POINT('Ctrl Pts',(-17.7862426480781,-20.8497543200834,
-1.03186589658319));
#113313=CARTESIAN_POINT('Ctrl Pts',(-17.656607916401,-20.7744053181977,
-1.02307442102728));
#113314=CARTESIAN_POINT('Ctrl Pts',(-17.6431403977316,-20.7663759646988,
-1.02214690228698));
#113315=CARTESIAN_POINT('Ctrl Pts',(-17.6248246333446,-20.7551784489659,
-1.02086417720725));
#113316=CARTESIAN_POINT('Ctrl Pts',(-17.6198979818765,-20.7521386625013,
-1.02051700874684));
#113317=CARTESIAN_POINT('Ctrl Pts',(-17.6120883109699,-20.747275688475,
-1.01996317633543));
#113318=CARTESIAN_POINT('Ctrl Pts',(-17.6091970814683,-20.7454656477596,
-1.0197573735147));
#113319=CARTESIAN_POINT('Ctrl Pts',(-17.6032371940535,-20.7417144078601,
-1.01933152364533));
#113320=CARTESIAN_POINT('Ctrl Pts',(-17.6001691636093,-20.7397723061611,
-1.01911141362441));
#113321=CARTESIAN_POINT('Ctrl Pts',(-17.5928705319652,-20.7351258365693,
-1.01858568352044));
#113322=CARTESIAN_POINT('Ctrl Pts',(-17.5886445411204,-20.7324143010771,
-1.01827959036972));
#113323=CARTESIAN_POINT('Ctrl Pts',(-17.5744204527725,-20.7232160550712,
-1.01724372036873));
#113324=CARTESIAN_POINT('Ctrl Pts',(-17.5644677098496,-20.7166600940052,
-1.01650953184276));
#113325=CARTESIAN_POINT('Ctrl Pts',(-17.540689410603,-20.7007076003327,
-1.01473383048842));
#113326=CARTESIAN_POINT('Ctrl Pts',(-17.5269189469453,-20.6912307865022,
-1.01368767159871));
#113327=CARTESIAN_POINT('Ctrl Pts',(-17.4756948782964,-20.6550770995942,
-1.00973304630827));
#113328=CARTESIAN_POINT('Ctrl Pts',(-17.4390033230139,-20.6273466648571,
-1.00677227010053));
#113329=CARTESIAN_POINT('Ctrl Pts',(-17.3454270830285,-20.5517128670429,
-0.998935716966504));
#113330=CARTESIAN_POINT('Ctrl Pts',(-17.2901113344371,-20.5019680554739,
-0.99401212471712));
#113331=CARTESIAN_POINT('Ctrl Pts',(-17.1277266796459,-20.3396860537082,
-0.978845205443246));
#113332=CARTESIAN_POINT('Ctrl Pts',(-17.0303087573192,-20.2181908556132,
-0.968729374174171));
#113333=CARTESIAN_POINT('Ctrl Pts',(-16.9342096071964,-20.0669065472817,
-0.957687408827122));
#113334=CARTESIAN_POINT('Ctrl Pts',(-16.9217171354024,-20.0464829645925,
-0.956225145876773));
#113335=CARTESIAN_POINT('Ctrl Pts',(-16.9046537474558,-20.0174930080576,
-0.954188309082515));
#113336=CARTESIAN_POINT('Ctrl Pts',(-16.8997915754078,-20.0091009989466,
-0.953603162011575));
#113337=CARTESIAN_POINT('Ctrl Pts',(-16.8920196450153,-19.9954717341781,
-0.952659964534795));
#113338=CARTESIAN_POINT('Ctrl Pts',(-16.8890741879184,-19.9902550925667,
-0.952300626726747));
#113339=CARTESIAN_POINT('Ctrl Pts',(-16.8829819345063,-19.979357433358,
-0.951553413427386));
#113340=CARTESIAN_POINT('Ctrl Pts',(-16.8798390522542,-19.9736742905474,
-0.951165681462966));
#113341=CARTESIAN_POINT('Ctrl Pts',(-16.8724721964518,-19.9602071546126,
-0.950251414745203));
#113342=CARTESIAN_POINT('Ctrl Pts',(-16.8682707964321,-19.9524109018718,
-0.949725690312238));
#113343=CARTESIAN_POINT('Ctrl Pts',(-16.8544956832457,-19.9264607394634,
-0.947987351125742));
#113344=CARTESIAN_POINT('Ctrl Pts',(-16.8451368537631,-19.9081936351888,
-0.946782341173989));
#113345=CARTESIAN_POINT('Ctrl Pts',(-16.7969202976145,-19.810610399808,
-0.940438829375276));
#113346=CARTESIAN_POINT('Ctrl Pts',(-16.7627867205766,-19.7290523564093,
-0.935466793701247));
#113347=CARTESIAN_POINT('Ctrl Pts',(-16.6909632089416,-19.5219305385132,
-0.923366387270467));
#113348=CARTESIAN_POINT('Ctrl Pts',(-16.6596431278252,-19.3945632604551,
-0.916389198105422));
#113349=CARTESIAN_POINT('Ctrl Pts',(-16.6347059999534,-19.2278193987965,
-0.907089195435979));
#113350=CARTESIAN_POINT('Ctrl Pts',(-16.6301253420164,-19.1903754013159,
-0.904988791609812));
#113351=CARTESIAN_POINT('Ctrl Pts',(-16.6221957050251,-19.1071643358583,
-0.900257140621528));
#113352=CARTESIAN_POINT('Ctrl Pts',(-16.6193297205363,-19.0613722280543,
-0.89761064508369));
#113353=CARTESIAN_POINT('Ctrl Pts',(-16.6177244937089,-19.007903114256,
-0.894433887255013));
#113354=CARTESIAN_POINT('Ctrl Pts',(-16.6175368194285,-19.0002781319863,
-0.893978812199759));
#113355=CARTESIAN_POINT('Ctrl Pts',(-16.6173018872752,-18.9880461539762,
-0.893245253663853));
#113356=CARTESIAN_POINT('Ctrl Pts',(-16.617228455125,-18.9834396488026,
-0.892968196487284));
#113357=CARTESIAN_POINT('Ctrl Pts',(-16.61712466768,-18.9752519527732,-0.892474265397267));
#113358=CARTESIAN_POINT('Ctrl Pts',(-16.6170883622654,-18.9716708852444,
-0.892257727461891));
#113359=CARTESIAN_POINT('Ctrl Pts',(-16.6170304186042,-18.9640471715229,
-0.891795644351456));
#113360=CARTESIAN_POINT('Ctrl Pts',(-16.6170112734264,-18.9600046126915,
-0.891549968274009));
#113361=CARTESIAN_POINT('Ctrl Pts',(-16.6169907237584,-18.9490245829682,
-0.890880961851548));
#113362=CARTESIAN_POINT('Ctrl Pts',(-16.6170118418035,-18.9420871912966,
-0.890456402181877));
#113363=CARTESIAN_POINT('Ctrl Pts',(-16.617293210134,-18.9067374667283,
-0.888283951342084));
#113364=CARTESIAN_POINT('Ctrl Pts',(-16.618091344353,-18.8783338039578,
-0.886508468251654));
#113365=CARTESIAN_POINT('Ctrl Pts',(-16.6221157620144,-18.7949400759451,
-0.881224236880963));
#113366=CARTESIAN_POINT('Ctrl Pts',(-16.6269167083662,-18.7400518345294,
-0.877655291514327));
#113367=CARTESIAN_POINT('Ctrl Pts',(-16.65147202781,-18.5466041013743,-0.864884454562608));
#113368=CARTESIAN_POINT('Ctrl Pts',(-16.6828138324906,-18.4098663781984,
-0.855532658905493));
#113369=CARTESIAN_POINT('Ctrl Pts',(-16.7562374772549,-18.1915276702295,
-0.840658450403927));
#113370=CARTESIAN_POINT('Ctrl Pts',(-16.7905171998272,-18.1077600411421,
-0.834959681366878));
#113371=CARTESIAN_POINT('Ctrl Pts',(-16.836057805489,-18.0140804844457,
-0.828604027268443));
#113372=CARTESIAN_POINT('Ctrl Pts',(-16.8421820600796,-18.0017881880842,
-0.827770278962194));
#113373=CARTESIAN_POINT('Ctrl Pts',(-16.8521963996708,-17.9821685689714,
-0.826439688166557));
#113374=CARTESIAN_POINT('Ctrl Pts',(-16.8560106148612,-17.9748031584242,
-0.825940203278252));
#113375=CARTESIAN_POINT('Ctrl Pts',(-16.8628603671227,-17.9617642336197,
-0.82505596551924));
#113376=CARTESIAN_POINT('Ctrl Pts',(-16.8658786504242,-17.9560818189135,
-0.824670609817944));
#113377=CARTESIAN_POINT('Ctrl Pts',(-16.872221887875,-17.9442699345436,
-0.823869539515819));
#113378=CARTESIAN_POINT('Ctrl Pts',(-16.8755513185703,-17.9381429470129,
-0.823453989786786));
#113379=CARTESIAN_POINT('Ctrl Pts',(-16.8842775647081,-17.9222718896201,
-0.822377440304785));
#113380=CARTESIAN_POINT('Ctrl Pts',(-16.889721162235,-17.912553683605,-0.821718118394523));
#113381=CARTESIAN_POINT('Ctrl Pts',(-16.9137064766448,-17.8705154483635,
-0.818865000877634));
#113382=CARTESIAN_POINT('Ctrl Pts',(-16.9330236198484,-17.838643958865,
-0.816699273047077));
#113383=CARTESIAN_POINT('Ctrl Pts',(-16.9865971554088,-17.7552989840656,
-0.811013087269197));
#113384=CARTESIAN_POINT('Ctrl Pts',(-17.0222843534298,-17.7047869361817,
-0.807543773668025));
#113385=CARTESIAN_POINT('Ctrl Pts',(-17.1467956067731,-17.5439843609605,
-0.796291847144478));
#113386=CARTESIAN_POINT('Ctrl Pts',(-17.2444599190256,-17.4410420768077,
-0.788767944894847));
#113387=CARTESIAN_POINT('Ctrl Pts',(-17.4090573587147,-17.2991362216952,
-0.776737456263016));
#113388=CARTESIAN_POINT('Ctrl Pts',(-17.4690615245864,-17.2527767252116,
-0.772455925017883));
#113389=CARTESIAN_POINT('Ctrl Pts',(-17.5392389823377,-17.2043371262278,
-0.767402312202162));
#113390=CARTESIAN_POINT('Ctrl Pts',(-17.5471004002235,-17.1989886645767,
-0.766835563151585));
#113391=CARTESIAN_POINT('Ctrl Pts',(-17.558807110148,-17.1911389290952,
-0.765990239723609));
#113392=CARTESIAN_POINT('Ctrl Pts',(-17.5626250568805,-17.1885968183335,
-0.765714339488015));
#113393=CARTESIAN_POINT('Ctrl Pts',(-17.5694381726738,-17.1840923179106,
-0.765221562130502));
#113394=CARTESIAN_POINT('Ctrl Pts',(-17.5724300862887,-17.1821251012263,
-0.765005012789305));
#113395=CARTESIAN_POINT('Ctrl Pts',(-17.5788826676815,-17.1779058661085,
-0.764537650669552));
#113396=CARTESIAN_POINT('Ctrl Pts',(-17.5823448928539,-17.1756564068724,
-0.764286678873976));
#113397=CARTESIAN_POINT('Ctrl Pts',(-17.591928511475,-17.1694695823861,
-0.763591468520061));
#113398=CARTESIAN_POINT('Ctrl Pts',(-17.5980635966468,-17.1655536787713,
-0.763145850445403));
#113399=CARTESIAN_POINT('Ctrl Pts',(-17.6319409930451,-17.1441754741181,
-0.760682597581648));
#113400=CARTESIAN_POINT('Ctrl Pts',(-17.6600642134983,-17.1273287352435,
-0.758628267009439));
#113401=CARTESIAN_POINT('Ctrl Pts',(-17.8308812954873,-17.030320612999,
-0.746145962448446));
#113402=CARTESIAN_POINT('Ctrl Pts',(-17.9820855660748,-16.9662759372,-0.735128700240828));
#113403=CARTESIAN_POINT('Ctrl Pts',(-18.2489533329964,-16.8881426260486,
-0.716988446011342));
#113404=CARTESIAN_POINT('Ctrl Pts',(-18.3611876309905,-16.8649456676826,
-0.70970887755997));
#113405=CARTESIAN_POINT('Ctrl Pts',(-18.4889228391326,-16.8491852852282,
-0.701850727411099));
#113406=CARTESIAN_POINT('Ctrl Pts',(-18.5030997550142,-16.8475814028804,
-0.700984159919865));
#113407=CARTESIAN_POINT('Ctrl Pts',(-18.5257061175593,-16.8452550689986,
-0.699611003539678));
#113408=CARTESIAN_POINT('Ctrl Pts',(-18.5341253637235,-16.8444396381666,
-0.699101510074506));
#113409=CARTESIAN_POINT('Ctrl Pts',(-18.5489929004768,-16.8430895622128,
-0.698205098472977));
#113410=CARTESIAN_POINT('Ctrl Pts',(-18.5554391366547,-16.8425339820225,
-0.697817528159776));
#113411=CARTESIAN_POINT('Ctrl Pts',(-18.5687874047758,-16.8414451633194,
-0.697017208627248));
#113412=CARTESIAN_POINT('Ctrl Pts',(-18.575689715888,-16.8409162082126,
-0.696604598181632));
#113413=CARTESIAN_POINT('Ctrl Pts',(-18.5934351201831,-16.8396438187476,
-0.695546898181894));
#113414=CARTESIAN_POINT('Ctrl Pts',(-18.6042816533274,-16.838950005536,
-0.694903368007642));
#113415=CARTESIAN_POINT('Ctrl Pts',(-18.6497600393507,-16.8363924185133,
-0.692217084498543));
#113416=CARTESIAN_POINT('Ctrl Pts',(-18.6844308352284,-16.8352962157233,
-0.6901983668217));
#113417=CARTESIAN_POINT('Ctrl Pts',(-18.7749975637378,-16.8346593857365,
-0.68498914065463));
#113418=CARTESIAN_POINT('Ctrl Pts',(-18.8308768709355,-16.8364793507137,
-0.681839231688125));
#113419=CARTESIAN_POINT('Ctrl Pts',(-19.0845520339329,-16.8548153909185,
-0.667705195157753));
#113420=CARTESIAN_POINT('Ctrl Pts',(-19.2794561841048,-16.8968775714436,
-0.657394736191735));
#113421=CARTESIAN_POINT('Ctrl Pts',(-19.4955716737775,-16.9764707687702,
-0.644170640165188));
#113422=CARTESIAN_POINT('Ctrl Pts',(-19.5252592060564,-16.9881731796752,
-0.642310073980115));
#113423=CARTESIAN_POINT('Ctrl Pts',(-19.5609544653769,-17.003184512385,
-0.640006136709419));
#113424=CARTESIAN_POINT('Ctrl Pts',(-19.5672269241438,-17.0058580774774,
-0.639598742980857));
#113425=CARTESIAN_POINT('Ctrl Pts',(-19.5775381800859,-17.0103121208054,
-0.638924664551405));
#113426=CARTESIAN_POINT('Ctrl Pts',(-19.5815845733286,-17.0120750345136,
-0.638659026358655));
#113427=CARTESIAN_POINT('Ctrl Pts',(-19.5888755231298,-17.0152786873457,
-0.638178326549731));
#113428=CARTESIAN_POINT('Ctrl Pts',(-19.5921219984902,-17.0167149464509,
-0.637963541108073));
#113429=CARTESIAN_POINT('Ctrl Pts',(-19.5984335811427,-17.0195262307363,
-0.637544504456728));
#113430=CARTESIAN_POINT('Ctrl Pts',(-19.6014989849624,-17.0209003661585,
-0.637340315752203));
#113431=CARTESIAN_POINT('Ctrl Pts',(-19.6105425853905,-17.0249802398308,
-0.636735959008615));
#113432=CARTESIAN_POINT('Ctrl Pts',(-19.6165114206642,-17.0277064543452,
-0.636334549578813));
#113433=CARTESIAN_POINT('Ctrl Pts',(-19.6448671951683,-17.0408173890174,
-0.63441587118083));
#113434=CARTESIAN_POINT('Ctrl Pts',(-19.6670830653751,-17.0515648159411,
-0.632877741802317));
#113435=CARTESIAN_POINT('Ctrl Pts',(-19.72928114307,-17.0830079997259,-0.628482572726861));
#113436=CARTESIAN_POINT('Ctrl Pts',(-19.7687968860003,-17.1045935662158,
-0.625584773412187));
#113437=CARTESIAN_POINT('Ctrl Pts',(-19.8895209047652,-17.1756281997965,
-0.616463024098987));
#113438=CARTESIAN_POINT('Ctrl Pts',(-19.9681082336591,-17.229298158072,
-0.610137882435616));
#113439=CARTESIAN_POINT('Ctrl Pts',(-20.1606326761606,-17.380734559692,
-0.593981586666354));
#113440=CARTESIAN_POINT('Ctrl Pts',(-20.2682887424195,-17.4856678468788,
-0.584307120692968));
#113441=CARTESIAN_POINT('Ctrl Pts',(-20.3729857366812,-17.6119946244293,
-0.574291013654049));
#113442=CARTESIAN_POINT('Ctrl Pts',(-20.3818931718843,-17.6229639730383,
-0.573432898024258));
#113443=CARTESIAN_POINT('Ctrl Pts',(-20.3959063681158,-17.6405784736316,
-0.572073073340814));
#113444=CARTESIAN_POINT('Ctrl Pts',(-20.4010835361085,-17.6471660323951,
-0.571568488046995));
#113445=CARTESIAN_POINT('Ctrl Pts',(-20.4101514297626,-17.6588463148458,
-0.570680724869194));
#113446=CARTESIAN_POINT('Ctrl Pts',(-20.4140583677801,-17.6639262632966,
-0.5702969011356));
#113447=CARTESIAN_POINT('Ctrl Pts',(-20.422097144815,-17.6744773843779,
-0.569504357168962));
#113448=CARTESIAN_POINT('Ctrl Pts',(-20.4262255985482,-17.6799510508288,
-0.569095773986404));
#113449=CARTESIAN_POINT('Ctrl Pts',(-20.43676584734,-17.6940678552726,-0.568048536260453));
#113450=CARTESIAN_POINT('Ctrl Pts',(-20.4431385100698,-17.7027400704754,
-0.56741142291253));
#113451=CARTESIAN_POINT('Ctrl Pts',(-20.4695464598245,-17.7392575584162,
-0.5647540918308));
#113452=CARTESIAN_POINT('Ctrl Pts',(-20.4889702401525,-17.7675400396342,
-0.562757567744567));
#113453=CARTESIAN_POINT('Ctrl Pts',(-20.5378433424859,-17.8425464601744,
-0.557608819686927));
#113454=CARTESIAN_POINT('Ctrl Pts',(-20.5661675725709,-17.8899733527495,
-0.554496467580978));
#113455=CARTESIAN_POINT('Ctrl Pts',(-20.6274486114797,-18.0023487122949,
-0.547383506223037));
#113456=CARTESIAN_POINT('Ctrl Pts',(-20.6589739959099,-18.067997180263,
-0.543420718962677));
#113457=CARTESIAN_POINT('Ctrl Pts',(-20.7006448004888,-18.1676293066662,
-0.537557147698845));
#113458=CARTESIAN_POINT('Ctrl Pts',(-20.7134202568039,-18.2004518733808,
-0.535648298079368));
#113459=CARTESIAN_POINT('Ctrl Pts',(-20.7392639646576,-18.272087190512,
-0.531505618451721));
#113460=CARTESIAN_POINT('Ctrl Pts',(-20.7520366525749,-18.3109907112703,
-0.529270323297309));
#113461=CARTESIAN_POINT('Ctrl Pts',(-20.7690499488225,-18.368374677458,
-0.52596440823563));
#113462=CARTESIAN_POINT('Ctrl Pts',(-20.7741834180245,-18.3865812122226,
-0.5249142252036));
#113463=CARTESIAN_POINT('Ctrl Pts',(-20.7947008200014,-18.4632692387766,
-0.52047639537556));
#113464=CARTESIAN_POINT('Ctrl Pts',(-20.8078179693683,-18.5223219603253,
-0.517024578340226));
#113465=CARTESIAN_POINT('Ctrl Pts',(-20.8199725808871,-18.5907667919248,
-0.512901088674033));
#113466=CARTESIAN_POINT('Ctrl Pts',(-20.8214989814923,-18.5996946857741,
-0.512360842528588));
#113467=CARTESIAN_POINT('Ctrl Pts',(-20.8236943601964,-18.6130508365701,
-0.511548707398552));
#113468=CARTESIAN_POINT('Ctrl Pts',(-20.8244066763095,-18.6174720023458,
-0.511279232147322));
#113469=CARTESIAN_POINT('Ctrl Pts',(-20.8256596119144,-18.6254089394062,
-0.510794262174948));
#113470=CARTESIAN_POINT('Ctrl Pts',(-20.8262054025299,-18.628923838553,
-0.510579064774684));
#113471=CARTESIAN_POINT('Ctrl Pts',(-20.827252039116,-18.6357780801854,
-0.510158586227158));
#113472=CARTESIAN_POINT('Ctrl Pts',(-20.8277537529317,-18.6391172367318,
-0.509953361381815));
#113473=CARTESIAN_POINT('Ctrl Pts',(-20.8288494962056,-18.6465306225135,
-0.509496908631086));
#113474=CARTESIAN_POINT('Ctrl Pts',(-20.8294396311101,-18.6506054014143,
-0.509245465875732));
#113475=CARTESIAN_POINT('Ctrl Pts',(-20.8308795002836,-18.6607561149897,
-0.508617762711576));
#113476=CARTESIAN_POINT('Ctrl Pts',(-20.831714710083,-18.6668340267681,
-0.508240727451475));
#113477=CARTESIAN_POINT('Ctrl Pts',(-20.8356021821279,-18.6960651320066,
-0.506421988151926));
#113478=CARTESIAN_POINT('Ctrl Pts',(-20.8382974724732,-18.7192631654612,
-0.504962284114994));
#113479=CARTESIAN_POINT('Ctrl Pts',(-20.8474812861682,-18.8116101392643,
-0.499099022991545));
#113480=CARTESIAN_POINT('Ctrl Pts',(-20.8509485264066,-18.8810102963083,
-0.494577353553003));
#113481=CARTESIAN_POINT('Ctrl Pts',(-20.8509994311265,-18.9504480302427,
-0.490010487033197));
#113482=CARTESIAN_POINT('Ctrl Pts',(-20.8509993841888,-18.9503852727442,
-0.489056278967187));
#113483=CARTESIAN_POINT('Ctrl Pts',(-20.8510540303841,-19.0220295465461,
-0.484732818461429));
#113484=CARTESIAN_POINT('Ctrl Pts',(-20.847467542629,-19.0938083387668,
-0.480409357955671));
#113485=CARTESIAN_POINT('Ctrl Pts',(-20.8402254594309,-19.1653150581775,
-0.476085897449914));
#113486=CARTESIAN_POINT('Ctrl Pts',(-20.832990974746,-19.2367467515573,
-0.471766973190315));
#113487=CARTESIAN_POINT('Ctrl Pts',(-20.8221085463431,-19.3079064470899,
-0.467448048930716));
#113488=CARTESIAN_POINT('Ctrl Pts',(-20.8076157348804,-19.3783880674413,
-0.463129124671117));
#113489=CARTESIAN_POINT('Ctrl Pts',(-20.7931333507106,-19.4488189776526,
-0.458813307792603));
#113490=CARTESIAN_POINT('Ctrl Pts',(-20.7750458355094,-19.518572295312,
-0.45449749091409));
#113491=CARTESIAN_POINT('Ctrl Pts',(-20.7534422763271,-19.5872494727135,
-0.450181674035576));
#113492=CARTESIAN_POINT('Ctrl Pts',(-20.7438446524082,-19.6177600804772,
-0.448264323891871));
#113493=CARTESIAN_POINT('Ctrl Pts',(-20.7335537498538,-19.6480584251371,
-0.446346973748166));
#113494=CARTESIAN_POINT('Ctrl Pts',(-20.7225805821191,-19.6781103693095,
-0.444429623604461));
#113495=CARTESIAN_POINT('Origin',(-23.734,10.1295,-7.));
#113496=CARTESIAN_POINT('',(-20.7043183293681,10.1259540182473,-11.2629985252183));
#113497=CARTESIAN_POINT('Ctrl Pts',(-22.1191569086782,11.6181146495903,
-10.9946458447559));
#113498=CARTESIAN_POINT('Ctrl Pts',(-22.1119092629397,11.7394000803016,
-10.9494485291601));
#113499=CARTESIAN_POINT('Ctrl Pts',(-22.1046616172012,11.8586337142555,
-10.8987204065082));
#113500=CARTESIAN_POINT('Ctrl Pts',(-22.0974139714626,11.975312836413,-10.8426740654046));
#113501=CARTESIAN_POINT('Ctrl Pts',(-22.0901668807576,12.0919830231423,
-10.7866320163975));
#113502=CARTESIAN_POINT('Ctrl Pts',(-22.0829197900526,12.2060987775499,
-10.7252727140119));
#113503=CARTESIAN_POINT('Ctrl Pts',(-22.0756726993475,12.3171800739265,
-10.6588556809671));
#113504=CARTESIAN_POINT('Ctrl Pts',(-22.0684238466281,12.4282883779462,
-10.5924224996814));
#113505=CARTESIAN_POINT('Ctrl Pts',(-22.0611749939087,12.5363604522096,
-10.5209293079317));
#113506=CARTESIAN_POINT('Ctrl Pts',(-22.0539261411893,12.6409430705206,
-10.4446803485279));
#113507=CARTESIAN_POINT('Ctrl Pts',(-22.0488803813273,12.7137406287231,
-10.3916051994283));
#113508=CARTESIAN_POINT('Ctrl Pts',(-22.0438346214652,12.7848480290955,
-10.3362267037117));
#113509=CARTESIAN_POINT('Ctrl Pts',(-22.0387888616031,12.8541212962082,
-10.2786594504841));
#113510=CARTESIAN_POINT('Ctrl Pts',(-22.031539428324,12.9536488087519,-10.1959504090815));
#113511=CARTESIAN_POINT('Ctrl Pts',(-22.0242899950448,13.0494257988114,
-10.1086908709218));
#113512=CARTESIAN_POINT('Ctrl Pts',(-22.0170405617656,13.1410453426988,
-10.0172443800378));
#113513=CARTESIAN_POINT('Ctrl Pts',(-22.0097925827507,13.2326465073522,
-9.92581623367251));
#113514=CARTESIAN_POINT('Ctrl Pts',(-22.0025446037359,13.3200916446911,
-9.8302030543376));
#113515=CARTESIAN_POINT('Ctrl Pts',(-21.995296624721,13.4030103443729,-9.73080556343431));
#113516=CARTESIAN_POINT('Ctrl Pts',(-21.9880484316003,13.485931493478,-9.63140513632318));
#113517=CARTESIAN_POINT('Ctrl Pts',(-21.9808002384797,13.5643257132271,
-9.5282204375736));
#113518=CARTESIAN_POINT('Ctrl Pts',(-21.9735520453591,13.6378623885564,
-9.4216858488588));
#113519=CARTESIAN_POINT('Ctrl Pts',(-21.9663041964995,13.7113955711794,
-9.31515632012281));
#113520=CARTESIAN_POINT('Ctrl Pts',(-21.9590563476398,13.7800714757147,
-9.20527750541117));
#113521=CARTESIAN_POINT('Ctrl Pts',(-21.9518084987802,13.8436025045766,
-9.0925132222994));
#113522=CARTESIAN_POINT('Ctrl Pts',(-21.9445591294989,13.9071468606963,
-8.97972528399588));
#113523=CARTESIAN_POINT('Ctrl Pts',(-21.9373097602177,13.9655440160805,
-8.86405097009453));
#113524=CARTESIAN_POINT('Ctrl Pts',(-21.9300603909364,14.0185518970946,
-8.74597947917628));
#113525=CARTESIAN_POINT('Ctrl Pts',(-21.9275213328559,14.0371176623905,
-8.70462548526845));
#113526=CARTESIAN_POINT('Ctrl Pts',(-21.9249822747754,14.0550227368447,
-8.66297762867487));
#113527=CARTESIAN_POINT('Ctrl Pts',(-21.9224432166949,14.072258099233,-8.62105754707614));
#113528=CARTESIAN_POINT('Ctrl Pts',(-21.9151753922206,14.1215927676882,
-8.50106509895149));
#113529=CARTESIAN_POINT('Ctrl Pts',(-21.9079075677462,14.1654535201482,
-8.37879985409838));
#113530=CARTESIAN_POINT('Ctrl Pts',(-21.9006397432719,14.2036508556539,
-8.25477639656434));
#113531=CARTESIAN_POINT('Ctrl Pts',(-21.8933732460253,14.2418412156796,
-8.13077558781263));
#113532=CARTESIAN_POINT('Ctrl Pts',(-21.8861067487787,14.2743701213767,
-8.0050175340044));
#113533=CARTESIAN_POINT('Ctrl Pts',(-21.8788402515321,14.3010977675838,
-7.87803249683022));
#113534=CARTESIAN_POINT('Ctrl Pts',(-21.8715735448853,14.3278261840071,
-7.75104380030113));
#113535=CARTESIAN_POINT('Ctrl Pts',(-21.8643068382385,14.3487529329938,
-7.6228283840705));
#113536=CARTESIAN_POINT('Ctrl Pts',(-21.8570401315917,14.3637891445478,
-7.49392756590881));
#113537=CARTESIAN_POINT('Ctrl Pts',(-21.8497738247676,14.3788245287919,
-7.36503384002021));
#113538=CARTESIAN_POINT('Ctrl Pts',(-21.8425075179435,14.3879699855593,
-7.23545512785121));
#113539=CARTESIAN_POINT('Ctrl Pts',(-21.8352412111193,14.3911884386049,
-7.10573860345731));
#113540=CARTESIAN_POINT('Ctrl Pts',(-21.8279736222961,14.3944074594842,
-6.97599919309588));
#113541=CARTESIAN_POINT('Ctrl Pts',(-21.8207060334729,14.3916973798453,
-6.84612226427044));
#113542=CARTESIAN_POINT('Ctrl Pts',(-21.8134384446498,14.3830732316722,
-6.71665610505596));
#113543=CARTESIAN_POINT('Ctrl Pts',(-21.8109914870288,14.3801695278977,
-6.67306555354588));
#113544=CARTESIAN_POINT('Ctrl Pts',(-21.8085445294078,14.3765958228007,
-6.62952155223097));
#113545=CARTESIAN_POINT('Ctrl Pts',(-21.8060975717868,14.3723540173125,
-6.58604494473972));
#113546=CARTESIAN_POINT('Ctrl Pts',(-21.7989004737786,14.35987783482,-6.45816965891825));
#113547=CARTESIAN_POINT('Ctrl Pts',(-21.7917033757704,14.3416132490332,
-6.33082772123226));
#113548=CARTESIAN_POINT('Ctrl Pts',(-21.7845062777622,14.3176299764922,
-6.20455276730157));
#113549=CARTESIAN_POINT('Ctrl Pts',(-21.7773108057981,14.2936521225045,
-6.07830634273716));
#113550=CARTESIAN_POINT('Ctrl Pts',(-21.770115333834,14.2639582246201,-5.95312677071234));
#113551=CARTESIAN_POINT('Ctrl Pts',(-21.7629198618699,14.2286692912606,
-5.82953850059646));
#113552=CARTESIAN_POINT('Ctrl Pts',(-21.7557239357197,14.1933781304247,
-5.70594242945247));
#113553=CARTESIAN_POINT('Ctrl Pts',(-21.7485280095695,14.1524913221394,
-5.5839382043744));
#113554=CARTESIAN_POINT('Ctrl Pts',(-21.7413320834193,14.1061801009768,
-5.46403633685718));
#113555=CARTESIAN_POINT('Ctrl Pts',(-21.7341362386062,14.0598694032798,
-5.34413582461646));
#113556=CARTESIAN_POINT('Ctrl Pts',(-21.7269403937931,14.0081345469274,
-5.22633795320274));
#113557=CARTESIAN_POINT('Ctrl Pts',(-21.7197445489799,13.951195264075,-5.11113412108044));
#113558=CARTESIAN_POINT('Ctrl Pts',(-21.7125463803664,13.8942375934544,
-4.9958930854447));
#113559=CARTESIAN_POINT('Ctrl Pts',(-21.7053482117529,13.8320722985288,
-4.8832480808549));
#113560=CARTESIAN_POINT('Ctrl Pts',(-21.6981500431394,13.7649656431987,
-4.77366701566866));
#113561=CARTESIAN_POINT('Ctrl Pts',(-21.6953506710525,13.7388678247307,
-4.73105087375697));
#113562=CARTESIAN_POINT('Ctrl Pts',(-21.6925512989656,13.7120231386475,
-4.68889785170956));
#113563=CARTESIAN_POINT('Ctrl Pts',(-21.6897519268786,13.6844490489701,
-4.64723433822518));
#113564=CARTESIAN_POINT('Ctrl Pts',(-21.6823651612314,13.6116886826953,
-4.53729589467605));
#113565=CARTESIAN_POINT('Ctrl Pts',(-21.6749783955841,13.5338219832499,
-4.43073073882055));
#113566=CARTESIAN_POINT('Ctrl Pts',(-21.6675916299368,13.4511815146991,
-4.32799683478733));
#113567=CARTESIAN_POINT('Ctrl Pts',(-21.6602057767909,13.3685512548839,
-4.2252756216705));
#113568=CARTESIAN_POINT('Ctrl Pts',(-21.652819923645,13.281148602485,-4.12638496293451));
#113569=CARTESIAN_POINT('Ctrl Pts',(-21.645434070499,13.1893468117984,-4.03175026516851));
#113570=CARTESIAN_POINT('Ctrl Pts',(-21.6380488592528,13.0975529995455,
-3.93712379204228));
#113571=CARTESIAN_POINT('Ctrl Pts',(-21.6306636480065,13.0013610322878,
-3.84675277061771));
#113572=CARTESIAN_POINT('Ctrl Pts',(-21.6232784367602,12.9011817562969,
-3.76102651418525));
#113573=CARTESIAN_POINT('Ctrl Pts',(-21.6158945838923,12.8010209065034,
-3.67531602557404));
#113574=CARTESIAN_POINT('Ctrl Pts',(-21.6085107310244,12.6968744537646,
-3.59424880257396));
#113575=CARTESIAN_POINT('Ctrl Pts',(-21.6011268781565,12.5891872591908,
-3.51817467598181));
#113576=CARTESIAN_POINT('Ctrl Pts',(-21.5937442414511,12.4815178013097,
-3.44211307923043));
#113577=CARTESIAN_POINT('Ctrl Pts',(-21.5863616047457,12.3703090248018,
-3.37104312100045));
#113578=CARTESIAN_POINT('Ctrl Pts',(-21.5789789680403,12.2560360828037,
-3.30527223079506));
#113579=CARTESIAN_POINT('Ctrl Pts',(-21.577121406017,12.2272836077984,-3.2887234674252));
#113580=CARTESIAN_POINT('Ctrl Pts',(-21.5752638439937,12.1983372842333,
-3.27250996499309));
#113581=CARTESIAN_POINT('Ctrl Pts',(-21.5734062819704,12.1692049547297,
-3.25663617882909));
#113582=CARTESIAN_POINT('Ctrl Pts',(-21.5663770387532,12.0589646359696,
-3.19656781915905));
#113583=CARTESIAN_POINT('Ctrl Pts',(-21.5593477955361,11.9460238764199,
-3.14134860569491));
#113584=CARTESIAN_POINT('Ctrl Pts',(-21.5523185523189,11.8308409812737,
-3.09121401641908));
#113585=CARTESIAN_POINT('Ctrl Pts',(-21.5452910829351,11.7156871525937,
-3.04109207863409));
#113586=CARTESIAN_POINT('Ctrl Pts',(-21.5382636135512,11.598292668025,-2.99605236218513));
#113587=CARTESIAN_POINT('Ctrl Pts',(-21.5312361441674,11.4791373964743,
-2.95628291073201));
#113588=CARTESIAN_POINT('Ctrl Pts',(-21.5242072492004,11.3599579532428,
-2.91650539170054));
#113589=CARTESIAN_POINT('Ctrl Pts',(-21.5171783542334,11.2390173728664,
-2.88200040031871));
#113590=CARTESIAN_POINT('Ctrl Pts',(-21.5101494592664,11.1168123916017,
-2.85290665147386));
#113591=CARTESIAN_POINT('Ctrl Pts',(-21.5031198947892,10.9945957701737,
-2.82381013141641));
#113592=CARTESIAN_POINT('Ctrl Pts',(-21.496090330312,10.8711148837365,-2.80012596375325));
#113593=CARTESIAN_POINT('Ctrl Pts',(-21.4890607658348,10.7468776224925,
-2.78194193126202));
#113594=CARTESIAN_POINT('Ctrl Pts',(-21.4820266213085,10.6225594155855,
-2.76374605112903));
#113595=CARTESIAN_POINT('Ctrl Pts',(-21.4749924767822,10.4974842312982,
-2.75105751390997));
#113596=CARTESIAN_POINT('Ctrl Pts',(-21.4679583322559,10.3721662707993,
-2.7439123504072));
#113597=CARTESIAN_POINT('Ctrl Pts',(-21.4643257671913,10.3074497095221,
-2.74022245304675));
#113598=CARTESIAN_POINT('Ctrl Pts',(-21.4606932021268,10.2426684536507,
-2.73801005930991));
#113599=CARTESIAN_POINT('Ctrl Pts',(-21.4570606370622,10.1778933606384,
-2.73727468834243));
#113600=CARTESIAN_POINT('Ctrl Pts',(-21.4494486360556,10.0421578502062,
-2.73573372639261));
#113601=CARTESIAN_POINT('Ctrl Pts',(-21.4418366350489,9.90636208137426,
-2.74068047835051));
#113602=CARTESIAN_POINT('Ctrl Pts',(-21.4342246340423,9.77110640803279,
-2.75209192269456));
#113603=CARTESIAN_POINT('Ctrl Pts',(-21.4264321638849,9.63264402511851,
-2.76377391530407));
#113604=CARTESIAN_POINT('Ctrl Pts',(-21.4186396937276,9.49474795528324,
-2.78223096696343));
#113605=CARTESIAN_POINT('Ctrl Pts',(-21.4108472235702,9.35805779034524,
-2.80738197337714));
#113606=CARTESIAN_POINT('Ctrl Pts',(-21.4032412105133,9.22463832793057,
-2.83193117014216));
#113607=CARTESIAN_POINT('Ctrl Pts',(-21.3956351974563,9.09236799004524,
-2.86285756196605));
#113608=CARTESIAN_POINT('Ctrl Pts',(-21.3880291843993,8.96183334801938,
-2.90003370869316));
#113609=CARTESIAN_POINT('Ctrl Pts',(-21.3801434856918,8.82649873181441,
-2.93857688367882));
#113610=CARTESIAN_POINT('Ctrl Pts',(-21.3722577869842,8.69303018501617,
-2.98383817560741));
#113611=CARTESIAN_POINT('Ctrl Pts',(-21.3643720882767,8.56206766416862,
-3.03561797090767));
#113612=CARTESIAN_POINT('Ctrl Pts',(-21.3564863895691,8.43110514332108,
-3.08739776620794));
#113613=CARTESIAN_POINT('Ctrl Pts',(-21.3486006908616,8.30264895994336,
-3.14569598622589));
#113614=CARTESIAN_POINT('Ctrl Pts',(-21.340714992154,8.17732045741597,-3.2102554131556));
#113615=CARTESIAN_POINT('Ctrl Pts',(-21.3336761719785,8.06545151277584,
-3.26788153021242));
#113616=CARTESIAN_POINT('Ctrl Pts',(-21.3266373518029,7.95611455042713,
-3.33047599778825));
#113617=CARTESIAN_POINT('Ctrl Pts',(-21.3195985316273,7.84976015631307,
-3.39778467535514));
#113618=CARTESIAN_POINT('Ctrl Pts',(-21.3125599213837,7.74340893420629,
-3.46509134544864));
#113619=CARTESIAN_POINT('Ctrl Pts',(-21.3055213111402,7.6400404255637,-3.53711173986184));
#113620=CARTESIAN_POINT('Ctrl Pts',(-21.2984827008966,7.54007733081936,
-3.61354769111783));
#113621=CARTESIAN_POINT('Ctrl Pts',(-21.2914403979205,7.44006179149318,
-3.69002374368832));
#113622=CARTESIAN_POINT('Ctrl Pts',(-21.2843980949443,7.34345554026389,
-3.77091974958848));
#113623=CARTESIAN_POINT('Ctrl Pts',(-21.2773557919682,7.25064938419331,
-3.85589629117145));
#113624=CARTESIAN_POINT('Ctrl Pts',(-21.270311531557,7.15781743229572,-3.94089645231006));
#113625=CARTESIAN_POINT('Ctrl Pts',(-21.2632672711458,7.06878795662045,
-4.02997914451082));
#113626=CARTESIAN_POINT('Ctrl Pts',(-21.2562230107345,6.98391525521804,
-4.12276771646865));
#113627=CARTESIAN_POINT('Ctrl Pts',(-21.2491723165041,6.89896503600872,
-4.21564103613083));
#113628=CARTESIAN_POINT('Ctrl Pts',(-21.2421216222736,6.8181794261953,-4.31222670801673));
#113629=CARTESIAN_POINT('Ctrl Pts',(-21.2350709280432,6.74187298426385,
-4.41211433748425));
#113630=CARTESIAN_POINT('Ctrl Pts',(-21.2315037344441,6.70326687792428,
-4.46265099399217));
#113631=CARTESIAN_POINT('Ctrl Pts',(-21.2279365408449,6.6658066369646,-4.51403236253905));
#113632=CARTESIAN_POINT('Ctrl Pts',(-21.2243693472458,6.62952875518707,
-4.56620249702597));
#113633=CARTESIAN_POINT('Ctrl Pts',(-21.2173459196766,6.55810143621733,
-4.66891998366267));
#113634=CARTESIAN_POINT('Ctrl Pts',(-21.2103224921073,6.49113206267362,
-4.77488133278218));
#113635=CARTESIAN_POINT('Ctrl Pts',(-21.203299064538,6.42891752586231,-4.88366865729751));
#113636=CARTESIAN_POINT('Ctrl Pts',(-21.1962814635001,6.3667546013078,-4.99236573346224));
#113637=CARTESIAN_POINT('Ctrl Pts',(-21.1892638624622,6.30933885072374,
-5.10388378270884));
#113638=CARTESIAN_POINT('Ctrl Pts',(-21.1822462614242,6.25692354442136,
-5.21777650231572));
#113639=CARTESIAN_POINT('Ctrl Pts',(-21.1752329179883,6.20454003866059,
-5.33160012282876));
#113640=CARTESIAN_POINT('Ctrl Pts',(-21.1682195745524,6.15715109672532,
-5.44779519409355));
#113641=CARTESIAN_POINT('Ctrl Pts',(-21.1612062311164,6.11496361461179,
-5.5658917019994));
#113642=CARTESIAN_POINT('Ctrl Pts',(-21.1541425572128,6.07247337879379,
-5.6848357161669));
#113643=CARTESIAN_POINT('Ctrl Pts',(-21.1470788833092,6.03525973704695,
-5.80570821283149));
#113644=CARTESIAN_POINT('Ctrl Pts',(-21.1400152094056,6.00348440058743,
-5.92800920087711));
#113645=CARTESIAN_POINT('Ctrl Pts',(-21.133004253243,5.97194621040375,-6.04939742993803));
#113646=CARTESIAN_POINT('Ctrl Pts',(-21.1259932970804,5.94576549596376,
-6.17219251371173));
#113647=CARTESIAN_POINT('Ctrl Pts',(-21.1189823409179,5.925049909777,-6.29589174211361));
#113648=CARTESIAN_POINT('Ctrl Pts',(-21.1119707114441,5.90433233412748,
-6.41960285021839));
#113649=CARTESIAN_POINT('Ctrl Pts',(-21.1049590819704,5.88908099593137,
-6.54421789437491));
#113650=CARTESIAN_POINT('Ctrl Pts',(-21.0979474524966,5.87935206069904,
-6.66922591689215));
#113651=CARTESIAN_POINT('Ctrl Pts',(-21.0909337323132,5.86962022451783,
-6.79427121398003));
#113652=CARTESIAN_POINT('Ctrl Pts',(-21.0839200121298,5.86541410001686,
-6.91970933719594));
#113653=CARTESIAN_POINT('Ctrl Pts',(-21.0769062919464,5.86673779564441,
-7.04502653792429));
#113654=CARTESIAN_POINT('Ctrl Pts',(-21.06980393907,5.8680782188723,-7.17192737767607));
#113655=CARTESIAN_POINT('Ctrl Pts',(-21.0627015861936,5.87508918354248,
-7.29870380973344));
#113656=CARTESIAN_POINT('Ctrl Pts',(-21.0555992333171,5.88772067164072,
-7.42482599909129));
#113657=CARTESIAN_POINT('Ctrl Pts',(-21.0485733140547,5.90021622305687,
-7.54959089532375));
#113658=CARTESIAN_POINT('Ctrl Pts',(-21.0415473947922,5.9182117997394,-7.67371518534136));
#113659=CARTESIAN_POINT('Ctrl Pts',(-21.0345214755298,5.9416072606581,-7.79669530171039));
#113660=CARTESIAN_POINT('Ctrl Pts',(-21.0273809058464,5.96538449360439,
-7.92168223335618));
#113661=CARTESIAN_POINT('Ctrl Pts',(-21.020240336163,5.99473928967706,-8.04548691534146));
#113662=CARTESIAN_POINT('Ctrl Pts',(-21.0130997664796,6.02951374026827,
-8.16759653562821));
#113663=CARTESIAN_POINT('Ctrl Pts',(-21.0059591967962,6.06428819085948,
-8.28970615591497));
#113664=CARTESIAN_POINT('Ctrl Pts',(-20.9988186271128,6.10448211338605,
-8.41012033914232));
#113665=CARTESIAN_POINT('Ctrl Pts',(-20.9916780574294,6.14988677165161,
-8.52834798156522));
#113666=CARTESIAN_POINT('Ctrl Pts',(-20.9848875394138,6.19306556040558,
-8.6407797582169));
#113667=CARTESIAN_POINT('Ctrl Pts',(-20.9780970213983,6.24110041539954,
-8.75160786112374));
#113668=CARTESIAN_POINT('Ctrl Pts',(-20.9713065033827,6.29385322449215,
-8.86037168693147));
#113669=CARTESIAN_POINT('Ctrl Pts',(-20.964525196406,6.34653447672102,-8.96898797939648));
#113670=CARTESIAN_POINT('Ctrl Pts',(-20.9577438894292,6.40392078324138,
-9.07554518694513));
#113671=CARTESIAN_POINT('Ctrl Pts',(-20.9509625824525,6.46582471863268,
-9.17959914495719));
#113672=CARTESIAN_POINT('Ctrl Pts',(-20.9441885968762,6.52766181978393,
-9.28354076169135));
#113673=CARTESIAN_POINT('Ctrl Pts',(-20.9374146112999,6.59400664137681,
-9.38498414360832));
#113674=CARTESIAN_POINT('Ctrl Pts',(-20.9306406257236,6.66462456931131,
-9.48350704645866));
#113675=CARTESIAN_POINT('Ctrl Pts',(-20.923872081502,6.73518577182298,-9.58195080859381));
#113676=CARTESIAN_POINT('Ctrl Pts',(-20.9171035372804,6.81001301240761,
-9.67747841681211));
#113677=CARTESIAN_POINT('Ctrl Pts',(-20.9103349930588,6.88882723169973,
-9.76969475011184));
#113678=CARTESIAN_POINT('Ctrl Pts',(-20.9035692778455,6.96760850947957,
-9.8618725402971));
#113679=CARTESIAN_POINT('Ctrl Pts',(-20.8968035626323,7.05037318437453,
-9.9507414859558));
#113680=CARTESIAN_POINT('Ctrl Pts',(-20.890037847419,7.13680097017415,-10.0359383256054));
#113681=CARTESIAN_POINT('Ctrl Pts',(-20.8832733657405,7.2232129983373,-10.1211196320463));
#113682=CARTESIAN_POINT('Ctrl Pts',(-20.8765088840621,7.31328651177657,
-10.2026298682361));
#113683=CARTESIAN_POINT('Ctrl Pts',(-20.8697444023836,7.40666387645209,
-10.28014213782));
#113684=CARTESIAN_POINT('Ctrl Pts',(-20.8629794634639,7.50004755291707,
-10.3576596468014));
#113685=CARTESIAN_POINT('Ctrl Pts',(-20.8562145245441,7.59673520141363,
-10.4311783842624));
#113686=CARTESIAN_POINT('Ctrl Pts',(-20.8494495856244,7.6963362060632,-10.5004118260392));
#113687=CARTESIAN_POINT('Ctrl Pts',(-20.8426824984199,7.79596884016584,
-10.5696672536977));
#113688=CARTESIAN_POINT('Ctrl Pts',(-20.8359154112155,7.8985163245618,-10.6346344420979));
#113689=CARTESIAN_POINT('Ctrl Pts',(-20.829148324011,8.00355986516484,-10.6950707088088));
#113690=CARTESIAN_POINT('Ctrl Pts',(-20.8223732475449,8.10872742076868,
-10.7555783269196));
#113691=CARTESIAN_POINT('Ctrl Pts',(-20.8155981710788,8.21639654982388,
-10.8115441384382));
#113692=CARTESIAN_POINT('Ctrl Pts',(-20.8088230946128,8.3261246357037,-10.8627718409776));
#113693=CARTESIAN_POINT('Ctrl Pts',(-20.8020434620293,8.43592651175376,
-10.9140339932283));
#113694=CARTESIAN_POINT('Ctrl Pts',(-20.7952638294458,8.54778971316061,
-10.9605515370318));
#113695=CARTESIAN_POINT('Ctrl Pts',(-20.7884841968622,8.66125425324206,
-11.002177335792));
#113696=CARTESIAN_POINT('Ctrl Pts',(-20.7816937465263,8.77489984020051,
-11.0438695537248));
#113697=CARTESIAN_POINT('Ctrl Pts',(-20.7749032961903,8.89015146681934,
-11.0806543242509));
#113698=CARTESIAN_POINT('Ctrl Pts',(-20.7681128458544,9.00653654290877,
-11.1124350540814));
#113699=CARTESIAN_POINT('Ctrl Pts',(-20.7650708197739,9.05867541725731,
-11.1266723732895));
#113700=CARTESIAN_POINT('Ctrl Pts',(-20.7620287936935,9.11104166406988,
-11.1399061162083));
#113701=CARTESIAN_POINT('Ctrl Pts',(-20.7589867676131,9.16359245771118,
-11.1521309733376));
#113702=CARTESIAN_POINT('Ctrl Pts',(-20.7486393029828,9.34234420543419,
-11.1937138767748));
#113703=CARTESIAN_POINT('Ctrl Pts',(-20.7382918383526,9.5237420713755,-11.2237406026673));
#113704=CARTESIAN_POINT('Ctrl Pts',(-20.7279443737223,9.70657007694164,
-11.2419687976436));
#113705=CARTESIAN_POINT('Ctrl Pts',(-20.7200690256185,9.84571857741016,
-11.2558420879492));
#113706=CARTESIAN_POINT('Ctrl Pts',(-20.7121936775147,9.9856955507432,-11.2628818575557));
#113707=CARTESIAN_POINT('Ctrl Pts',(-20.7043183294109,10.1259540174844,
-11.2629985252177));
#113708=CARTESIAN_POINT('Ctrl Pts',(-20.7043183293681,10.1259540182473,
-11.2629985252183));
#113709=CARTESIAN_POINT('Ctrl Pts',(-20.6972124917565,10.2525076480267,
-11.2631037931088));
#113710=CARTESIAN_POINT('Ctrl Pts',(-20.690106654145,10.3792358913459,-11.2575688510535));
#113711=CARTESIAN_POINT('Ctrl Pts',(-20.6830008165335,10.5055936861433,
-11.2463775785066));
#113712=CARTESIAN_POINT('Ctrl Pts',(-20.6761359770942,10.62766599072,-11.235565863779));
#113713=CARTESIAN_POINT('Ctrl Pts',(-20.6692711376549,10.7493921146474,
-11.2194752750085));
#113714=CARTESIAN_POINT('Ctrl Pts',(-20.6624062982156,10.8702797228384,
-11.1981441616781));
#113715=CARTESIAN_POINT('Ctrl Pts',(-20.6555455951751,10.9910944903822,
-11.176825901378));
#113716=CARTESIAN_POINT('Ctrl Pts',(-20.6486848921345,11.1110713460377,
-11.1502734673399));
#113717=CARTESIAN_POINT('Ctrl Pts',(-20.6418241890939,11.2297241573343,
-11.11857691486));
#113718=CARTESIAN_POINT('Ctrl Pts',(-20.6349660822477,11.3483320686035,
-11.0868923568375));
#113719=CARTESIAN_POINT('Ctrl Pts',(-20.6281079754014,11.4656165386136,
-11.0500676597437));
#113720=CARTESIAN_POINT('Ctrl Pts',(-20.6212498685552,11.5811033394191,
-11.0082435985089));
#113721=CARTESIAN_POINT('Ctrl Pts',(-20.6205160050467,11.5934612029986,
-11.0037681429635));
#113722=CARTESIAN_POINT('Ctrl Pts',(-20.6197821415383,11.6057984965267,
-10.9992354896429));
#113723=CARTESIAN_POINT('Ctrl Pts',(-20.6190482780298,11.6181146495903,
-10.9946458447559));
#113724=CARTESIAN_POINT('',(-21.113681670589,10.1291791134783,-11.262999987923));
#113725=CARTESIAN_POINT('Ctrl Pts',(-21.0285562874006,11.6181146495903,
-10.9946458447559));
#113726=CARTESIAN_POINT('Ctrl Pts',(-21.0355840156022,11.5004192767385,
-11.0385053164149));
#113727=CARTESIAN_POINT('Ctrl Pts',(-21.0426117438038,11.3807634475762,
-11.0771668462722));
#113728=CARTESIAN_POINT('Ctrl Pts',(-21.0496394720055,11.2596369012063,
-11.1104695090138));
#113729=CARTESIAN_POINT('Ctrl Pts',(-21.0566691422659,11.1384768824449,
-11.1437813746906));
#113730=CARTESIAN_POINT('Ctrl Pts',(-21.0636988125263,11.015845704538,-11.1717313079601));
#113731=CARTESIAN_POINT('Ctrl Pts',(-21.0707284827866,10.8922472189185,
-11.1942085880452));
#113732=CARTESIAN_POINT('Ctrl Pts',(-21.0773994741671,10.7749551694116,
-11.2155389970329));
#113733=CARTESIAN_POINT('Ctrl Pts',(-21.0840704655475,10.6567923830643,
-11.2319413112385));
#113734=CARTESIAN_POINT('Ctrl Pts',(-21.0907414569279,10.5381962379688,
-11.2433638054108));
#113735=CARTESIAN_POINT('Ctrl Pts',(-21.0983881948149,10.4022533796668,
-11.2564570345833));
#113736=CARTESIAN_POINT('Ctrl Pts',(-21.106034932702,10.2657163342166,-11.2630102654163));
#113737=CARTESIAN_POINT('Ctrl Pts',(-21.113681670589,10.1291791134783,-11.262999987923));
#113738=CARTESIAN_POINT('Ctrl Pts',(-22.5286570444943,11.618114651272,-10.9946458441291));
#113739=CARTESIAN_POINT('Ctrl Pts',(-22.5118635566228,11.897231423232,-10.8906322888935));
#113740=CARTESIAN_POINT('Ctrl Pts',(-22.4949369598826,12.1647784889961,
-10.7576137578564));
#113741=CARTESIAN_POINT('Ctrl Pts',(-22.465868647502,12.6053453742023,-10.4775732694343));
#113742=CARTESIAN_POINT('Ctrl Pts',(-22.4535277673545,12.7845915575229,
-10.342725835719));
#113743=CARTESIAN_POINT('Ctrl Pts',(-22.4257236293028,13.1587098476615,
-10.0121171914199));
#113744=CARTESIAN_POINT('Ctrl Pts',(-22.4102376602721,13.3468564292045,
-9.81026178837383));
#113745=CARTESIAN_POINT('Ctrl Pts',(-22.3707644790326,13.7710499653168,
-9.25626921794873));
#113746=CARTESIAN_POINT('Ctrl Pts',(-22.3475332219828,13.9766060759535,
-8.88452249893456));
#113747=CARTESIAN_POINT('Ctrl Pts',(-22.2991968843045,14.2796126782055,
-8.07143533541486));
#113748=CARTESIAN_POINT('Ctrl Pts',(-22.2738516834091,14.3687709152418,
-7.63244160595406));
#113749=CARTESIAN_POINT('Ctrl Pts',(-22.23441490211,14.399879921126,-6.92636524613201));
#113750=CARTESIAN_POINT('Ctrl Pts',(-22.2200357352687,14.3873239022266,
-6.66458234195366));
#113751=CARTESIAN_POINT('Ctrl Pts',(-22.1818226587369,14.2917628569607,
-5.98591647449479));
#113752=CARTESIAN_POINT('Ctrl Pts',(-22.1576959023024,14.1704129201896,
-5.57739311561262));
#113753=CARTESIAN_POINT('Ctrl Pts',(-22.120506117992,13.8882519171042,-4.97428159231956));
#113754=CARTESIAN_POINT('Ctrl Pts',(-22.1071892271123,13.7672009592946,
-4.76418119343851));
#113755=CARTESIAN_POINT('Ctrl Pts',(-22.0671851319122,13.3567031829939,
-4.17411333030861));
#113756=CARTESIAN_POINT('Ctrl Pts',(-22.0400476309531,13.0207019334589,
-3.83117957033724));
#113757=CARTESIAN_POINT('Ctrl Pts',(-21.9977759452388,12.4066947984301,
-3.38514702377261));
#113758=CARTESIAN_POINT('Ctrl Pts',(-21.9822619869133,12.1625184551894,
-3.24239234048036));
#113759=CARTESIAN_POINT('Ctrl Pts',(-21.9508603667187,11.6519681345354,
-3.0083368422622));
#113760=CARTESIAN_POINT('Ctrl Pts',(-21.935050555265,11.387067969271,-2.91713343544298));
#113761=CARTESIAN_POINT('Ctrl Pts',(-21.8879448747146,10.5757587952574,
-2.72432313185626));
#113762=CARTESIAN_POINT('Ctrl Pts',(-21.8579334985496,10.0164989908293,
-2.70258320307757));
#113763=CARTESIAN_POINT('Ctrl Pts',(-21.8116752950662,9.20696693094667,
-2.82958879436635));
#113764=CARTESIAN_POINT('Ctrl Pts',(-21.7966322572004,8.94955550495293,
-2.89498639316289));
#113765=CARTESIAN_POINT('Ctrl Pts',(-21.7656932431054,8.42658696557584,
-3.08114689744676));
#113766=CARTESIAN_POINT('Ctrl Pts',(-21.749753784929,8.16393679313984,-3.2060725422022));
#113767=CARTESIAN_POINT('Ctrl Pts',(-21.7179039395933,7.67711327384761,
-3.50184230045521));
#113768=CARTESIAN_POINT('Ctrl Pts',(-21.7020905381782,7.45307322008557,
-3.67012909058175));
#113769=CARTESIAN_POINT('Ctrl Pts',(-21.6554089466727,6.84416001296812,
-4.22892638374964));
#113770=CARTESIAN_POINT('Ctrl Pts',(-21.6257875944964,6.5161027709379,-4.67284096003034));
#113771=CARTESIAN_POINT('Ctrl Pts',(-21.5799691432257,6.16697497015337,
-5.40572474724432));
#113772=CARTESIAN_POINT('Ctrl Pts',(-21.5649274230386,6.07559613988268,
-5.65493869451876));
#113773=CARTESIAN_POINT('Ctrl Pts',(-21.5243316192289,5.88959640808551,
-6.35891158709622));
#113774=CARTESIAN_POINT('Ctrl Pts',(-21.4989586169474,5.84505290256321,
-6.82310483597467));
#113775=CARTESIAN_POINT('Ctrl Pts',(-21.4577103596116,5.89390770742929,
-7.55139806143824));
#113776=CARTESIAN_POINT('Ctrl Pts',(-21.4426230694252,5.93668363740592,
-7.8152198623368));
#113777=CARTESIAN_POINT('Ctrl Pts',(-21.4153081095326,6.06029511506826,
-8.29036328542627));
#113778=CARTESIAN_POINT('Ctrl Pts',(-21.4029254648302,6.13379986021384,
-8.50261308988648));
#113779=CARTESIAN_POINT('Ctrl Pts',(-21.3748148471002,6.33555715266349,
-8.96396493236319));
#113780=CARTESIAN_POINT('Ctrl Pts',(-21.359056941832,6.47232512473378,-9.20821749927028));
#113781=CARTESIAN_POINT('Ctrl Pts',(-21.3114335368598,6.95387034171625,
-9.89922444270409));
#113782=CARTESIAN_POINT('Ctrl Pts',(-21.2810313155863,7.36408465176337,
-10.2928121714641));
#113783=CARTESIAN_POINT('Ctrl Pts',(-21.2277055352677,8.16233740054543,
-10.8013827607725));
#113784=CARTESIAN_POINT('Ctrl Pts',(-21.2060291048435,8.51211569060141,
-10.9628682676951));
#113785=CARTESIAN_POINT('Ctrl Pts',(-21.1729824186689,9.08072693148724,
-11.1373756926973));
#113786=CARTESIAN_POINT('Ctrl Pts',(-21.1612647077837,9.28702167925944,
-11.1842599164102));
#113787=CARTESIAN_POINT('Ctrl Pts',(-21.1375559300196,9.70555363933832,
-11.2471601909553));
#113788=CARTESIAN_POINT('Ctrl Pts',(-21.1255964907356,9.91722036984201,
-11.2629838551454));
#113789=CARTESIAN_POINT('Ctrl Pts',(-21.1136182899058,10.1291755310197,
-11.2629999876519));
#113790=CARTESIAN_POINT('Origin',(23.734,10.1295,-7.));
#113791=CARTESIAN_POINT('Ctrl Pts',(18.0286142064722,8.64088528410776,-10.9946458200483));
#113792=CARTESIAN_POINT('Ctrl Pts',(18.039789912646,8.82947631661819,-11.0649247381119));
#113793=CARTESIAN_POINT('Ctrl Pts',(18.0508911903356,9.0228507750007,-11.1217761943531));
#113794=CARTESIAN_POINT('Ctrl Pts',(18.0855389971032,9.6287916599252,-11.2541654000867));
#113795=CARTESIAN_POINT('Ctrl Pts',(18.1093854435775,10.0489723497352,-11.2827744784006));
#113796=CARTESIAN_POINT('Ctrl Pts',(18.1471816832798,10.7245663649431,-11.2291906086153));
#113797=CARTESIAN_POINT('Ctrl Pts',(18.1614166816315,10.9801743034163,-11.1852727903175));
#113798=CARTESIAN_POINT('Ctrl Pts',(18.1906211821946,11.4861716741905,-11.0500376008415));
#113799=CARTESIAN_POINT('Ctrl Pts',(18.2056646969047,11.7351865714645,-10.9579192772123));
#113800=CARTESIAN_POINT('Ctrl Pts',(18.2520848009178,12.4766910552346,-10.60204548056));
#113801=CARTESIAN_POINT('Ctrl Pts',(18.2822647792475,12.9271688953905,-10.2645189885224));
#113802=CARTESIAN_POINT('Ctrl Pts',(18.329563093998,13.4867230231185,-9.64202969247538));
#113803=CARTESIAN_POINT('Ctrl Pts',(18.345361847618,13.6526624310861,-9.41631982831584));
#113804=CARTESIAN_POINT('Ctrl Pts',(18.3745501635932,13.9192880709676,-8.96714577060878));
#113805=CARTESIAN_POINT('Ctrl Pts',(18.3879432541682,14.0251847377267,-8.74808388406812));
#113806=CARTESIAN_POINT('Ctrl Pts',(18.4231081417801,14.2510441149974,-8.15680596322861));
#113807=CARTESIAN_POINT('Ctrl Pts',(18.4452891829018,14.3395625397132,-7.77503814968497));
#113808=CARTESIAN_POINT('Ctrl Pts',(18.4823845661745,14.3994874163579,-7.11696128038773));
#113809=CARTESIAN_POINT('Ctrl Pts',(18.4973478486563,14.3982981455231,-6.84560261077265));
#113810=CARTESIAN_POINT('Ctrl Pts',(18.5347900650453,14.3311933762226,-6.1739546972112));
#113811=CARTESIAN_POINT('Ctrl Pts',(18.5577037585298,14.2339972468066,-5.7794830445814));
#113812=CARTESIAN_POINT('Ctrl Pts',(18.6118397780143,13.8735890188588,-4.88640863501065));
#113813=CARTESIAN_POINT('Ctrl Pts',(18.6422260148492,13.5645771307568,-4.414328195284));
#113814=CARTESIAN_POINT('Ctrl Pts',(18.7055320765152,12.7810685956465,-3.61529310228987));
#113815=CARTESIAN_POINT('Ctrl Pts',(18.7359956167877,12.3137769030668,-3.29648990138105));
#113816=CARTESIAN_POINT('Ctrl Pts',(18.7812358386468,11.5729102061597,-2.98133198485659));
#113817=CARTESIAN_POINT('Ctrl Pts',(18.7951410793747,11.3397496995108,-2.90507356509229));
#113818=CARTESIAN_POINT('Ctrl Pts',(18.8352496442113,10.6462105342338,-2.74269191595506));
#113819=CARTESIAN_POINT('Ctrl Pts',(18.8606370473304,10.1766533737762,-2.71170947289427));
#113820=CARTESIAN_POINT('Ctrl Pts',(18.9017617215762,9.44980269284018,-2.78332847763197));
#113821=CARTESIAN_POINT('Ctrl Pts',(18.9166849818414,9.19107287097638,-2.83326683536358));
#113822=CARTESIAN_POINT('Ctrl Pts',(18.9543381270769,8.54735185340598,-3.02055239473558));
#113823=CARTESIAN_POINT('Ctrl Pts',(18.9765378256604,8.17445315844397,-3.18988433444434));
#113824=CARTESIAN_POINT('Ctrl Pts',(19.0126006065023,7.63363564858332,-3.53605748654641));
#113825=CARTESIAN_POINT('Ctrl Pts',(19.0259264357665,7.4467759557336,-3.67867063866158));
#113826=CARTESIAN_POINT('Ctrl Pts',(19.071107642773,6.85183247790683,-4.21585674879132));
#113827=CARTESIAN_POINT('Ctrl Pts',(19.1018278831666,6.51104879615158,-4.67591755065589));
#113828=CARTESIAN_POINT('Ctrl Pts',(19.1493271776637,6.15427869555142,-5.43625436953596));
#113829=CARTESIAN_POINT('Ctrl Pts',(19.1647097775749,6.06232265312795,-5.69395204102108));
#113830=CARTESIAN_POINT('Ctrl Pts',(19.2024951208292,5.89678902636713,-6.35108753953332));
#113831=CARTESIAN_POINT('Ctrl Pts',(19.2246658134463,5.8543184988969,-6.7555744181102));
#113832=CARTESIAN_POINT('Ctrl Pts',(19.26284741727,5.87964274858108,-7.43003476984898));
#113833=CARTESIAN_POINT('Ctrl Pts',(19.2781161088495,5.91544590216238,-7.698549978111));
#113834=CARTESIAN_POINT('Ctrl Pts',(19.3146038421075,6.06281319314975,-8.33484019050179));
#113835=CARTESIAN_POINT('Ctrl Pts',(19.3355181941132,6.19904208319337,-8.69447252750772));
#113836=CARTESIAN_POINT('Ctrl Pts',(19.3695601003676,6.48666077411959,-9.22523293463471));
#113837=CARTESIAN_POINT('Ctrl Pts',(19.3820628650678,6.60680851926175,-9.41093055469459));
#113838=CARTESIAN_POINT('Ctrl Pts',(19.4101570323969,6.91027278029702,-9.80851650725058));
#113839=CARTESIAN_POINT('Ctrl Pts',(19.4256027430348,7.10115775317109,-10.0133596513102));
#113840=CARTESIAN_POINT('Ctrl Pts',(19.4697929587333,7.6988327593341,-10.5401551096626));
#113841=CARTESIAN_POINT('Ctrl Pts',(19.4992344458114,8.14600379075274,-10.8087494351287));
#113842=CARTESIAN_POINT('Ctrl Pts',(19.5283263127743,8.63383708158961,-10.9920139762997));
#113843=CARTESIAN_POINT('Ctrl Pts',(19.5285362900556,8.63736040044845,-10.9933322634436));
#113844=CARTESIAN_POINT('Ctrl Pts',(19.5287462306467,8.64088535560039,-10.9946458466902));
#113845=CARTESIAN_POINT('',(17.734,10.6581555755053,-11.2300936493755));
#113846=CARTESIAN_POINT('Ctrl Pts',(19.1191572628085,8.64088535679774,-10.9946458471364));
#113847=CARTESIAN_POINT('Ctrl Pts',(19.1119070035151,8.51958773180664,-10.949443987533));
#113848=CARTESIAN_POINT('Ctrl Pts',(19.1046567442216,8.40033276577294,-10.8987066521256));
#113849=CARTESIAN_POINT('Ctrl Pts',(19.0974064849282,8.28362436418113,-10.8426438993342));
#113850=CARTESIAN_POINT('Ctrl Pts',(19.0901561780298,8.16691519628698,-10.7865807784372));
#113851=CARTESIAN_POINT('Ctrl Pts',(19.0829058711315,8.0527529401722,-10.7251923151352));
#113852=CARTESIAN_POINT('Ctrl Pts',(19.0756555642332,7.9416194002362,-10.6587357763546));
#113853=CARTESIAN_POINT('Ctrl Pts',(19.0684059379202,7.83049629239121,-10.5922854758408));
#113854=CARTESIAN_POINT('Ctrl Pts',(19.0611563116072,7.72240162884374,-10.5207682287737));
#113855=CARTESIAN_POINT('Ctrl Pts',(19.0539066852942,7.61779038959773,-10.444486004183));
#113856=CARTESIAN_POINT('Ctrl Pts',(19.0466552587319,7.51315317296975,-10.3681848369578));
#113857=CARTESIAN_POINT('Ctrl Pts',(19.0394038321697,7.41200138947097,-10.2871165304907));
#113858=CARTESIAN_POINT('Ctrl Pts',(19.0321524056074,7.31475933410449,-10.2016252097574));
#113859=CARTESIAN_POINT('Ctrl Pts',(19.0260356350683,7.23273308253644,-10.1295110143619));
#113860=CARTESIAN_POINT('Ctrl Pts',(19.0199188645292,7.15348829353742,-10.0542504741919));
#113861=CARTESIAN_POINT('Ctrl Pts',(19.0138020939901,7.07726035300143,-9.97607159478566));
#113862=CARTESIAN_POINT('Ctrl Pts',(19.0065510835014,6.98689737586705,-9.88339591389356));
#113863=CARTESIAN_POINT('Ctrl Pts',(18.9993000730127,6.90074211026185,-9.78658493399704));
#113864=CARTESIAN_POINT('Ctrl Pts',(18.992049062524,6.81916133806592,-9.68604298984668));
#113865=CARTESIAN_POINT('Ctrl Pts',(18.9847994766285,6.7375965939005,-9.58552079899487));
#113866=CARTESIAN_POINT('Ctrl Pts',(18.9775498907331,6.66060476803244,-9.48126937442019));
#113867=CARTESIAN_POINT('Ctrl Pts',(18.9703003048376,6.58851243587805,-9.37372619961396));
#113868=CARTESIAN_POINT('Ctrl Pts',(18.9630504777803,6.51641770552822,-9.26617944731835));
#113869=CARTESIAN_POINT('Ctrl Pts',(18.9558006507229,6.44922299010419,-9.15534101108407));
#113870=CARTESIAN_POINT('Ctrl Pts',(18.9485508236655,6.38721176553186,-9.04167768517985));
#113871=CARTESIAN_POINT('Ctrl Pts',(18.9413013297149,6.32520339017975,-8.92801958174701));
#113872=CARTESIAN_POINT('Ctrl Pts',(18.9340518357642,6.26837819329272,-8.81153715258735));
#113873=CARTESIAN_POINT('Ctrl Pts',(18.9268023418135,6.21697378950106,-8.6927219654033));
#113874=CARTESIAN_POINT('Ctrl Pts',(18.9195513251248,6.16555858834258,-8.57388182138549));
#113875=CARTESIAN_POINT('Ctrl Pts',(18.912300308436,6.11956659127571,-8.45270825822438));
#113876=CARTESIAN_POINT('Ctrl Pts',(18.9050492917472,6.07918748442404,-8.32971332480681));
#113877=CARTESIAN_POINT('Ctrl Pts',(18.9025183441921,6.06509326755094,-8.28678227949547));
#113878=CARTESIAN_POINT('Ctrl Pts',(18.899987396637,6.05168245386202,-8.24362948664952));
#113879=CARTESIAN_POINT('Ctrl Pts',(18.8974564490819,6.03896168920779,-8.20027718796169));
#113880=CARTESIAN_POINT('Ctrl Pts',(18.8902054210853,6.00251738578437,-8.07607519457316));
#113881=CARTESIAN_POINT('Ctrl Pts',(18.8829543930887,5.97172744130365,-7.95018973388214));
#113882=CARTESIAN_POINT('Ctrl Pts',(18.8757033650922,5.94672659447985,-7.82314982723281));
#113883=CARTESIAN_POINT('Ctrl Pts',(18.868453762145,5.92173066108953,-7.69613488782295));
#113884=CARTESIAN_POINT('Ctrl Pts',(18.8612041591979,5.90252162251066,-7.56796629405867));
#113885=CARTESIAN_POINT('Ctrl Pts',(18.8539545562508,5.88918316891847,-7.43918352888816));
#113886=CARTESIAN_POINT('Ctrl Pts',(18.8467047129841,5.87584427316525,-7.31039649465304));
#113887=CARTESIAN_POINT('Ctrl Pts',(18.8394548697173,5.86837639052481,-7.18099559180068));
#113888=CARTESIAN_POINT('Ctrl Pts',(18.8322050264506,5.86681140365952,-7.05152601894956));
#113889=CARTESIAN_POINT('Ctrl Pts',(18.8249555168243,5.86524648881548,-6.9220624043351));
#113890=CARTESIAN_POINT('Ctrl Pts',(18.817706007198,5.86958392877581,-6.79253047173123));
#113891=CARTESIAN_POINT('Ctrl Pts',(18.8104564975717,5.8798034831745,-6.66347583313945));
#113892=CARTESIAN_POINT('Ctrl Pts',(18.8032054661206,5.89002518287282,-6.53439410326178));
#113893=CARTESIAN_POINT('Ctrl Pts',(18.7959544346696,5.90613143543126,-6.40579021215201));
#113894=CARTESIAN_POINT('Ctrl Pts',(18.7887034032186,5.92805006088456,-6.27820542457924));
#113895=CARTESIAN_POINT('Ctrl Pts',(18.7861725368703,5.93570043613603,-6.23367382275086));
#113896=CARTESIAN_POINT('Ctrl Pts',(18.783641670522,5.94405844734606,-6.1892663079349));
#113897=CARTESIAN_POINT('Ctrl Pts',(18.7811108041737,5.95311955176749,-6.14500564234539));
#113898=CARTESIAN_POINT('Ctrl Pts',(18.773859872354,5.97907961497491,-6.0181988401207));
#113899=CARTESIAN_POINT('Ctrl Pts',(18.7666089405343,6.01082393879235,-5.89255237034654));
#113900=CARTESIAN_POINT('Ctrl Pts',(18.7593580087146,6.04822384784453,-5.76859674767075));
#113901=CARTESIAN_POINT('Ctrl Pts',(18.7521085017796,6.08561640741904,-5.64466548358579));
#113902=CARTESIAN_POINT('Ctrl Pts',(18.7448589948447,6.12866223542571,-5.52242473459185));
#113903=CARTESIAN_POINT('Ctrl Pts',(18.7376094879098,6.17718265209152,-5.4023903538656));
#113904=CARTESIAN_POINT('Ctrl Pts',(18.7303597394478,6.22570468528001,-5.28235197403316));
#113905=CARTESIAN_POINT('Ctrl Pts',(18.7231099909859,6.27970154543043,-5.16452043124017));
#113906=CARTESIAN_POINT('Ctrl Pts',(18.7158602425239,6.33894610020495,-5.04939236832506));
#113907=CARTESIAN_POINT('Ctrl Pts',(18.7086108267425,6.39818793633194,-4.93426958847141));
#113908=CARTESIAN_POINT('Ctrl Pts',(18.7013614109611,6.46267682563546,-4.82185034692949));
#113909=CARTESIAN_POINT('Ctrl Pts',(18.6941119951796,6.53213938755326,-4.71260724316597));
#113910=CARTESIAN_POINT('Ctrl Pts',(18.6868610553831,6.60161655230259,-4.6033411736696));
#113911=CARTESIAN_POINT('Ctrl Pts',(18.6796101155865,6.67606929206711,-4.49725286707198));
#113912=CARTESIAN_POINT('Ctrl Pts',(18.6723591757899,6.75518036948062,-4.39478675899811));
#113913=CARTESIAN_POINT('Ctrl Pts',(18.6698278369485,6.78279843674699,-4.3590153353514));
#113914=CARTESIAN_POINT('Ctrl Pts',(18.667296498107,6.81098385947148,-4.32368509049485));
#113915=CARTESIAN_POINT('Ctrl Pts',(18.6647651592655,6.83972195599233,-4.28881401944369));
#113916=CARTESIAN_POINT('Ctrl Pts',(18.6575139800672,6.92204403957849,-4.18892364487664));
#113917=CARTESIAN_POINT('Ctrl Pts',(18.6502628008689,7.00893389101168,-4.09276746335985));
#113918=CARTESIAN_POINT('Ctrl Pts',(18.6430116216706,7.1000293559808,-4.00075399191298));
#113919=CARTESIAN_POINT('Ctrl Pts',(18.6357618670361,7.19110692437069,-3.90875859739654));
#113920=CARTESIAN_POINT('Ctrl Pts',(18.6285121124016,7.28638821505115,-3.82090453494306));
#113921=CARTESIAN_POINT('Ctrl Pts',(18.6212623577671,7.38547375701612,-3.7375639503868));
#113922=CARTESIAN_POINT('Ctrl Pts',(18.6140123636244,7.48456257244293,-3.65422061253054));
#113923=CARTESIAN_POINT('Ctrl Pts',(18.6067623694818,7.58745562811984,-3.57539127582746));
#113924=CARTESIAN_POINT('Ctrl Pts',(18.5995123753391,7.69371963756569,-3.50140842252495));
#113925=CARTESIAN_POINT('Ctrl Pts',(18.5922627157194,7.79997874386997,-3.42742898287495));
#113926=CARTESIAN_POINT('Ctrl Pts',(18.5850130560997,7.9096082081335,-3.35829577537722));
#113927=CARTESIAN_POINT('Ctrl Pts',(18.5777633964799,8.02214513874008,-3.29429838104521));
#113928=CARTESIAN_POINT('Ctrl Pts',(18.5705122175814,8.13470565320906,-3.23028757506482));
#113929=CARTESIAN_POINT('Ctrl Pts',(18.5632610386828,8.25017455020292,-3.17141490238704));
#113930=CARTESIAN_POINT('Ctrl Pts',(18.5560098597843,8.36806337543537,-3.11792452190296));
#113931=CARTESIAN_POINT('Ctrl Pts',(18.553479744642,8.4091976938689,-3.09926040900147));
#113932=CARTESIAN_POINT('Ctrl Pts',(18.5509496294997,8.45062643100319,-3.08125116393092));
#113933=CARTESIAN_POINT('Ctrl Pts',(18.5484195143573,8.49232821961963,-3.06390579869763));
#113934=CARTESIAN_POINT('Ctrl Pts',(18.5411687396156,8.61183672361191,-3.01419765142135));
#113935=CARTESIAN_POINT('Ctrl Pts',(18.5339179648738,8.73363233864965,-2.96992735561749));
#113936=CARTESIAN_POINT('Ctrl Pts',(18.526667190132,8.85720382874785,-2.93128626558502));
#113937=CARTESIAN_POINT('Ctrl Pts',(18.5194178403275,8.98075103432083,-2.89265276937961));
#113938=CARTESIAN_POINT('Ctrl Pts',(18.512168490523,9.10607308895427,-2.85964637530119));
#113939=CARTESIAN_POINT('Ctrl Pts',(18.5049191407185,9.23264281572258,-2.83240882631106));
#113940=CARTESIAN_POINT('Ctrl Pts',(18.4976695478915,9.35921678553134,-2.80517036422721));
#113941=CARTESIAN_POINT('Ctrl Pts',(18.4904199550646,9.48703817382436,-2.7837012099904));
#113942=CARTESIAN_POINT('Ctrl Pts',(18.4831703622376,9.61556849839147,-2.76809222552589));
#113943=CARTESIAN_POINT('Ctrl Pts',(18.4759211008008,9.7440929476379,-2.7524839545723));
#113944=CARTESIAN_POINT('Ctrl Pts',(18.468671839364,9.8733259249023,-2.74273535747441));
#113945=CARTESIAN_POINT('Ctrl Pts',(18.4614225779272,10.0027228802262,-2.7388855258393));
#113946=CARTESIAN_POINT('Ctrl Pts',(18.4541717893004,10.1321470953937,-2.73503488316649));
#113947=CARTESIAN_POINT('Ctrl Pts',(18.4469210006736,10.2617350119484,-2.73708549773513));
#113948=CARTESIAN_POINT('Ctrl Pts',(18.4396702120468,10.3909407646312,-2.74502435652223));
#113949=CARTESIAN_POINT('Ctrl Pts',(18.4371380978476,10.4360618870127,-2.74779675799403));
#113950=CARTESIAN_POINT('Ctrl Pts',(18.4346059836484,10.4811364186229,-2.7512867892791));
#113951=CARTESIAN_POINT('Ctrl Pts',(18.4320738694491,10.5261412037448,-2.75549240129178));
#113952=CARTESIAN_POINT('Ctrl Pts',(18.4248227506678,10.6550196890614,-2.76753585188386));
#113953=CARTESIAN_POINT('Ctrl Pts',(18.4175716318865,10.7833724865782,-2.78545561878685));
#113954=CARTESIAN_POINT('Ctrl Pts',(18.4103205131052,10.9106582237015,-2.80918136522904));
#113955=CARTESIAN_POINT('Ctrl Pts',(18.4030708203354,11.0379189286979,-2.83290244574471));
#113956=CARTESIAN_POINT('Ctrl Pts',(18.3958211275656,11.1641126522594,-2.86242716480153));
#113957=CARTESIAN_POINT('Ctrl Pts',(18.3885714347958,11.2887071690741,-2.89763388528435));
#113958=CARTESIAN_POINT('Ctrl Pts',(18.3813215040001,11.4133057766442,-2.93284176169347));
#113959=CARTESIAN_POINT('Ctrl Pts',(18.3740715732044,11.536304738905,-2.97373192183976));
#113960=CARTESIAN_POINT('Ctrl Pts',(18.3668216424088,11.6571856682521,-3.02013247720264));
#113961=CARTESIAN_POINT('Ctrl Pts',(18.3595720468175,11.7780610086043,-3.06653088721086));
#113962=CARTESIAN_POINT('Ctrl Pts',(18.3523224512263,11.8968181898397,-3.11843905729658));
#113963=CARTESIAN_POINT('Ctrl Pts',(18.3450728556351,12.0129577051053,-3.17563651399614));
#113964=CARTESIAN_POINT('Ctrl Pts',(18.3378217412121,12.1291215522637,-3.2328459538901));
#113965=CARTESIAN_POINT('Ctrl Pts',(18.3305706267891,12.2426663281592,-3.29534674046882));
#113966=CARTESIAN_POINT('Ctrl Pts',(18.3233195123661,12.3531157624676,-3.3628717453318));
#113967=CARTESIAN_POINT('Ctrl Pts',(18.3207890830911,12.3916594215088,-3.38643601961256));
#113968=CARTESIAN_POINT('Ctrl Pts',(18.318258653816,12.4298263586739,-3.41061174409129));
#113969=CARTESIAN_POINT('Ctrl Pts',(18.3157282245409,12.4675971128062,-3.43538629146338));
#113970=CARTESIAN_POINT('Ctrl Pts',(18.308476572844,12.5758397560588,-3.50638467512143));
#113971=CARTESIAN_POINT('Ctrl Pts',(18.3012249211471,12.6808655344705,-3.58232974729542));
#113972=CARTESIAN_POINT('Ctrl Pts',(18.2939732694502,12.7822289939055,-3.66290577224841));
#113973=CARTESIAN_POINT('Ctrl Pts',(18.2867230375805,12.8835726070214,-3.74346602092941));
#113974=CARTESIAN_POINT('Ctrl Pts',(18.2794728057108,12.9812550611857,-3.82865519873923));
#113975=CARTESIAN_POINT('Ctrl Pts',(18.272222573841,13.0748630102606,-3.91811652754548));
#113976=CARTESIAN_POINT('Ctrl Pts',(18.2649721003639,13.1684740787353,-4.00758083756907));
#113977=CARTESIAN_POINT('Ctrl Pts',(18.2577216268868,13.2580101184567,-4.10131734695304));
#113978=CARTESIAN_POINT('Ctrl Pts',(18.2504711534097,13.3430935434766,-4.19893135797681));
#113979=CARTESIAN_POINT('Ctrl Pts',(18.2432210145619,13.428173041662,-4.29654086384509));
#113980=CARTESIAN_POINT('Ctrl Pts',(18.2359708757141,13.5088001104695,-4.39802725173114));
#113981=CARTESIAN_POINT('Ctrl Pts',(18.2287207368664,13.584636598925,-4.50296173782437));
#113982=CARTESIAN_POINT('Ctrl Pts',(18.2214690829431,13.6604889350776,-4.60791815227929));
#113983=CARTESIAN_POINT('Ctrl Pts',(18.2142174290198,13.7315484893428,-4.71632382367757));
#113984=CARTESIAN_POINT('Ctrl Pts',(18.2069657750966,13.7975194901171,-4.82771962672384));
#113985=CARTESIAN_POINT('Ctrl Pts',(18.2044380432753,13.8205152093976,-4.86654921223581));
#113986=CARTESIAN_POINT('Ctrl Pts',(18.201910311454,13.8428930454219,-4.90574186097849));
#113987=CARTESIAN_POINT('Ctrl Pts',(18.1993825796327,13.8646417522872,-4.94527736900554));
#113988=CARTESIAN_POINT('Ctrl Pts',(18.192134450428,13.927004949233,-5.05864322053447));
#113989=CARTESIAN_POINT('Ctrl Pts',(18.1848863212232,13.9842146238742,-5.17487118894443));
#113990=CARTESIAN_POINT('Ctrl Pts',(18.1776381920185,14.0360251498106,-5.29347421528507));
#113991=CARTESIAN_POINT('Ctrl Pts',(18.1703915005286,14.0878253987829,-5.41205371592257));
#113992=CARTESIAN_POINT('Ctrl Pts',(18.1631448090387,14.1342284968229,-5.53300701759747));
#113993=CARTESIAN_POINT('Ctrl Pts',(18.1558981175488,14.1750364017306,-5.65582582145293));
#113994=CARTESIAN_POINT('Ctrl Pts',(18.1486511750523,14.2158457201186,-5.77864887943421));
#113995=CARTESIAN_POINT('Ctrl Pts',(18.1414042325558,14.2510593454277,-5.90333724128653));
#113996=CARTESIAN_POINT('Ctrl Pts',(18.1341572900592,14.2805285869955,-6.02936584134581));
#113997=CARTESIAN_POINT('Ctrl Pts',(18.1269106671075,14.309996529154,-6.15538888433221));
#113998=CARTESIAN_POINT('Ctrl Pts',(18.1196640441559,14.3337205171969,-6.28275170972903));
#113999=CARTESIAN_POINT('Ctrl Pts',(18.1124174212041,14.3516026666731,-6.41091760162758));
#114000=CARTESIAN_POINT('Ctrl Pts',(18.1051692316137,14.3694886820697,-6.53911120155683));
#114001=CARTESIAN_POINT('Ctrl Pts',(18.0979210420233,14.3815302891234,-6.66810787166596));
#114002=CARTESIAN_POINT('Ctrl Pts',(18.0906728524328,14.3876812579306,-6.79736393556808));
#114003=CARTESIAN_POINT('Ctrl Pts',(18.0881275465301,14.3898412589926,-6.84275405931048));
#114004=CARTESIAN_POINT('Ctrl Pts',(18.0855822406273,14.3912753162859,-6.88817613537974));
#114005=CARTESIAN_POINT('Ctrl Pts',(18.0830369347245,14.3919829512416,-6.93360654870618));
#114006=CARTESIAN_POINT('Ctrl Pts',(18.0757781803886,14.3940009987767,-7.06316591104304));
#114007=CARTESIAN_POINT('Ctrl Pts',(18.0685194260528,14.3901080601192,-7.19283957595163));
#114008=CARTESIAN_POINT('Ctrl Pts',(18.0612606717169,14.3803155764213,-7.32208063470887));
#114009=CARTESIAN_POINT('Ctrl Pts',(18.0540033125099,14.3705249748337,-7.45129685340011));
#114010=CARTESIAN_POINT('Ctrl Pts',(18.0467459533029,14.3548371161971,-7.58008028877821));
#114011=CARTESIAN_POINT('Ctrl Pts',(18.0394885940959,14.3333154303526,-7.70788758113798));
#114012=CARTESIAN_POINT('Ctrl Pts',(18.0322310294306,14.3117931352219,-7.83569849176514));
#114013=CARTESIAN_POINT('Ctrl Pts',(18.0249734647654,14.2844367364672,-7.96253286415625));
#114014=CARTESIAN_POINT('Ctrl Pts',(18.0177159001001,14.2513611175704,-8.08785565561839));
#114015=CARTESIAN_POINT('Ctrl Pts',(18.0104587108012,14.2182872093681,-8.21317196529727));
#114016=CARTESIAN_POINT('Ctrl Pts',(18.0032015215023,14.1794947619858,-8.33697651802529));
#114017=CARTESIAN_POINT('Ctrl Pts',(17.9959443322034,14.1351490069288,-8.45874776205162));
#114018=CARTESIAN_POINT('Ctrl Pts',(17.9886857467642,14.0907947206216,-8.58054243246768));
#114019=CARTESIAN_POINT('Ctrl Pts',(17.981427161325,14.0408851109871,-8.7003026895735));
#114020=CARTESIAN_POINT('Ctrl Pts',(17.9741685758858,13.9856343135614,-8.817525008294));
#114021=CARTESIAN_POINT('Ctrl Pts',(17.971676147196,13.9666624803039,-8.85777641439939));
#114022=CARTESIAN_POINT('Ctrl Pts',(17.9691837185061,13.9470612951703,-8.8977287593196));
#114023=CARTESIAN_POINT('Ctrl Pts',(17.9666912898163,13.9268407111584,-8.93736225920162));
#114024=CARTESIAN_POINT('Ctrl Pts',(17.959457012044,13.868150437668,-9.05239854826719));
#114025=CARTESIAN_POINT('Ctrl Pts',(17.9522227342717,13.8042175019266,-9.16478836006122));
#114026=CARTESIAN_POINT('Ctrl Pts',(17.9449884564993,13.735305827901,-9.2740565805352));
#114027=CARTESIAN_POINT('Ctrl Pts',(17.9377556208397,13.6664078910309,-9.38330301900235));
#114028=CARTESIAN_POINT('Ctrl Pts',(17.9305227851801,13.5925333815593,-9.48942881237161));
#114029=CARTESIAN_POINT('Ctrl Pts',(17.9232899495204,13.5139905279122,-9.5919862782184));
#114030=CARTESIAN_POINT('Ctrl Pts',(17.9160567323261,13.435443531101,-9.69454915400889));
#114031=CARTESIAN_POINT('Ctrl Pts',(17.9088235151317,13.3522279072543,-9.79354304685971));
#114032=CARTESIAN_POINT('Ctrl Pts',(17.9015902979374,13.2646934763842,-9.88855168997165));
#114033=CARTESIAN_POINT('Ctrl Pts',(17.8943572886278,13.1771615612799,-9.98355760250672));
#114034=CARTESIAN_POINT('Ctrl Pts',(17.8871242793183,13.0853113257864,-10.0745782395425));
#114035=CARTESIAN_POINT('Ctrl Pts',(17.8798912700088,12.9895307352709,-10.1612328597093));
#114036=CARTESIAN_POINT('Ctrl Pts',(17.8726564173338,12.8937257346344,-10.2479095642018));
#114037=CARTESIAN_POINT('Ctrl Pts',(17.8654215646588,12.7939886377373,-10.3302177959126));
#114038=CARTESIAN_POINT('Ctrl Pts',(17.8581867119838,12.6907421457889,-10.4078156743924));
#114039=CARTESIAN_POINT('Ctrl Pts',(17.8555730229586,12.6534429449591,-10.4358489644226));
#114040=CARTESIAN_POINT('Ctrl Pts',(17.8529593339334,12.6156860341656,-10.4632678865055));
#114041=CARTESIAN_POINT('Ctrl Pts',(17.8503456449081,12.5774923427427,-10.4900576628293));
#114042=CARTESIAN_POINT('Ctrl Pts',(17.843054929369,12.4709535246718,-10.5647860014525));
#114043=CARTESIAN_POINT('Ctrl Pts',(17.83576421383,12.3609735972743,-10.6346442279424));
#114044=CARTESIAN_POINT('Ctrl Pts',(17.8284734982909,12.2480155917303,-10.6993324651342));
#114045=CARTESIAN_POINT('Ctrl Pts',(17.8211843011505,12.1350811113517,-10.7640072300494));
#114046=CARTESIAN_POINT('Ctrl Pts',(17.8138951040101,12.0191700832606,-10.8235139860041));
#114047=CARTESIAN_POINT('Ctrl Pts',(17.8066059068697,11.9007717818896,-10.8775978742878));
#114048=CARTESIAN_POINT('Ctrl Pts',(17.7993170289403,11.7823786654573,-10.9316793941115));
#114049=CARTESIAN_POINT('Ctrl Pts',(17.7920281510109,11.661498799066,-10.9803383769681));
#114050=CARTESIAN_POINT('Ctrl Pts',(17.7847392730815,11.5386434575797,-11.0233672111753));
#114051=CARTESIAN_POINT('Ctrl Pts',(17.7774511732815,11.4158012316036,-11.0663914518083));
#114052=CARTESIAN_POINT('Ctrl Pts',(17.7701630734815,11.2909842708733,-11.1037866334837));
#114053=CARTESIAN_POINT('Ctrl Pts',(17.7628749736815,11.1647210635762,-11.1353943402689));
#114054=CARTESIAN_POINT('Ctrl Pts',(17.755586336441,11.0384485453526,-11.167004377876));
#114055=CARTESIAN_POINT('Ctrl Pts',(17.7482976992005,10.910729895161,-11.1928260056546));
#114056=CARTESIAN_POINT('Ctrl Pts',(17.74100906196,10.7821062475066,-11.2127513676593));
#114057=CARTESIAN_POINT('Ctrl Pts',(17.7386727079734,10.740876266913,-11.2191383913813));
#114058=CARTESIAN_POINT('Ctrl Pts',(17.7363363539867,10.6995533730216,-11.2249199633334));
#114059=CARTESIAN_POINT('Ctrl Pts',(17.734,10.6581555755053,-11.2300936493755));
#114060=CARTESIAN_POINT('Origin',(17.734,10.1295,-7.));
#114061=CARTESIAN_POINT('Origin',(-18.734,-18.952,1.76670989022851));
#114062=CARTESIAN_POINT('',(-21.2964370736898,-18.9538544369521,-1.0332901097715));
#114063=CARTESIAN_POINT('Ctrl Pts',(-17.1722616763361,-16.9190322283098,
-0.516748667021866));
#114064=CARTESIAN_POINT('Ctrl Pts',(-16.5519397059328,-17.4014734539573,
-0.555987270520924));
#114065=CARTESIAN_POINT('Ctrl Pts',(-15.7420434198304,-19.0426368321606,
-0.637617809580458));
#114066=CARTESIAN_POINT('Ctrl Pts',(-17.1190396890662,-21.5123500683105,
-0.76164028420047));
#114067=CARTESIAN_POINT('Ctrl Pts',(-20.0126665309401,-21.6957542121544,
-0.888816090881905));
#114068=CARTESIAN_POINT('Ctrl Pts',(-21.2376962809792,-20.0341121664399,
-0.979366032738912));
#114069=CARTESIAN_POINT('Ctrl Pts',(-21.2973788721029,-19.0694704700222,
-1.02752403903544));
#114070=CARTESIAN_POINT('Ctrl Pts',(-21.2964370736898,-18.9538544369521,
-1.0332901097715));
#114071=CARTESIAN_POINT('Ctrl Pts',(-21.2964370736898,-18.9538544369521,
-1.0332901097715));
#114072=CARTESIAN_POINT('Ctrl Pts',(-21.2904548055299,-18.219465735772,
-1.06991597459592));
#114073=CARTESIAN_POINT('Ctrl Pts',(-20.5735369171316,-16.6248681111266,
-1.14893377498083));
#114074=CARTESIAN_POINT('Ctrl Pts',(-18.4657781175424,-16.1791426091993,
-1.24342933697954));
#114075=CARTESIAN_POINT('Ctrl Pts',(-17.4224626768032,-16.7324608551944,
-1.30129903415381));
#114076=CARTESIAN_POINT('Ctrl Pts',(-17.1763037562512,-16.9242236971175,
-1.31677679576762));
#114077=CARTESIAN_POINT('',(-21.2938947462506,-18.950658323174,-0.966709917955182));
#114078=CARTESIAN_POINT('Ctrl Pts',(-21.2939996483808,-18.9506582509922,
-0.966709918807928));
#114079=CARTESIAN_POINT('Ctrl Pts',(-21.2939507847444,-18.8574285254183,
-0.971325634427595));
#114080=CARTESIAN_POINT('Ctrl Pts',(-21.2888049399727,-18.7643768813754,
-0.975941350047264));
#114081=CARTESIAN_POINT('Ctrl Pts',(-21.2786450004472,-18.6720324631339,
-0.980557065666932));
#114082=CARTESIAN_POINT('Ctrl Pts',(-21.2684492555577,-18.5793626073736,
-0.98518904785764));
#114083=CARTESIAN_POINT('Ctrl Pts',(-21.2532041411694,-18.4874052362913,
-0.989821030048348));
#114084=CARTESIAN_POINT('Ctrl Pts',(-21.2330434185021,-18.3966784783199,
-0.994453012239056));
#114085=CARTESIAN_POINT('Ctrl Pts',(-21.2127838652416,-18.3055069654919,
-0.999107701033865));
#114086=CARTESIAN_POINT('Ctrl Pts',(-21.1875605220101,-18.2155784195034,
-1.00376238982867));
#114087=CARTESIAN_POINT('Ctrl Pts',(-21.1575575881288,-18.1273979038206,
-1.00841707862348));
#114088=CARTESIAN_POINT('Ctrl Pts',(-21.1382431842027,-18.0706316520587,
-1.01141353689948));
#114089=CARTESIAN_POINT('Ctrl Pts',(-21.1169490236919,-18.0145893782908,
-1.01440999517548));
#114090=CARTESIAN_POINT('Ctrl Pts',(-21.0937343882856,-17.9594005758905,
-1.01740645345148));
#114091=CARTESIAN_POINT('Ctrl Pts',(-21.0613129620801,-17.8823242120765,
-1.02159128983477));
#114092=CARTESIAN_POINT('Ctrl Pts',(-21.0250509387666,-17.8066946664276,
-1.02577612621805));
#114093=CARTESIAN_POINT('Ctrl Pts',(-20.9850989461096,-17.7329210301116,
-1.02996096260134));
#114094=CARTESIAN_POINT('Ctrl Pts',(-20.9452038038474,-17.6592523712966,
-1.03413984409765));
#114095=CARTESIAN_POINT('Ctrl Pts',(-20.9016293390032,-17.5874347771646,
-1.03831872559397));
#114096=CARTESIAN_POINT('Ctrl Pts',(-20.8545742066751,-17.5178573871528,
-1.04249760709029));
#114097=CARTESIAN_POINT('Ctrl Pts',(-20.8066785470568,-17.447037163635,
-1.0467511343004));
#114098=CARTESIAN_POINT('Ctrl Pts',(-20.7551768351364,-17.378538408205,
-1.05100466151051));
#114099=CARTESIAN_POINT('Ctrl Pts',(-20.700327539557,-17.3127452891086,
-1.05525818872062));
#114100=CARTESIAN_POINT('Ctrl Pts',(-20.6465383152431,-17.2482237523413,
-1.05942950809333));
#114101=CARTESIAN_POINT('Ctrl Pts',(-20.5895300617654,-17.1863045680918,
-1.06360082746604));
#114102=CARTESIAN_POINT('Ctrl Pts',(-20.5295891698328,-17.1273193339164,
-1.06777214683875));
#114103=CARTESIAN_POINT('Ctrl Pts',(-20.4696683865407,-17.0683538877827,
-1.0719420668402));
#114104=CARTESIAN_POINT('Ctrl Pts',(-20.4068172462802,-17.0123207593135,
-1.07611198684164));
#114105=CARTESIAN_POINT('Ctrl Pts',(-20.3413596900249,-16.9595154136398,
-1.08028190684309));
#114106=CARTESIAN_POINT('Ctrl Pts',(-20.2759044627329,-16.9067119467669,
-1.08445167847984));
#114107=CARTESIAN_POINT('Ctrl Pts',(-20.2078433623746,-16.8571363224976,
-1.08862145011659));
#114108=CARTESIAN_POINT('Ctrl Pts',(-20.1375330967625,-16.8110434739836,
-1.09279122175334));
#114109=CARTESIAN_POINT('Ctrl Pts',(-20.0647584945777,-16.763335096196,
-1.0971071416183));
#114110=CARTESIAN_POINT('Ctrl Pts',(-19.9895745735351,-16.719358459641,
-1.10142306148326));
#114111=CARTESIAN_POINT('Ctrl Pts',(-19.912407443714,-16.6793460675678,
-1.10573898134823));
#114112=CARTESIAN_POINT('Ctrl Pts',(-19.8377461836544,-16.6406330090789,
-1.10991474914186));
#114113=CARTESIAN_POINT('Ctrl Pts',(-19.7612289942278,-16.6056308240551,
-1.1140905169355));
#114114=CARTESIAN_POINT('Ctrl Pts',(-19.6832631274215,-16.5745014164215,
-1.11826628472913));
#114115=CARTESIAN_POINT('Ctrl Pts',(-19.6013720862764,-16.5418048056381,
-1.12265228062976));
#114116=CARTESIAN_POINT('Ctrl Pts',(-19.5178832247938,-16.513381343314,
-1.12703827653039));
#114117=CARTESIAN_POINT('Ctrl Pts',(-19.4332853705762,-16.4893591470744,
-1.13142427243102));
#114118=CARTESIAN_POINT('Ctrl Pts',(-19.3486875163586,-16.4653369508349,
-1.13581026833165));
#114119=CARTESIAN_POINT('Ctrl Pts',(-19.262981251447,-16.4457160760172,
-1.14019626423228));
#114120=CARTESIAN_POINT('Ctrl Pts',(-19.1766642016327,-16.4305622346382,
-1.14458226013291));
#114121=CARTESIAN_POINT('Ctrl Pts',(-19.090189137421,-16.4153806522147,
-1.14897628515989));
#114122=CARTESIAN_POINT('Ctrl Pts',(-19.0027632421913,-16.4046231875652,
-1.15337031018687));
#114123=CARTESIAN_POINT('Ctrl Pts',(-18.9148794933972,-16.3983981107329,
-1.15776433521386));
#114124=CARTESIAN_POINT('Ctrl Pts',(-18.8313212938358,-16.3924794258865,
-1.161942090773));
#114125=CARTESIAN_POINT('Ctrl Pts',(-18.7473497761972,-16.3906576251858,
-1.16611984633214));
#114126=CARTESIAN_POINT('Ctrl Pts',(-18.6633997116546,-16.3929737009391,
-1.17029760189128));
#114127=CARTESIAN_POINT('Ctrl Pts',(-18.579531146622,-16.3952875282243,
-1.17447130164614));
#114128=CARTESIAN_POINT('Ctrl Pts',(-18.4956844505271,-16.4017312432599,
-1.178645001401));
#114129=CARTESIAN_POINT('Ctrl Pts',(-18.4122970204125,-16.4122938766612,
-1.18281870115586));
#114130=CARTESIAN_POINT('Ctrl Pts',(-18.3289655293808,-16.4228494242941,
-1.18698960105303));
#114131=CARTESIAN_POINT('Ctrl Pts',(-18.2460931473904,-16.4375183441828,
-1.19116050095021));
#114132=CARTESIAN_POINT('Ctrl Pts',(-18.1641134026781,-16.4562377384469,
-1.19533140084739));
#114133=CARTESIAN_POINT('Ctrl Pts',(-18.0821640628827,-16.4749501900005,
-1.19950075382751));
#114134=CARTESIAN_POINT('Ctrl Pts',(-18.0011071501552,-16.4977100272984,
-1.20367010680763));
#114135=CARTESIAN_POINT('Ctrl Pts',(-17.9213658855002,-16.5244032880334,
-1.20783945978775));
#114136=CARTESIAN_POINT('Ctrl Pts',(-17.8416024611271,-16.5511039666986,
-1.21200997141123));
#114137=CARTESIAN_POINT('Ctrl Pts',(-17.7631558535378,-16.5817401119467,
-1.21618048303471));
#114138=CARTESIAN_POINT('Ctrl Pts',(-17.686433123936,-16.6161481981569,
-1.22035099465819));
#114139=CARTESIAN_POINT('Ctrl Pts',(-17.6096979315643,-16.6505618735851,
-1.22452218373576));
#114140=CARTESIAN_POINT('Ctrl Pts',(-17.5346875892803,-16.6887485101164,
-1.22869337281333));
#114141=CARTESIAN_POINT('Ctrl Pts',(-17.4617864601774,-16.7304976459405,
-1.2328645618909));
#114142=CARTESIAN_POINT('Ctrl Pts',(-17.3888184724273,-16.7722850704821,
-1.23703957642442));
#114143=CARTESIAN_POINT('Ctrl Pts',(-17.317963950821,-16.8176412746798,
-1.24121459095794));
#114144=CARTESIAN_POINT('Ctrl Pts',(-17.2495794043259,-16.866311745457,
-1.24538960549146));
#114145=CARTESIAN_POINT('Ctrl Pts',(-17.2241952839492,-16.8843780652956,
-1.24693935725447));
#114146=CARTESIAN_POINT('Ctrl Pts',(-17.1991511792523,-16.902900638027,
-1.24848910901749));
#114147=CARTESIAN_POINT('Ctrl Pts',(-17.1744641548914,-16.9218650419685,
-1.2500388607805));
#114148=CARTESIAN_POINT('Ctrl Pts',(-17.1769962711794,-16.9251779373085,
-0.450077505597091));
#114149=CARTESIAN_POINT('Ctrl Pts',(-16.8637710635621,-17.1646622668181,
-0.469619412639974));
#114150=CARTESIAN_POINT('Ctrl Pts',(-16.0386998885363,-18.1402336475912,
-0.531553255243333));
#114151=CARTESIAN_POINT('Ctrl Pts',(-16.1425599588014,-20.5170161467511,
-0.63587903340717));
#114152=CARTESIAN_POINT('Ctrl Pts',(-18.6471935254001,-21.9777207549249,
-0.763054840088606));
#114153=CARTESIAN_POINT('Ctrl Pts',(-20.8878308446456,-20.8376582577765,
-0.873331792362382));
#114154=CARTESIAN_POINT('Ctrl Pts',(-21.2880301148004,-19.4648724899129,
-0.941216809075682));
#114155=CARTESIAN_POINT('Ctrl Pts',(-21.2904838985449,-18.9506606701336,
-0.966709890228504));
#114156=CARTESIAN_POINT('Origin',(18.734,-18.952,1.76670989022851));
#114157=CARTESIAN_POINT('',(16.1715629797346,-18.9538544393498,-1.0332901097715));
#114158=CARTESIAN_POINT('Ctrl Pts',(20.2957383198016,-16.919032322281,-0.51674866945634));
#114159=CARTESIAN_POINT('Ctrl Pts',(20.9160602511037,-17.401473545096,-0.555987272143906));
#114160=CARTESIAN_POINT('Ctrl Pts',(21.7259565235638,-19.0426368089358,
-0.637617810391948));
#114161=CARTESIAN_POINT('Ctrl Pts',(20.3489602682313,-21.5123500369818,
-0.761640284200471));
#114162=CARTESIAN_POINT('Ctrl Pts',(17.4553335005934,-21.6957541409811,
-0.888816090881904));
#114163=CARTESIAN_POINT('Ctrl Pts',(16.230303771566,-20.0341121451265,-0.979366032738913));
#114164=CARTESIAN_POINT('Ctrl Pts',(16.1706211813573,-19.0694704699527,
-1.02752403903544));
#114165=CARTESIAN_POINT('Ctrl Pts',(16.1715629797346,-18.9538544393498,
-1.0332901097715));
#114166=CARTESIAN_POINT('Ctrl Pts',(16.1715629797346,-18.9538544393498,
-1.0332901097715));
#114167=CARTESIAN_POINT('Ctrl Pts',(16.1775452476667,-18.2194657538418,
-1.06991597459592));
#114168=CARTESIAN_POINT('Ctrl Pts',(16.8944631229174,-16.6248681563667,
-1.14893377498083));
#114169=CARTESIAN_POINT('Ctrl Pts',(19.0022218964003,-16.1791426646111,
-1.24342933787015));
#114170=CARTESIAN_POINT('Ctrl Pts',(20.0455373273649,-16.7324609199408,
-1.30129903593505));
#114171=CARTESIAN_POINT('Ctrl Pts',(20.2916962531305,-16.9242237737287,
-1.31677679843947));
#114172=CARTESIAN_POINT('',(16.174105230784,-18.9506583124956,-0.966709917954191));
#114173=CARTESIAN_POINT('Ctrl Pts',(16.1740003516248,-18.9506582403292,
-0.96670991880675));
#114174=CARTESIAN_POINT('Ctrl Pts',(16.1740492156647,-18.8574284856305,
-0.971325636022637));
#114175=CARTESIAN_POINT('Ctrl Pts',(16.1791950640212,-18.7643768125493,
-0.975941353238524));
#114176=CARTESIAN_POINT('Ctrl Pts',(16.1893550102722,-18.6720323657042,
-0.980557070454411));
#114177=CARTESIAN_POINT('Ctrl Pts',(16.1995507619901,-18.57936248052,-0.985189054282917));
#114178=CARTESIAN_POINT('Ctrl Pts',(16.2147958864483,-18.487405080462,-0.989821038111424));
#114179=CARTESIAN_POINT('Ctrl Pts',(16.234956622384,-18.3966782943254,-0.994453021939931));
#114180=CARTESIAN_POINT('Ctrl Pts',(16.25521618901,-18.3055067530499,-0.999107712387932));
#114181=CARTESIAN_POINT('Ctrl Pts',(16.2804395488529,-18.2155781794355,
-1.00376240283593));
#114182=CARTESIAN_POINT('Ctrl Pts',(16.3104425025438,-18.1273976373283,
-1.00841709328394));
#114183=CARTESIAN_POINT('Ctrl Pts',(16.3297568808632,-18.0706314812951,
-1.01141354667312));
#114184=CARTESIAN_POINT('Ctrl Pts',(16.3510510092264,-18.0145893008769,
-1.0144100000623));
#114185=CARTESIAN_POINT('Ctrl Pts',(16.3742656062904,-17.9594005887852,
-1.01740645345148));
#114186=CARTESIAN_POINT('Ctrl Pts',(16.4066870283893,-17.8823242335553,
-1.02159128939168));
#114187=CARTESIAN_POINT('Ctrl Pts',(16.442949046845,-17.806694695872,-1.02577612533188));
#114188=CARTESIAN_POINT('Ctrl Pts',(16.4829010339938,-17.7329210668517,
-1.02996096127207));
#114189=CARTESIAN_POINT('Ctrl Pts',(16.5227961707087,-17.6592524154088,
-1.03413984232102));
#114190=CARTESIAN_POINT('Ctrl Pts',(16.5663706293486,-17.5874348279767,
-1.03831872336996));
#114191=CARTESIAN_POINT('Ctrl Pts',(16.6134257549123,-17.517857443951,-1.0424976044189));
#114192=CARTESIAN_POINT('Ctrl Pts',(16.6613214140263,-17.4470372170912,
-1.04675113174031));
#114193=CARTESIAN_POINT('Ctrl Pts',(16.7128231258243,-17.378538458199,-1.05100465906173));
#114194=CARTESIAN_POINT('Ctrl Pts',(16.767672421654,-17.312745335637,-1.05525818638315));
#114195=CARTESIAN_POINT('Ctrl Pts',(16.8214616389431,-17.2482238041918,
-1.05942950530122));
#114196=CARTESIAN_POINT('Ctrl Pts',(16.8784698848833,-17.1863046245575,
-1.06360082421929));
#114197=CARTESIAN_POINT('Ctrl Pts',(16.9384107688485,-17.1273193942576,
-1.06777214313735));
#114198=CARTESIAN_POINT('Ctrl Pts',(16.9983315441488,-17.0683539520246,
-1.07194206268243));
#114199=CARTESIAN_POINT('Ctrl Pts',(17.0611826759855,-17.0123208267143,
-1.07611198222751));
#114200=CARTESIAN_POINT('Ctrl Pts',(17.1266402234641,-16.9595154834292,
-1.08028190177259));
#114201=CARTESIAN_POINT('Ctrl Pts',(17.192095441962,-16.9067120189591,-1.08445167295186));
#114202=CARTESIAN_POINT('Ctrl Pts',(17.2601565331721,-16.8571363963205,
-1.08862144413112));
#114203=CARTESIAN_POINT('Ctrl Pts',(17.3304667893585,-16.8110435486385,
-1.09279121531039));
#114204=CARTESIAN_POINT('Ctrl Pts',(17.4032413988251,-16.7633351605427,
-1.09710713571227));
#114205=CARTESIAN_POINT('Ctrl Pts',(17.4784253279814,-16.7193585145734,
-1.10142305611414));
#114206=CARTESIAN_POINT('Ctrl Pts',(17.5555924665286,-16.6793461141085,
-1.10573897651602));
#114207=CARTESIAN_POINT('Ctrl Pts',(17.6302537175965,-16.6406330565404,
-1.10991474385404));
#114208=CARTESIAN_POINT('Ctrl Pts',(17.7067708977367,-16.6056308716597,
-1.11409051119206));
#114209=CARTESIAN_POINT('Ctrl Pts',(17.7847367550311,-16.5745014633546,
-1.11826627853008));
#114210=CARTESIAN_POINT('Ctrl Pts',(17.8666278144111,-16.5418048405963,
-1.12265227546388));
#114211=CARTESIAN_POINT('Ctrl Pts',(17.950116694982,-16.5133813683478,-1.12703827239769));
#114212=CARTESIAN_POINT('Ctrl Pts',(18.0347145687176,-16.4893591643124,
-1.13142426933149));
#114213=CARTESIAN_POINT('Ctrl Pts',(18.1193124424532,-16.465336960277,-1.1358102662653));
#114214=CARTESIAN_POINT('Ctrl Pts',(18.2050187273114,-16.445716079792,-1.1401962631991));
#114215=CARTESIAN_POINT('Ctrl Pts',(18.2913357970735,-16.4305622348653,
-1.14458226013291));
#114216=CARTESIAN_POINT('Ctrl Pts',(18.3778108630074,-16.4153806520938,
-1.14897628526701));
#114217=CARTESIAN_POINT('Ctrl Pts',(18.4652367601027,-16.4046231872553,
-1.15337031040112));
#114218=CARTESIAN_POINT('Ctrl Pts',(18.5531205108655,-16.398398110431,-1.15776433553522));
#114219=CARTESIAN_POINT('Ctrl Pts',(18.6366787085168,-16.39247942586,-1.16194209100712));
#114220=CARTESIAN_POINT('Ctrl Pts',(18.7206502243009,-16.3906576252416,
-1.16611984647902));
#114221=CARTESIAN_POINT('Ctrl Pts',(18.8046002870634,-16.3929737009037,
-1.17029760195092));
#114222=CARTESIAN_POINT('Ctrl Pts',(18.8884688502721,-16.3952875280966,
-1.17447130161636));
#114223=CARTESIAN_POINT('Ctrl Pts',(18.9723155446172,-16.4017312428622,
-1.1786450012818));
#114224=CARTESIAN_POINT('Ctrl Pts',(19.0557029730719,-16.4122938758359,
-1.18281870094723));
#114225=CARTESIAN_POINT('Ctrl Pts',(19.1390344624023,-16.422849423036,-1.18698960075292));
#114226=CARTESIAN_POINT('Ctrl Pts',(19.2219068427816,-16.4375183423304,
-1.19116050055861));
#114227=CARTESIAN_POINT('Ctrl Pts',(19.3038865859859,-16.4562377358584,
-1.1953314003643));
#114228=CARTESIAN_POINT('Ctrl Pts',(19.3858359242349,-16.4749501866673,
-1.19950075325099));
#114229=CARTESIAN_POINT('Ctrl Pts',(19.4668928355199,-16.4977100230749,
-1.20367010613769));
#114230=CARTESIAN_POINT('Ctrl Pts',(19.5466340988466,-16.5244032827935,
-1.20783945902438));
#114231=CARTESIAN_POINT('Ctrl Pts',(19.6263975218472,-16.5511039604273,
-1.21200997055212));
#114232=CARTESIAN_POINT('Ctrl Pts',(19.7048441281799,-16.5817401045136,
-1.21618048207985));
#114233=CARTESIAN_POINT('Ctrl Pts',(19.7815668566494,-16.61614818945,-1.22035099360759));
#114234=CARTESIAN_POINT('Ctrl Pts',(19.8583020478613,-16.650561863592,-1.22452218258792));
#114235=CARTESIAN_POINT('Ctrl Pts',(19.9333123891112,-16.6887484987226,
-1.22869337156825));
#114236=CARTESIAN_POINT('Ctrl Pts',(20.0062135173125,-16.7304976330493,
-1.23286456054858));
#114237=CARTESIAN_POINT('Ctrl Pts',(20.0791815041405,-16.7722850560811,
-1.23703957498366));
#114238=CARTESIAN_POINT('Ctrl Pts',(20.1500360249586,-16.8176412586702,
-1.24121458941875));
#114239=CARTESIAN_POINT('Ctrl Pts',(20.2184205708046,-16.8663117277569,
-1.24538960385383));
#114240=CARTESIAN_POINT('Ctrl Pts',(20.2438047145168,-16.8843780637479,
-1.2469393570197));
#114241=CARTESIAN_POINT('Ctrl Pts',(20.2688488419368,-16.902900653468,-1.24848911018556));
#114242=CARTESIAN_POINT('Ctrl Pts',(20.293535888361,-16.9218650751948,-1.25003886335143));
#114243=CARTESIAN_POINT('Ctrl Pts',(20.2910039261765,-16.9251777670034,
-0.450077510764929));
#114244=CARTESIAN_POINT('Ctrl Pts',(20.6042291142437,-17.1646622078131,
-0.469619416085199));
#114245=CARTESIAN_POINT('Ctrl Pts',(21.4293002690834,-18.1402340273379,
-0.531553256965945));
#114246=CARTESIAN_POINT('Ctrl Pts',(21.3254401485204,-20.5170159135665,
-0.635879033407171));
#114247=CARTESIAN_POINT('Ctrl Pts',(18.8208065113563,-21.977721108989,-0.763054840088605));
#114248=CARTESIAN_POINT('Ctrl Pts',(16.5801690201362,-20.8376582933814,
-0.873331792362383));
#114249=CARTESIAN_POINT('Ctrl Pts',(16.1799697387475,-19.4648724906692,
-0.941216809075683));
#114250=CARTESIAN_POINT('Ctrl Pts',(16.1775159588735,-18.9506606593868,
-0.966709890228505));
#114251=CARTESIAN_POINT('Origin',(18.734,19.211,1.76670989022852));
#114252=CARTESIAN_POINT('',(16.1715629762874,19.209145560805,-1.0332901097715));
#114253=CARTESIAN_POINT('Ctrl Pts',(20.2957383200499,21.2439676837843,-0.516748669299169));
#114254=CARTESIAN_POINT('Ctrl Pts',(20.9160602538759,20.7615264607868,-0.555987272039123));
#114255=CARTESIAN_POINT('Ctrl Pts',(21.725956527216,19.1203631895649,-0.637617810339557));
#114256=CARTESIAN_POINT('Ctrl Pts',(20.3489602709871,16.6506499609975,-0.76164028420047));
#114257=CARTESIAN_POINT('Ctrl Pts',(17.4553334985585,16.4672458544258,-0.888816090881905));
#114258=CARTESIAN_POINT('Ctrl Pts',(16.2303037681755,18.1288878534983,-0.979366032738912));
#114259=CARTESIAN_POINT('Ctrl Pts',(16.1706211779077,19.0935295300429,-1.02752403903544));
#114260=CARTESIAN_POINT('Ctrl Pts',(16.1715629762874,19.209145560805,-1.0332901097715));
#114261=CARTESIAN_POINT('Ctrl Pts',(16.1715629762874,19.209145560805,-1.0332901097715));
#114262=CARTESIAN_POINT('Ctrl Pts',(16.1775452442342,19.9435342473242,-1.06991597459592));
#114263=CARTESIAN_POINT('Ctrl Pts',(16.8944631203331,21.5381318465523,-1.14893377498083));
#114264=CARTESIAN_POINT('Ctrl Pts',(19.0022218955,21.9838573389643,-1.24342933781265));
#114265=CARTESIAN_POINT('Ctrl Pts',(20.0455373270949,21.4305390842377,-1.30129903582005));
#114266=CARTESIAN_POINT('Ctrl Pts',(20.2916962525238,21.2387762312158,-1.31677679826698));
#114267=CARTESIAN_POINT('',(16.1741052276289,19.2123416889722,-0.966709917954053));
#114268=CARTESIAN_POINT('Ctrl Pts',(16.1740003516256,19.2123417611365,-0.966709918806587));
#114269=CARTESIAN_POINT('Ctrl Pts',(16.174049215721,19.3055715198376,-0.971325636241826));
#114270=CARTESIAN_POINT('Ctrl Pts',(16.17919506457,19.3986231969093,-0.975941353677064));
#114271=CARTESIAN_POINT('Ctrl Pts',(16.1893550117453,19.490967647685,-0.980557071112303));
#114272=CARTESIAN_POINT('Ctrl Pts',(16.1995507644016,19.5836375369126,-0.985189055165875));
#114273=CARTESIAN_POINT('Ctrl Pts',(16.2147958902436,19.6755949409525,-0.989821039219448));
#114274=CARTESIAN_POINT('Ctrl Pts',(16.2349566280026,19.7663217309596,-0.99445302327302));
#114275=CARTESIAN_POINT('Ctrl Pts',(16.2552161964654,19.8574932761445,-0.99910771394821));
#114276=CARTESIAN_POINT('Ctrl Pts',(16.2804395585911,19.9474218535553,-1.0037624046234));
#114277=CARTESIAN_POINT('Ctrl Pts',(16.3104425150043,20.0356023992939,-1.00841709529859));
#114278=CARTESIAN_POINT('Ctrl Pts',(16.3297568898048,20.0923685421719,-1.01141354801622));
#114279=CARTESIAN_POINT('Ctrl Pts',(16.3510510137503,20.1484107097619,-1.01441000073385));
#114280=CARTESIAN_POINT('Ctrl Pts',(16.3742656055452,20.2035994094432,-1.01740645345148));
#114281=CARTESIAN_POINT('Ctrl Pts',(16.4066870270799,20.2806757634937,-1.0215912893308));
#114282=CARTESIAN_POINT('Ctrl Pts',(16.4429490448682,20.3563053000825,-1.02577612521011));
#114283=CARTESIAN_POINT('Ctrl Pts',(16.4829010312601,20.4300789281004,-1.02996096108943));
#114284=CARTESIAN_POINT('Ctrl Pts',(16.5227961672129,20.5037475785304,-1.03413984207691));
#114285=CARTESIAN_POINT('Ctrl Pts',(16.5663706250003,20.575565165042,-1.03831872306438));
#114286=CARTESIAN_POINT('Ctrl Pts',(16.6134257496346,20.6451425482453,-1.04249760405186));
#114287=CARTESIAN_POINT('Ctrl Pts',(16.6613214086794,20.7159627755642,-1.04675113138857));
#114288=CARTESIAN_POINT('Ctrl Pts',(16.7128231204605,20.7844615349321,-1.05100465872528));
#114289=CARTESIAN_POINT('Ctrl Pts',(16.7676724163246,20.8502546579702,-1.05525818606199));
#114290=CARTESIAN_POINT('Ctrl Pts',(16.8214616326485,20.9147761886841,-1.05942950491759));
#114291=CARTESIAN_POINT('Ctrl Pts',(16.878469877553,20.9766953676843,-1.06360082377319));
#114292=CARTESIAN_POINT('Ctrl Pts',(16.9384107604234,21.0356805974517,-1.06777214262878));
#114293=CARTESIAN_POINT('Ctrl Pts',(16.9983315346257,21.0946460391488,-1.07194206211116));
#114294=CARTESIAN_POINT('Ctrl Pts',(17.0611826653049,21.150679164025,-1.07611198159354));
#114295=CARTESIAN_POINT('Ctrl Pts',(17.1266402115777,21.2034845069819,-1.08028190107591));
#114296=CARTESIAN_POINT('Ctrl Pts',(17.1920954288672,21.2562879711218,-1.08445167219232));
#114297=CARTESIAN_POINT('Ctrl Pts',(17.2601565188203,21.3058635935363,-1.08862144330872));
#114298=CARTESIAN_POINT('Ctrl Pts',(17.3304667737115,21.3519564411039,-1.09279121442513));
#114299=CARTESIAN_POINT('Ctrl Pts',(17.4032413841786,21.399664830616,-1.09710713490077));
#114300=CARTESIAN_POINT('Ctrl Pts',(17.4784253144497,21.4436414778789,-1.10142305537642));
#114301=CARTESIAN_POINT('Ctrl Pts',(17.5555924541958,21.4836538794968,-1.10573897585207));
#114302=CARTESIAN_POINT('Ctrl Pts',(17.6302537040283,21.5223669369384,-1.10991474312749));
#114303=CARTESIAN_POINT('Ctrl Pts',(17.7067708828925,21.5573691217994,-1.11409051040291));
#114304=CARTESIAN_POINT('Ctrl Pts',(17.7847367388801,21.5884985301968,-1.11826627767833));
#114305=CARTESIAN_POINT('Ctrl Pts',(17.8666278007655,21.6211951546004,-1.12265227475409));
#114306=CARTESIAN_POINT('Ctrl Pts',(17.9501166839591,21.6496186282125,-1.12703827182985));
#114307=CARTESIAN_POINT('Ctrl Pts',(18.0347145603764,21.6736408333191,-1.13142426890562));
#114308=CARTESIAN_POINT('Ctrl Pts',(18.1193124367938,21.6976630384256,-1.13581026598138));
#114309=CARTESIAN_POINT('Ctrl Pts',(18.2050187243926,21.7172839196893,-1.14019626305714));
#114310=CARTESIAN_POINT('Ctrl Pts',(18.2913357968955,21.7324377651034,-1.1445822601329));
#114311=CARTESIAN_POINT('Ctrl Pts',(18.3778108626164,21.7476193478439,-1.14897628525888));
#114312=CARTESIAN_POINT('Ctrl Pts',(18.4652367595084,21.7583768126755,-1.15337031038486));
#114313=CARTESIAN_POINT('Ctrl Pts',(18.55312051008,21.7646018895134,-1.15776433551083));
#114314=CARTESIAN_POINT('Ctrl Pts',(18.6366787074649,21.7705205740913,-1.16194209097077));
#114315=CARTESIAN_POINT('Ctrl Pts',(18.7206502229926,21.7723423747436,-1.16611984643071));
#114316=CARTESIAN_POINT('Ctrl Pts',(18.8046002855114,21.7700262991391,-1.17029760189066));
#114317=CARTESIAN_POINT('Ctrl Pts',(18.8884688484699,21.7677124720041,-1.17447130154382));
#114318=CARTESIAN_POINT('Ctrl Pts',(18.9723155425776,21.7612687573207,-1.17864500119699));
#114319=CARTESIAN_POINT('Ctrl Pts',(19.0557029708096,21.7507061244507,-1.18281870085015));
#114320=CARTESIAN_POINT('Ctrl Pts',(19.1390344599114,21.7401505773549,-1.18698960064328));
#114321=CARTESIAN_POINT('Ctrl Pts',(19.2219068400769,21.7254816581869,-1.1911605004364));
#114322=CARTESIAN_POINT('Ctrl Pts',(19.3038865830838,21.7067622648043,-1.19533140022953));
#114323=CARTESIAN_POINT('Ctrl Pts',(19.3858359211298,21.688049814142,-1.19950075310337));
#114324=CARTESIAN_POINT('Ctrl Pts',(19.4668928322285,21.6652899779005,-1.20367010597722));
#114325=CARTESIAN_POINT('Ctrl Pts',(19.5466340953869,21.6385967183646,-1.20783945885106));
#114326=CARTESIAN_POINT('Ctrl Pts',(19.6263975182123,21.6118960409159,-1.21200997036559));
#114327=CARTESIAN_POINT('Ctrl Pts',(19.704844124388,21.581259897032,-1.21618048188011));
#114328=CARTESIAN_POINT('Ctrl Pts',(19.7815668527197,21.5468518123123,-1.22035099339464));
#114329=CARTESIAN_POINT('Ctrl Pts',(19.8583020437901,21.5124381383889,-1.22452218236154));
#114330=CARTESIAN_POINT('Ctrl Pts',(19.9333123849178,21.4742515034917,-1.22869337132845));
#114331=CARTESIAN_POINT('Ctrl Pts',(20.0062135130172,21.4325023694105,-1.23286456029535));
#114332=CARTESIAN_POINT('Ctrl Pts',(20.0791814997391,21.3907149466269,-1.23703957471676));
#114333=CARTESIAN_POINT('Ctrl Pts',(20.1500360204715,21.3453587442986,-1.24121458913816));
#114334=CARTESIAN_POINT('Ctrl Pts',(20.218420566253,21.2966882754825,-1.24538960355956));
#114335=CARTESIAN_POINT('Ctrl Pts',(20.2438047105659,21.2786219391475,-1.24693935675848));
#114336=CARTESIAN_POINT('Ctrl Pts',(20.2688488385727,21.2600993490623,-1.2484891099574));
#114337=CARTESIAN_POINT('Ctrl Pts',(20.2935358855687,21.2411349269503,-1.25003886315632));
#114338=CARTESIAN_POINT('Ctrl Pts',(20.2910039445873,21.2378222631174,-0.450077510930245));
#114339=CARTESIAN_POINT('Ctrl Pts',(20.6042291338676,20.9983378060478,-0.46961941619541));
#114340=CARTESIAN_POINT('Ctrl Pts',(21.4293002909665,20.0227659246052,-0.53155325702105));
#114341=CARTESIAN_POINT('Ctrl Pts',(21.3254401632976,17.6459841184673,-0.635879033407171));
#114342=CARTESIAN_POINT('Ctrl Pts',(18.8208065164127,16.1852788423107,-0.763054840088604));
#114343=CARTESIAN_POINT('Ctrl Pts',(16.5801690015235,17.3253417016998,-0.873331792362383));
#114344=CARTESIAN_POINT('Ctrl Pts',(16.1799697185864,18.6981275092202,-0.941216809075682));
#114345=CARTESIAN_POINT('Ctrl Pts',(16.1775159392447,19.2123393420905,-0.966709890228504));
#114346=CARTESIAN_POINT('Origin',(-18.734,19.211,1.76670989022852));
#114347=CARTESIAN_POINT('',(-21.2964371839251,19.2091455679848,-1.0332901097715));
#114348=CARTESIAN_POINT('Ctrl Pts',(-17.1722616682727,21.2439679654049,
-0.516748662007315));
#114349=CARTESIAN_POINT('Ctrl Pts',(-16.5519396172804,20.761526733893,-0.555987267177887));
#114350=CARTESIAN_POINT('Ctrl Pts',(-15.7420433029967,19.120363119997,-0.637617807908939));
#114351=CARTESIAN_POINT('Ctrl Pts',(-17.1190396009992,16.6506498669621,
-0.761640284200469));
#114352=CARTESIAN_POINT('Ctrl Pts',(-20.0126665959802,16.4672456410459,
-0.888816090881905));
#114353=CARTESIAN_POINT('Ctrl Pts',(-21.2376963893991,18.1288877895766,
-0.979366032738913));
#114354=CARTESIAN_POINT('Ctrl Pts',(-21.2973789824122,19.0935295298239,
-1.02752403903544));
#114355=CARTESIAN_POINT('Ctrl Pts',(-21.2964371839251,19.2091455679848,
-1.0332901097715));
#114356=CARTESIAN_POINT('Ctrl Pts',(-21.2964371839251,19.2091455679848,
-1.0332901097715));
#114357=CARTESIAN_POINT('Ctrl Pts',(-21.2904549152958,19.943534301501,-1.06991597459592));
#114358=CARTESIAN_POINT('Ctrl Pts',(-20.5735369997583,21.5381319822354,
-1.14893377498083));
#114359=CARTESIAN_POINT('Ctrl Pts',(-18.4657781462453,21.983857505142,-1.24342933514492));
#114360=CARTESIAN_POINT('Ctrl Pts',(-17.4224626852965,21.4305392783363,
-1.30129903048459));
#114361=CARTESIAN_POINT('Ctrl Pts',(-17.1763037754663,21.2387764608407,
-1.31677679026378));
#114362=CARTESIAN_POINT('',(-21.2938947647296,19.2123416854176,-0.966709917954385));
#114363=CARTESIAN_POINT('Ctrl Pts',(-21.2939996483763,19.212341757587,-0.96670991880698));
#114364=CARTESIAN_POINT('Ctrl Pts',(-21.2939507844152,19.3055715065957,
-0.971325635711016));
#114365=CARTESIAN_POINT('Ctrl Pts',(-21.2888049367591,19.3986231740038,
-0.975941352615052));
#114366=CARTESIAN_POINT('Ctrl Pts',(-21.2786449918221,19.4909676152607,
-0.980557069519088));
#114367=CARTESIAN_POINT('Ctrl Pts',(-21.2684492414382,19.5836374946964,
-0.985189053027621));
#114368=CARTESIAN_POINT('Ctrl Pts',(-21.2532041189474,19.6755948890935,
-0.989821036536154));
#114369=CARTESIAN_POINT('Ctrl Pts',(-21.233043385604,19.7663216697276,-0.994453020044687));
#114370=CARTESIAN_POINT('Ctrl Pts',(-21.2127838215892,19.8574932054453,
-0.999107710169702));
#114371=CARTESIAN_POINT('Ctrl Pts',(-21.1875604649916,19.9474217736623,
-1.00376240029472));
#114372=CARTESIAN_POINT('Ctrl Pts',(-21.1575575151709,20.035602310607,-1.00841709041973));
#114373=CARTESIAN_POINT('Ctrl Pts',(-21.1382431318488,20.0923684853426,
-1.01141354476365));
#114374=CARTESIAN_POINT('Ctrl Pts',(-21.1169489972049,20.1484106839985,
-1.01440999910756));
#114375=CARTESIAN_POINT('Ctrl Pts',(-21.09373439265,20.2035994137337,-1.01740645345148));
#114376=CARTESIAN_POINT('Ctrl Pts',(-21.0613129697488,20.2806757706407,
-1.02159128947824));
#114377=CARTESIAN_POINT('Ctrl Pts',(-21.0250509503441,20.3563053098801,
-1.02577612550499));
#114378=CARTESIAN_POINT('Ctrl Pts',(-20.9850989621192,20.4300789403257,
-1.02996096153175));
#114379=CARTESIAN_POINT('Ctrl Pts',(-20.9452038243207,20.5037475932088,
-1.03413984266809));
#114380=CARTESIAN_POINT('Ctrl Pts',(-20.9016293644687,20.5755651819498,
-1.03831872380443));
#114381=CARTESIAN_POINT('Ctrl Pts',(-20.8545742375835,20.6451425671449,
-1.04249760494077));
#114382=CARTESIAN_POINT('Ctrl Pts',(-20.806678578371,20.7159627933518,-1.04675113224044));
#114383=CARTESIAN_POINT('Ctrl Pts',(-20.7551768665491,20.7844615515677,
-1.05100465954011));
#114384=CARTESIAN_POINT('Ctrl Pts',(-20.7003275707683,20.8502546734527,
-1.05525818683978));
#114385=CARTESIAN_POINT('Ctrl Pts',(-20.6465383521068,20.9147762059375,
-1.05942950584667));
#114386=CARTESIAN_POINT('Ctrl Pts',(-20.5895301046941,20.9766953864735,
-1.06360082485355));
#114387=CARTESIAN_POINT('Ctrl Pts',(-20.5295892191724,21.0356806175306,
-1.06777214386044));
#114388=CARTESIAN_POINT('Ctrl Pts',(-20.4696684423108,21.0946460605256,
-1.07194206349468));
#114389=CARTESIAN_POINT('Ctrl Pts',(-20.4068173088285,21.150679186453,-1.07611198312891));
#114390=CARTESIAN_POINT('Ctrl Pts',(-20.3413597596352,21.2034845302048,
-1.08028190276314));
#114391=CARTESIAN_POINT('Ctrl Pts',(-20.2759045394194,21.2562879951442,
-1.08445167403178));
#114392=CARTESIAN_POINT('Ctrl Pts',(-20.2078434464222,21.3058636181013,
-1.08862144530041));
#114393=CARTESIAN_POINT('Ctrl Pts',(-20.1375331883945,21.3519564659458,
-1.09279121656905));
#114394=CARTESIAN_POINT('Ctrl Pts',(-20.0647585803504,21.3996648520279,
-1.09710713686604));
#114395=CARTESIAN_POINT('Ctrl Pts',(-19.9895746527792,21.443641496158,-1.10142305716302));
#114396=CARTESIAN_POINT('Ctrl Pts',(-19.9124075159367,21.4836538949836,
-1.10573897746001));
#114397=CARTESIAN_POINT('Ctrl Pts',(-19.8377462631121,21.5223669527316,
-1.10991474488704));
#114398=CARTESIAN_POINT('Ctrl Pts',(-19.7612290811577,21.5573691376402,
-1.11409051231407));
#114399=CARTESIAN_POINT('Ctrl Pts',(-19.6832632220051,21.5884985458142,
-1.1182662797411));
#114400=CARTESIAN_POINT('Ctrl Pts',(-19.6013721661874,21.621195166233,-1.12265227647306));
#114401=CARTESIAN_POINT('Ctrl Pts',(-19.5178832893455,21.6496186365428,
-1.12703827320503));
#114402=CARTESIAN_POINT('Ctrl Pts',(-19.4332854194228,21.6736408390552,
-1.131424269937));
#114403=CARTESIAN_POINT('Ctrl Pts',(-19.3486875495001,21.6976630415676,
-1.13581026666897));
#114404=CARTESIAN_POINT('Ctrl Pts',(-19.2629812685386,21.7172839209455,
-1.14019626340094));
#114405=CARTESIAN_POINT('Ctrl Pts',(-19.1766642026735,21.7324377651791,
-1.1445822601329));
#114406=CARTESIAN_POINT('Ctrl Pts',(-19.0901891434539,21.7476193467629,
-1.148976284922));
#114407=CARTESIAN_POINT('Ctrl Pts',(-19.0027632532416,21.7583768110981,
-1.15337030971109));
#114408=CARTESIAN_POINT('Ctrl Pts',(-18.9148795094127,21.7646018881326,
-1.15776433450019));
#114409=CARTESIAN_POINT('Ctrl Pts',(-18.831321311443,21.770520573393,-1.16194208998959));
#114410=CARTESIAN_POINT('Ctrl Pts',(-18.7473497953179,21.7723423746674,
-1.16611984547899));
#114411=CARTESIAN_POINT('Ctrl Pts',(-18.663399732195,21.7700262996276,-1.1702976009684));
#114412=CARTESIAN_POINT('Ctrl Pts',(-18.5795311686207,21.7677124730563,
-1.1744713006516));
#114413=CARTESIAN_POINT('Ctrl Pts',(-18.4956844738905,21.7612687588782,
-1.1786450003348));
#114414=CARTESIAN_POINT('Ctrl Pts',(-18.4122970450345,21.7507061264576,
-1.182818700018));
#114415=CARTESIAN_POINT('Ctrl Pts',(-18.328965555298,21.7401505798097,-1.1869895998417));
#114416=CARTESIAN_POINT('Ctrl Pts',(-18.2460931744964,21.7254816610328,
-1.19116049966539));
#114417=CARTESIAN_POINT('Ctrl Pts',(-18.1641134308566,21.7067622679875,
-1.19533139948908));
#114418=CARTESIAN_POINT('Ctrl Pts',(-18.082164092168,21.68804981766,-1.199500752394));
#114419=CARTESIAN_POINT('Ctrl Pts',(-18.0011071804304,21.6652899816987,
-1.20367010529891));
#114420=CARTESIAN_POINT('Ctrl Pts',(-17.921365916641,21.6385967223909,-1.20783945820382));
#114421=CARTESIAN_POINT('Ctrl Pts',(-17.8416024931822,21.6118960451696,
-1.21200996974954));
#114422=CARTESIAN_POINT('Ctrl Pts',(-17.7631558863812,21.581259901461,-1.21618048129526));
#114423=CARTESIAN_POINT('Ctrl Pts',(-17.6864331574362,21.546851816867,-1.22035099284098));
#114424=CARTESIAN_POINT('Ctrl Pts',(-17.6096979657455,21.5124381430661,
-1.22452218183947));
#114425=CARTESIAN_POINT('Ctrl Pts',(-17.5346876240098,21.4742515082411,
-1.22869337083796));
#114426=CARTESIAN_POINT('Ctrl Pts',(-17.4617864953189,21.4325023741844,
-1.23286455983645));
#114427=CARTESIAN_POINT('Ctrl Pts',(-17.3888185080204,21.3907149514342,
-1.23703957428859));
#114428=CARTESIAN_POINT('Ctrl Pts',(-17.3179639867267,21.3453587490929,
-1.24121458874073));
#114429=CARTESIAN_POINT('Ctrl Pts',(-17.2495794404032,21.2966882802198,
-1.24538960319287));
#114430=CARTESIAN_POINT('Ctrl Pts',(-17.2241953382174,21.2786219739895,
-1.24693935381897));
#114431=CARTESIAN_POINT('Ctrl Pts',(-17.1991512512063,21.2600994155247,
-1.24848910444507));
#114432=CARTESIAN_POINT('Ctrl Pts',(-17.1744642439897,21.2411350264762,
-1.25003885507116));
#114433=CARTESIAN_POINT('Ctrl Pts',(-17.1769962363369,21.2378222944355,
-0.450077502023298));
#114434=CARTESIAN_POINT('Ctrl Pts',(-16.8637709891942,20.998337861822,-0.469619410257445));
#114435=CARTESIAN_POINT('Ctrl Pts',(-16.0386997591895,20.0227661055849,
-0.531553254052069));
#114436=CARTESIAN_POINT('Ctrl Pts',(-16.1425598724776,17.6459840408836,
-0.635879033407169));
#114437=CARTESIAN_POINT('Ctrl Pts',(-18.6471934958306,16.1852789602342,
-0.763054840088606));
#114438=CARTESIAN_POINT('Ctrl Pts',(-20.8878309534133,17.3253417136014,
-0.873331792362382));
#114439=CARTESIAN_POINT('Ctrl Pts',(-21.2880302326024,18.6981275094852,
-0.941216809075682));
#114440=CARTESIAN_POINT('Ctrl Pts',(-21.2904840132329,19.212339338513,-0.966709890228504));
#114441=CARTESIAN_POINT('Origin',(26.8463464956315,10.1295,-7.));
#114442=CARTESIAN_POINT('',(21.5963464956316,10.1298829051514,-12.098999985623));
#114443=CARTESIAN_POINT('Ctrl Pts',(22.5651720735026,6.08350804222181,-3.89745662547247));
#114444=CARTESIAN_POINT('Ctrl Pts',(22.5448385294137,6.3478784765494,-3.55278409554048));
#114445=CARTESIAN_POINT('Ctrl Pts',(22.4857231036888,7.24322563422365,-2.64786715344243));
#114446=CARTESIAN_POINT('Ctrl Pts',(22.3878257963277,9.21233876997001,-1.77459149097018));
#114447=CARTESIAN_POINT('Ctrl Pts',(22.2714801514196,11.7661169025298,-1.95345839105347));
#114448=CARTESIAN_POINT('Ctrl Pts',(22.1551345065114,13.9387381504676,-3.30737374765752));
#114449=CARTESIAN_POINT('Ctrl Pts',(22.0387888616032,15.2245708351663,-5.52111016209781));
#114450=CARTESIAN_POINT('Ctrl Pts',(21.922443216695,15.3236941270903,-8.07916377113051));
#114451=CARTESIAN_POINT('Ctrl Pts',(21.8060975717868,14.2141213326594,-10.3860101586105));
#114452=CARTESIAN_POINT('Ctrl Pts',(21.6973986661381,12.2874582761103,-11.804511236185));
#114453=CARTESIAN_POINT('Ctrl Pts',(21.6274816421253,10.7948600303933,-12.0984964626806));
#114454=CARTESIAN_POINT('Ctrl Pts',(21.5963464997487,10.1298830029783,-12.0991317633798));
#114455=CARTESIAN_POINT('Ctrl Pts',(21.5963464956316,10.1298829051514,-12.098999985623));
#114456=CARTESIAN_POINT('Ctrl Pts',(21.5886997577445,9.96656989073889,-12.0990122494776));
#114457=CARTESIAN_POINT('Ctrl Pts',(21.5810530198574,9.80325714346398,-12.0911738586918));
#114458=CARTESIAN_POINT('Ctrl Pts',(21.5734062819704,9.64065518488774,-12.0755129540508));
#114459=CARTESIAN_POINT('Ctrl Pts',(21.5666845761133,9.49772331596717,-12.0617465616352));
#114460=CARTESIAN_POINT('Ctrl Pts',(21.5599628702561,9.35531775886811,-12.0419328173513));
#114461=CARTESIAN_POINT('Ctrl Pts',(21.553241164399,9.21397363696974,-12.0161352133487));
#114462=CARTESIAN_POINT('Ctrl Pts',(21.5465211079346,9.07266419852288,-11.9903439396408));
#114463=CARTESIAN_POINT('Ctrl Pts',(21.5398010514701,8.93241603785332,-11.9585717981774));
#114464=CARTESIAN_POINT('Ctrl Pts',(21.5330809950056,8.79375579412643,-11.9209336935662));
#114465=CARTESIAN_POINT('Ctrl Pts',(21.5263596207543,8.65506835945939,-11.8832882082133));
#114466=CARTESIAN_POINT('Ctrl Pts',(21.5196382465029,8.51796982061406,-11.8397745520151));
#114467=CARTESIAN_POINT('Ctrl Pts',(21.5129168722516,8.38297363001403,-11.790558071764));
#114468=CARTESIAN_POINT('Ctrl Pts',(21.5061950124626,8.24796768757988,-11.7413380362204));
#114469=CARTESIAN_POINT('Ctrl Pts',(21.4994731526736,8.11506473991455,-11.6864144868448));
#114470=CARTESIAN_POINT('Ctrl Pts',(21.4927512928847,7.9847596072539,-11.6260014751104));
#114471=CARTESIAN_POINT('Ctrl Pts',(21.4860249738077,7.85436803004691,-11.5655483853277));
#114472=CARTESIAN_POINT('Ctrl Pts',(21.4792986547307,7.72657804372845,-11.4995987153755));
#114473=CARTESIAN_POINT('Ctrl Pts',(21.4725723356537,7.60186164562879,-11.4284134122179));
#114474=CARTESIAN_POINT('Ctrl Pts',(21.4674017694565,7.50599132118198,-11.3736927963763));
#114475=CARTESIAN_POINT('Ctrl Pts',(21.4622312032594,7.41193676657903,-11.3158793604137));
#114476=CARTESIAN_POINT('Ctrl Pts',(21.4570606370622,7.31990104245665,-11.2551092462793));
#114477=CARTESIAN_POINT('Ctrl Pts',(21.4497821926166,7.19034522990356,-11.1695650557955));
#114478=CARTESIAN_POINT('Ctrl Pts',(21.4425037481711,7.06471083663906,-11.0781083746355));
#114479=CARTESIAN_POINT('Ctrl Pts',(21.4352253037255,6.94350501939066,-10.9811100190188));
#114480=CARTESIAN_POINT('Ctrl Pts',(21.4279477400291,6.82231386900175,-10.8841234009679));
#114481=CARTESIAN_POINT('Ctrl Pts',(21.4206701763327,6.70555042157178,-10.7815966068709));
#114482=CARTESIAN_POINT('Ctrl Pts',(21.4133926126363,6.59368928068819,-10.6739411477594));
#114483=CARTESIAN_POINT('Ctrl Pts',(21.4061193938006,6.48189492329082,-10.5663499612524));
#114484=CARTESIAN_POINT('Ctrl Pts',(21.3988461749649,6.374997207616,-10.4536364025609));
#114485=CARTESIAN_POINT('Ctrl Pts',(21.3915729561292,6.27343466828419,-10.3362495646368));
#114486=CARTESIAN_POINT('Ctrl Pts',(21.3843045826288,6.17193978875607,-10.2189409284834));
#114487=CARTESIAN_POINT('Ctrl Pts',(21.3770362091284,6.07577315665127,-10.0969654188858));
#114488=CARTESIAN_POINT('Ctrl Pts',(21.369767835628,5.98533451912964,-9.97080687140086));
#114489=CARTESIAN_POINT('Ctrl Pts',(21.362508451111,5.89500772938303,-9.84480434741678));
#114490=CARTESIAN_POINT('Ctrl Pts',(21.3552490665939,5.81039493847136,-9.71462931976104));
#114491=CARTESIAN_POINT('Ctrl Pts',(21.3479896820768,5.73185403598033,-9.58079657763674));
#114492=CARTESIAN_POINT('Ctrl Pts',(21.3455647854359,5.70561853761555,-9.53609160766829));
#114493=CARTESIAN_POINT('Ctrl Pts',(21.3431398887949,5.68006019676905,-9.49097876732916));
#114494=CARTESIAN_POINT('Ctrl Pts',(21.340714992154,5.65519129922816,-9.44547800035033));
#114495=CARTESIAN_POINT('Ctrl Pts',(21.3339842151457,5.58616278850139,-9.31918168277893));
#114496=CARTESIAN_POINT('Ctrl Pts',(21.3272534381374,5.5224727999895,-9.18993727191009));
#114497=CARTESIAN_POINT('Ctrl Pts',(21.320522661129,5.46436371111823,-9.05822846306196));
#114498=CARTESIAN_POINT('Ctrl Pts',(21.3137921028903,5.40625651095962,-8.92652393512925));
#114499=CARTESIAN_POINT('Ctrl Pts',(21.3070615446517,5.35372999568267,-8.79235550376611));
#114500=CARTESIAN_POINT('Ctrl Pts',(21.300330986413,5.30697886832862,-8.65622792350057));
#114501=CARTESIAN_POINT('Ctrl Pts',(21.2935969859559,5.26020383098296,-8.52003072332451));
#114502=CARTESIAN_POINT('Ctrl Pts',(21.2868629854988,5.21921020433081,-8.38187271779159));
#114503=CARTESIAN_POINT('Ctrl Pts',(21.2801289850417,5.18414331691865,-8.24227544333075));
#114504=CARTESIAN_POINT('Ctrl Pts',(21.2733933187736,5.14906775489954,-8.10264363625022));
#114505=CARTESIAN_POINT('Ctrl Pts',(21.2666576525055,5.11992193614115,-7.96157220729945));
#114506=CARTESIAN_POINT('Ctrl Pts',(21.2599219862373,5.09680022375913,-7.81959377878623));
#114507=CARTESIAN_POINT('Ctrl Pts',(21.2531800695621,5.07365705542753,-7.6774836004288));
#114508=CARTESIAN_POINT('Ctrl Pts',(21.2464381528869,5.05654921504795,-7.53446510332613));
#114509=CARTESIAN_POINT('Ctrl Pts',(21.2396962362116,5.04551934956637,-7.39107767261309));
#114510=CARTESIAN_POINT('Ctrl Pts',(21.234587273223,5.03716101806669,-7.28241998492061));
#114511=CARTESIAN_POINT('Ctrl Pts',(21.2294783102344,5.03229187939357,-7.1735505847344));
#114512=CARTESIAN_POINT('Ctrl Pts',(21.2243693472458,5.03091055206464,-7.06470426108234));
#114513=CARTESIAN_POINT('Ctrl Pts',(21.2176540847332,5.02909492418669,-6.92163576783203));
#114514=CARTESIAN_POINT('Ctrl Pts',(21.2109388222206,5.03330382692002,-6.77836163457666));
#114515=CARTESIAN_POINT('Ctrl Pts',(21.204223559708,5.04355066274045,-6.63541758294017));
#114516=CARTESIAN_POINT('Ctrl Pts',(21.1975132922854,5.05378987654069,-6.4925798590002));
#114517=CARTESIAN_POINT('Ctrl Pts',(21.1908030248627,5.07005805418267,-6.35007209501922));
#114518=CARTESIAN_POINT('Ctrl Pts',(21.1840927574401,5.0923165571577,-6.20842943261171));
#114519=CARTESIAN_POINT('Ctrl Pts',(21.1773862402139,5.11456262042581,-6.06686593065854));
#114520=CARTESIAN_POINT('Ctrl Pts',(21.1706797229878,5.14279228431588,-5.92616693170634));
#114521=CARTESIAN_POINT('Ctrl Pts',(21.1639732057617,5.1769151576724,-5.78686176404052));
#114522=CARTESIAN_POINT('Ctrl Pts',(21.1572691966892,5.21102526950076,-5.64760869476631));
#114523=CARTESIAN_POINT('Ctrl Pts',(21.1505651876166,5.25102411227424,-5.50974877692657));
#114524=CARTESIAN_POINT('Ctrl Pts',(21.1438611785441,5.29677036811347,-5.3738003489467));
#114525=CARTESIAN_POINT('Ctrl Pts',(21.137157010186,5.34251771087248,-5.23784869086563));
#114526=CARTESIAN_POINT('Ctrl Pts',(21.1304528418279,5.39401263052893,-5.10380896672768));
#114527=CARTESIAN_POINT('Ctrl Pts',(21.1237486734698,5.45106410989234,-4.97218377998582));
#114528=CARTESIAN_POINT('Ctrl Pts',(21.1170447259729,5.50811370975889,-4.84056292948781));
#114529=CARTESIAN_POINT('Ctrl Pts',(21.1103407784761,5.57071935366059,-4.7113567955426));
#114530=CARTESIAN_POINT('Ctrl Pts',(21.1036368309793,5.63864230175156,-4.58504697062599));
#114531=CARTESIAN_POINT('Ctrl Pts',(21.0969291756063,5.7066028172431,-4.45866728519946));
#114532=CARTESIAN_POINT('Ctrl Pts',(21.0902215202333,5.77988633723191,-4.33518743528798));
#114533=CARTESIAN_POINT('Ctrl Pts',(21.0835138648603,5.85820842230719,-4.21506386817751));
#114534=CARTESIAN_POINT('Ctrl Pts',(21.0774380885725,5.92915235738501,-4.10625626252948));
#114535=CARTESIAN_POINT('Ctrl Pts',(21.0713623122848,6.00422960092619,-4.00020221885507));
#114536=CARTESIAN_POINT('Ctrl Pts',(21.065286535997,6.08319878352127,-3.89721939777838));
#114537=CARTESIAN_POINT('',(21.7216535043236,10.1294562983577,-12.0989999998127));
#114538=CARTESIAN_POINT('Ctrl Pts',(21.7216535043236,10.1294562983577,-12.0989999998127));
#114539=CARTESIAN_POINT('Ctrl Pts',(21.7145780823896,9.97829741836422,-12.0989987042859));
#114540=CARTESIAN_POINT('Ctrl Pts',(21.7075026604556,9.8271603213621,-12.092271455827));
#114541=CARTESIAN_POINT('Ctrl Pts',(21.7004272385216,9.67663880551781,-12.0788500409573));
#114542=CARTESIAN_POINT('Ctrl Pts',(21.6933497400828,9.52607311440785,-12.065424687152));
#114543=CARTESIAN_POINT('Ctrl Pts',(21.686272241644,9.37612366434497,-12.0453012699465));
#114544=CARTESIAN_POINT('Ctrl Pts',(21.6791947432053,9.22737926268248,-12.0185634573353));
#114545=CARTESIAN_POINT('Ctrl Pts',(21.6769530559598,9.18026679336472,-12.0100946722101));
#114546=CARTESIAN_POINT('Ctrl Pts',(21.6747113687143,9.13327515566229,-12.0009627140914));
#114547=CARTESIAN_POINT('Ctrl Pts',(21.6724696814689,9.08642286948864,-11.9911713154133));
#114548=CARTESIAN_POINT('Ctrl Pts',(21.6655384929631,8.94155786744673,-11.960896784428));
#114549=CARTESIAN_POINT('Ctrl Pts',(21.6586073044574,8.79798658804774,-11.9243058365266));
#114550=CARTESIAN_POINT('Ctrl Pts',(21.6516761159517,8.65626323121066,-11.8815340235511));
#114551=CARTESIAN_POINT('Ctrl Pts',(21.64474624141,8.51456674125142,-11.8387703189433));
#114552=CARTESIAN_POINT('Ctrl Pts',(21.6378163668684,8.37471779167141,-11.7898281825944));
#114553=CARTESIAN_POINT('Ctrl Pts',(21.6308864923267,8.2372559332038,-11.7348931763742));
#114554=CARTESIAN_POINT('Ctrl Pts',(21.6239563464653,8.09978869280394,-11.6799560193284));
#114555=CARTESIAN_POINT('Ctrl Pts',(21.6170262006039,7.9647090391401,-11.6190256426999));
#114556=CARTESIAN_POINT('Ctrl Pts',(21.6100960547425,7.83253754293167,-11.5523361552964));
#114557=CARTESIAN_POINT('Ctrl Pts',(21.6031662631196,7.70037280274875,-11.4856500767661));
#114558=CARTESIAN_POINT('Ctrl Pts',(21.5962364714968,7.57111621763294,-11.4132056266103));
#114559=CARTESIAN_POINT('Ctrl Pts',(21.5893066798739,7.44526470784607,-11.3352833697874));
#114560=CARTESIAN_POINT('Ctrl Pts',(21.5823752942246,7.31938424904482,-11.2573431888844));
#114561=CARTESIAN_POINT('Ctrl Pts',(21.5754439085753,7.19691071214243,-11.1739228579809));
#114562=CARTESIAN_POINT('Ctrl Pts',(21.568512522926,7.07831346210215,-11.0853471958881));
#114563=CARTESIAN_POINT('Ctrl Pts',(21.5643830274709,7.00765705517126,-11.0325766803587));
#114564=CARTESIAN_POINT('Ctrl Pts',(21.5602535320158,6.9383759408189,-10.9779771655619));
#114565=CARTESIAN_POINT('Ctrl Pts',(21.5561240365606,6.87056406102977,-10.9216243504048));
#114566=CARTESIAN_POINT('Ctrl Pts',(21.5491919803161,6.75673035668187,-10.8270266232852));
#114567=CARTESIAN_POINT('Ctrl Pts',(21.5422599240716,6.64699821171827,-10.7274524655712));
#114568=CARTESIAN_POINT('Ctrl Pts',(21.5353278678271,6.54179397638852,-10.6232811770744));
#114569=CARTESIAN_POINT('Ctrl Pts',(21.5283971552673,6.43661013346749,-10.5191300807637));
#114570=CARTESIAN_POINT('Ctrl Pts',(21.5214664427075,6.33595268411619,-10.4103838641845));
#114571=CARTESIAN_POINT('Ctrl Pts',(21.5145357301477,6.24021162379281,-10.297459162249));
#114572=CARTESIAN_POINT('Ctrl Pts',(21.5076047985457,6.14446753761436,-10.1845308913768));
#114573=CARTESIAN_POINT('Ctrl Pts',(21.5006738669437,6.05364036800616,-10.0674241210261));
#114574=CARTESIAN_POINT('Ctrl Pts',(21.4937429353417,5.96808061140313,-9.94658949842187));
#114575=CARTESIAN_POINT('Ctrl Pts',(21.4868123893406,5.88252561489794,-9.82576159842469));
#114576=CARTESIAN_POINT('Ctrl Pts',(21.4798818433394,5.80223763552051,-9.7012065317229));
#114577=CARTESIAN_POINT('Ctrl Pts',(21.4729512973382,5.72752452675666,-9.57340492984763));
#114578=CARTESIAN_POINT('Ctrl Pts',(21.4660192119694,5.65279482320388,-9.44557494151323));
#114579=CARTESIAN_POINT('Ctrl Pts',(21.4590871266005,5.58364263152974,-9.31449726290405));
#114580=CARTESIAN_POINT('Ctrl Pts',(21.4521550412316,5.5203307404732,-9.18067873310885));
#114581=CARTESIAN_POINT('Ctrl Pts',(21.4480294913719,5.48265140599206,-9.10103819387072));
#114582=CARTESIAN_POINT('Ctrl Pts',(21.4439039415122,5.44703976938654,-9.02042734711839));
#114583=CARTESIAN_POINT('Ctrl Pts',(21.4397783916525,5.41354327869334,-8.93895673050291));
#114584=CARTESIAN_POINT('Ctrl Pts',(21.4328288078177,5.35711766800913,-8.8017175988741));
#114585=CARTESIAN_POINT('Ctrl Pts',(21.425879223983,5.3066782204933,-8.66199295346232));
#114586=CARTESIAN_POINT('Ctrl Pts',(21.4189296401482,5.26242423305924,-8.52032051846249));
#114587=CARTESIAN_POINT('Ctrl Pts',(21.4119812825149,5.21817805390603,-8.37867308049059));
#114588=CARTESIAN_POINT('Ctrl Pts',(21.4050329248816,5.18011525469409,-8.23507885105442));
#114589=CARTESIAN_POINT('Ctrl Pts',(21.3980845672483,5.14838550186882,-8.09009144410335));
#114590=CARTESIAN_POINT('Ctrl Pts',(21.3911359899612,5.11665474599245,-7.94509945376403));
#114591=CARTESIAN_POINT('Ctrl Pts',(21.3841874126742,5.09125751019233,-7.79871451694216));
#114592=CARTESIAN_POINT('Ctrl Pts',(21.3772388353872,5.07229262147526,-7.6515017502624));
#114593=CARTESIAN_POINT('Ctrl Pts',(21.3702906875388,5.05332890483344,-7.50429808168186));
#114594=CARTESIAN_POINT('Ctrl Pts',(21.3633425396903,5.04079678109596,-7.35626701042103));
#114595=CARTESIAN_POINT('Ctrl Pts',(21.3563943918419,5.03474335699634,-7.20798016388597));
#114596=CARTESIAN_POINT('Ctrl Pts',(21.3494449282258,5.02868878656242,-7.05966523633523));
#114597=CARTESIAN_POINT('Ctrl Pts',(21.3424954646096,5.02911538076994,-6.91109476395886));
#114598=CARTESIAN_POINT('Ctrl Pts',(21.3355460009934,5.03601815715149,-6.76284242248547));
#114599=CARTESIAN_POINT('Ctrl Pts',(21.331508249577,5.04002878252507,-6.67670540028748));
#114600=CARTESIAN_POINT('Ctrl Pts',(21.3274704981606,5.04622466346145,-6.59067577933083));
#114601=CARTESIAN_POINT('Ctrl Pts',(21.3234327467442,5.0545967490254,-6.50486568161013));
#114602=CARTESIAN_POINT('Ctrl Pts',(21.31655060643,5.06886653971637,-6.35860676866734));
#114603=CARTESIAN_POINT('Ctrl Pts',(21.3096684661157,5.08946675265018,-6.21293115702204));
#114604=CARTESIAN_POINT('Ctrl Pts',(21.3027863258014,5.11632565505071,-6.06839708719742));
#114605=CARTESIAN_POINT('Ctrl Pts',(21.2959056901371,5.14317868525947,-5.92389461701757));
#114606=CARTESIAN_POINT('Ctrl Pts',(21.2890250544729,5.17628761360455,-5.78053352530322));
#114607=CARTESIAN_POINT('Ctrl Pts',(21.2821444188086,5.21552937377503,-5.63886309116306));
#114608=CARTESIAN_POINT('Ctrl Pts',(21.2752633519625,5.25477359306887,-5.49718377910633));
#114609=CARTESIAN_POINT('Ctrl Pts',(21.2683822851165,5.30015132574767,-5.35719566559861));
#114610=CARTESIAN_POINT('Ctrl Pts',(21.2615012182705,5.35148915214393,-5.21943454549694));
#114611=CARTESIAN_POINT('Ctrl Pts',(21.2546203142567,5.4028257636912,-5.08167668534937));
#114612=CARTESIAN_POINT('Ctrl Pts',(21.247739410243,5.46012206546334,-4.946146031246));
#114613=CARTESIAN_POINT('Ctrl Pts',(21.2408585062293,5.52315589001064,-4.81335989692717));
#114614=CARTESIAN_POINT('Ctrl Pts',(21.2339753023867,5.58621078257564,-4.68052938102991));
#114615=CARTESIAN_POINT('Ctrl Pts',(21.2270920985441,5.65500688289976,-4.55044552515016));
#114616=CARTESIAN_POINT('Ctrl Pts',(21.2202088947016,5.72927504815719,-4.42360302492416));
#114617=CARTESIAN_POINT('Ctrl Pts',(21.2158349637464,5.7764687437722,-4.34300097523082));
#114618=CARTESIAN_POINT('Ctrl Pts',(21.2114610327912,5.82587110691438,-4.26370729362511));
#114619=CARTESIAN_POINT('Ctrl Pts',(21.2070871018361,5.87740373338063,-4.1858432276432));
#114620=CARTESIAN_POINT('Ctrl Pts',(21.2015511092381,5.9426274969921,-4.08729231375261));
#114621=CARTESIAN_POINT('Ctrl Pts',(21.1960151166401,6.01128077510044,-3.99100686207785));
#114622=CARTESIAN_POINT('Ctrl Pts',(21.1904791240421,6.08319878352127,-3.89721939777839));
#114623=CARTESIAN_POINT('Ctrl Pts',(22.6904763725673,6.08319878352126,-3.8972193977784));
#114624=CARTESIAN_POINT('Ctrl Pts',(22.6832062449146,6.17769169863551,-3.77399225206862));
#114625=CARTESIAN_POINT('Ctrl Pts',(22.6759361172618,6.27782641665125,-3.65507385892176));
#114626=CARTESIAN_POINT('Ctrl Pts',(22.6686659896091,6.38318054496964,-3.54096956635808));
#114627=CARTESIAN_POINT('Ctrl Pts',(22.6617335873508,6.48364056877638,-3.4321658570933));
#114628=CARTESIAN_POINT('Ctrl Pts',(22.6548011850925,6.58884578356875,-3.32773933975731));
#114629=CARTESIAN_POINT('Ctrl Pts',(22.6478687828343,6.69839058953318,-3.22809209902919));
#114630=CARTESIAN_POINT('Ctrl Pts',(22.6409364801077,6.80793382271231,-3.12844628898247));
#114631=CARTESIAN_POINT('Ctrl Pts',(22.6340041773811,6.92181627608599,-3.03357983863798));
#114632=CARTESIAN_POINT('Ctrl Pts',(22.6270718746546,7.03959749637345,-2.94385607774054));
#114633=CARTESIAN_POINT('Ctrl Pts',(22.6201382212635,7.15740166472249,-2.85411483539414));
#114634=CARTESIAN_POINT('Ctrl Pts',(22.6132045678725,7.27910585338731,-2.76951848290543));
#114635=CARTESIAN_POINT('Ctrl Pts',(22.6062709144814,7.40423831077666,-2.69038868048967));
#114636=CARTESIAN_POINT('Ctrl Pts',(22.6052588898991,7.42250243731776,-2.67883902539102));
#114637=CARTESIAN_POINT('Ctrl Pts',(22.6042468653167,7.44083954937272,-2.66740575310795));
#114638=CARTESIAN_POINT('Ctrl Pts',(22.6032348407344,7.45924813015834,-2.65608978550349));
#114639=CARTESIAN_POINT('Ctrl Pts',(22.5963013558529,7.58536721737684,-2.57856292333584));
#114640=CARTESIAN_POINT('Ctrl Pts',(22.5893678709714,7.71488667542901,-2.50651889974946));
#114641=CARTESIAN_POINT('Ctrl Pts',(22.5824343860899,7.84731029346214,-2.44024001252559));
#114642=CARTESIAN_POINT('Ctrl Pts',(22.5755022191216,7.97970874048394,-2.37397372355758));
#114643=CARTESIAN_POINT('Ctrl Pts',(22.5685700521532,8.11500995065022,-2.31347053248643));
#114644=CARTESIAN_POINT('Ctrl Pts',(22.5616378851848,8.25269401104442,-2.25896632791746));
#114645=CARTESIAN_POINT('Ctrl Pts',(22.5547054748914,8.39038290426868,-2.20446021020359));
#114646=CARTESIAN_POINT('Ctrl Pts',(22.547773064598,8.53045450894211,-2.15595362514327));
#114647=CARTESIAN_POINT('Ctrl Pts',(22.5408406543045,8.6723693620486,-2.11363414141518));
#114648=CARTESIAN_POINT('Ctrl Pts',(22.5339086194588,8.81427652928531,-2.07131694963917));
#114649=CARTESIAN_POINT('Ctrl Pts',(22.526976584613,8.95802642811843,-2.03518628227907));
#114650=CARTESIAN_POINT('Ctrl Pts',(22.5200445497673,9.10306486807958,-2.00537970212354));
#114651=CARTESIAN_POINT('Ctrl Pts',(22.5131109730705,9.24813556807392,-1.97556649226857));
#114652=CARTESIAN_POINT('Ctrl Pts',(22.5061773963736,9.39449505792168,-1.95208024682281));
#114653=CARTESIAN_POINT('Ctrl Pts',(22.4992438196768,9.54157877108382,-1.93500744042109));
#114654=CARTESIAN_POINT('Ctrl Pts',(22.4951256117266,9.62893935615773,-1.92486702226029));
#114655=CARTESIAN_POINT('Ctrl Pts',(22.4910074037764,9.71655526433281,-1.91698814636579));
#114656=CARTESIAN_POINT('Ctrl Pts',(22.4868891958262,9.80430724843803,-1.9113802780782));
#114657=CARTESIAN_POINT('Ctrl Pts',(22.4799556232921,9.95204984768639,-1.90193865638155));
#114658=CARTESIAN_POINT('Ctrl Pts',(22.4730220507579,10.1002293919555,-1.89893406231333));
#114659=CARTESIAN_POINT('Ctrl Pts',(22.4660884782238,10.2482752299219,-1.90238355260451));
#114660=CARTESIAN_POINT('Ctrl Pts',(22.4591562219442,10.3962929631829,-1.90583238805183));
#114661=CARTESIAN_POINT('Ctrl Pts',(22.4522239656647,10.5441767104752,-1.91573285564485));
#114662=CARTESIAN_POINT('Ctrl Pts',(22.4452917093852,10.6913566113617,-1.93204990669116));
#114663=CARTESIAN_POINT('Ctrl Pts',(22.4383592081633,10.838541712659,-1.94836753427928));
#114664=CARTESIAN_POINT('Ctrl Pts',(22.4314267069415,10.9850225888615,-1.9711021658943));
#114665=CARTESIAN_POINT('Ctrl Pts',(22.4244942057197,11.1302347335151,-2.00016690347203));
#114666=CARTESIAN_POINT('Ctrl Pts',(22.4175620792479,11.2754390284404,-2.02923006989818));
#114667=CARTESIAN_POINT('Ctrl Pts',(22.410629952776,11.4193744050801,-2.06462259177438));
#114668=CARTESIAN_POINT('Ctrl Pts',(22.4036978263042,11.5614867616133,-2.10620649040397));
#114669=CARTESIAN_POINT('Ctrl Pts',(22.3967641577058,11.7036307325799,-2.14779963982234));
#114670=CARTESIAN_POINT('Ctrl Pts',(22.3898304891073,11.8439505557084,-2.19558682522712));
#114671=CARTESIAN_POINT('Ctrl Pts',(22.3828968205088,11.9819068852309,-2.24938006871217));
#114672=CARTESIAN_POINT('Ctrl Pts',(22.3787790639786,12.063836179762,-2.28132671809408));
#114673=CARTESIAN_POINT('Ctrl Pts',(22.3746613074483,12.1449322010469,-2.31539070984882));
#114674=CARTESIAN_POINT('Ctrl Pts',(22.370543550918,12.2250851901569,-2.35152458210273));
#114675=CARTESIAN_POINT('Ctrl Pts',(22.3636099924989,12.3600483499194,-2.41236749798139));
#114676=CARTESIAN_POINT('Ctrl Pts',(22.3566764340798,12.4923832519696,-2.47910262136328));
#114677=CARTESIAN_POINT('Ctrl Pts',(22.3497428756607,12.6215776949439,-2.55147780017193));
#114678=CARTESIAN_POINT('Ctrl Pts',(22.3428106341768,12.7507475991896,-2.62383923229903));
#114679=CARTESIAN_POINT('Ctrl Pts',(22.3358783926929,12.8767779461898,-2.7018384210654));
#114680=CARTESIAN_POINT('Ctrl Pts',(22.328946151209,12.9991816332476,-2.78517754539985));
#114681=CARTESIAN_POINT('Ctrl Pts',(22.3220136656563,13.1215896298659,-2.86851960391878));
#114682=CARTESIAN_POINT('Ctrl Pts',(22.3150811801037,13.2403704359038,-2.95720179093612));
#114683=CARTESIAN_POINT('Ctrl Pts',(22.308148694551,13.3550659593708,-3.0508829794816));
#114684=CARTESIAN_POINT('Ctrl Pts',(22.3012165842048,13.4697552751808,-3.14455909772731));
#114685=CARTESIAN_POINT('Ctrl Pts',(22.2942844738585,13.580359495408,-3.24323346626158));
#114686=CARTESIAN_POINT('Ctrl Pts',(22.2873523635122,13.6864536413925,-3.34652469654105));
#114687=CARTESIAN_POINT('Ctrl Pts',(22.2804187116004,13.7925713806377,-3.44983889676766));
#114688=CARTESIAN_POINT('Ctrl Pts',(22.2734850596885,13.8941768046595,-3.55777177953251));
#114689=CARTESIAN_POINT('Ctrl Pts',(22.2665514077766,13.9908813866036,-3.66990468797189));
#114690=CARTESIAN_POINT('Ctrl Pts',(22.2624335738543,14.0483133738203,-3.73649942045101));
#114691=CARTESIAN_POINT('Ctrl Pts',(22.2583157399321,14.1040175187899,-3.80457484120395));
#114692=CARTESIAN_POINT('Ctrl Pts',(22.2541979060098,14.1579190618731,-3.874037610281));
#114693=CARTESIAN_POINT('Ctrl Pts',(22.2472642956059,14.248678501657,-3.99099904861213));
#114694=CARTESIAN_POINT('Ctrl Pts',(22.240330685202,14.3343563570106,-4.11193599116586));
#114695=CARTESIAN_POINT('Ctrl Pts',(22.2333970747981,14.4146181346602,-4.23638577728254));
#114696=CARTESIAN_POINT('Ctrl Pts',(22.2264647807023,14.4948646750486,-4.36081193728546));
#114697=CARTESIAN_POINT('Ctrl Pts',(22.2195324866065,14.569697010104,-4.48874933264206));
#114698=CARTESIAN_POINT('Ctrl Pts',(22.2126001925108,14.6388242094336,-4.61970670416093));
#114699=CARTESIAN_POINT('Ctrl Pts',(22.2056676539223,14.7079538467869,-4.75066869437094));
#114700=CARTESIAN_POINT('Ctrl Pts',(22.1987351153338,14.7713777885139,-4.88465058310104));
#114701=CARTESIAN_POINT('Ctrl Pts',(22.1918025767453,14.8288510170149,-5.0211364324741));
#114702=CARTESIAN_POINT('Ctrl Pts',(22.1848704132515,14.8863211358465,-5.1576148970895));
#114703=CARTESIAN_POINT('Ctrl Pts',(22.1779382497577,14.9378410582831,-5.29659674622179));
#114704=CARTESIAN_POINT('Ctrl Pts',(22.1710060862639,14.9832138788456,-5.43754597433969));
#114705=CARTESIAN_POINT('Ctrl Pts',(22.1640723815,15.028596787423,-5.57852654055607));
#114706=CARTESIAN_POINT('Ctrl Pts',(22.1571386767362,15.0678297619024,-5.72147504499835));
#114707=CARTESIAN_POINT('Ctrl Pts',(22.1502049719723,15.1007655570025,-5.86583962255727));
#114708=CARTESIAN_POINT('Ctrl Pts',(22.1460874016821,15.1203244300737,-5.95157031282543));
#114709=CARTESIAN_POINT('Ctrl Pts',(22.1419698313918,15.1376635206223,-6.03780011735071));
#114710=CARTESIAN_POINT('Ctrl Pts',(22.1378522611016,15.1527604864707,-6.12441157781638));
#114711=CARTESIAN_POINT('Ctrl Pts',(22.1309189472056,15.1781813040225,-6.27025108997362));
#114712=CARTESIAN_POINT('Ctrl Pts',(22.1239856333095,15.1972510326479,-6.41722360612244));
#114713=CARTESIAN_POINT('Ctrl Pts',(22.1170523194135,15.2098907721861,-6.56476374015239));
#114714=CARTESIAN_POINT('Ctrl Pts',(22.1101203233419,15.2225281092719,-6.71227583102913));
#114715=CARTESIAN_POINT('Ctrl Pts',(22.1031883272702,15.2287378674464,-6.86035499529274));
#114716=CARTESIAN_POINT('Ctrl Pts',(22.0962563311985,15.2284930298674,-7.00843097644238));
#114717=CARTESIAN_POINT('Ctrl Pts',(22.089324090006,15.2282481836307,-7.1565121936757));
#114718=CARTESIAN_POINT('Ctrl Pts',(22.0823918488135,15.2215482821266,-7.30458989694499));
#114719=CARTESIAN_POINT('Ctrl Pts',(22.075459607621,15.2084184326879,-7.45209352362448));
#114720=CARTESIAN_POINT('Ctrl Pts',(22.0685277404533,15.195289291662,-7.59958919183699));
#114721=CARTESIAN_POINT('Ctrl Pts',(22.0615958732855,15.1757309271479,-7.7465105161877));
#114722=CARTESIAN_POINT('Ctrl Pts',(22.0546640061178,15.1498203546765,-7.89229173279893));
#114723=CARTESIAN_POINT('Ctrl Pts',(22.0477305934374,15.1239040052452,-8.038105452445));
#114724=CARTESIAN_POINT('Ctrl Pts',(22.040797180757,15.0916326758373,-8.18277823079126));
#114725=CARTESIAN_POINT('Ctrl Pts',(22.0338637680765,15.0531346874517,-8.32575354592097));
#114726=CARTESIAN_POINT('Ctrl Pts',(22.0297447174488,15.030263531423,-8.41069332791254));
#114727=CARTESIAN_POINT('Ctrl Pts',(22.0256256668211,15.0051957146653,-8.49503421516273));
#114728=CARTESIAN_POINT('Ctrl Pts',(22.0215066161934,14.9779665423999,-8.57866183434858));
#114729=CARTESIAN_POINT('Ctrl Pts',(22.0145723805751,14.9321274612027,-8.71944515265239));
#114730=CARTESIAN_POINT('Ctrl Pts',(22.0076381449568,14.8801445592657,-8.85825478409665));
#114731=CARTESIAN_POINT('Ctrl Pts',(22.0007039093386,14.8222129650008,-8.99455409255137));
#114732=CARTESIAN_POINT('Ctrl Pts',(21.9937709880668,14.7642923513531,-9.13082756621661));
#114733=CARTESIAN_POINT('Ctrl Pts',(21.986838066795,14.7004254241925,-9.26459136227122));
#114734=CARTESIAN_POINT('Ctrl Pts',(21.9799051455232,14.6308554344628,-9.39532884018717));
#114735=CARTESIAN_POINT('Ctrl Pts',(21.9729719829147,14.5612830229847,-9.52607086910665));
#114736=CARTESIAN_POINT('Ctrl Pts',(21.9660388203062,14.4860073039592,-9.65378607580445));
#114737=CARTESIAN_POINT('Ctrl Pts',(21.9591056576977,14.4053177264321,-9.77798196004382));
#114738=CARTESIAN_POINT('Ctrl Pts',(21.9521728734695,14.3246325525718,-9.9021710662419));
#114739=CARTESIAN_POINT('Ctrl Pts',(21.9452400892412,14.23853429223,-10.0228409576983));
#114740=CARTESIAN_POINT('Ctrl Pts',(21.9383073050129,14.1473560123797,-10.1395276816401));
#114741=CARTESIAN_POINT('Ctrl Pts',(21.9313729900041,14.0561576000789,-10.2562401703768));
#114742=CARTESIAN_POINT('Ctrl Pts',(21.9244386749953,13.9598771305219,-10.3689674737665));
#114743=CARTESIAN_POINT('Ctrl Pts',(21.9175043599865,13.8588886754882,-10.4772778300189));
#114744=CARTESIAN_POINT('Ctrl Pts',(21.9133898970861,13.7989673637105,-10.541543578253));
#114745=CARTESIAN_POINT('Ctrl Pts',(21.9092754341856,13.7373893106772,-10.6042549247956));
#114746=CARTESIAN_POINT('Ctrl Pts',(21.9051609712852,13.6742389692849,-10.6653276305991));
#114747=CARTESIAN_POINT('Ctrl Pts',(21.8982288511239,13.5678421526517,-10.7682240098965));
#114748=CARTESIAN_POINT('Ctrl Pts',(21.8912967309625,13.4569435049872,-10.8665024520393));
#114749=CARTESIAN_POINT('Ctrl Pts',(21.8843646108012,13.3419664401948,-10.959780343734));
#114750=CARTESIAN_POINT('Ctrl Pts',(21.877433811209,13.2270112785383,-11.0530404659862));
#114751=CARTESIAN_POINT('Ctrl Pts',(21.8705030116169,13.1079795066484,-11.1413017300309));
#114752=CARTESIAN_POINT('Ctrl Pts',(21.8635722120248,12.9853276996924,-11.2242217211777));
#114753=CARTESIAN_POINT('Ctrl Pts',(21.8566411598445,12.8626714227769,-11.3071447342857));
#114754=CARTESIAN_POINT('Ctrl Pts',(21.8497101076642,12.7363951190217,-11.3847258969099));
#114755=CARTESIAN_POINT('Ctrl Pts',(21.8427790554839,12.6069848824144,-11.4566657556304));
#114756=CARTESIAN_POINT('Ctrl Pts',(21.8358483702673,12.4775814974173,-11.5286018055031));
#114757=CARTESIAN_POINT('Ctrl Pts',(21.8289176850508,12.3450448012554,-11.5948969892324));
#114758=CARTESIAN_POINT('Ctrl Pts',(21.8219869998343,12.209886058069,-11.6552975038543));
#114759=CARTESIAN_POINT('Ctrl Pts',(21.8150547479171,12.0746967618724,-11.7157116721808));
#114760=CARTESIAN_POINT('Ctrl Pts',(21.8081224959999,11.9368845365068,-11.7702283738593));
#114761=CARTESIAN_POINT('Ctrl Pts',(21.8011902440826,11.796981800889,-11.81864145208));
#114762=CARTESIAN_POINT('Ctrl Pts',(21.7970652715141,11.7137339683553,-11.8474492077709));
#114763=CARTESIAN_POINT('Ctrl Pts',(21.7929402989456,11.6297463168939,-11.8740967543871));
#114764=CARTESIAN_POINT('Ctrl Pts',(21.788815326377,11.5451338329821,-11.8985489536103));
#114765=CARTESIAN_POINT('Ctrl Pts',(21.781841763805,11.4020903481749,-11.939887153677));
#114766=CARTESIAN_POINT('Ctrl Pts',(21.7748682012329,11.2572131443299,-11.9749619273583));
#114767=CARTESIAN_POINT('Ctrl Pts',(21.7678946386609,11.1110621236963,-12.0036323603283));
#114768=CARTESIAN_POINT('Ctrl Pts',(21.7609226052006,10.9649431499895,-12.0322965066555));
#114769=CARTESIAN_POINT('Ctrl Pts',(21.7539505717403,10.8175512332713,-12.0545590528571));
#114770=CARTESIAN_POINT('Ctrl Pts',(21.7469785382801,10.669456698842,-12.0703301434301));
#114771=CARTESIAN_POINT('Ctrl Pts',(21.7400073493926,10.5213801041739,-12.0860993235369));
#114772=CARTESIAN_POINT('Ctrl Pts',(21.7330361605051,10.3726013821705,-12.0953785825651));
#114773=CARTESIAN_POINT('Ctrl Pts',(21.7260649716176,10.2236966737367,-12.0981298518826));
#114774=CARTESIAN_POINT('Ctrl Pts',(21.7245944825346,10.192287002918,-12.0987101993042));
#114775=CARTESIAN_POINT('Ctrl Pts',(21.7231239934515,10.1608717378449,-12.0990002690569));
#114776=CARTESIAN_POINT('Ctrl Pts',(21.7216535043684,10.1294562993151,-12.0989999998127));
#114777=CARTESIAN_POINT('Origin',(-26.8463464956315,10.1295,-7.));
#114778=CARTESIAN_POINT('',(-21.5963464956315,10.1291161856969,-12.0989999855547));
#114779=CARTESIAN_POINT('Ctrl Pts',(-22.5651720736884,14.1754919335065,
-3.89745664672419));
#114780=CARTESIAN_POINT('Ctrl Pts',(-22.5448385295376,13.9111214980616,
-3.55278411761959));
#114781=CARTESIAN_POINT('Ctrl Pts',(-22.4857231037507,13.0157743410226,
-2.64786717956705));
#114782=CARTESIAN_POINT('Ctrl Pts',(-22.3878257963277,11.0466612589386,
-1.77459151989547));
#114783=CARTESIAN_POINT('Ctrl Pts',(-22.2714801514196,8.49288304070303,
-1.95345842253097));
#114784=CARTESIAN_POINT('Ctrl Pts',(-22.1551345065114,6.32026199879215,
-3.30737376532056));
#114785=CARTESIAN_POINT('Ctrl Pts',(-22.0387888616032,5.03442895202576,
-5.52111017618096));
#114786=CARTESIAN_POINT('Ctrl Pts',(-21.922443216695,4.93530635993922,-8.0791637580032));
#114787=CARTESIAN_POINT('Ctrl Pts',(-21.8060975717868,6.0448778396091,-10.3860101436405));
#114788=CARTESIAN_POINT('Ctrl Pts',(-21.6973986661372,7.9715431412064,-11.8045112188381));
#114789=CARTESIAN_POINT('Ctrl Pts',(-21.6274816421238,9.46413915462446,
-12.0984964029847));
#114790=CARTESIAN_POINT('Ctrl Pts',(-21.5963464997463,10.1291160878984,
-12.0991317151048));
#114791=CARTESIAN_POINT('Ctrl Pts',(-21.5963464956315,10.1291161856969,
-12.0989999855547));
#114792=CARTESIAN_POINT('Ctrl Pts',(-21.5886997577445,10.2924291785527,
-12.0990122785264));
#114793=CARTESIAN_POINT('Ctrl Pts',(-21.5810530198574,10.4557419617455,
-12.0911739196201));
#114794=CARTESIAN_POINT('Ctrl Pts',(-21.5734062819704,10.6183440341081,
-12.0755130292727));
#114795=CARTESIAN_POINT('Ctrl Pts',(-21.5666848517297,10.761270142277,-12.0617472138972));
#114796=CARTESIAN_POINT('Ctrl Pts',(-21.5599634214889,10.9036700321504,
-12.0419345290273));
#114797=CARTESIAN_POINT('Ctrl Pts',(-21.5532419912482,11.0450086188271,
-12.0161384519223));
#114798=CARTESIAN_POINT('Ctrl Pts',(-21.5465222109883,11.1863125096208,
-11.9903487072541));
#114799=CARTESIAN_POINT('Ctrl Pts',(-21.5398024307283,11.3265552547391,
-11.9585785632498));
#114800=CARTESIAN_POINT('Ctrl Pts',(-21.5330826504684,11.4652102525116,
-11.9209429097822));
#114801=CARTESIAN_POINT('Ctrl Pts',(-21.5263615518046,11.6038924540449,
-11.8832998722942));
#114802=CARTESIAN_POINT('Ctrl Pts',(-21.5196404531407,11.7409859290593,
-11.8397891166586));
#114803=CARTESIAN_POINT('Ctrl Pts',(-21.5129193544769,11.8759772620419,
-11.7905759750964));
#114804=CARTESIAN_POINT('Ctrl Pts',(-21.5061977698631,12.0109783551886,
-11.7413592753181));
#114805=CARTESIAN_POINT('Ctrl Pts',(-21.4994761852493,12.1438766594992,
-11.6864394991817));
#114806=CARTESIAN_POINT('Ctrl Pts',(-21.4927546006356,12.2741773917404,
-11.6260306835729));
#114807=CARTESIAN_POINT('Ctrl Pts',(-21.4860285543178,12.4045646159827,
-11.5655817693456));
#114808=CARTESIAN_POINT('Ctrl Pts',(-21.479302508,12.5323504905475,-11.4996366941743));
#114809=CARTESIAN_POINT('Ctrl Pts',(-21.4725764616822,12.6570630553875,
-11.4284563903284));
#114810=CARTESIAN_POINT('Ctrl Pts',(-21.4674045201422,12.7529598221028,
-11.3737228436212));
#114811=CARTESIAN_POINT('Ctrl Pts',(-21.4622325786022,12.8470398696579,
-11.3158948186789));
#114812=CARTESIAN_POINT('Ctrl Pts',(-21.4570606370622,12.9390999696984,
-11.255108577965));
#114813=CARTESIAN_POINT('Ctrl Pts',(-21.4497817937609,13.0686627339555,
-11.1695597530969));
#114814=CARTESIAN_POINT('Ctrl Pts',(-21.4425029504596,13.1943036068353,
-11.0780978347688));
#114815=CARTESIAN_POINT('Ctrl Pts',(-21.4352241071583,13.3155153827349,
-10.9810936915597));
#114816=CARTESIAN_POINT('Ctrl Pts',(-21.427946142148,13.4367125327922,-10.8841012532143));
#114817=CARTESIAN_POINT('Ctrl Pts',(-21.4206681771377,13.553481456089,-10.7815680846603));
#114818=CARTESIAN_POINT('Ctrl Pts',(-21.4133902121274,13.6653475008962,
-10.6739057487102));
#114819=CARTESIAN_POINT('Ctrl Pts',(-21.4061165971437,13.7771466835695,
-10.5663077623448));
#114820=CARTESIAN_POINT('Ctrl Pts',(-21.39884298216,13.884048659969,-10.4535869088841));
#114821=CARTESIAN_POINT('Ctrl Pts',(-21.3915693671764,13.9856148483401,
-10.3361923320473));
#114822=CARTESIAN_POINT('Ctrl Pts',(-21.3843006041387,14.0871132858521,
-10.2188760645726));
#114823=CARTESIAN_POINT('Ctrl Pts',(-21.377031841101,14.1832828744343,-10.0968924881681));
#114824=CARTESIAN_POINT('Ctrl Pts',(-21.3697630780634,14.2737238199281,
-9.97072548889001));
#114825=CARTESIAN_POINT('Ctrl Pts',(-21.362503319337,14.3640527300697,-9.8447147812575));
#114826=CARTESIAN_POINT('Ctrl Pts',(-21.3552435606107,14.4486670178919,
-9.714531202894));
#114827=CARTESIAN_POINT('Ctrl Pts',(-21.3479838018843,14.5272087473904,
-9.58068959255577));
#114828=CARTESIAN_POINT('Ctrl Pts',(-21.3455608653075,14.5534219641621,
-9.53602010071664));
#114829=CARTESIAN_POINT('Ctrl Pts',(-21.3431379287308,14.5789591128104,
-9.49094340429971));
#114830=CARTESIAN_POINT('Ctrl Pts',(-21.340714992154,14.6038079371955,-9.44547939740844));
#114831=CARTESIAN_POINT('Ctrl Pts',(-21.3339843753385,14.6728348844358,
-9.31918603413384));
#114832=CARTESIAN_POINT('Ctrl Pts',(-21.3272537585231,14.7365235713096,
-9.18994468860557));
#114833=CARTESIAN_POINT('Ctrl Pts',(-21.3205231417076,14.7946316255852,
-9.05823903275719));
#114834=CARTESIAN_POINT('Ctrl Pts',(-21.3137927443259,14.852737785403,-8.92653767081938));
#114835=CARTESIAN_POINT('Ctrl Pts',(-21.3070623469442,14.9052635284585,
-8.79237249361583));
#114836=CARTESIAN_POINT('Ctrl Pts',(-21.3003319495625,14.9520141566811,
-8.65624823278712));
#114837=CARTESIAN_POINT('Ctrl Pts',(-21.2935981100412,14.9987886946639,
-8.52005435367601));
#114838=CARTESIAN_POINT('Ctrl Pts',(-21.28686427052,15.0397820953059,-8.38189973457362));
#114839=CARTESIAN_POINT('Ctrl Pts',(-21.2801304309987,15.0748490349447,
-8.24230588929287));
#114840=CARTESIAN_POINT('Ctrl Pts',(-21.2733949256715,15.1099246493843,
-8.10267751152055));
#114841=CARTESIAN_POINT('Ctrl Pts',(-21.2666594203442,15.1390707988718,
-7.96160955465916));
#114842=CARTESIAN_POINT('Ctrl Pts',(-21.259923915017,15.1621931252,-7.8196346183301));
#114843=CARTESIAN_POINT('Ctrl Pts',(-21.2531821581971,15.1853369122869,
-7.67752790936666));
#114844=CARTESIAN_POINT('Ctrl Pts',(-21.2464404013771,15.2024456529537,
-7.53451290148324));
#114845=CARTESIAN_POINT('Ctrl Pts',(-21.2396986445572,15.2134767052047,
-7.39112895691341));
#114846=CARTESIAN_POINT('Ctrl Pts',(-21.2345888787867,15.2218374477692,
-7.28245426104888));
#114847=CARTESIAN_POINT('Ctrl Pts',(-21.2294791130163,15.2267078994303,
-7.17356777436203));
#114848=CARTESIAN_POINT('Ctrl Pts',(-21.2243693472458,15.2280894461353,
-7.06470440292566));
#114849=CARTESIAN_POINT('Ctrl Pts',(-21.2176540790633,15.229905078602,-6.92163586176665));
#114850=CARTESIAN_POINT('Ctrl Pts',(-21.2109388108808,15.2256961764928,
-6.77836167525376));
#114851=CARTESIAN_POINT('Ctrl Pts',(-21.2042235426983,15.2154493359987,
-6.63541756535092));
#114852=CARTESIAN_POINT('Ctrl Pts',(-21.1975132699025,15.2052101179746,
-6.49257978941473));
#114853=CARTESIAN_POINT('Ctrl Pts',(-21.1908029971066,15.1889419313426,
-6.3500719684068));
#114854=CARTESIAN_POINT('Ctrl Pts',(-21.1840927243108,15.1666834132725,
-6.2084292444435));
#114855=CARTESIAN_POINT('Ctrl Pts',(-21.1773862020136,15.14443733591,-6.06686568728304));
#114856=CARTESIAN_POINT('Ctrl Pts',(-21.1706796797165,15.116207652359,-5.92616662852227));
#114857=CARTESIAN_POINT('Ctrl Pts',(-21.1639731574193,15.0820847524494,
-5.78686139711654));
#114858=CARTESIAN_POINT('Ctrl Pts',(-21.1572691435834,15.0479746156336,
-5.64760827047765));
#114859=CARTESIAN_POINT('Ctrl Pts',(-21.1505651297475,15.0079757415206,
-5.50974829121759));
#114860=CARTESIAN_POINT('Ctrl Pts',(-21.1438611159116,14.9622294466977,
-5.37379979860372));
#114861=CARTESIAN_POINT('Ctrl Pts',(-21.1371569432884,14.916482068355,-5.23784808599431));
#114862=CARTESIAN_POINT('Ctrl Pts',(-21.1304527706652,14.864987106323,-5.10380830382993));
#114863=CARTESIAN_POINT('Ctrl Pts',(-21.123748598042,14.8079355765373,-4.97218305653825));
#114864=CARTESIAN_POINT('Ctrl Pts',(-21.1170446465545,14.7508859285836,
-4.84056215087628));
#114865=CARTESIAN_POINT('Ctrl Pts',(-21.1103406950669,14.6882802290009,
-4.71135595904673));
#114866=CARTESIAN_POINT('Ctrl Pts',(-21.1036367435794,14.6203572164572,
-4.58504607468499));
#114867=CARTESIAN_POINT('Ctrl Pts',(-21.096929084689,14.5523966412952,-4.45866633873984));
#114868=CARTESIAN_POINT('Ctrl Pts',(-21.0902214257986,14.479113053607,-4.3351864363366));
#114869=CARTESIAN_POINT('Ctrl Pts',(-21.0835137669082,14.4007908917012,
-4.21506281606388));
#114870=CARTESIAN_POINT('Ctrl Pts',(-21.0774380110089,14.3298471622981,
-4.10625558444275));
#114871=CARTESIAN_POINT('Ctrl Pts',(-21.0713622551095,14.2547701490326,
-4.00020189286647));
#114872=CARTESIAN_POINT('Ctrl Pts',(-21.0652864992102,14.1758012177496,
-3.89721939943571));
#114873=CARTESIAN_POINT('',(-21.7216535043236,10.1295436686122,-12.098999999813));
#114874=CARTESIAN_POINT('Ctrl Pts',(-21.7216535043236,10.1295436686122,
-12.098999999813));
#114875=CARTESIAN_POINT('Ctrl Pts',(-21.7145780772905,10.2807026533976,
-12.0989987052645));
#114876=CARTESIAN_POINT('Ctrl Pts',(-21.7075026502575,10.4318398568485,
-12.0922714484638));
#114877=CARTESIAN_POINT('Ctrl Pts',(-21.7004272232244,10.582361479932,-12.0788500155049));
#114878=CARTESIAN_POINT('Ctrl Pts',(-21.693349719895,10.7329272738466,-12.0654246440032));
#114879=CARTESIAN_POINT('Ctrl Pts',(-21.6862722165656,10.8828768275428,
-12.0453011997449));
#114880=CARTESIAN_POINT('Ctrl Pts',(-21.6791947132363,11.0316213327613,
-12.0185633503003));
#114881=CARTESIAN_POINT('Ctrl Pts',(-21.6769530359805,11.0787335923755,
-12.0100945971002));
#114882=CARTESIAN_POINT('Ctrl Pts',(-21.6747113587247,11.1257250216099,
-12.0009626767532));
#114883=CARTESIAN_POINT('Ctrl Pts',(-21.6724696814689,11.1725771008058,
-11.9911713216213));
#114884=CARTESIAN_POINT('Ctrl Pts',(-21.665538500834,11.3174419439415,-11.9608968247447));
#114885=CARTESIAN_POINT('Ctrl Pts',(-21.6586073201992,11.4610130681156,
-11.9243059246399));
#114886=CARTESIAN_POINT('Ctrl Pts',(-21.6516761395644,11.6027362745548,
-11.88153417271));
#114887=CARTESIAN_POINT('Ctrl Pts',(-21.6447462728878,11.7444326142333,
-11.8387705291094));
#114888=CARTESIAN_POINT('Ctrl Pts',(-21.6378164062113,11.884281418354,-11.7898284670043));
#114889=CARTESIAN_POINT('Ctrl Pts',(-21.6308865395347,12.0217431373186,
-11.7348935478288));
#114890=CARTESIAN_POINT('Ctrl Pts',(-21.6239564014542,12.1592102398846,
-11.6799564771618));
#114891=CARTESIAN_POINT('Ctrl Pts',(-21.6170262633738,12.2942897616118,
-11.6190261995686));
#114892=CARTESIAN_POINT('Ctrl Pts',(-21.6100961252933,12.426461132908,-11.5523368234249));
#114893=CARTESIAN_POINT('Ctrl Pts',(-21.6031663413856,12.5586257494336,
-11.4856508555187));
#114894=CARTESIAN_POINT('Ctrl Pts',(-21.5962365574778,12.6878822178597,
-11.4132065281025));
#114895=CARTESIAN_POINT('Ctrl Pts',(-21.5893067735701,12.8137336190688,
-11.3352844056949));
#114896=CARTESIAN_POINT('Ctrl Pts',(-21.5823753954677,12.9396139723548,
-11.2573443573264));
#114897=CARTESIAN_POINT('Ctrl Pts',(-21.5754440173652,13.0620874116896,
-11.1739241703709));
#114898=CARTESIAN_POINT('Ctrl Pts',(-21.5685126392628,13.1806845732687,
-11.0853486631923));
#114899=CARTESIAN_POINT('Ctrl Pts',(-21.5643831050287,13.2513416679423,
-11.0325776869467));
#114900=CARTESIAN_POINT('Ctrl Pts',(-21.5602535707947,13.3206234444385,
-10.9779776769825));
#114901=CARTESIAN_POINT('Ctrl Pts',(-21.5561240365606,13.3884359580966,
-10.9216243345105));
#114902=CARTESIAN_POINT('Ctrl Pts',(-21.5491919873467,13.5022695420679,
-10.8270267064872));
#114903=CARTESIAN_POINT('Ctrl Pts',(-21.5422599381329,13.6120015769791,
-10.7274526569437));
#114904=CARTESIAN_POINT('Ctrl Pts',(-21.535327888919,13.7172057131023,-10.6232814845348));
#114905=CARTESIAN_POINT('Ctrl Pts',(-21.5283971834842,13.8223894553827,
-10.5191305057286));
#114906=CARTESIAN_POINT('Ctrl Pts',(-21.5214664780495,13.9230468150587,
-10.4103844146959));
#114907=CARTESIAN_POINT('Ctrl Pts',(-21.5145357726147,14.0187877971565,
-10.2974598452277));
#114908=CARTESIAN_POINT('Ctrl Pts',(-21.5076048482097,14.1145318041177,
-10.1845317079939));
#114909=CARTESIAN_POINT('Ctrl Pts',(-21.5006739238046,14.2053589060595,
-10.06742507829));
#114910=CARTESIAN_POINT('Ctrl Pts',(-21.4937429993995,14.2909186070078,
-9.94659060224677));
#114911=CARTESIAN_POINT('Ctrl Pts',(-21.4868124606186,14.3764735475678,
-9.82576284921712));
#114912=CARTESIAN_POINT('Ctrl Pts',(-21.4798819218377,14.4567614830456,
-9.70120793542299));
#114913=CARTESIAN_POINT('Ctrl Pts',(-21.4729513830568,14.5314745604009,
-9.57340649132294));
#114914=CARTESIAN_POINT('Ctrl Pts',(-21.4660193048808,14.6062042328509,
-9.44557666026405));
#114915=CARTESIAN_POINT('Ctrl Pts',(-21.4590872267048,14.6753564058714,
-9.31449914377409));
#114916=CARTESIAN_POINT('Ctrl Pts',(-21.4521551485288,14.7386682911608,
-9.18068077988451));
#114917=CARTESIAN_POINT('Ctrl Pts',(-21.4480295629033,14.7763479879615,
-9.10103956631653));
#114918=CARTESIAN_POINT('Ctrl Pts',(-21.4439039772779,14.8119599512988,
-9.020428027734));
#114919=CARTESIAN_POINT('Ctrl Pts',(-21.4397783916524,14.8454567318764,
-8.93895670479501));
#114920=CARTESIAN_POINT('Ctrl Pts',(-21.4328287564197,14.9018827590196,
-8.80171655812195));
#114921=CARTESIAN_POINT('Ctrl Pts',(-21.425879121187,14.9523225305843,-8.661990870534));
#114922=CARTESIAN_POINT('Ctrl Pts',(-21.4189294859543,14.9965767489365,
-8.52031737474841));
#114923=CARTESIAN_POINT('Ctrl Pts',(-21.4119810766083,15.0408231610291,
-8.37866886957668));
#114924=CARTESIAN_POINT('Ctrl Pts',(-21.4050326672623,15.0788860995113,
-8.23507355414718));
#114925=CARTESIAN_POINT('Ctrl Pts',(-21.3980842579163,15.110615897284,-8.09008505072978));
#114926=CARTESIAN_POINT('Ctrl Pts',(-21.3911356289697,15.1423466978592,
-7.94509196503175));
#114927=CARTESIAN_POINT('Ctrl Pts',(-21.3841870000231,15.1677438841323,
-7.79870592238976));
#114928=CARTESIAN_POINT('Ctrl Pts',(-21.3772383710765,15.1867086284737,
-7.65149204760402));
#114929=CARTESIAN_POINT('Ctrl Pts',(-21.3702901717336,15.2056722003069,
-7.50428727441542));
#114930=CARTESIAN_POINT('Ctrl Pts',(-21.3633419723906,15.2182040846995,
-7.35625509628934));
#114931=CARTESIAN_POINT('Ctrl Pts',(-21.3563937730477,15.2242571742947,
-7.20796714878315));
#114932=CARTESIAN_POINT('Ctrl Pts',(-21.349444258653,15.2303114095286,-7.05965113554095));
#114933=CARTESIAN_POINT('Ctrl Pts',(-21.3424947442583,15.2298843862783,
-6.91107958341258));
#114934=CARTESIAN_POINT('Ctrl Pts',(-21.3355452298636,15.2229810863828,
-6.76282617627361));
#114935=CARTESIAN_POINT('Ctrl Pts',(-21.3315077354905,15.2189704414799,
-6.67669464777756));
#114936=CARTESIAN_POINT('Ctrl Pts',(-21.3274702411173,15.2127748193448,
-6.59067051003166));
#114937=CARTESIAN_POINT('Ctrl Pts',(-21.3234327467442,15.204403268655,-6.50486586282613));
#114938=CARTESIAN_POINT('Ctrl Pts',(-21.3165507415352,15.190133761349,-6.35860980041302));
#114939=CARTESIAN_POINT('Ctrl Pts',(-21.3096687363261,15.1695340759322,
-6.2129369909791));
#114940=CARTESIAN_POINT('Ctrl Pts',(-21.3027867311171,15.1426759370888,
-6.06840565491519));
#114941=CARTESIAN_POINT('Ctrl Pts',(-21.2959062311046,15.1158236725188,
-5.92390592999837));
#114942=CARTESIAN_POINT('Ctrl Pts',(-21.2890257310922,15.0827157467963,
-5.78054751496072));
#114943=CARTESIAN_POINT('Ctrl Pts',(-21.2821452310798,15.043475218225,-5.63887966929049));
#114944=CARTESIAN_POINT('Ctrl Pts',(-21.2752642995611,15.0042322287083,
-5.49720293900956));
#114945=CARTESIAN_POINT('Ctrl Pts',(-21.2683833680424,14.9588559542226,
-5.35721731924835));
#114946=CARTESIAN_POINT('Ctrl Pts',(-21.2615024365237,14.9075198065233,
-5.21945858557822));
#114947=CARTESIAN_POINT('Ctrl Pts',(-21.2546216674167,14.8561848705188,
-5.08170310344812));
#114948=CARTESIAN_POINT('Ctrl Pts',(-21.2477408983096,14.7988904640697,
-4.94617472034563));
#114949=CARTESIAN_POINT('Ctrl Pts',(-21.2408601292026,14.7358587467217,
-4.81339073072018));
#114950=CARTESIAN_POINT('Ctrl Pts',(-21.2339770585298,14.672805945736,-4.68056232584397));
#114951=CARTESIAN_POINT('Ctrl Pts',(-21.227093987857,14.6040121460503,-4.5504804560366));
#114952=CARTESIAN_POINT('Ctrl Pts',(-21.2202109171841,14.52974648257,-4.4236397975768));
#114953=CARTESIAN_POINT('Ctrl Pts',(-21.2158363120681,14.4825461897285,
-4.34302493543258));
#114954=CARTESIAN_POINT('Ctrl Pts',(-21.2114617069521,14.433136544005,-4.2637188372088));
#114955=CARTESIAN_POINT('Ctrl Pts',(-21.2070871018361,14.3815959889042,
-4.1858428080249));
#114956=CARTESIAN_POINT('Ctrl Pts',(-21.2015511135273,14.3163722937598,
-4.08729201871722));
#114957=CARTESIAN_POINT('Ctrl Pts',(-21.1960151252186,14.2477191097718,
-3.99100671202062));
#114958=CARTESIAN_POINT('Ctrl Pts',(-21.1904791369099,14.1758012177496,
-3.89721939943572));
#114959=CARTESIAN_POINT('Ctrl Pts',(-22.6904763727661,14.1758012177496,
-3.89721939943571));
#114960=CARTESIAN_POINT('Ctrl Pts',(-22.6832062450968,14.0813083024994,
-3.77399225344413));
#114961=CARTESIAN_POINT('Ctrl Pts',(-22.6759361174275,13.9811735843942,
-3.6550738601199));
#114962=CARTESIAN_POINT('Ctrl Pts',(-22.6686659897582,13.8758194560258,
-3.54096956743624));
#114963=CARTESIAN_POINT('Ctrl Pts',(-22.6617335870542,13.7753594259407,
-3.43216585130876));
#114964=CARTESIAN_POINT('Ctrl Pts',(-22.6548011843501,13.6701542043166,
-3.32773932770549));
#114965=CARTESIAN_POINT('Ctrl Pts',(-22.6478687816461,13.5606093910262,
-3.22809208134504));
#114966=CARTESIAN_POINT('Ctrl Pts',(-22.6409364784718,13.4510661504903,
-3.12844626563806));
#114967=CARTESIAN_POINT('Ctrl Pts',(-22.6340041752975,13.3371836892631,
-3.03357981027087));
#114968=CARTESIAN_POINT('Ctrl Pts',(-22.6270718721233,13.2194024606833,
-2.94385604502711));
#114969=CARTESIAN_POINT('Ctrl Pts',(-22.6201382182847,13.101598284045,-2.85411479833708));
#114970=CARTESIAN_POINT('Ctrl Pts',(-22.6132045644461,12.9798940866522,
-2.7695184421809));
#114971=CARTESIAN_POINT('Ctrl Pts',(-22.6062709106076,12.8547616201541,
-2.69038863681246));
#114972=CARTESIAN_POINT('Ctrl Pts',(-22.6052588873165,12.8364975167663,
-2.67883899676501));
#114973=CARTESIAN_POINT('Ctrl Pts',(-22.6042468640255,12.8181604280522,
-2.66740573923635));
#114974=CARTESIAN_POINT('Ctrl Pts',(-22.6032348407344,12.7997518707891,
-2.65608978608592));
#114975=CARTESIAN_POINT('Ctrl Pts',(-22.5963013561296,12.6736327888376,
-2.57856292711801));
#114976=CARTESIAN_POINT('Ctrl Pts',(-22.5893678715248,12.5441133362429,
-2.50651890621843));
#114977=CARTESIAN_POINT('Ctrl Pts',(-22.5824343869199,12.4116897238054,
-2.4402400211681));
#114978=CARTESIAN_POINT('Ctrl Pts',(-22.5755022202333,12.2792912824762,
-2.37397373442229));
#114979=CARTESIAN_POINT('Ctrl Pts',(-22.5685700535467,12.1439900781449,
-2.31347054505179));
#114980=CARTESIAN_POINT('Ctrl Pts',(-22.5616378868601,12.0063060236781,
-2.25896634166286));
#114981=CARTESIAN_POINT('Ctrl Pts',(-22.5547054768533,11.8686171364782,
-2.20446022516737));
#114982=CARTESIAN_POINT('Ctrl Pts',(-22.5477730668465,11.7285455379248,
-2.15595364079637));
#114983=CARTESIAN_POINT('Ctrl Pts',(-22.5408406568397,11.5866306909856,
-2.11363415723017));
#114984=CARTESIAN_POINT('Ctrl Pts',(-22.5339086222827,11.4447235299589,
-2.07131696562884));
#114985=CARTESIAN_POINT('Ctrl Pts',(-22.5269765877257,11.3009736373842,
-2.03518629791231));
#114986=CARTESIAN_POINT('Ctrl Pts',(-22.5200445531686,11.155935203683,-2.00537971687135));
#114987=CARTESIAN_POINT('Ctrl Pts',(-22.5131109767612,11.0108645099633,
-1.97556650613346));
#114988=CARTESIAN_POINT('Ctrl Pts',(-22.5061774003538,10.8645050263921,
-1.9520802592744));
#114989=CARTESIAN_POINT('Ctrl Pts',(-22.4992438239464,10.7174213194626,
-1.93500745093131));
#114990=CARTESIAN_POINT('Ctrl Pts',(-22.495125614573,10.6300607042532,-1.92486702768973));
#114991=CARTESIAN_POINT('Ctrl Pts',(-22.4910074051996,10.5424447657293,
-1.91698814828052));
#114992=CARTESIAN_POINT('Ctrl Pts',(-22.4868891958262,10.4546927511912,
-1.9113802780545));
#114993=CARTESIAN_POINT('Ctrl Pts',(-22.4799556232166,10.3069501501543,
-1.90193865625436));
#114994=CARTESIAN_POINT('Ctrl Pts',(-22.4730220506069,10.158770604134,-1.89893406224141));
#114995=CARTESIAN_POINT('Ctrl Pts',(-22.4660884779973,10.0107247644674,
-1.90238355273524));
#114996=CARTESIAN_POINT('Ctrl Pts',(-22.4591562216396,9.86270702945001,
-1.90583238838649));
#114997=CARTESIAN_POINT('Ctrl Pts',(-22.4522239652819,9.71482328045241,
-1.91573285633567));
#114998=CARTESIAN_POINT('Ctrl Pts',(-22.4452917089242,9.56764337792384,
-1.93204990787901));
#114999=CARTESIAN_POINT('Ctrl Pts',(-22.4383592076211,9.420458274917,-1.94836753597166));
#115000=CARTESIAN_POINT('Ctrl Pts',(-22.4314267063179,9.27397739706878,
-1.97110216823797));
#115001=CARTESIAN_POINT('Ctrl Pts',(-22.4244942050148,9.12876525084503,
-2.00016690660241));
#115002=CARTESIAN_POINT('Ctrl Pts',(-22.41756207846,8.98356095431581,-2.02923007382199));
#115003=CARTESIAN_POINT('Ctrl Pts',(-22.4106299519053,8.83962557614821,
-2.06462259662998));
#115004=CARTESIAN_POINT('Ctrl Pts',(-22.4036978253505,8.69751321817358,
-2.10620649631859));
#115005=CARTESIAN_POINT('Ctrl Pts',(-22.3967641566674,8.55536924572963,
-2.14779964680663));
#115006=CARTESIAN_POINT('Ctrl Pts',(-22.3898304879842,8.41504942121115,
-2.19558683341147));
#115007=CARTESIAN_POINT('Ctrl Pts',(-22.3828968193011,8.27709309039585,
-2.24938007821602));
#115008=CARTESIAN_POINT('Ctrl Pts',(-22.3787790631734,8.19516380410787,
-2.28132672486794));
#115009=CARTESIAN_POINT('Ctrl Pts',(-22.3746613070457,8.11406779091711,
-2.31539071346896));
#115010=CARTESIAN_POINT('Ctrl Pts',(-22.370543550918,8.03391480971792,-2.35152458215918));
#115011=CARTESIAN_POINT('Ctrl Pts',(-22.3636099925257,7.89895165060084,
-2.41236749775123));
#115012=CARTESIAN_POINT('Ctrl Pts',(-22.3566764341333,7.76661674914673,
-2.47910262080128));
#115013=CARTESIAN_POINT('Ctrl Pts',(-22.3497428757409,7.63742230671767,
-2.55147779924112));
#115014=CARTESIAN_POINT('Ctrl Pts',(-22.3428106342854,7.5082524030468,-2.62383923098281));
#115015=CARTESIAN_POINT('Ctrl Pts',(-22.3358783928298,7.3822220565691,-2.70183841932422));
#115016=CARTESIAN_POINT('Ctrl Pts',(-22.3289461513742,7.25981836998035,
-2.78517754320212));
#115017=CARTESIAN_POINT('Ctrl Pts',(-22.322013665852,7.13741037386829,-2.86851960123916));
#115018=CARTESIAN_POINT('Ctrl Pts',(-22.3150811803298,7.01862956828097,
-2.95720178773977));
#115019=CARTESIAN_POINT('Ctrl Pts',(-22.3081486948075,6.90393404520842,
-3.05088297574135));
#115020=CARTESIAN_POINT('Ctrl Pts',(-22.3012165844928,6.78924472981139,
-3.14455909342806));
#115021=CARTESIAN_POINT('Ctrl Pts',(-22.2942844741781,6.67864050993959,
-3.24323346137456));
#115022=CARTESIAN_POINT('Ctrl Pts',(-22.2873523638634,6.5725463642529,-3.34652469104477));
#115023=CARTESIAN_POINT('Ctrl Pts',(-22.2804187119845,6.4664286253275,-3.44983889064064));
#115024=CARTESIAN_POINT('Ctrl Pts',(-22.2734850601056,6.36482320156598,
-3.55777177275135));
#115025=CARTESIAN_POINT('Ctrl Pts',(-22.2665514082267,6.2681186198229,-3.66990468052016));
#115026=CARTESIAN_POINT('Ctrl Pts',(-22.2624335741544,6.21068663035953,
-3.73649941534445));
#115027=CARTESIAN_POINT('Ctrl Pts',(-22.2583157400821,6.15498248326484,
-3.80457483855878));
#115028=CARTESIAN_POINT('Ctrl Pts',(-22.2541979060098,6.10108093818732,
-3.87403761020318));
#115029=CARTESIAN_POINT('Ctrl Pts',(-22.247264295271,6.01032149396891,-3.99099905424433));
#115030=CARTESIAN_POINT('Ctrl Pts',(-22.2403306845322,5.92464363472474,
-4.11193600283431));
#115031=CARTESIAN_POINT('Ctrl Pts',(-22.2333970737934,5.84438185374589,
-4.23638579525945));
#115032=CARTESIAN_POINT('Ctrl Pts',(-22.2264647793601,5.76413530999738,
-4.36081196161838));
#115033=CARTESIAN_POINT('Ctrl Pts',(-22.2195324849268,5.68930297214713,
-4.48874936360589));
#115034=CARTESIAN_POINT('Ctrl Pts',(-22.2126001904935,5.62017577060433,
-4.61970674197797));
#115035=CARTESIAN_POINT('Ctrl Pts',(-22.2056676515668,5.55104613103073,
-4.75066873905461));
#115036=CARTESIAN_POINT('Ctrl Pts',(-22.1987351126401,5.48762218766616,
-4.88465063487431));
#115037=CARTESIAN_POINT('Ctrl Pts',(-22.1918025737133,5.43014895812622,
-5.02113649150837));
#115038=CARTESIAN_POINT('Ctrl Pts',(-22.1848704098817,5.37267883825905,
-5.15761496337642));
#115039=CARTESIAN_POINT('Ctrl Pts',(-22.1779382460501,5.3211589153847,-5.2965968199325));
#115040=CARTESIAN_POINT('Ctrl Pts',(-22.1710060822185,5.27578609499789,
-5.43754605559421));
#115041=CARTESIAN_POINT('Ctrl Pts',(-22.1640723771204,5.23040318662025,
-5.57852662928132));
#115042=CARTESIAN_POINT('Ctrl Pts',(-22.1571386720224,5.19117021294783,
-5.72147514131237));
#115043=CARTESIAN_POINT('Ctrl Pts',(-22.1502049669243,5.15823441927751,
-5.8658397265272));
#115044=CARTESIAN_POINT('Ctrl Pts',(-22.1460873983168,5.13867555599091,
-5.95157038217522));
#115045=CARTESIAN_POINT('Ctrl Pts',(-22.1419698297092,5.12133647341795,
-6.03780015164788));
#115046=CARTESIAN_POINT('Ctrl Pts',(-22.1378522611016,5.10623951371014,
-6.12441157677879));
#115047=CARTESIAN_POINT('Ctrl Pts',(-22.1309189485113,5.08081870089726,
-6.27025106157069));
#115048=CARTESIAN_POINT('Ctrl Pts',(-22.123985635921,5.06174897458694,-6.41722355017293));
#115049=CARTESIAN_POINT('Ctrl Pts',(-22.1170523233307,5.04910923496427,
-6.56476365668796));
#115050=CARTESIAN_POINT('Ctrl Pts',(-22.1101203285711,5.03647189780609,
-6.71227571991427));
#115051=CARTESIAN_POINT('Ctrl Pts',(-22.1031883338116,5.03026213714831,
-6.86035485655776));
#115052=CARTESIAN_POINT('Ctrl Pts',(-22.096256339052,5.03050696985794,-7.00843081032554));
#115053=CARTESIAN_POINT('Ctrl Pts',(-22.0893240991684,5.03075181122517,
-7.15651200024495));
#115054=CARTESIAN_POINT('Ctrl Pts',(-22.0823918592848,5.03745170547963,
-7.30458967643834));
#115055=CARTESIAN_POINT('Ctrl Pts',(-22.0754596194012,5.05058154531326,
-7.45209327648446));
#115056=CARTESIAN_POINT('Ctrl Pts',(-22.0685277535374,5.0637106767437,-7.5995889181684));
#115057=CARTESIAN_POINT('Ctrl Pts',(-22.0615958876737,5.08326902931621,
-7.74651021643196));
#115058=CARTESIAN_POINT('Ctrl Pts',(-22.0546640218099,5.10917958752434,
-7.89229140760191));
#115059=CARTESIAN_POINT('Ctrl Pts',(-22.0477306104145,5.13509592276128,
-8.03810510220675));
#115060=CARTESIAN_POINT('Ctrl Pts',(-22.0407971990191,5.16736723568739,
-8.18277785615135));
#115061=CARTESIAN_POINT('Ctrl Pts',(-22.0338637876236,5.20586520532844,
-8.32575314772379));
#115062=CARTESIAN_POINT('Ctrl Pts',(-22.0297447304802,5.22873639063859,
-8.41069306582378));
#115063=CARTESIAN_POINT('Ctrl Pts',(-22.0256256733368,5.25380424364472,
-8.49503408736322));
#115064=CARTESIAN_POINT('Ctrl Pts',(-22.0215066161934,5.28103345893842,
-8.57866183845887));
#115065=CARTESIAN_POINT('Ctrl Pts',(-22.0145723772777,5.32687256185952,
-8.71944522307671));
#115066=CARTESIAN_POINT('Ctrl Pts',(-22.0076381383619,5.37885549112866,
-8.85825491842587));
#115067=CARTESIAN_POINT('Ctrl Pts',(-22.0007038994462,5.43678711804054,
-8.99455428792793));
#115068=CARTESIAN_POINT('Ctrl Pts',(-21.993770974864,5.49470776444206,-9.1308278228951));
#115069=CARTESIAN_POINT('Ctrl Pts',(-21.9868380502819,5.55857472969261,
-9.26459167738601));
#115070=CARTESIAN_POINT('Ctrl Pts',(-21.9799051256997,5.62814476255884,
-9.39532921043455));
#115071=CARTESIAN_POINT('Ctrl Pts',(-21.9729719597937,5.69771721704527,
-9.52607129424495));
#115072=CARTESIAN_POINT('Ctrl Pts',(-21.9660387938876,5.77299298410511,
-9.65378655254162));
#115073=CARTESIAN_POINT('Ctrl Pts',(-21.9591056279816,5.85368261440674,
-9.77798248465653));
#115074=CARTESIAN_POINT('Ctrl Pts',(-21.9521728404709,5.93436784086443,
-9.90217163845925));
#115075=CARTESIAN_POINT('Ctrl Pts',(-21.9452400529602,6.02046615852026,
-10.0228415738131));
#115076=CARTESIAN_POINT('Ctrl Pts',(-21.9383072654495,6.11164450011518,
-10.1395283375127));
#115077=CARTESIAN_POINT('Ctrl Pts',(-21.9313729472104,6.20284297347965,
-10.2562408651272));
#115078=CARTESIAN_POINT('Ctrl Pts',(-21.9244386289712,6.29912350845597,
-10.3689682033144));
#115079=CARTESIAN_POINT('Ctrl Pts',(-21.9175043107321,6.40011203297749,
-10.4772785898498));
#115080=CARTESIAN_POINT('Ctrl Pts',(-21.9133898642498,6.4600331189647,-10.5415440696718));
#115081=CARTESIAN_POINT('Ctrl Pts',(-21.9092754177675,6.5216109328709,-10.6042551600696));
#115082=CARTESIAN_POINT('Ctrl Pts',(-21.9051609712852,6.58476102287579,
-10.6653276230177));
#115083=CARTESIAN_POINT('Ctrl Pts',(-21.8982288574645,6.69115774320861,
-10.7682239096234));
#115084=CARTESIAN_POINT('Ctrl Pts',(-21.8912967436438,6.80205628720019,
-10.8665022681371));
#115085=CARTESIAN_POINT('Ctrl Pts',(-21.8843646298231,6.91703324183498,
-10.959780085773));
#115086=CARTESIAN_POINT('Ctrl Pts',(-21.8774338365917,7.0319882930012,-11.0530401336937));
#115087=CARTESIAN_POINT('Ctrl Pts',(-21.8705030433603,7.15101994789269,
-11.1413013330034));
#115088=CARTESIAN_POINT('Ctrl Pts',(-21.863572250129,7.27367163221487,-11.2242212695068));
#115089=CARTESIAN_POINT('Ctrl Pts',(-21.8566412042781,7.39632778705076,
-11.3071442283471));
#115090=CARTESIAN_POINT('Ctrl Pts',(-21.8497101584272,7.52260396312254,
-11.3847253467466));
#115091=CARTESIAN_POINT('Ctrl Pts',(-21.8427791125763,7.65201406730398,
-11.4566651717729));
#115092=CARTESIAN_POINT('Ctrl Pts',(-21.8358484336565,7.78141732048679,
-11.5286011882895));
#115093=CARTESIAN_POINT('Ctrl Pts',(-21.8289177547367,7.91395388012075,
-11.5948963491388));
#115094=CARTESIAN_POINT('Ctrl Pts',(-21.8219870758168,8.04911248293015,
-11.6552968518474));
#115095=CARTESIAN_POINT('Ctrl Pts',(-21.8150548300911,8.18430164079854,
-11.7157110091875));
#115096=CARTESIAN_POINT('Ctrl Pts',(-21.8081225843653,8.32211372406473,
-11.7702277106694));
#115097=CARTESIAN_POINT('Ctrl Pts',(-21.8011903386395,8.46201631468121,
-11.8186407999762));
#115098=CARTESIAN_POINT('Ctrl Pts',(-21.797065334552,8.54526477138227,-11.8474488081137));
#115099=CARTESIAN_POINT('Ctrl Pts',(-21.7929403304645,8.62925305861412,
-11.8740965742915));
#115100=CARTESIAN_POINT('Ctrl Pts',(-21.788815326377,8.71386618713863,-11.898548959425));
#115101=CARTESIAN_POINT('Ctrl Pts',(-21.7818417513357,8.85690992448683,
-11.939887231837));
#115102=CARTESIAN_POINT('Ctrl Pts',(-21.7748681762943,9.00178738562049,
-11.9749620552806));
#115103=CARTESIAN_POINT('Ctrl Pts',(-21.7678946012529,9.14793866626696,
-12.0036325152953));
#115104=CARTESIAN_POINT('Ctrl Pts',(-21.7609225553009,9.29405790045778,
-12.0322966887649));
#115105=CARTESIAN_POINT('Ctrl Pts',(-21.7539505093488,9.44145008039454,
-12.0545592393556));
#115106=CARTESIAN_POINT('Ctrl Pts',(-21.7469784633968,9.58954487878361,
-12.0703303114365));
#115107=CARTESIAN_POINT('Ctrl Pts',(-21.740007262077,9.73762173614916,-12.0860994729225));
#115108=CARTESIAN_POINT('Ctrl Pts',(-21.7330360607571,9.88640072158192,
-12.0953786905622));
#115109=CARTESIAN_POINT('Ctrl Pts',(-21.7260648594373,10.0353056921974,
-12.0981298955968));
#115110=CARTESIAN_POINT('Ctrl Pts',(-21.7245944077477,10.0667145635801,
-12.0987102136662));
#115111=CARTESIAN_POINT('Ctrl Pts',(-21.723123956058,10.0981290288572,-12.0990002688469));
#115112=CARTESIAN_POINT('Ctrl Pts',(-21.7216535043684,10.1295436676547,
-12.098999999813));
#115113=CARTESIAN_POINT('Origin',(11.,-13.5,-22.));
#115114=CARTESIAN_POINT('',(7.,-13.5,-22.));
#115115=CARTESIAN_POINT('Origin',(11.,-13.5,-22.));
#115116=CARTESIAN_POINT('',(7.,-13.5,-16.));
#115117=CARTESIAN_POINT('',(7.,-13.5,-22.));
#115118=CARTESIAN_POINT('Origin',(11.,-13.5,-16.));
#115119=CARTESIAN_POINT('Origin',(2.22044604925031E-15,2.25,-16.));
#115120=CARTESIAN_POINT('Origin',(11.,17.5,-22.));
#115121=CARTESIAN_POINT('',(6.55407155365721,16.8045,-22.));
#115122=CARTESIAN_POINT('',(9.25758668237251,21.6489752747581,-22.));
#115123=CARTESIAN_POINT('Origin',(11.,17.5,-22.));
#115124=CARTESIAN_POINT('',(6.55407155365721,16.8045,-16.));
#115125=CARTESIAN_POINT('',(6.55407155365721,16.8045,-22.));
#115126=CARTESIAN_POINT('',(9.25758668237251,21.6489752747581,-16.));
#115127=CARTESIAN_POINT('Origin',(11.,17.5,-16.));
#115128=CARTESIAN_POINT('',(9.25758668237251,21.6489752747581,-22.));
#115129=CARTESIAN_POINT('Origin',(2.22044604925031E-15,2.25,-16.));
#115130=CARTESIAN_POINT('',(9.25758668237251,21.5062266006623,-16.));
#115131=CARTESIAN_POINT('',(9.25758668237251,11.8781133003311,-16.));
#115132=CARTESIAN_POINT('',(7.0995,16.8045,-16.));
#115133=CARTESIAN_POINT('',(-3.54975,16.8045,-16.));
#115134=CARTESIAN_POINT('',(7.0995,19.4175,-16.));
#115135=CARTESIAN_POINT('',(7.0995,9.52725,-16.));
#115136=CARTESIAN_POINT('Origin',(10.7505,17.8045,-16.));
#115137=CARTESIAN_POINT('Origin',(-11.,-13.5,-22.));
#115138=CARTESIAN_POINT('',(-15.,-13.5,-22.));
#115139=CARTESIAN_POINT('Origin',(-11.,-13.5,-22.));
#115140=CARTESIAN_POINT('',(-15.,-13.5,-16.));
#115141=CARTESIAN_POINT('',(-15.,-13.5,-22.));
#115142=CARTESIAN_POINT('Origin',(-11.,-13.5,-16.));
#115143=CARTESIAN_POINT('Origin',(2.22044604925031E-15,2.25,-16.));
#115144=CARTESIAN_POINT('Origin',(-11.,17.5,-22.));
#115145=CARTESIAN_POINT('',(-9.25758668237251,21.6489752747581,-22.));
#115146=CARTESIAN_POINT('',(-6.55407155365721,16.8045,-22.));
#115147=CARTESIAN_POINT('Origin',(-11.,17.5,-22.));
#115148=CARTESIAN_POINT('',(-9.25758668237251,21.6489752747581,-16.));
#115149=CARTESIAN_POINT('',(-9.25758668237251,21.6489752747581,-22.));
#115150=CARTESIAN_POINT('',(-6.55407155365721,16.8045,-16.));
#115151=CARTESIAN_POINT('Origin',(-11.,17.5,-16.));
#115152=CARTESIAN_POINT('',(-6.55407155365721,16.8045,-22.));
#115153=CARTESIAN_POINT('Origin',(2.22044604925031E-15,2.25,-16.));
#115154=CARTESIAN_POINT('',(-7.0995,16.8045,-16.));
#115155=CARTESIAN_POINT('',(-7.0995,19.4175,-16.));
#115156=CARTESIAN_POINT('',(-7.0995,10.83375,-16.));
#115157=CARTESIAN_POINT('',(-3.54975,16.8045,-16.));
#115158=CARTESIAN_POINT('',(-9.25758668237251,21.5062266006622,-16.));
#115159=CARTESIAN_POINT('',(-9.25758668237251,13.2726133003311,-16.));
#115160=CARTESIAN_POINT('Origin',(-10.7505,17.8045,-16.));
#115161=CARTESIAN_POINT('Origin',(1.5089639216641E-15,6.00000008940697,
-22.));
#115162=CARTESIAN_POINT('',(-5.,6.00000008940697,-22.));
#115163=CARTESIAN_POINT('Origin',(1.5089639216641E-15,6.00000008940697,
-22.));
#115164=CARTESIAN_POINT('',(-5.,6.00000008940697,-16.));
#115165=CARTESIAN_POINT('',(-5.,6.00000008940697,-22.));
#115166=CARTESIAN_POINT('Origin',(1.5089639216641E-15,6.00000008940697,
-16.));
#115167=CARTESIAN_POINT('Origin',(2.22044604925031E-15,2.25,-16.));
#115168=CARTESIAN_POINT('Origin',(7.0995,16.8045,0.));
#115169=CARTESIAN_POINT('',(7.0995,16.8045,0.));
#115170=CARTESIAN_POINT('',(7.0995,16.8045,0.));
#115171=CARTESIAN_POINT('',(7.0995,19.4175,0.));
#115172=CARTESIAN_POINT('',(7.0995,16.8045,0.));
#115173=CARTESIAN_POINT('',(7.0995,19.4175,0.));
#115174=CARTESIAN_POINT('Origin',(-9.25758668237251,24.2952266006623,0.));
#115175=CARTESIAN_POINT('',(-9.25758668237251,24.2952266006623,-22.));
#115176=CARTESIAN_POINT('',(-9.25758668237251,21.5062266006623,-22.));
#115177=CARTESIAN_POINT('',(-9.25758668237251,24.2952266006623,0.));
#115178=CARTESIAN_POINT('',(-9.25758668237251,24.2952266006623,0.));
#115179=CARTESIAN_POINT('',(-9.25758668237251,21.5062266006623,0.));
#115180=CARTESIAN_POINT('',(-9.25758668237251,21.5062266006623,0.));
#115181=CARTESIAN_POINT('',(-9.25758668237251,21.5062266006623,0.));
#115182=CARTESIAN_POINT('Origin',(-7.0995,16.8045,0.));
#115183=CARTESIAN_POINT('',(7.0995,16.8045,-22.));
#115184=CARTESIAN_POINT('',(-7.0995,16.8045,0.));
#115185=CARTESIAN_POINT('',(-7.0995,16.8045,0.));
#115186=CARTESIAN_POINT('',(7.0995,16.8045,0.));
#115187=CARTESIAN_POINT('Origin',(0.,1.05261330033112,-22.));
#115188=CARTESIAN_POINT('',(9.25758668237251,24.2952266006623,-22.));
#115189=CARTESIAN_POINT('',(9.25758668237251,21.5062266006623,-22.));
#115190=CARTESIAN_POINT('',(9.06658668237251,24.4862266006622,-22.));
#115191=CARTESIAN_POINT('Origin',(9.06658668237251,24.2952266006623,-22.));
#115192=CARTESIAN_POINT('',(7.30158668237251,24.4862266006622,-22.));
#115193=CARTESIAN_POINT('',(9.06658668237251,24.4862266006622,-22.));
#115194=CARTESIAN_POINT('',(7.11058668237251,24.6772266006623,-22.));
#115195=CARTESIAN_POINT('Origin',(7.30158668237251,24.6772266006623,-22.));
#115196=CARTESIAN_POINT('',(7.11058668237251,25.8032266006622,-22.));
#115197=CARTESIAN_POINT('',(7.11058668237251,24.6772266006623,-22.));
#115198=CARTESIAN_POINT('',(7.36458668237251,26.0572266006622,-22.));
#115199=CARTESIAN_POINT('Origin',(7.36458668237251,25.8032266006622,-22.));
#115200=CARTESIAN_POINT('',(18.734,24.211,-22.));
#115201=CARTESIAN_POINT('',(7.36458668237251,26.0572266006622,-22.));
#115202=CARTESIAN_POINT('',(23.734,19.211,-22.));
#115203=CARTESIAN_POINT('Origin',(18.734,19.211,-22.));
#115204=CARTESIAN_POINT('',(23.734,6.1295,-22.));
#115205=CARTESIAN_POINT('',(23.734,19.211,-22.));
#115206=CARTESIAN_POINT('',(23.534,6.1295,-22.));
#115207=CARTESIAN_POINT('',(11.867,6.1295,-22.));
#115208=CARTESIAN_POINT('',(23.534,-5.8705,-22.));
#115209=CARTESIAN_POINT('',(23.534,0.591056650165565,-22.));
#115210=CARTESIAN_POINT('',(23.734,-5.8705,-22.));
#115211=CARTESIAN_POINT('',(11.867,-5.8705,-22.));
#115212=CARTESIAN_POINT('',(23.734,-18.952,-22.));
#115213=CARTESIAN_POINT('',(23.734,19.211,-22.));
#115214=CARTESIAN_POINT('',(18.734,-23.952,-22.));
#115215=CARTESIAN_POINT('Origin',(18.734,-18.952,-22.));
#115216=CARTESIAN_POINT('',(-18.734,-23.952,-22.));
#115217=CARTESIAN_POINT('',(-18.734,-23.952,-22.));
#115218=CARTESIAN_POINT('',(-23.734,-18.952,-22.));
#115219=CARTESIAN_POINT('Origin',(-18.734,-18.952,-22.));
#115220=CARTESIAN_POINT('',(-23.734,-5.8705,-22.));
#115221=CARTESIAN_POINT('',(-23.734,19.211,-22.));
#115222=CARTESIAN_POINT('',(-23.534,-5.8705,-22.));
#115223=CARTESIAN_POINT('',(-11.867,-5.8705,-22.));
#115224=CARTESIAN_POINT('',(-23.534,6.1295,-22.));
#115225=CARTESIAN_POINT('',(-23.534,0.591056650165565,-22.));
#115226=CARTESIAN_POINT('',(-23.734,6.1295,-22.));
#115227=CARTESIAN_POINT('',(-11.867,6.1295,-22.));
#115228=CARTESIAN_POINT('',(-23.734,19.211,-22.));
#115229=CARTESIAN_POINT('',(-23.734,19.211,-22.));
#115230=CARTESIAN_POINT('',(-18.734,24.211,-22.));
#115231=CARTESIAN_POINT('Origin',(-18.734,19.211,-22.));
#115232=CARTESIAN_POINT('',(-7.36458668237251,26.0572266006623,-22.));
#115233=CARTESIAN_POINT('',(-7.36458668237251,26.0572266006622,-22.));
#115234=CARTESIAN_POINT('',(-7.11058668237251,25.8032266006623,-22.));
#115235=CARTESIAN_POINT('Origin',(-7.36458668237251,25.8032266006623,-22.));
#115236=CARTESIAN_POINT('',(-7.11058668237251,24.6772266006623,-22.));
#115237=CARTESIAN_POINT('',(-7.11058668237251,24.6772266006623,-22.));
#115238=CARTESIAN_POINT('',(-7.30158668237251,24.4862266006622,-22.));
#115239=CARTESIAN_POINT('Origin',(-7.30158668237251,24.6772266006623,-22.));
#115240=CARTESIAN_POINT('',(-9.06658668237251,24.4862266006622,-22.));
#115241=CARTESIAN_POINT('',(-9.06658668237251,24.4862266006622,-22.));
#115242=CARTESIAN_POINT('Origin',(-9.06658668237251,24.2952266006623,-22.));
#115243=CARTESIAN_POINT('',(-21.234,0.12950000000008,-22.));
#115244=CARTESIAN_POINT('Origin',(-18.734,0.12950000000008,-22.));
#115245=CARTESIAN_POINT('',(16.234,0.12950000000008,-22.));
#115246=CARTESIAN_POINT('Origin',(18.734,0.12950000000008,-22.));
#115247=CARTESIAN_POINT('Ctrl Pts',(-17.1140743056112,17.8480877707428,
-22.));
#115248=CARTESIAN_POINT('Ctrl Pts',(-17.0603911270984,17.8998883320905,
-22.));
#115249=CARTESIAN_POINT('Ctrl Pts',(-17.0098645090452,17.954561484389,-22.));
#115250=CARTESIAN_POINT('Ctrl Pts',(-16.9624881824911,18.0117359214698,
-22.));
#115251=CARTESIAN_POINT('Ctrl Pts',(-16.9134245435091,18.0709466316275,
-22.));
#115252=CARTESIAN_POINT('Ctrl Pts',(-16.8677390829668,18.1328404012573,
-22.));
#115253=CARTESIAN_POINT('Ctrl Pts',(-16.8254531772989,18.1970544303157,
-22.));
#115254=CARTESIAN_POINT('Ctrl Pts',(-16.7853186877899,18.2580013873422,
-22.));
#115255=CARTESIAN_POINT('Ctrl Pts',(-16.7482465752162,18.3210394463055,
-22.));
#115256=CARTESIAN_POINT('Ctrl Pts',(-16.7142835835435,18.3858911656733,
-22.));
#115257=CARTESIAN_POINT('Ctrl Pts',(-16.6991852702862,18.414721122225,-22.));
#115258=CARTESIAN_POINT('Ctrl Pts',(-16.6847017945038,18.443909871674,-22.));
#115259=CARTESIAN_POINT('Ctrl Pts',(-16.6708392558117,18.4734345779294,
-22.));
#115260=CARTESIAN_POINT('Ctrl Pts',(-16.6640109132328,18.4879777156138,
-22.));
#115261=CARTESIAN_POINT('Ctrl Pts',(-16.6573332485221,18.5026023792008,
-22.));
#115262=CARTESIAN_POINT('Ctrl Pts',(-16.6508071085471,18.5173059065043,
-22.));
#115263=CARTESIAN_POINT('Ctrl Pts',(-16.6447949281281,18.53085147238,-22.));
#115264=CARTESIAN_POINT('Ctrl Pts',(-16.638910878667,18.5444653615358,-22.));
#115265=CARTESIAN_POINT('Ctrl Pts',(-16.6331635636444,18.5581259521741,
-22.));
#115266=CARTESIAN_POINT('Ctrl Pts',(-16.6020947551997,18.6319723086221,
-22.));
#115267=CARTESIAN_POINT('Ctrl Pts',(-16.5749611536668,18.7073070289839,
-22.));
#115268=CARTESIAN_POINT('Ctrl Pts',(-16.5517843887068,18.7837489743025,
-22.));
#115269=CARTESIAN_POINT('Ctrl Pts',(-16.5281812491805,18.8615971944543,
-22.));
#115270=CARTESIAN_POINT('Ctrl Pts',(-16.5086813563681,18.9405945618165,
-22.));
#115271=CARTESIAN_POINT('Ctrl Pts',(-16.4933484509613,19.0203740751675,
-22.));
#115272=CARTESIAN_POINT('Ctrl Pts',(-16.4794162132308,19.0928656947625,
-22.));
#115273=CARTESIAN_POINT('Ctrl Pts',(-16.4689246908346,19.1660040425392,
-22.));
#115274=CARTESIAN_POINT('Ctrl Pts',(-16.461955492605,19.2395296145576,-22.));
#115275=CARTESIAN_POINT('Ctrl Pts',(-16.4592975702873,19.2675708974063,
-22.));
#115276=CARTESIAN_POINT('Ctrl Pts',(-16.4571523310073,19.2956686091404,
-22.));
#115277=CARTESIAN_POINT('Ctrl Pts',(-16.4555256621827,19.3238086400899,
-22.));
#115278=CARTESIAN_POINT('Ctrl Pts',(-16.4546321787531,19.3392651675542,
-22.));
#115279=CARTESIAN_POINT('Ctrl Pts',(-16.4538951614737,19.3547344644167,
-22.));
#115280=CARTESIAN_POINT('Ctrl Pts',(-16.4533156881431,19.3702141998337,
-22.));
#115281=CARTESIAN_POINT('Ctrl Pts',(-16.4528679850542,19.3821738966753,
-22.));
#115282=CARTESIAN_POINT('Ctrl Pts',(-16.4525144924858,19.3941365263619,
-22.));
#115283=CARTESIAN_POINT('Ctrl Pts',(-16.452255631388,19.4060924704157,-22.));
#115284=CARTESIAN_POINT('Ctrl Pts',(-16.4504487968614,19.4895442238956,
-22.));
#115285=CARTESIAN_POINT('Ctrl Pts',(-16.4532437926239,19.5727897376045,
-22.));
#115286=CARTESIAN_POINT('Ctrl Pts',(-16.4606968610006,19.6554483758564,
-22.));
#115287=CARTESIAN_POINT('Ctrl Pts',(-16.4681356985408,19.7379491862844,
-22.));
#115288=CARTESIAN_POINT('Ctrl Pts',(-16.4802144629511,19.8198663642554,
-22.));
#115289=CARTESIAN_POINT('Ctrl Pts',(-16.4970384375915,19.9008370756969,
-22.));
#115290=CARTESIAN_POINT('Ctrl Pts',(-16.5135067566735,19.9800960820143,
-22.));
#115291=CARTESIAN_POINT('Ctrl Pts',(-16.5345215459181,20.058449172967,-22.));
#115292=CARTESIAN_POINT('Ctrl Pts',(-16.5598157066501,20.135668594405,-22.));
#115293=CARTESIAN_POINT('Ctrl Pts',(-16.5701726792029,20.1672869365532,
-22.));
#115294=CARTESIAN_POINT('Ctrl Pts',(-16.5812477391057,20.1987151389824,
-22.));
#115295=CARTESIAN_POINT('Ctrl Pts',(-16.5930250010084,20.2299370972628,
-22.));
#115296=CARTESIAN_POINT('Ctrl Pts',(-16.5995762661519,20.2473047442324,
-22.));
#115297=CARTESIAN_POINT('Ctrl Pts',(-16.6063470587533,20.2646137128558,
-22.));
#115298=CARTESIAN_POINT('Ctrl Pts',(-16.6133222512795,20.2818311531004,
-22.));
#115299=CARTESIAN_POINT('Ctrl Pts',(-16.644281419466,20.3582502091005,-22.));
#115300=CARTESIAN_POINT('Ctrl Pts',(-16.6792964912941,20.432962513728,-22.));
#115301=CARTESIAN_POINT('Ctrl Pts',(-16.7180394494849,20.5057444546798,
-22.));
#115302=CARTESIAN_POINT('Ctrl Pts',(-16.7588463546246,20.5824036954551,
-22.));
#115303=CARTESIAN_POINT('Ctrl Pts',(-16.8037889572456,20.6569222708542,
-22.));
#115304=CARTESIAN_POINT('Ctrl Pts',(-16.8525444691545,20.7290332608009,
-22.));
#115305=CARTESIAN_POINT('Ctrl Pts',(-16.9012999810635,20.8011442507477,
-22.));
#115306=CARTESIAN_POINT('Ctrl Pts',(-16.9538690009003,20.8708485410036,
-22.));
#115307=CARTESIAN_POINT('Ctrl Pts',(-17.0099819921104,20.9378605149736,
-22.));
#115308=CARTESIAN_POINT('Ctrl Pts',(-17.0318957015214,20.9640305852723,
-22.));
#115309=CARTESIAN_POINT('Ctrl Pts',(-17.0543504354563,20.9897897710343,
-22.));
#115310=CARTESIAN_POINT('Ctrl Pts',(-17.0773320398146,21.0151198306804,
-22.));
#115311=CARTESIAN_POINT('Ctrl Pts',(-17.08646379095,21.0251847416122,-22.));
#115312=CARTESIAN_POINT('Ctrl Pts',(-17.0956794941242,21.0351826951285,
-22.));
#115313=CARTESIAN_POINT('Ctrl Pts',(-17.1049759541041,21.045110003522,-22.));
#115314=CARTESIAN_POINT('Ctrl Pts',(-17.1654855277221,21.1097256958788,
-22.));
#115315=CARTESIAN_POINT('Ctrl Pts',(-17.2292148909452,21.171140300117,-22.));
#115316=CARTESIAN_POINT('Ctrl Pts',(-17.2958559579295,21.2290794537635,
-22.));
#115317=CARTESIAN_POINT('Ctrl Pts',(-17.3510488196551,21.2770652955339,
-22.));
#115318=CARTESIAN_POINT('Ctrl Pts',(-17.4082400388151,21.3226671775257,
-22.));
#115319=CARTESIAN_POINT('Ctrl Pts',(-17.4672777521355,21.3657152682276,
-22.));
#115320=CARTESIAN_POINT('Ctrl Pts',(-17.4867746843808,21.3799317014277,
-22.));
#115321=CARTESIAN_POINT('Ctrl Pts',(-17.5064731515178,21.3938694861353,
-22.));
#115322=CARTESIAN_POINT('Ctrl Pts',(-17.5263681121617,21.4075220975473,
-22.));
#115323=CARTESIAN_POINT('Ctrl Pts',(-17.542293137778,21.4184504019736,-22.));
#115324=CARTESIAN_POINT('Ctrl Pts',(-17.55834542777,21.429196741247,-22.));
#115325=CARTESIAN_POINT('Ctrl Pts',(-17.5745064519429,21.439747587913,-22.));
#115326=CARTESIAN_POINT('Ctrl Pts',(-17.6490342197562,21.4884036039023,
-22.));
#115327=CARTESIAN_POINT('Ctrl Pts',(-17.7259441256673,21.5329559340006,
-22.));
#115328=CARTESIAN_POINT('Ctrl Pts',(-17.8049553049308,21.5731139747841,
-22.));
#115329=CARTESIAN_POINT('Ctrl Pts',(-17.8827965257828,21.6126773751883,
-22.));
#115330=CARTESIAN_POINT('Ctrl Pts',(-17.9626779315913,21.6479763829434,
-22.));
#115331=CARTESIAN_POINT('Ctrl Pts',(-18.0443633906767,21.6786957524571,
-22.));
#115332=CARTESIAN_POINT('Ctrl Pts',(-18.0530581575347,21.6819655847986,
-22.));
#115333=CARTESIAN_POINT('Ctrl Pts',(-18.0617733892786,21.6851834888842,
-22.));
#115334=CARTESIAN_POINT('Ctrl Pts',(-18.070508670429,21.6883495949495,-22.));
#115335=CARTESIAN_POINT('Ctrl Pts',(-19.3957372685686,21.6839949024184,
-22.));
#115336=CARTESIAN_POINT('Ctrl Pts',(-19.477389057327,21.6544306829991,-22.));
#115337=CARTESIAN_POINT('Ctrl Pts',(-19.5571491338507,21.6204660242302,
-22.));
#115338=CARTESIAN_POINT('Ctrl Pts',(-19.6348154715244,21.5824187572536,
-22.));
#115339=CARTESIAN_POINT('Ctrl Pts',(-19.7143271161377,21.5434675093776,
-22.));
#115340=CARTESIAN_POINT('Ctrl Pts',(-19.7916450682551,21.5002366973253,
-22.));
#115341=CARTESIAN_POINT('Ctrl Pts',(-19.8665231148743,21.4530209100808,
-22.));
#115342=CARTESIAN_POINT('Ctrl Pts',(-19.9365885412315,21.4088398127707,
-22.));
#115343=CARTESIAN_POINT('Ctrl Pts',(-20.0045177600144,21.3611685582697,
-22.));
#115344=CARTESIAN_POINT('Ctrl Pts',(-20.0700782126376,21.3102210028104,
-22.));
#115345=CARTESIAN_POINT('Ctrl Pts',(-20.0997466183463,21.2871654459197,
-22.));
#115346=CARTESIAN_POINT('Ctrl Pts',(-20.1289294820831,21.2634386377592,
-22.));
#115347=CARTESIAN_POINT('Ctrl Pts',(-20.1576028623549,21.2390591151444,
-22.));
#115348=CARTESIAN_POINT('Ctrl Pts',(-20.1753080822265,21.2240052636568,
-22.));
#115349=CARTESIAN_POINT('Ctrl Pts',(-20.1928190152044,21.2087025308569,
-22.));
#115350=CARTESIAN_POINT('Ctrl Pts',(-20.2101297112266,21.1931551680194,
-22.));
#115351=CARTESIAN_POINT('Ctrl Pts',(-20.222291744835,21.182232005305,-22.));
#115352=CARTESIAN_POINT('Ctrl Pts',(-20.2343567146449,21.1711862914419,
-22.));
#115353=CARTESIAN_POINT('Ctrl Pts',(-20.2463056588354,21.1600355900683,
-22.));
#115354=CARTESIAN_POINT('Ctrl Pts',(-20.3097374358009,21.1008413389894,
-22.));
#115355=CARTESIAN_POINT('Ctrl Pts',(-20.3700068738243,21.0385997406358,
-22.));
#115356=CARTESIAN_POINT('Ctrl Pts',(-20.4268834135291,20.9735889911136,
-22.));
#115357=CARTESIAN_POINT('Ctrl Pts',(-20.4830375566033,20.9094039519221,
-22.));
#115358=CARTESIAN_POINT('Ctrl Pts',(-20.5358848927175,20.8425188203043,
-22.));
#115359=CARTESIAN_POINT('Ctrl Pts',(-20.5851610183652,20.7731751875981,
-22.));
#115360=CARTESIAN_POINT('Ctrl Pts',(-20.6305982452152,20.7092338300246,
-22.));
#115361=CARTESIAN_POINT('Ctrl Pts',(-20.6729988898206,20.6432013951078,
-22.));
#115362=CARTESIAN_POINT('Ctrl Pts',(-20.7121179614365,20.5752560755747,
-22.0000000000001));
#115363=CARTESIAN_POINT('Ctrl Pts',(-20.7284900120376,20.5468197103046,
-22.0000000000001));
#115364=CARTESIAN_POINT('Ctrl Pts',(-20.7442868026563,20.5180482040854,
-22.));
#115365=CARTESIAN_POINT('Ctrl Pts',(-20.7594882606863,20.4889543859677,
-22.));
#115366=CARTESIAN_POINT('Ctrl Pts',(-20.769344952432,20.4700898272965,-22.));
#115367=CARTESIAN_POINT('Ctrl Pts',(-20.7789513234994,20.4510897578356,
-22.));
#115368=CARTESIAN_POINT('Ctrl Pts',(-20.7883016018661,20.4319576715327,
-22.));
#115369=CARTESIAN_POINT('Ctrl Pts',(-20.7942275528717,20.4198322778685,
-22.));
#115370=CARTESIAN_POINT('Ctrl Pts',(-20.800046810587,20.4076616313445,-22.));
#115371=CARTESIAN_POINT('Ctrl Pts',(-20.8057567064001,20.3954502940177,
-22.));
#115372=CARTESIAN_POINT('Ctrl Pts',(-20.8408822399145,20.3203298798152,
-22.));
#115373=CARTESIAN_POINT('Ctrl Pts',(-20.8718943362061,20.2436277257691,
-22.));
#115374=CARTESIAN_POINT('Ctrl Pts',(-20.898546197771,20.1655724028405,-22.));
#115375=CARTESIAN_POINT('Ctrl Pts',(-20.9251980593358,20.0875170799122,
-22.));
#115376=CARTESIAN_POINT('Ctrl Pts',(-20.9474901582818,20.008107858314,-22.));
#115377=CARTESIAN_POINT('Ctrl Pts',(-20.9651213884777,19.9275640466204,
-22.));
#115378=CARTESIAN_POINT('Ctrl Pts',(-20.982945860616,19.8461374580334,-22.));
#115379=CARTESIAN_POINT('Ctrl Pts',(-20.9960059981342,19.7635500467728,
-22.));
#115380=CARTESIAN_POINT('Ctrl Pts',(-21.0043774598022,19.6801932612386,
-22.));
#115381=CARTESIAN_POINT('Ctrl Pts',(-21.0078359299807,19.6457563888755,
-22.));
#115382=CARTESIAN_POINT('Ctrl Pts',(-21.0104935728588,19.6111883610475,
-22.));
#115383=CARTESIAN_POINT('Ctrl Pts',(-21.0123533015418,19.5765177064329,
-22.));
#115384=CARTESIAN_POINT('Ctrl Pts',(-21.01308526083,19.5628718945969,-22.));
#115385=CARTESIAN_POINT('Ctrl Pts',(-21.0136936024307,19.5492081941022,
-22.));
#115386=CARTESIAN_POINT('Ctrl Pts',(-21.0141780332164,19.535546001816,-22.));
#115387=CARTESIAN_POINT('Ctrl Pts',(-21.0170628012175,19.4541881354373,
-22.));
#115388=CARTESIAN_POINT('Ctrl Pts',(-21.0155662532645,19.372753622897,-22.));
#115389=CARTESIAN_POINT('Ctrl Pts',(-21.009821014486,19.2915996489843,-22.));
#115390=CARTESIAN_POINT('Ctrl Pts',(-21.0040551150003,19.2101538336792,
-22.));
#115391=CARTESIAN_POINT('Ctrl Pts',(-20.9940095377782,19.1289895606253,
-22.));
#115392=CARTESIAN_POINT('Ctrl Pts',(-20.9797676620298,19.0484794559438,
-22.));
#115393=CARTESIAN_POINT('Ctrl Pts',(-20.9656474978692,18.9686573935437,
-22.));
#115394=CARTESIAN_POINT('Ctrl Pts',(-20.9474020142807,18.8894774430529,
-22.));
#115395=CARTESIAN_POINT('Ctrl Pts',(-20.9250689442011,18.8113285395616,
-22.));
#115396=CARTESIAN_POINT('Ctrl Pts',(-20.915771730189,18.7787953017227,-22.));
#115397=CARTESIAN_POINT('Ctrl Pts',(-20.9057656352848,18.7464411369984,
-22.));
#115398=CARTESIAN_POINT('Ctrl Pts',(-20.8950513997073,18.714296014732,-22.));
#115399=CARTESIAN_POINT('Ctrl Pts',(-20.8895107302012,18.6976727570651,
-22.));
#115400=CARTESIAN_POINT('Ctrl Pts',(-20.8837798036466,18.681103370745,-22.));
#115401=CARTESIAN_POINT('Ctrl Pts',(-20.8778666056241,18.6646133670345,
-22.));
#115402=CARTESIAN_POINT('Ctrl Pts',(-20.8511334433403,18.5900631923957,
-22.));
#115403=CARTESIAN_POINT('Ctrl Pts',(-20.8206474037361,18.5170371727757,
-22.));
#115404=CARTESIAN_POINT('Ctrl Pts',(-20.7864673395051,18.4458945668894,
-22.));
#115405=CARTESIAN_POINT('Ctrl Pts',(-20.7601551393027,18.3911281838789,
-22.));
#115406=CARTESIAN_POINT('Ctrl Pts',(-20.7316529155262,18.3374783045939,
-21.9999999999999));
#115407=CARTESIAN_POINT('Ctrl Pts',(-20.7009723139099,18.2851235072403,
-22.));
#115408=CARTESIAN_POINT('Ctrl Pts',(-20.6917380438118,18.2693657217269,
-22.));
#115409=CARTESIAN_POINT('Ctrl Pts',(-20.6823063515041,18.2537253600017,
-22.));
#115410=CARTESIAN_POINT('Ctrl Pts',(-20.6726773431573,18.2382075723836,
-21.9999999999999));
#115411=CARTESIAN_POINT('Ctrl Pts',(-20.6644524248536,18.2249525692911,
-21.9999999999999));
#115412=CARTESIAN_POINT('Ctrl Pts',(-20.6560858067932,18.2117907655657,
-22.));
#115413=CARTESIAN_POINT('Ctrl Pts',(-20.6475820990968,18.1987316736659,
-22.));
#115414=CARTESIAN_POINT('Ctrl Pts',(-20.6064305731469,18.1355355269518,
-22.));
#115415=CARTESIAN_POINT('Ctrl Pts',(-20.562041925838,18.0746943297042,-22.));
#115416=CARTESIAN_POINT('Ctrl Pts',(-20.5144495325811,18.0165478115783,
-22.));
#115417=CARTESIAN_POINT('Ctrl Pts',(-20.4703173158396,17.9626288013103,
-21.9999999999999));
#115418=CARTESIAN_POINT('Ctrl Pts',(-20.4234297243619,17.9110267653547,
-22.));
#115419=CARTESIAN_POINT('Ctrl Pts',(-20.3737908005412,17.8620457668345,
-22.));
#115420=CARTESIAN_POINT('Ctrl Pts',(-20.368202240041,17.8565312783541,-22.));
#115421=CARTESIAN_POINT('Ctrl Pts',(-20.3625787852046,17.8510500502091,
-22.));
#115422=CARTESIAN_POINT('Ctrl Pts',(-20.3569208045551,17.8456022314362,
-21.9999999999999));
#115423=CARTESIAN_POINT('Ctrl Pts',(20.3539256943888,17.8480877707428,-22.));
#115424=CARTESIAN_POINT('Ctrl Pts',(20.4076088569716,17.8998883167192,-22.));
#115425=CARTESIAN_POINT('Ctrl Pts',(20.458135458206,17.9545614547721,-22.));
#115426=CARTESIAN_POINT('Ctrl Pts',(20.5055117676562,18.0117358784471,-22.));
#115427=CARTESIAN_POINT('Ctrl Pts',(20.5545753925304,18.0709465790724,-22.));
#115428=CARTESIAN_POINT('Ctrl Pts',(20.6002608381613,18.1328403404639,-22.));
#115429=CARTESIAN_POINT('Ctrl Pts',(20.6425467287669,18.1970543621741,-22.));
#115430=CARTESIAN_POINT('Ctrl Pts',(20.6826812143677,18.2580013280008,-22.));
#115431=CARTESIAN_POINT('Ctrl Pts',(20.719753321312,18.3210393976475,-22.));
#115432=CARTESIAN_POINT('Ctrl Pts',(20.7537163061537,18.3858911290265,-22.));
#115433=CARTESIAN_POINT('Ctrl Pts',(20.7688146169019,18.4147210919254,-22.));
#115434=CARTESIAN_POINT('Ctrl Pts',(20.7832980898944,18.4439098480094,-22.));
#115435=CARTESIAN_POINT('Ctrl Pts',(20.79716062556,18.4734345611379,-22.));
#115436=CARTESIAN_POINT('Ctrl Pts',(20.8039889483082,18.4879776631471,-22.));
#115437=CARTESIAN_POINT('Ctrl Pts',(20.8106665939401,18.5026022906791,-22.));
#115438=CARTESIAN_POINT('Ctrl Pts',(20.8171927156004,18.5173057815627,-22.));
#115439=CARTESIAN_POINT('Ctrl Pts',(20.8232049158819,18.5308513966511,-22.));
#115440=CARTESIAN_POINT('Ctrl Pts',(20.8290889843231,18.5444653356248,-22.));
#115441=CARTESIAN_POINT('Ctrl Pts',(20.834836317356,18.5581259764514,-22.));
#115442=CARTESIAN_POINT('Ctrl Pts',(20.8659051086395,18.6319723320064,-22.));
#115443=CARTESIAN_POINT('Ctrl Pts',(20.8930386939032,18.7073070517052,-22.));
#115444=CARTESIAN_POINT('Ctrl Pts',(20.9162154441631,18.7837489961395,-22.));
#115445=CARTESIAN_POINT('Ctrl Pts',(20.9398185727455,18.8615972286714,-22.));
#115446=CARTESIAN_POINT('Ctrl Pts',(20.9593184548407,18.9405946085753,-22.));
#115447=CARTESIAN_POINT('Ctrl Pts',(20.9746513504475,19.0203741339709,-22.));
#115448=CARTESIAN_POINT('Ctrl Pts',(20.9885835808443,19.0928657726845,-22.));
#115449=CARTESIAN_POINT('Ctrl Pts',(20.9990750958876,19.1660041393162,-22.));
#115450=CARTESIAN_POINT('Ctrl Pts',(21.0060442872368,19.2395297293499,-22.));
#115451=CARTESIAN_POINT('Ctrl Pts',(21.0087022058165,19.2675710073175,-22.));
#115452=CARTESIAN_POINT('Ctrl Pts',(21.0108474418568,19.2956687140012,-22.));
#115453=CARTESIAN_POINT('Ctrl Pts',(21.0124741079748,19.3238087397167,-22.));
#115454=CARTESIAN_POINT('Ctrl Pts',(21.0133675811686,19.3392651129519,-22.));
#115455=CARTESIAN_POINT('Ctrl Pts',(21.0141045914371,19.3547342552799,-22.));
#115456=CARTESIAN_POINT('Ctrl Pts',(21.0146840610199,19.370213835923,-22.));
#115457=CARTESIAN_POINT('Ctrl Pts',(21.0151317606382,19.3821733978234,-22.));
#115458=CARTESIAN_POINT('Ctrl Pts',(21.0154852519447,19.3941358929903,-22.));
#115459=CARTESIAN_POINT('Ctrl Pts',(21.0157441139737,19.4060917025175,-22.));
#115460=CARTESIAN_POINT('Ctrl Pts',(21.0175509756949,19.4895434728017,-22.));
#115461=CARTESIAN_POINT('Ctrl Pts',(21.0147560087132,19.5727890030198,-22.));
#115462=CARTESIAN_POINT('Ctrl Pts',(21.0073029715582,19.655447656657,-22.));
#115463=CARTESIAN_POINT('Ctrl Pts',(20.9998641358153,19.737948808113,-22.));
#115464=CARTESIAN_POINT('Ctrl Pts',(20.987785339035,19.819866321382,-22.));
#115465=CARTESIAN_POINT('Ctrl Pts',(20.9709612973755,19.9008373573407,-22.));
#115466=CARTESIAN_POINT('Ctrl Pts',(20.9545235681866,19.9799491420218,-22.));
#115467=CARTESIAN_POINT('Ctrl Pts',(20.933556230191,20.0581583683546,-22.));
#115468=CARTESIAN_POINT('Ctrl Pts',(20.9083249440286,20.1352385562694,-22.));
#115469=CARTESIAN_POINT('Ctrl Pts',(20.8979275365846,20.1670020626737,-22.));
#115470=CARTESIAN_POINT('Ctrl Pts',(20.886805437583,20.198573773065,-22.));
#115471=CARTESIAN_POINT('Ctrl Pts',(20.8749747526326,20.2299373637517,-22.));
#115472=CARTESIAN_POINT('Ctrl Pts',(20.8684234889834,20.2473050100404,-22.));
#115473=CARTESIAN_POINT('Ctrl Pts',(20.8616526979763,20.2646139778576,-22.));
#115474=CARTESIAN_POINT('Ctrl Pts',(20.854677507136,20.2818314171768,-22.));
#115475=CARTESIAN_POINT('Ctrl Pts',(20.8237183426601,20.3582504783803,-22.));
#115476=CARTESIAN_POINT('Ctrl Pts',(20.7887032753635,20.4329627854485,-22.));
#115477=CARTESIAN_POINT('Ctrl Pts',(20.7499603220885,20.5057447265529,-22.));
#115478=CARTESIAN_POINT('Ctrl Pts',(20.7091534306779,20.5824039514244,-22.));
#115479=CARTESIAN_POINT('Ctrl Pts',(20.6642108439443,20.6569225092783,-22.));
#115480=CARTESIAN_POINT('Ctrl Pts',(20.6154553493761,20.7290334807154,-22.));
#115481=CARTESIAN_POINT('Ctrl Pts',(20.5666998548079,20.8011444521525,-22.));
#115482=CARTESIAN_POINT('Ctrl Pts',(20.5141308537666,20.8708487229331,-22.));
#115483=CARTESIAN_POINT('Ctrl Pts',(20.4580178821339,20.9378606771181,-22.));
#115484=CARTESIAN_POINT('Ctrl Pts',(20.4361041795504,20.9640307406671,-22.));
#115485=CARTESIAN_POINT('Ctrl Pts',(20.4136494525221,20.9897899196015,-22.));
#115486=CARTESIAN_POINT('Ctrl Pts',(20.3906678551117,21.0151199723788,-22.));
#115487=CARTESIAN_POINT('Ctrl Pts',(20.3815361086865,21.0251848784325,-22.));
#115488=CARTESIAN_POINT('Ctrl Pts',(20.3723204102617,21.0351828270963,-22.));
#115489=CARTESIAN_POINT('Ctrl Pts',(20.3630239550768,21.0451101306559,-22.));
#115490=CARTESIAN_POINT('Ctrl Pts',(20.3025143985113,21.1097258066671,-22.));
#115491=CARTESIAN_POINT('Ctrl Pts',(20.2387850522984,21.1711403943427,-22.));
#115492=CARTESIAN_POINT('Ctrl Pts',(20.1721440016479,21.2290795318307,-22.));
#115493=CARTESIAN_POINT('Ctrl Pts',(20.1169511545801,21.277065359236,-22.));
#115494=CARTESIAN_POINT('Ctrl Pts',(20.0597599496963,21.3226672272365,-22.));
#115495=CARTESIAN_POINT('Ctrl Pts',(20.0007222499054,21.3657153046774,-22.));
#115496=CARTESIAN_POINT('Ctrl Pts',(19.9812253064434,21.3799317449347,-22.));
#115497=CARTESIAN_POINT('Ctrl Pts',(19.9615268276842,21.3938695363309,-22.));
#115498=CARTESIAN_POINT('Ctrl Pts',(19.9416318550109,21.4075221540601,-22.));
#115499=CARTESIAN_POINT('Ctrl Pts',(19.9257068576964,21.4184504375137,-22.));
#115500=CARTESIAN_POINT('Ctrl Pts',(19.9096545963614,21.4291967564363,-22.));
#115501=CARTESIAN_POINT('Ctrl Pts',(19.8934936011196,21.4397475834371,-22.));
#115502=CARTESIAN_POINT('Ctrl Pts',(19.8189658486552,21.4884035858209,-22.));
#115503=CARTESIAN_POINT('Ctrl Pts',(19.7420559565434,21.5329559037425,-22.));
#115504=CARTESIAN_POINT('Ctrl Pts',(19.6630447888977,21.5731139344032,-22.));
#115505=CARTESIAN_POINT('Ctrl Pts',(19.5852035756509,21.6126773267864,-22.));
#115506=CARTESIAN_POINT('Ctrl Pts',(19.5053221751299,21.6479763280926,-22.));
#115507=CARTESIAN_POINT('Ctrl Pts',(19.423636718432,21.6786956932901,-22.));
#115508=CARTESIAN_POINT('Ctrl Pts',(19.414941951073,21.6819655254562,-22.));
#115509=CARTESIAN_POINT('Ctrl Pts',(19.4062267187917,21.6851834293815,-22.));
#115510=CARTESIAN_POINT('Ctrl Pts',(19.3974914370682,21.6883495353011,-22.));
#115511=CARTESIAN_POINT('Ctrl Pts',(18.0722627314313,21.6839949024184,-22.));
#115512=CARTESIAN_POINT('Ctrl Pts',(17.9906108868453,21.6544306627852,-22.));
#115513=CARTESIAN_POINT('Ctrl Pts',(17.9108507545872,21.6204659928942,-22.));
#115514=CARTESIAN_POINT('Ctrl Pts',(17.8331843622587,21.5824187212757,-22.));
#115515=CARTESIAN_POINT('Ctrl Pts',(17.7536727057571,21.5434674902341,-22.));
#115516=CARTESIAN_POINT('Ctrl Pts',(17.6763547404512,21.5002367065515,-22.));
#115517=CARTESIAN_POINT('Ctrl Pts',(17.6014766800473,21.4530209559463,-22.));
#115518=CARTESIAN_POINT('Ctrl Pts',(17.53141126818,21.408839910191,-22.));
#115519=CARTESIAN_POINT('Ctrl Pts',(17.4634820616961,21.361168717218,-22.));
#115520=CARTESIAN_POINT('Ctrl Pts',(17.3979216194972,21.3102212303572,-22.));
#115521=CARTESIAN_POINT('Ctrl Pts',(17.3682532365539,21.287165718535,-22.));
#115522=CARTESIAN_POINT('Ctrl Pts',(17.3390703946074,21.2634389577077,-22.));
#115523=CARTESIAN_POINT('Ctrl Pts',(17.3103970351346,21.2390594843875,-22.));
#115524=CARTESIAN_POINT('Ctrl Pts',(17.2926918259638,21.2240056615169,-22.));
#115525=CARTESIAN_POINT('Ctrl Pts',(17.2751809033557,21.2087029580218,-22.));
#115526=CARTESIAN_POINT('Ctrl Pts',(17.2578702173692,21.1931556251064,-22.));
#115527=CARTESIAN_POINT('Ctrl Pts',(17.2457081795529,21.1822324733025,-22.));
#115528=CARTESIAN_POINT('Ctrl Pts',(17.2336432055526,21.1711867704329,-22.));
#115529=CARTESIAN_POINT('Ctrl Pts',(17.2216942572027,21.160036080102,-22.));
#115530=CARTESIAN_POINT('Ctrl Pts',(17.1582624698647,21.1008418985699,-22.));
#115531=CARTESIAN_POINT('Ctrl Pts',(17.0979930211183,21.0386003723497,-22.));
#115532=CARTESIAN_POINT('Ctrl Pts',(17.0411164708952,20.973589694329,-22.));
#115533=CARTESIAN_POINT('Ctrl Pts',(16.9849623314079,20.9094047417006,-22.));
#115534=CARTESIAN_POINT('Ctrl Pts',(16.9321149974354,20.842519697379,-22.));
#115535=CARTESIAN_POINT('Ctrl Pts',(16.8828388728193,20.7731761494008,-22.));
#115536=CARTESIAN_POINT('Ctrl Pts',(16.8374016308099,20.7092348472829,-22.));
#115537=CARTESIAN_POINT('Ctrl Pts',(16.7950009722518,20.6432024641596,-22.));
#115538=CARTESIAN_POINT('Ctrl Pts',(16.7558818883965,20.5752571902803,-22.));
#115539=CARTESIAN_POINT('Ctrl Pts',(16.7395098281522,20.5468208362648,-22.));
#115540=CARTESIAN_POINT('Ctrl Pts',(16.7237130285085,20.5180493400384,-22.));
#115541=CARTESIAN_POINT('Ctrl Pts',(16.7085115621276,20.4889555304732,-22.));
#115542=CARTESIAN_POINT('Ctrl Pts',(16.6986548604459,20.4700909686944,-22.));
#115543=CARTESIAN_POINT('Ctrl Pts',(16.6890484799558,20.4510908953963,-22.));
#115544=CARTESIAN_POINT('Ctrl Pts',(16.6796981927033,20.4319588044811,-22.));
#115545=CARTESIAN_POINT('Ctrl Pts',(16.6737722459446,20.4198334281067,-22.));
#115546=CARTESIAN_POINT('Ctrl Pts',(16.6679529923645,20.4076627987652,-22.));
#115547=CARTESIAN_POINT('Ctrl Pts',(16.6622431005404,20.3954514784257,-22.));
#115548=CARTESIAN_POINT('Ctrl Pts',(16.6271175635218,20.3203311087503,-22.));
#115549=CARTESIAN_POINT('Ctrl Pts',(16.5961054651676,20.2436289901797,-22.));
#115550=CARTESIAN_POINT('Ctrl Pts',(16.5694536034806,20.1655736906577,-22.));
#115551=CARTESIAN_POINT('Ctrl Pts',(16.5428017417936,20.087518391136,-22.));
#115552=CARTESIAN_POINT('Ctrl Pts',(16.5205096446651,20.0081091808815,-22.));
#115553=CARTESIAN_POINT('Ctrl Pts',(16.5028784187468,19.9275653652902,-22.));
#115554=CARTESIAN_POINT('Ctrl Pts',(16.4850539498385,19.8461387677624,-22.));
#115555=CARTESIAN_POINT('Ctrl Pts',(16.4719938186516,19.7635513318282,-22.));
#115556=CARTESIAN_POINT('Ctrl Pts',(16.4636223658545,19.6801945089039,-22.));
#115557=CARTESIAN_POINT('Ctrl Pts',(16.4601638998612,19.6457576262764,-22.));
#115558=CARTESIAN_POINT('Ctrl Pts',(16.457506261361,19.6111895860526,-22.));
#115559=CARTESIAN_POINT('Ctrl Pts',(16.4556465372103,19.5765189171097,-22.));
#115560=CARTESIAN_POINT('Ctrl Pts',(16.4549145796191,19.5628730980147,-22.));
#115561=CARTESIAN_POINT('Ctrl Pts',(16.4543062397689,19.5492093899537,-22.));
#115562=CARTESIAN_POINT('Ctrl Pts',(16.4538218107824,19.535547189819,-22.));
#115563=CARTESIAN_POINT('Ctrl Pts',(16.450937053514,19.4541892772202,-22.));
#115564=CARTESIAN_POINT('Ctrl Pts',(16.4524336138896,19.3727547084354,-22.));
#115565=CARTESIAN_POINT('Ctrl Pts',(16.4581788662374,19.291600671179,-22.));
#115566=CARTESIAN_POINT('Ctrl Pts',(16.4639447791335,19.210154795236,-22.));
#115567=CARTESIAN_POINT('Ctrl Pts',(16.4739903706141,19.128990454367,-22.));
#115568=CARTESIAN_POINT('Ctrl Pts',(16.4882322609366,19.0484802775444,-22.));
#115569=CARTESIAN_POINT('Ctrl Pts',(16.502352437732,18.9686581538777,-22.));
#115570=CARTESIAN_POINT('Ctrl Pts',(16.520597933207,18.8894781376979,-22.));
#115571=CARTESIAN_POINT('Ctrl Pts',(16.5429310139029,18.8113291667476,-22.));
#115572=CARTESIAN_POINT('Ctrl Pts',(16.5522282344977,18.7787958932563,-22.));
#115573=CARTESIAN_POINT('Ctrl Pts',(16.5622343360937,18.7464416926568,-21.9999999999999));
#115574=CARTESIAN_POINT('Ctrl Pts',(16.5729485784318,18.7142965345087,-22.));
#115575=CARTESIAN_POINT('Ctrl Pts',(16.5784892537261,18.6976732514091,-22.));
#115576=CARTESIAN_POINT('Ctrl Pts',(16.5842201862524,18.6811038396758,-22.));
#115577=CARTESIAN_POINT('Ctrl Pts',(16.5901333904085,18.6646138106646,-22.));
#115578=CARTESIAN_POINT('Ctrl Pts',(16.6168665610553,18.5900635756494,-22.));
#115579=CARTESIAN_POINT('Ctrl Pts',(16.6473526068873,18.5170374956828,-22.));
#115580=CARTESIAN_POINT('Ctrl Pts',(16.6815326747322,18.4458948319453,-22.));
#115581=CARTESIAN_POINT('Ctrl Pts',(16.7078448953081,18.3911283677852,-22.));
#115582=CARTESIAN_POINT('Ctrl Pts',(16.7363471408355,18.3374784103201,-22.));
#115583=CARTESIAN_POINT('Ctrl Pts',(16.7670277653193,18.2851235392682,-22.));
#115584=CARTESIAN_POINT('Ctrl Pts',(16.7762620345021,18.2693657448798,-22.));
#115585=CARTESIAN_POINT('Ctrl Pts',(16.7856937256623,18.2537253744878,-22.));
#115586=CARTESIAN_POINT('Ctrl Pts',(16.7953227326228,18.2382075784408,-22.));
#115587=CARTESIAN_POINT('Ctrl Pts',(16.8035476401832,18.2249525835537,-22.));
#115588=CARTESIAN_POINT('Ctrl Pts',(16.8119142470167,18.2117907879613,-22.));
#115589=CARTESIAN_POINT('Ctrl Pts',(16.8204179429878,18.198731704156,-22.));
#115590=CARTESIAN_POINT('Ctrl Pts',(16.8615694556779,18.1355355298381,-22.));
#115591=CARTESIAN_POINT('Ctrl Pts',(16.9059580849723,18.0746943089279,-22.));
#115592=CARTESIAN_POINT('Ctrl Pts',(16.9535504550157,18.0165477730385,-22.));
#115593=CARTESIAN_POINT('Ctrl Pts',(16.9976827241168,17.9626286560281,-22.));
#115594=CARTESIAN_POINT('Ctrl Pts',(17.0445703727031,17.9110265261487,-22.));
#115595=CARTESIAN_POINT('Ctrl Pts',(17.0942093579555,17.8620454496849,-22.));
#115596=CARTESIAN_POINT('Ctrl Pts',(17.0997979190133,17.8565309587036,-22.));
#115597=CARTESIAN_POINT('Ctrl Pts',(17.1054213743828,17.8510497281848,-22.));
#115598=CARTESIAN_POINT('Ctrl Pts',(17.1110793555412,17.8456019071633,-22.));
#115599=CARTESIAN_POINT('Ctrl Pts',(20.3539256943887,-20.3149122292573,
-22.));
#115600=CARTESIAN_POINT('Ctrl Pts',(20.408139566195,-20.2625995855167,-22.));
#115601=CARTESIAN_POINT('Ctrl Pts',(20.4591341972937,-20.2073573541925,
-22.));
#115602=CARTESIAN_POINT('Ctrl Pts',(20.5069159265706,-20.1495677196682,
-22.));
#115603=CARTESIAN_POINT('Ctrl Pts',(20.5546976558475,-20.091778085144,-22.));
#115604=CARTESIAN_POINT('Ctrl Pts',(20.5992668013762,-20.0314403792713,
-22.));
#115605=CARTESIAN_POINT('Ctrl Pts',(20.6406036312651,-19.9688911346062,
-22.));
#115606=CARTESIAN_POINT('Ctrl Pts',(20.6814854208042,-19.9070304388754,
-22.));
#115607=CARTESIAN_POINT('Ctrl Pts',(20.7192059247084,-19.8430059080155,
-22.));
#115608=CARTESIAN_POINT('Ctrl Pts',(20.7537163516506,-19.7771088559497,
-22.));
#115609=CARTESIAN_POINT('Ctrl Pts',(20.7688146634378,-19.748278895671,-22.));
#115610=CARTESIAN_POINT('Ctrl Pts',(20.7832981375853,-19.7190901423257,
-22.));
#115611=CARTESIAN_POINT('Ctrl Pts',(20.7971606745034,-19.6895654320343,
-22.));
#115612=CARTESIAN_POINT('Ctrl Pts',(20.8039890054239,-19.6750223153312,
-22.));
#115613=CARTESIAN_POINT('Ctrl Pts',(20.8106666589183,-19.660397672949,-22.));
#115614=CARTESIAN_POINT('Ctrl Pts',(20.8171927881263,-19.6456941670648,
-22.));
#115615=CARTESIAN_POINT('Ctrl Pts',(20.8232049803476,-19.6321485719831,
-22.));
#115616=CARTESIAN_POINT('Ctrl Pts',(20.8290890410869,-19.618534653263,-22.));
#115617=CARTESIAN_POINT('Ctrl Pts',(20.8348363668121,-19.6048740328408,
-22.));
#115618=CARTESIAN_POINT('Ctrl Pts',(20.8661434568434,-19.5304612896112,
-22.));
#115619=CARTESIAN_POINT('Ctrl Pts',(20.8934547915536,-19.4545373140852,
-21.9999999999999));
#115620=CARTESIAN_POINT('Ctrl Pts',(20.916748098317,-19.3774919314298,-22.));
#115621=CARTESIAN_POINT('Ctrl Pts',(20.9400414050804,-19.3004465487744,
-22.));
#115622=CARTESIAN_POINT('Ctrl Pts',(20.9593170648394,-19.2222788660794,
-21.9999999999999));
#115623=CARTESIAN_POINT('Ctrl Pts',(20.9745132363111,-19.1433443390627,
-21.9999999999999));
#115624=CARTESIAN_POINT('Ctrl Pts',(20.9885143247977,-19.0706175144489,
-21.9999999999999));
#115625=CARTESIAN_POINT('Ctrl Pts',(20.9990521599664,-18.9972388060651,
-22.));
#115626=CARTESIAN_POINT('Ctrl Pts',(21.0060443782249,-18.923470317406,-22.));
#115627=CARTESIAN_POINT('Ctrl Pts',(21.0087022983456,-18.8954290373673,
-22.));
#115628=CARTESIAN_POINT('Ctrl Pts',(21.010847535719,-18.8673313285427,-22.));
#115629=CARTESIAN_POINT('Ctrl Pts',(21.012474202948,-18.8391913006101,-22.));
#115630=CARTESIAN_POINT('Ctrl Pts',(21.0133676804257,-18.8237348626051,
-22.));
#115631=CARTESIAN_POINT('Ctrl Pts',(21.0141046936245,-18.8082656553794,
-22.));
#115632=CARTESIAN_POINT('Ctrl Pts',(21.0146841647679,-18.7927860097385,
-22.));
#115633=CARTESIAN_POINT('Ctrl Pts',(21.0151318658524,-18.7808263906625,
-22.));
#115634=CARTESIAN_POINT('Ctrl Pts',(21.01548535769,-18.768863838497,-22.));
#115635=CARTESIAN_POINT('Ctrl Pts',(21.0157442193216,-18.7569079719692,
-22.));
#115636=CARTESIAN_POINT('Ctrl Pts',(21.017551069503,-18.6734562086591,-22.));
#115637=CARTESIAN_POINT('Ctrl Pts',(21.0147560903276,-18.5902106853063,
-22.));
#115638=CARTESIAN_POINT('Ctrl Pts',(21.0073030399704,-18.5075520380822,
-22.));
#115639=CARTESIAN_POINT('Ctrl Pts',(20.9998642034238,-18.4250510302545,
-22.));
#115640=CARTESIAN_POINT('Ctrl Pts',(20.9877854202568,-18.3431336582205,
-22.));
#115641=CARTESIAN_POINT('Ctrl Pts',(20.9709614068361,-18.2621627589815,
-22.));
#115642=CARTESIAN_POINT('Ctrl Pts',(20.9545236784523,-18.1830509789684,
-22.));
#115643=CARTESIAN_POINT('Ctrl Pts',(20.9335563404747,-18.104841755941,-22.));
#115644=CARTESIAN_POINT('Ctrl Pts',(20.9083250537327,-18.0277615701596,
-22.));
#115645=CARTESIAN_POINT('Ctrl Pts',(20.8979276440165,-17.9959980584227,
-22.));
#115646=CARTESIAN_POINT('Ctrl Pts',(20.8868055423579,-17.9644263425748,
-22.));
#115647=CARTESIAN_POINT('Ctrl Pts',(20.874974854388,-17.9330627463293,-22.));
#115648=CARTESIAN_POINT('Ctrl Pts',(20.8684235902148,-17.9156951000059,
-22.));
#115649=CARTESIAN_POINT('Ctrl Pts',(20.8616527986486,-17.8983861321004,
-22.));
#115650=CARTESIAN_POINT('Ctrl Pts',(20.854677607217,-17.8811686926409,-22.));
#115651=CARTESIAN_POINT('Ctrl Pts',(20.8226256793881,-17.8020522795121,
-22.));
#115652=CARTESIAN_POINT('Ctrl Pts',(20.7862268153504,-17.724765227739,-22.));
#115653=CARTESIAN_POINT('Ctrl Pts',(20.7458439642001,-17.6495556859564,
-22.));
#115654=CARTESIAN_POINT('Ctrl Pts',(20.7054483430734,-17.5743223612055,
-22.));
#115655=CARTESIAN_POINT('Ctrl Pts',(20.6610656710241,-17.501167065488,-22.));
#115656=CARTESIAN_POINT('Ctrl Pts',(20.6130013967575,-17.4303438070485,
-22.));
#115657=CARTESIAN_POINT('Ctrl Pts',(20.5649371224908,-17.359520548609,-22.));
#115658=CARTESIAN_POINT('Ctrl Pts',(20.5131906957729,-17.2910285130232,
-22.));
#115659=CARTESIAN_POINT('Ctrl Pts',(20.4580179345364,-17.2251393904043,
-22.));
#115660=CARTESIAN_POINT('Ctrl Pts',(20.4361042290218,-17.1989693239199,
-22.));
#115661=CARTESIAN_POINT('Ctrl Pts',(20.4136494990236,-17.1732101420222,
-22.));
#115662=CARTESIAN_POINT('Ctrl Pts',(20.3906678986206,-17.1478800862692,
-22.));
#115663=CARTESIAN_POINT('Ctrl Pts',(20.3815361507949,-17.1378151788001,
-22.));
#115664=CARTESIAN_POINT('Ctrl Pts',(20.3723204509639,-17.1278172287239,
-22.));
#115665=CARTESIAN_POINT('Ctrl Pts',(20.3630239943621,-17.1178899237497,
-22.));
#115666=CARTESIAN_POINT('Ctrl Pts',(20.3025144308281,-17.0532742409372,
-22.));
#115667=CARTESIAN_POINT('Ctrl Pts',(20.2387850776616,-16.9918596463668,
-22.));
#115668=CARTESIAN_POINT('Ctrl Pts',(20.1721440203356,-16.9339205021469,
-22.));
#115669=CARTESIAN_POINT('Ctrl Pts',(20.1169511671352,-16.8859346686413,
-22.));
#115670=CARTESIAN_POINT('Ctrl Pts',(20.0597599562651,-16.8403327947037,
-22.));
#115671=CARTESIAN_POINT('Ctrl Pts',(20.0007222507865,-16.7972847116374,
-22.));
#115672=CARTESIAN_POINT('Ctrl Pts',(19.9812253134723,-16.7830682753746,
-22.));
#115673=CARTESIAN_POINT('Ctrl Pts',(19.9615268410592,-16.7691304877775,
-22.));
#115674=CARTESIAN_POINT('Ctrl Pts',(19.94163187493,-16.7554778736493,-22.));
#115675=CARTESIAN_POINT('Ctrl Pts',(19.9257068621322,-16.7445495788584,
-22.));
#115676=CARTESIAN_POINT('Ctrl Pts',(19.9096545851051,-16.733803248942,-22.));
#115677=CARTESIAN_POINT('Ctrl Pts',(19.8934935740057,-16.7232524113246,
-22.));
#115678=CARTESIAN_POINT('Ctrl Pts',(19.818965815021,-16.6745964034672,-22.));
#115679=CARTESIAN_POINT('Ctrl Pts',(19.7420559170313,-16.630044080676,-22.));
#115680=CARTESIAN_POINT('Ctrl Pts',(19.6630447444111,-16.5898860460099,
-22.));
#115681=CARTESIAN_POINT('Ctrl Pts',(19.585203529837,-16.5503226514967,-22.));
#115682=CARTESIAN_POINT('Ctrl Pts',(19.5053221290521,-16.5150236485074,
-22.));
#115683=CARTESIAN_POINT('Ctrl Pts',(19.4236366733768,-16.4843042822826,
-22.));
#115684=CARTESIAN_POINT('Ctrl Pts',(19.4149419062245,-16.481034450044,-22.));
#115685=CARTESIAN_POINT('Ctrl Pts',(19.4062266741651,-16.4778165460524,
-22.));
#115686=CARTESIAN_POINT('Ctrl Pts',(19.3974913926779,-16.4746504400725,
-22.));
#115687=CARTESIAN_POINT('Ctrl Pts',(18.0722627314314,-16.4790050975816,
-22.));
#115688=CARTESIAN_POINT('Ctrl Pts',(17.9909906838445,-16.5084318215279,
-22.));
#115689=CARTESIAN_POINT('Ctrl Pts',(17.9115928093154,-16.5422181704993,
-22.));
#115690=CARTESIAN_POINT('Ctrl Pts',(17.8342682750801,-16.580050621616,-22.));
#115691=CARTESIAN_POINT('Ctrl Pts',(17.7547379110741,-16.6189623155343,
-22.));
#115692=CARTESIAN_POINT('Ctrl Pts',(17.6774001286652,-16.6621548599534,
-22.));
#115693=CARTESIAN_POINT('Ctrl Pts',(17.6025009734493,-16.7093334978469,
-22.));
#115694=CARTESIAN_POINT('Ctrl Pts',(17.5320732406115,-16.7536956070808,
-22.));
#115695=CARTESIAN_POINT('Ctrl Pts',(17.463801490032,-16.8015830463496,-22.));
#115696=CARTESIAN_POINT('Ctrl Pts',(17.3979216159377,-16.8527787647009,
-22.));
#115697=CARTESIAN_POINT('Ctrl Pts',(17.368253233471,-16.875834275562,-22.));
#115698=CARTESIAN_POINT('Ctrl Pts',(17.3390703919806,-16.89956103538,-22.));
#115699=CARTESIAN_POINT('Ctrl Pts',(17.3103970329429,-16.9239405076492,
-22.));
#115700=CARTESIAN_POINT('Ctrl Pts',(17.2926918239748,-16.938994329927,-22.));
#115701=CARTESIAN_POINT('Ctrl Pts',(17.2751809015629,-16.9542970328152,
-22.));
#115702=CARTESIAN_POINT('Ctrl Pts',(17.257870215766,-16.9698443651112,-22.));
#115703=CARTESIAN_POINT('Ctrl Pts',(17.2457081778958,-16.9807675166481,
-22.));
#115704=CARTESIAN_POINT('Ctrl Pts',(17.2336432038411,-16.9918132192483,
-22.));
#115705=CARTESIAN_POINT('Ctrl Pts',(17.2216942554371,-17.0029639093079,
-22.));
#115706=CARTESIAN_POINT('Ctrl Pts',(17.1582584279828,-17.0621618593448,
-22.));
#115707=CARTESIAN_POINT('Ctrl Pts',(17.0979853415004,-17.1244075418475,
-22.));
#115708=CARTESIAN_POINT('Ctrl Pts',(17.0411056012962,-17.1894227118676,
-22.));
#115709=CARTESIAN_POINT('Ctrl Pts',(16.9845622276309,-17.2540534053124,
-22.));
#115710=CARTESIAN_POINT('Ctrl Pts',(16.9313716721992,-17.321421754448,-22.));
#115711=CARTESIAN_POINT('Ctrl Pts',(16.8818040511554,-17.3912811759233,
-22.));
#115712=CARTESIAN_POINT('Ctrl Pts',(16.8334273398594,-17.4594621576379,
-22.));
#115713=CARTESIAN_POINT('Ctrl Pts',(16.7885012591507,-17.5300167108658,
-22.));
#115714=CARTESIAN_POINT('Ctrl Pts',(16.7473243285991,-17.6027294194541,
-22.));
#115715=CARTESIAN_POINT('Ctrl Pts',(16.7339893719969,-17.6262770904551,
-22.));
#115716=CARTESIAN_POINT('Ctrl Pts',(16.7210480077419,-17.6500511631478,
-22.));
#115717=CARTESIAN_POINT('Ctrl Pts',(16.7085115583106,-17.6740444448892,
-22.));
#115718=CARTESIAN_POINT('Ctrl Pts',(16.6986548564673,-17.6929090066348,
-22.));
#115719=CARTESIAN_POINT('Ctrl Pts',(16.6890484758239,-17.7119090799142,
-22.));
#115720=CARTESIAN_POINT('Ctrl Pts',(16.679698188427,-17.7310411708259,-22.));
#115721=CARTESIAN_POINT('Ctrl Pts',(16.6737722417175,-17.7431665469103,
-22.));
#115722=CARTESIAN_POINT('Ctrl Pts',(16.6679529881854,-17.7553371759649,
-22.));
#115723=CARTESIAN_POINT('Ctrl Pts',(16.6622430964078,-17.7675484960222,
-22.));
#115724=CARTESIAN_POINT('Ctrl Pts',(16.6271175593077,-17.8426688647472,
-22.));
#115725=CARTESIAN_POINT('Ctrl Pts',(16.5961054609041,-17.9193709825623,
-22.));
#115726=CARTESIAN_POINT('Ctrl Pts',(16.5694535992104,-17.9974262815892,
-22.));
#115727=CARTESIAN_POINT('Ctrl Pts',(16.5428017375166,-18.0754815806163,
-22.));
#115728=CARTESIAN_POINT('Ctrl Pts',(16.5205096404242,-18.1548907906356,
-22.));
#115729=CARTESIAN_POINT('Ctrl Pts',(16.502878414596,-18.2354346063206,-22.));
#115730=CARTESIAN_POINT('Ctrl Pts',(16.4850539457493,-18.3168612040769,
-22.));
#115731=CARTESIAN_POINT('Ctrl Pts',(16.4719938146952,-18.3994486405796,
-22.));
#115732=CARTESIAN_POINT('Ctrl Pts',(16.4636223620895,-18.4828054643466,
-22.));
#115733=CARTESIAN_POINT('Ctrl Pts',(16.4601638961884,-18.5172423471919,
-22.));
#115734=CARTESIAN_POINT('Ctrl Pts',(16.4575062577843,-18.5518103876793,
-22.));
#115735=CARTESIAN_POINT('Ctrl Pts',(16.455646533733,-18.5864810569274,-22.));
#115736=CARTESIAN_POINT('Ctrl Pts',(16.4549145761463,-18.6001268767863,
-22.));
#115737=CARTESIAN_POINT('Ctrl Pts',(16.4543062363129,-18.6137905856188,
-22.));
#115738=CARTESIAN_POINT('Ctrl Pts',(16.4538218073552,-18.6274527865309,
-22.));
#115739=CARTESIAN_POINT('Ctrl Pts',(16.4509320250045,-18.7089524294446,
-22.));
#115740=CARTESIAN_POINT('Ctrl Pts',(16.4524388232547,-18.790528997647,-22.));
#115741=CARTESIAN_POINT('Ctrl Pts',(16.4582089280278,-18.8718234286525,
-22.));
#115742=CARTESIAN_POINT('Ctrl Pts',(16.4640073807546,-18.9535172511518,
-22.));
#115743=CARTESIAN_POINT('Ctrl Pts',(16.4741115013324,-19.034927191256,-22.));
#115744=CARTESIAN_POINT('Ctrl Pts',(16.4884372995143,-19.1156771272516,
-22.));
#115745=CARTESIAN_POINT('Ctrl Pts',(16.5025241468048,-19.1950801736051,
-22.));
#115746=CARTESIAN_POINT('Ctrl Pts',(16.52069350435,-19.2738459251496,-22.));
#115747=CARTESIAN_POINT('Ctrl Pts',(16.5429083122977,-19.3515913790962,
-22.));
#115748=CARTESIAN_POINT('Ctrl Pts',(16.5522119453725,-19.3841514254605,
-22.));
#115749=CARTESIAN_POINT('Ctrl Pts',(16.5622256148023,-19.416532131398,-22.));
#115750=CARTESIAN_POINT('Ctrl Pts',(16.5729485780652,-19.4487034546206,
-22.));
#115751=CARTESIAN_POINT('Ctrl Pts',(16.578489253474,-19.4653267382297,-22.));
#115752=CARTESIAN_POINT('Ctrl Pts',(16.5842201861179,-19.481896150472,-22.));
#115753=CARTESIAN_POINT('Ctrl Pts',(16.5901333903942,-19.4983861799902,
-22.));
#115754=CARTESIAN_POINT('Ctrl Pts',(16.6168665612538,-19.5729364163756,
-22.));
#115755=CARTESIAN_POINT('Ctrl Pts',(16.6473526072598,-19.6459624977086,
-22.));
#115756=CARTESIAN_POINT('Ctrl Pts',(16.6815326752298,-19.7171051627545,
-22.));
#115757=CARTESIAN_POINT('Ctrl Pts',(16.7078448962084,-19.7718716285595,
-22.));
#115758=CARTESIAN_POINT('Ctrl Pts',(16.7363471421602,-19.8255215876092,
-22.));
#115759=CARTESIAN_POINT('Ctrl Pts',(16.7670277670848,-19.8778764601534,
-22.));
#115760=CARTESIAN_POINT('Ctrl Pts',(16.7762620361372,-19.8936342545421,
-22.));
#115761=CARTESIAN_POINT('Ctrl Pts',(16.7856937271573,-19.9092746249327,
-22.));
#115762=CARTESIAN_POINT('Ctrl Pts',(16.7953227339677,-19.9247924209762,
-22.));
#115763=CARTESIAN_POINT('Ctrl Pts',(16.8035476416632,-19.9380474162847,
-21.9999999999999));
#115764=CARTESIAN_POINT('Ctrl Pts',(16.8119142486341,-19.9512092122917,
-22.));
#115765=CARTESIAN_POINT('Ctrl Pts',(16.8204179447442,-19.9642682965029,
-22.));
#115766=CARTESIAN_POINT('Ctrl Pts',(16.8615694572081,-20.0274644714052,
-22.));
#115767=CARTESIAN_POINT('Ctrl Pts',(16.905958086176,-20.0883056928111,-21.9999999999999));
#115768=CARTESIAN_POINT('Ctrl Pts',(16.9535504557831,-20.1464522290647,
-22.));
#115769=CARTESIAN_POINT('Ctrl Pts',(16.9976827257099,-20.2003713479159,
-22.));
#115770=CARTESIAN_POINT('Ctrl Pts',(17.0445703751811,-20.251973479394,-22.));
#115771=CARTESIAN_POINT('Ctrl Pts',(17.0942093613684,-20.3009545571532,
-22.));
#115772=CARTESIAN_POINT('Ctrl Pts',(17.0997979224383,-20.3064690481884,
-22.));
#115773=CARTESIAN_POINT('Ctrl Pts',(17.1054213778192,-20.3119502787582,
-22.));
#115774=CARTESIAN_POINT('Ctrl Pts',(17.1110793589886,-20.3173980998282,
-22.));
#115775=CARTESIAN_POINT('Ctrl Pts',(-17.1140743056112,-20.3149122292573,
-22.));
#115776=CARTESIAN_POINT('Ctrl Pts',(-17.0603910881415,-20.2631116303188,
-22.));
#115777=CARTESIAN_POINT('Ctrl Pts',(-17.009864429043,-20.2084384430965,
-22.));
#115778=CARTESIAN_POINT('Ctrl Pts',(-16.9624880608118,-20.1512639730765,
-22.));
#115779=CARTESIAN_POINT('Ctrl Pts',(-16.9134243877873,-20.0920532398113,
-22.));
#115780=CARTESIAN_POINT('Ctrl Pts',(-16.867738891267,-20.0301594501991,
-22.));
#115781=CARTESIAN_POINT('Ctrl Pts',(-16.8254529492616,-19.9659454033071,
-22.));
#115782=CARTESIAN_POINT('Ctrl Pts',(-16.7853184507726,-19.904998468091,
-22.));
#115783=CARTESIAN_POINT('Ctrl Pts',(-16.7482463250022,-19.8419604355298,
-22.));
#115784=CARTESIAN_POINT('Ctrl Pts',(-16.71428331717,-19.777108745806,-22.));
#115785=CARTESIAN_POINT('Ctrl Pts',(-16.6991849978544,-19.7482788045816,
-22.));
#115786=CARTESIAN_POINT('Ctrl Pts',(-16.6847015153359,-19.7190900711551,
-22.));
#115787=CARTESIAN_POINT('Ctrl Pts',(-16.6708389693358,-19.6895653814969,
-22.));
#115788=CARTESIAN_POINT('Ctrl Pts',(-16.6640105788719,-19.6750221576682,
-22.));
#115789=CARTESIAN_POINT('Ctrl Pts',(-16.6573328680918,-19.6603974070189,
-22.));
#115790=CARTESIAN_POINT('Ctrl Pts',(-16.6508066838924,-19.6456937917726,
-22.));
#115791=CARTESIAN_POINT('Ctrl Pts',(-16.6447945515434,-19.6321483449743,
-22.));
#115792=CARTESIAN_POINT('Ctrl Pts',(-16.6389105480172,-19.6185345763602,
-22.));
#115793=CARTESIAN_POINT('Ctrl Pts',(-16.6331632765825,-19.6048741071589,
-22.));
#115794=CARTESIAN_POINT('Ctrl Pts',(-16.6018561398417,-19.530461373728,
-22.));
#115795=CARTESIAN_POINT('Ctrl Pts',(-16.5745447598008,-19.4545374092054,
-22.));
#115796=CARTESIAN_POINT('Ctrl Pts',(-16.5512514111518,-19.3774920371772,
-22.));
#115797=CARTESIAN_POINT('Ctrl Pts',(-16.5279580625028,-19.3004466651491,
-22.));
#115798=CARTESIAN_POINT('Ctrl Pts',(-16.5086823642981,-19.2222789927081,
-22.));
#115799=CARTESIAN_POINT('Ctrl Pts',(-16.4934861598923,-19.1433444740215,
-22.));
#115800=CARTESIAN_POINT('Ctrl Pts',(-16.4781825851218,-19.0638522352736,
-22.));
#115801=CARTESIAN_POINT('Ctrl Pts',(-16.4670158957966,-18.9835813665502,
-22.));
#115802=CARTESIAN_POINT('Ctrl Pts',(-16.4600957863878,-18.9028735673802,
-22.));
#115803=CARTESIAN_POINT('Ctrl Pts',(-16.4582781144994,-18.8816744375601,
-22.));
#115804=CARTESIAN_POINT('Ctrl Pts',(-16.4567536954935,-18.8604450906499,
-22.));
#115805=CARTESIAN_POINT('Ctrl Pts',(-16.4555251072067,-18.8391916010845,
-22.));
#115806=CARTESIAN_POINT('Ctrl Pts',(-16.4546315989448,-18.8237346992684,
-22.));
#115807=CARTESIAN_POINT('Ctrl Pts',(-16.45389456466,-18.8082650273129,-22.));
#115808=CARTESIAN_POINT('Ctrl Pts',(-16.4533150822428,-18.7927849162226,
-22.));
#115809=CARTESIAN_POINT('Ctrl Pts',(-16.4528673708036,-18.7808248936061,
-22.));
#115810=CARTESIAN_POINT('Ctrl Pts',(-16.4525138752178,-18.7688619391664,
-22.));
#115811=CARTESIAN_POINT('Ctrl Pts',(-16.4522550163972,-18.7569056703414,
-22.));
#115812=CARTESIAN_POINT('Ctrl Pts',(-16.4504482477209,-18.6734539573408,
-22.));
#115813=CARTESIAN_POINT('Ctrl Pts',(-16.4532433131771,-18.5902084834056,
-22.));
#115814=CARTESIAN_POINT('Ctrl Pts',(-16.4606964571555,-18.5075498822213,
-22.));
#115815=CARTESIAN_POINT('Ctrl Pts',(-16.4681352990784,-18.4250498970387,
-22.));
#115816=CARTESIAN_POINT('Ctrl Pts',(-16.4802139851741,-18.3431335304585,
-22.));
#115817=CARTESIAN_POINT('Ctrl Pts',(-16.4970377976341,-18.2621636043343,
-22.));
#115818=CARTESIAN_POINT('Ctrl Pts',(-16.5135061122501,-18.1829046241824,
-22.));
#115819=CARTESIAN_POINT('Ctrl Pts',(-16.5345209017837,-18.1045515514237,
-22.));
#115820=CARTESIAN_POINT('Ctrl Pts',(-16.5598150664329,-18.027332141339,
-22.));
#115821=CARTESIAN_POINT('Ctrl Pts',(-16.5701720519776,-17.9957137690736,
-22.));
#115822=CARTESIAN_POINT('Ctrl Pts',(-16.5812471270599,-17.964285535797,
-22.));
#115823=CARTESIAN_POINT('Ctrl Pts',(-16.5930244062011,-17.9330635460661,
-22.));
#115824=CARTESIAN_POINT('Ctrl Pts',(-16.5995756745648,-17.9156958984863,
-22.));
#115825=CARTESIAN_POINT('Ctrl Pts',(-16.606346470602,-17.8983869289424,
-22.));
#115826=CARTESIAN_POINT('Ctrl Pts',(-16.613321666761,-17.8811694874779,
-22.));
#115827=CARTESIAN_POINT('Ctrl Pts',(-16.6442808434086,-17.804750444978,
-22.));
#115828=CARTESIAN_POINT('Ctrl Pts',(-16.6792959255797,-17.7300381471314,
-22.));
#115829=CARTESIAN_POINT('Ctrl Pts',(-16.7180388949534,-17.6572562073793,
-22.));
#115830=CARTESIAN_POINT('Ctrl Pts',(-16.7588458333272,-17.5805969275616,
-22.));
#115831=CARTESIAN_POINT('Ctrl Pts',(-16.8037884744598,-17.5060783091779,
-22.));
#115832=CARTESIAN_POINT('Ctrl Pts',(-16.852544028446,-17.4339672739469,
-22.));
#115833=CARTESIAN_POINT('Ctrl Pts',(-16.9012995824321,-17.3618562387159,
-22.));
#115834=CARTESIAN_POINT('Ctrl Pts',(-16.9538686479157,-17.2921519008718,
-22.));
#115835=CARTESIAN_POINT('Ctrl Pts',(-17.0099816867116,-17.2251398785991,
-22.));
#115836=CARTESIAN_POINT('Ctrl Pts',(-17.0318954130067,-17.1989697914665,
-22.));
#115837=CARTESIAN_POINT('Ctrl Pts',(-17.0543501640382,-17.1732105886975,
-22.));
#115838=CARTESIAN_POINT('Ctrl Pts',(-17.0773317856131,-17.1478805119615,
-22.));
#115839=CARTESIAN_POINT('Ctrl Pts',(-17.0864635488618,-17.1378155884281,
-22.));
#115840=CARTESIAN_POINT('Ctrl Pts',(-17.095679264258,-17.127817622382,-22.));
#115841=CARTESIAN_POINT('Ctrl Pts',(-17.1049757365821,-17.1178903015161,
-22.));
#115842=CARTESIAN_POINT('Ctrl Pts',(-17.165485351815,-17.0532745693386,
-22.));
#115843=CARTESIAN_POINT('Ctrl Pts',(-17.2292147565865,-16.9918599247989,
-22.));
#115844=CARTESIAN_POINT('Ctrl Pts',(-17.2958558635168,-16.9339207318737,
-22.));
#115845=CARTESIAN_POINT('Ctrl Pts',(-17.3510487599444,-16.8859348561654,
-22.));
#115846=CARTESIAN_POINT('Ctrl Pts',(-17.4082400128264,-16.8403329410748,
-22.));
#115847=CARTESIAN_POINT('Ctrl Pts',(-17.4672777580111,-16.7972848189689,
-22.));
#115848=CARTESIAN_POINT('Ctrl Pts',(-17.4896865553589,-16.7809451596297,
-22.));
#115849=CARTESIAN_POINT('Ctrl Pts',(-17.5123617016702,-16.7649735008075,
-22.));
#115850=CARTESIAN_POINT('Ctrl Pts',(-17.5352952134256,-16.7493800153535,
-22.));
#115851=CARTESIAN_POINT('Ctrl Pts',(-17.5482870635507,-16.7405462951581,
-22.));
#115852=CARTESIAN_POINT('Ctrl Pts',(-17.561360861439,-16.7318346842869,
-22.));
#115853=CARTESIAN_POINT('Ctrl Pts',(-17.5745065855726,-16.7232523975405,
-22.));
#115854=CARTESIAN_POINT('Ctrl Pts',(-17.6490343908001,-16.674596348734,
-22.));
#115855=CARTESIAN_POINT('Ctrl Pts',(-17.7259443303905,-16.6300439893022,
-22.));
#115856=CARTESIAN_POINT('Ctrl Pts',(-17.8049555380688,-16.5898859241833,
-22.));
#115857=CARTESIAN_POINT('Ctrl Pts',(-17.8827967752859,-16.5503225057145,
-22.));
#115858=CARTESIAN_POINT('Ctrl Pts',(-17.962678191744,-16.51502348347,-22.));
#115859=CARTESIAN_POINT('Ctrl Pts',(-18.0443636543755,-16.484304104371,
-22.));
#115860=CARTESIAN_POINT('Ctrl Pts',(-18.0530584200154,-16.4810342716093,
-22.));
#115861=CARTESIAN_POINT('Ctrl Pts',(-18.0617736504531,-16.47781636714,-22.));
#115862=CARTESIAN_POINT('Ctrl Pts',(-18.0705089302108,-16.4746502607264,
-22.));
#115863=CARTESIAN_POINT('Ctrl Pts',(-19.3957372685685,-16.4790050975816,
-22.));
#115864=CARTESIAN_POINT('Ctrl Pts',(-19.4773890957418,-16.5085693309101,
-22.));
#115865=CARTESIAN_POINT('Ctrl Pts',(-19.5571492106161,-16.5425339973349,
-22.));
#115866=CARTESIAN_POINT('Ctrl Pts',(-19.6348155858968,-16.5805812675105,
-22.));
#115867=CARTESIAN_POINT('Ctrl Pts',(-19.7143272387952,-16.6195325038595,
-22.));
#115868=CARTESIAN_POINT('Ctrl Pts',(-19.7916452000862,-16.662763296461,
-22.));
#115869=CARTESIAN_POINT('Ctrl Pts',(-19.8665232562821,-16.7099790585762,
-22.));
#115870=CARTESIAN_POINT('Ctrl Pts',(-19.9365886725381,-16.754160120352,
-22.));
#115871=CARTESIAN_POINT('Ctrl Pts',(-20.0045178827344,-16.8018313324451,
-22.));
#115872=CARTESIAN_POINT('Ctrl Pts',(-20.0700783280693,-16.8527788406207,
-22.));
#115873=CARTESIAN_POINT('Ctrl Pts',(-20.0997467181299,-16.8758343665167,
-22.));
#115874=CARTESIAN_POINT('Ctrl Pts',(-20.1289295668893,-16.8995611421252,
-22.));
#115875=CARTESIAN_POINT('Ctrl Pts',(-20.1576029328649,-16.9239406308391,
-22.));
#115876=CARTESIAN_POINT('Ctrl Pts',(-20.1753081453826,-16.9389944626467,
-22.));
#115877=CARTESIAN_POINT('Ctrl Pts',(-20.1928190712341,-16.9542971752936,
-22.));
#115878=CARTESIAN_POINT('Ctrl Pts',(-20.2101297603596,-16.9698445175537,
-22.));
#115879=CARTESIAN_POINT('Ctrl Pts',(-20.2222917967556,-16.9807676726665,
-22.));
#115880=CARTESIAN_POINT('Ctrl Pts',(-20.2343567693431,-16.9918133788689,
-22.));
#115881=CARTESIAN_POINT('Ctrl Pts',(-20.2463057162916,-17.002964072546,
-22.));
#115882=CARTESIAN_POINT('Ctrl Pts',(-20.3097375002003,-17.0621582755838,
-22.));
#115883=CARTESIAN_POINT('Ctrl Pts',(-20.3700069454282,-17.1243998240975,
-22.));
#115884=CARTESIAN_POINT('Ctrl Pts',(-20.4268834922199,-17.1894105241984,
-22.));
#115885=CARTESIAN_POINT('Ctrl Pts',(-20.483037632838,-17.2535955037914,
-22.));
#115886=CARTESIAN_POINT('Ctrl Pts',(-20.535884967494,-17.3204805753055,
-22.));
#115887=CARTESIAN_POINT('Ctrl Pts',(-20.585161092451,-17.389824149674,-22.));
#115888=CARTESIAN_POINT('Ctrl Pts',(-20.6305983299564,-17.4537654693455,
-22.));
#115889=CARTESIAN_POINT('Ctrl Pts',(-20.6729989843627,-17.519797868898,
-22.));
#115890=CARTESIAN_POINT('Ctrl Pts',(-20.7121180645734,-17.5877431573068,
-22.));
#115891=CARTESIAN_POINT('Ctrl Pts',(-20.7391058385126,-17.6346177789475,
-22.));
#115892=CARTESIAN_POINT('Ctrl Pts',(-20.7645310103452,-17.6824030516845,
-22.));
#115893=CARTESIAN_POINT('Ctrl Pts',(-20.788301742955,-17.7310415486134,
-22.0000000000001));
#115894=CARTESIAN_POINT('Ctrl Pts',(-20.7942276911041,-17.7431669305097,
-22.0000000000001));
#115895=CARTESIAN_POINT('Ctrl Pts',(-20.8000469460378,-17.755337565341,
-22.));
#115896=CARTESIAN_POINT('Ctrl Pts',(-20.8057568391674,-17.7675488911101,
-22.));
#115897=CARTESIAN_POINT('Ctrl Pts',(-20.8408823751017,-17.8426692746921,
-22.));
#115898=CARTESIAN_POINT('Ctrl Pts',(-20.8718944728201,-17.9193714043448,
-22.));
#115899=CARTESIAN_POINT('Ctrl Pts',(-20.8985463344755,-17.9974267111826,
-22.));
#115900=CARTESIAN_POINT('Ctrl Pts',(-20.9251981961308,-18.0754820180205,
-22.));
#115901=CARTESIAN_POINT('Ctrl Pts',(-20.9474902938315,-18.1548912318264,
-22.));
#115902=CARTESIAN_POINT('Ctrl Pts',(-20.9651215210881,-18.2354350462128,
-22.));
#115903=CARTESIAN_POINT('Ctrl Pts',(-20.9829459910005,-18.3168616409281,
-22.));
#115904=CARTESIAN_POINT('Ctrl Pts',(-20.9960061241615,-18.3994490691394,
-22.));
#115905=CARTESIAN_POINT('Ctrl Pts',(-21.0043775797276,-18.4828058803714,
-22.));
#115906=CARTESIAN_POINT('Ctrl Pts',(-21.007836047032,-18.5172427598331,
-22.));
#115907=CARTESIAN_POINT('Ctrl Pts',(-21.0104936869016,-18.5518107962264,
-22.));
#115908=CARTESIAN_POINT('Ctrl Pts',(-21.012353412468,-18.5864814607357,
-22.));
#115909=CARTESIAN_POINT('Ctrl Pts',(-21.0130853706128,-18.6001272780164,
-22.));
#115910=CARTESIAN_POINT('Ctrl Pts',(-21.013693711025,-18.613790984168,-22.));
#115911=CARTESIAN_POINT('Ctrl Pts',(-21.0141781405805,-18.627453182305,
-22.));
#115912=CARTESIAN_POINT('Ctrl Pts',(-21.0170629011428,-18.7088110803349,
-22.));
#115913=CARTESIAN_POINT('Ctrl Pts',(-21.0155663446046,-18.7902456314198,
-22.));
#115914=CARTESIAN_POINT('Ctrl Pts',(-21.0098210964673,-18.8713996487605,
-22.));
#115915=CARTESIAN_POINT('Ctrl Pts',(-21.0040551877191,-18.9528455058144,
-22.));
#115916=CARTESIAN_POINT('Ctrl Pts',(-20.9940096006471,-19.0340098255527,
-22.));
#115917=CARTESIAN_POINT('Ctrl Pts',(-20.9797677148279,-19.1145199798923,
-22.));
#115918=CARTESIAN_POINT('Ctrl Pts',(-20.9656475419196,-19.1943420845335,
-22.));
#115919=CARTESIAN_POINT('Ctrl Pts',(-20.9474020500876,-19.2735220803043,
-22.));
#115920=CARTESIAN_POINT('Ctrl Pts',(-20.9250689726277,-19.3516710302886,
-22.));
#115921=CARTESIAN_POINT('Ctrl Pts',(-20.9157717541756,-19.3842042922679,
-22.));
#115922=CARTESIAN_POINT('Ctrl Pts',(-20.9057656547729,-19.4165584812898,
-22.));
#115923=CARTESIAN_POINT('Ctrl Pts',(-20.8950514146661,-19.4487036278629,
-22.));
#115924=CARTESIAN_POINT('Ctrl Pts',(-20.8895107411906,-19.4653269029819,
-22.));
#115925=CARTESIAN_POINT('Ctrl Pts',(-20.8837798105413,-19.4818963067406,
-22.));
#115926=CARTESIAN_POINT('Ctrl Pts',(-20.8778666083137,-19.4983863278128,
-22.));
#115927=CARTESIAN_POINT('Ctrl Pts',(-20.8511334402601,-19.5729365440179,
-22.));
#115928=CARTESIAN_POINT('Ctrl Pts',(-20.8206473963514,-19.6459626051823,
-22.));
#115929=CARTESIAN_POINT('Ctrl Pts',(-20.7864673296103,-19.7171052508947,
-22.));
#115930=CARTESIAN_POINT('Ctrl Pts',(-20.7601551154116,-19.771871689674,
-22.));
#115931=CARTESIAN_POINT('Ctrl Pts',(-20.7316528766953,-19.8255216226873,
-22.));
#115932=CARTESIAN_POINT('Ctrl Pts',(-20.7009722593753,-19.8778764706885,
-22.));
#115933=CARTESIAN_POINT('Ctrl Pts',(-20.691737989898,-19.893634262321,-22.));
#115934=CARTESIAN_POINT('Ctrl Pts',(-20.6823062983705,-19.9092746300216,
-22.));
#115935=CARTESIAN_POINT('Ctrl Pts',(-20.6726772909679,-19.9247924234514,
-22.));
#115936=CARTESIAN_POINT('Ctrl Pts',(-20.6644523795805,-19.9380474216617,
-22.));
#115937=CARTESIAN_POINT('Ctrl Pts',(-20.6560857687532,-19.9512092205436,
-22.));
#115938=CARTESIAN_POINT('Ctrl Pts',(-20.6475820686168,-19.9642683076145,
-22.));
#115939=CARTESIAN_POINT('Ctrl Pts',(-20.6064305516755,-20.0274644733087,
-22.));
#115940=CARTESIAN_POINT('Ctrl Pts',(-20.5620419166416,-20.0883056868182,
-22.));
#115941=CARTESIAN_POINT('Ctrl Pts',(-20.5144495392311,-20.1464522171397,
-22.));
#115942=CARTESIAN_POINT('Ctrl Pts',(-20.4703172870207,-20.2003713000042,
-22.));
#115943=CARTESIAN_POINT('Ctrl Pts',(-20.4234296568856,-20.2519733998006,
-22.));
#115944=CARTESIAN_POINT('Ctrl Pts',(-20.3737906915119,-20.3009544512441,
-22.));
#115945=CARTESIAN_POINT('Ctrl Pts',(-20.368202130628,-20.3064689414452,
-22.));
#115946=CARTESIAN_POINT('Ctrl Pts',(-20.3625786754248,-20.3119501712233,
-22.));
#115947=CARTESIAN_POINT('Ctrl Pts',(-20.3569206944252,-20.3173979915434,
-22.));
#115948=CARTESIAN_POINT('Ctrl Pts',(-23.5308805332535,12.9159404490031,
-3.78088374166161));
#115949=CARTESIAN_POINT('Ctrl Pts',(-23.4920947707073,12.3929457330403,
-3.32818299800387));
#115950=CARTESIAN_POINT('Ctrl Pts',(-23.414527126525,11.1227145575666,-2.68291372642237));
#115951=CARTESIAN_POINT('Ctrl Pts',(-23.2981776007066,8.98517233796921,
-2.72051551203619));
#115952=CARTESIAN_POINT('Ctrl Pts',(-23.1818319557984,7.11449327439195,
-3.75456823383891));
#115953=CARTESIAN_POINT('Ctrl Pts',(-23.0654863108902,5.94567083410245,
-5.54430593302147));
#115954=CARTESIAN_POINT('Ctrl Pts',(-22.949140665982,5.75110708678027,-7.67299084799178));
#115955=CARTESIAN_POINT('Ctrl Pts',(-22.8327950210738,6.57598682635251,
-9.64497510434418));
#115956=CARTESIAN_POINT('Ctrl Pts',(-22.7164493761656,8.22829836165371,
-11.0010927381981));
#115957=CARTESIAN_POINT('Ctrl Pts',(-22.6001037312574,10.3232843871488,
-11.4255808825339));
#115958=CARTESIAN_POINT('Ctrl Pts',(-22.4837580863492,12.373152711629,-10.8195997802356));
#115959=CARTESIAN_POINT('Ctrl Pts',(-22.367412441441,13.9005991739366,-9.32424845126734));
#115960=CARTESIAN_POINT('Ctrl Pts',(-22.2510667965328,14.5499677602782,
-7.28771036251242));
#115961=CARTESIAN_POINT('Ctrl Pts',(-22.1347211516246,14.1700608207003,
-5.18418037574749));
#115962=CARTESIAN_POINT('Ctrl Pts',(-22.0183755067164,12.8493270829512,
-3.5034534546303));
#115963=CARTESIAN_POINT('Ctrl Pts',(-21.9020298618082,10.8953137792879,
-2.63687434737169));
#115964=CARTESIAN_POINT('Ctrl Pts',(-21.7856842169001,8.76295316144695,
-2.78622511569276));
#115965=CARTESIAN_POINT('Ctrl Pts',(-21.6693385719918,6.94885218972505,
-3.91672099675241));
#115966=CARTESIAN_POINT('Ctrl Pts',(-21.5529929270836,5.87520384764723,
-5.7651525900255));
#115967=CARTESIAN_POINT('Ctrl Pts',(-21.4366472821754,5.79243819862009,
-7.90108306247407));
#115968=CARTESIAN_POINT('Ctrl Pts',(-21.3203016372673,6.71891118246527,
-9.82725987337206));
#115969=CARTESIAN_POINT('Ctrl Pts',(-21.2039559923591,8.44081429108934,
-11.0950054485607));
#115970=CARTESIAN_POINT('Ctrl Pts',(-21.0876103474509,10.5532071885089,
-11.4095079136007));
#115971=CARTESIAN_POINT('Ctrl Pts',(-20.9712647025427,12.5726070805758,
-10.6967524773169));
#115972=CARTESIAN_POINT('Ctrl Pts',(-20.8549190576345,14.01129149844,-9.12434942623869));
#115973=CARTESIAN_POINT('Ctrl Pts',(-20.6997915310902,14.7563922376921,
-6.36488911986088));
#115974=CARTESIAN_POINT('Ctrl Pts',(-20.5058821229099,12.994051845457,-2.90538039035574));
#115975=CARTESIAN_POINT('Ctrl Pts',(-20.2731908330935,8.33355232269001,
-2.33672443840605));
#115976=CARTESIAN_POINT('Ctrl Pts',(-20.0792814249132,5.79107032299367,
-5.27097555050355));
#115977=CARTESIAN_POINT('Ctrl Pts',(-19.9241538983689,5.85079178660098,
-8.12863711914554));
#115978=CARTESIAN_POINT('Ctrl Pts',(-19.8078082534607,6.86917854738371,
-10.0008424002799));
#115979=CARTESIAN_POINT('Ctrl Pts',(-19.6914626085525,8.65794742930395,
-11.1782557190028));
#115980=CARTESIAN_POINT('Ctrl Pts',(-19.5751169636443,10.7839875685715,
-11.3809103015019));
#115981=CARTESIAN_POINT('Ctrl Pts',(-19.4587713187361,12.7602040696624,
-10.5643948394832));
#115982=CARTESIAN_POINT('Ctrl Pts',(-19.3424256738279,14.1226489554401,
-8.91750284853353));
#115983=CARTESIAN_POINT('Ctrl Pts',(-19.2260800289197,14.5559010795726,
-6.82433736708493));
#115984=CARTESIAN_POINT('Ctrl Pts',(-19.1097343840116,13.9582122926688,
-4.77197574410858));
#115985=CARTESIAN_POINT('Ctrl Pts',(-18.9933887391034,12.4691657270705,
-3.23844269973861));
#115986=CARTESIAN_POINT('Ctrl Pts',(-18.8770430941952,10.4352783026865,
-2.58074261501136));
#115987=CARTESIAN_POINT('Ctrl Pts',(-18.760697449287,8.33022292180678,-2.95205001253969));
#115988=CARTESIAN_POINT('Ctrl Pts',(-18.6443518043788,6.64410352432277,
-4.2658924562235));
#115989=CARTESIAN_POINT('Ctrl Pts',(-18.5280061594706,5.76954396207305,
-6.21635733927994));
#115990=CARTESIAN_POINT('Ctrl Pts',(-18.4116605145624,5.91017031183124,
-8.34928752511129));
#115991=CARTESIAN_POINT('Ctrl Pts',(-18.2953148696542,7.0332421902222,-10.1680447514146));
#115992=CARTESIAN_POINT('Ctrl Pts',(-18.178969224746,8.87725972928098,-11.2491426006833));
#115993=CARTESIAN_POINT('Ctrl Pts',(-18.0626235798378,11.0128500131701,
-11.3408528567028));
#115994=CARTESIAN_POINT('Ctrl Pts',(-17.9462779349296,12.9427659614882,
-10.4218246313654));
#115995=CARTESIAN_POINT('Ctrl Pts',(-17.8299322900214,14.2176127610098,
-8.70604080762527));
#115996=CARTESIAN_POINT('Ctrl Pts',(-17.7135866451132,14.5406046262916,
-6.59302619008096));
#115997=CARTESIAN_POINT('Ctrl Pts',(-17.597241000205,13.8364209745585,-4.57475160186675));
#115998=CARTESIAN_POINT('Ctrl Pts',(-17.4808953552968,12.2692662804362,
-3.12122783010914));
#115999=CARTESIAN_POINT('Ctrl Pts',(-17.3645497103886,10.2035478774237,
-2.57077055143018));
#116000=CARTESIAN_POINT('Ctrl Pts',(-17.2869859471165,8.81549756936472,
-2.89162768514917));
#116001=CARTESIAN_POINT('Ctrl Pts',(-17.2482040654804,8.19904022858213,
-3.20522926485876));
#116002=CARTESIAN_POINT('Ctrl Pts',(-23.6934851051207,13.100263928033,-3.56793868900448));
#116003=CARTESIAN_POINT('Ctrl Pts',(-23.6546993425745,12.5426730283998,
-3.08529171912816));
#116004=CARTESIAN_POINT('Ctrl Pts',(-23.5771316983922,11.1884158585721,
-2.39733778256787));
#116005=CARTESIAN_POINT('Ctrl Pts',(-23.4607821725738,8.90947488106098,
-2.43742693228256));
#116006=CARTESIAN_POINT('Ctrl Pts',(-23.3444365276657,6.91505009979918,
-3.53988240615246));
#116007=CARTESIAN_POINT('Ctrl Pts',(-23.2280908827574,5.66890986912247,
-5.4480115388869));
#116008=CARTESIAN_POINT('Ctrl Pts',(-23.1117452378493,5.46147569895942,
-7.71750929966068));
#116009=CARTESIAN_POINT('Ctrl Pts',(-22.9953995929411,6.34092136454444,
-9.81994062831756));
#116010=CARTESIAN_POINT('Ctrl Pts',(-22.8790539480329,8.10253357079198,
-11.265765659412));
#116011=CARTESIAN_POINT('Ctrl Pts',(-22.7627083031247,10.3361032551902,
-11.7183337620325));
#116012=CARTESIAN_POINT('Ctrl Pts',(-22.6463626582165,12.5215706954729,
-11.0722669134044));
#116013=CARTESIAN_POINT('Ctrl Pts',(-22.5300170133083,14.1500579842821,
-9.47799785611141));
#116014=CARTESIAN_POINT('Ctrl Pts',(-22.4136713684001,14.8423824059262,
-7.30674244876793));
#116015=CARTESIAN_POINT('Ctrl Pts',(-22.2973257234919,14.4373445618512,
-5.06406361870253));
#116016=CARTESIAN_POINT('Ctrl Pts',(-22.1809800785837,13.0292440772185,
-3.27215634434632));
#116017=CARTESIAN_POINT('Ctrl Pts',(-22.0646344336755,10.9459724826303,
-2.34825289126802));
#116018=CARTESIAN_POINT('Ctrl Pts',(-21.9482887887673,8.67255587065623,
-2.50748323667555));
#116019=CARTESIAN_POINT('Ctrl Pts',(-21.8319431438591,6.73845183102772,
-3.71276160013153));
#116020=CARTESIAN_POINT('Ctrl Pts',(-21.7155974989509,5.59378148030178,
-5.68346723738891));
#116021=CARTESIAN_POINT('Ctrl Pts',(-21.5992518540427,5.50554087042331,
-7.96068985042091));
#116022=CARTESIAN_POINT('Ctrl Pts',(-21.4829062091345,6.49330018955362,
-10.0142835638186));
#116023=CARTESIAN_POINT('Ctrl Pts',(-21.3665605642263,8.32910746277151,
-11.3658907105068));
#116024=CARTESIAN_POINT('Ctrl Pts',(-21.2502149193181,10.5812354864414,
-11.7011975636472));
#116025=CARTESIAN_POINT('Ctrl Pts',(-21.1338692744099,12.7342190026592,
-10.9412932418523));
#116026=CARTESIAN_POINT('Ctrl Pts',(-21.0175236295017,14.2680726236628,
-9.26487547877277));
#116027=CARTESIAN_POINT('Ctrl Pts',(-20.8623961029575,15.0624618953634,
-6.32287643409223));
#116028=CARTESIAN_POINT('Ctrl Pts',(-20.6684866947772,13.1835424057901,
-2.63452065171533));
#116029=CARTESIAN_POINT('Ctrl Pts',(-20.4357954049608,8.21475009809699,
-2.02824801806984));
#116030=CARTESIAN_POINT('Ctrl Pts',(-20.2418859967804,5.50408250960656,
-5.15660030807799));
#116031=CARTESIAN_POINT('Ctrl Pts',(-20.0867584702362,5.56775455753331,
-8.20329664414551));
#116032=CARTESIAN_POINT('Ctrl Pts',(-19.970412825328,6.65350776456926,-10.1993486024987));
#116033=CARTESIAN_POINT('Ctrl Pts',(-19.8540671804198,8.56060399262535,
-11.4546479995839));
#116034=CARTESIAN_POINT('Ctrl Pts',(-19.7377215355116,10.8272820253628,
-11.6707082149582));
#116035=CARTESIAN_POINT('Ctrl Pts',(-19.6213758906034,12.9342255624209,
-10.8001801252177));
#116036=CARTESIAN_POINT('Ctrl Pts',(-19.5050302456952,14.3867963941607,
-9.04434596704268));
#116037=CARTESIAN_POINT('Ctrl Pts',(-19.388684600787,14.8487082152359,-6.8127172559693));
#116038=CARTESIAN_POINT('Ctrl Pts',(-19.2723389558788,14.211482219985,-4.62459158509811));
#116039=CARTESIAN_POINT('Ctrl Pts',(-19.1559933109706,12.6239349871618,
-2.98961508585478));
#116040=CARTESIAN_POINT('Ctrl Pts',(-19.0396476660624,10.4555055860592,
-2.28840803588138));
#116041=CARTESIAN_POINT('Ctrl Pts',(-18.9233020211542,8.2112004568156,-2.68427747683199));
#116042=CARTESIAN_POINT('Ctrl Pts',(-18.8069563762461,6.41354399292294,
-4.08503080720052));
#116043=CARTESIAN_POINT('Ctrl Pts',(-18.6906107313378,5.48113217648616,
-6.16451925259414));
#116044=CARTESIAN_POINT('Ctrl Pts',(-18.5742650864296,5.6310609816548,-8.43854310957185));
#116045=CARTESIAN_POINT('Ctrl Pts',(-18.4579194415215,6.82842424348439,
-10.3776114157632));
#116046=CARTESIAN_POINT('Ctrl Pts',(-18.3415737966133,8.79442383613891,
-11.5302240597658));
#116047=CARTESIAN_POINT('Ctrl Pts',(-18.2252281517051,11.0712837570842,
-11.6280009638123));
#116048=CARTESIAN_POINT('Ctrl Pts',(-18.1088825067969,13.128863952437,-10.6481788751495));
#116049=CARTESIAN_POINT('Ctrl Pts',(-17.9925368618887,14.4880420705777,
-8.8188956784843));
#116050=CARTESIAN_POINT('Ctrl Pts',(-17.8761912169805,14.8323998991367,
-6.56610480780444));
#116051=CARTESIAN_POINT('Ctrl Pts',(-17.7598455720723,14.0816343868042,
-4.4143210344682));
#116052=CARTESIAN_POINT('Ctrl Pts',(-17.6434999271641,12.4108121603283,
-2.86464643395019));
#116053=CARTESIAN_POINT('Ctrl Pts',(-17.5271542822559,10.2084461562965,
-2.27777631870772));
#116054=CARTESIAN_POINT('Ctrl Pts',(-17.4495905189838,8.72857609951769,
-2.61985820287125));
#116055=CARTESIAN_POINT('Ctrl Pts',(-17.4108086373477,8.07134000756269,
-2.9542045769733));
#116056=CARTESIAN_POINT('Ctrl Pts',(-23.856089676988,13.284587407063,-3.35499363634734));
#116057=CARTESIAN_POINT('Ctrl Pts',(-23.8173039144417,12.6924003237593,
-2.84240044025244));
#116058=CARTESIAN_POINT('Ctrl Pts',(-23.7397362702595,11.2541171595776,
-2.11176183871335));
#116059=CARTESIAN_POINT('Ctrl Pts',(-23.6233867444411,8.83377742415274,
-2.15433835252893));
#116060=CARTESIAN_POINT('Ctrl Pts',(-23.5070410995329,6.7156069252064,-3.325196578466));
#116061=CARTESIAN_POINT('Ctrl Pts',(-23.3906954546247,5.39214890414247,
-5.35171714475233));
#116062=CARTESIAN_POINT('Ctrl Pts',(-23.2743498097165,5.17184431113857,
-7.76202775132957));
#116063=CARTESIAN_POINT('Ctrl Pts',(-23.1580041648084,6.10585590273637,
-9.99490615229094));
#116064=CARTESIAN_POINT('Ctrl Pts',(-23.0416585199001,7.97676877993027,
-11.530438580626));
#116065=CARTESIAN_POINT('Ctrl Pts',(-22.925312874992,10.3489221232315,-12.0110866415312));
#116066=CARTESIAN_POINT('Ctrl Pts',(-22.8089672300837,12.669988679317,-11.3249340465732));
#116067=CARTESIAN_POINT('Ctrl Pts',(-22.6926215851756,14.3995167946276,
-9.63174726095547));
#116068=CARTESIAN_POINT('Ctrl Pts',(-22.5762759402673,15.1347970515741,
-7.32577453502343));
#116069=CARTESIAN_POINT('Ctrl Pts',(-22.4599302953592,14.7046283030022,
-4.94394686165757));
#116070=CARTESIAN_POINT('Ctrl Pts',(-22.343584650451,13.2091610714859,-3.04085923406232));
#116071=CARTESIAN_POINT('Ctrl Pts',(-22.2272390055428,10.9966311859728,
-2.05963143516434));
#116072=CARTESIAN_POINT('Ctrl Pts',(-22.1108933606346,8.58215857986552,
-2.22874135765833));
#116073=CARTESIAN_POINT('Ctrl Pts',(-21.9945477157264,6.5280514723304,-3.50880220351063));
#116074=CARTESIAN_POINT('Ctrl Pts',(-21.8782020708182,5.31235911295633,
-5.60178188475233));
#116075=CARTESIAN_POINT('Ctrl Pts',(-21.76185642591,5.21864354222653,-8.02029663836774));
#116076=CARTESIAN_POINT('Ctrl Pts',(-21.6455107810018,6.26768919664197,
-10.201307254265));
#116077=CARTESIAN_POINT('Ctrl Pts',(-21.5291651360936,8.21740063445369,
-11.6367759724529));
#116078=CARTESIAN_POINT('Ctrl Pts',(-21.4128194911854,10.609263784374,-11.9928872136937));
#116079=CARTESIAN_POINT('Ctrl Pts',(-21.2964738462772,12.8958309247427,
-11.1858340063878));
#116080=CARTESIAN_POINT('Ctrl Pts',(-21.180128201369,14.5248537488857,-9.40540153130685));
#116081=CARTESIAN_POINT('Ctrl Pts',(-21.0250006748248,15.3685315530349,
-6.28086374832358));
#116082=CARTESIAN_POINT('Ctrl Pts',(-20.8310912666444,13.3730329661233,
-2.36366091307492));
#116083=CARTESIAN_POINT('Ctrl Pts',(-20.598399976828,8.09594787350394,-1.71977159773362));
#116084=CARTESIAN_POINT('Ctrl Pts',(-20.4044905686477,5.21709469621947,
-5.04222506565243));
#116085=CARTESIAN_POINT('Ctrl Pts',(-20.2493630421035,5.28471732846564,
-8.27795616914549));
#116086=CARTESIAN_POINT('Ctrl Pts',(-20.1330173971953,6.43783698175481,
-10.3978548047174));
#116087=CARTESIAN_POINT('Ctrl Pts',(-20.0166717522871,8.46326055594674,
-11.7310402801651));
#116088=CARTESIAN_POINT('Ctrl Pts',(-19.9003261073789,10.8705764821541,
-11.9605061284144));
#116089=CARTESIAN_POINT('Ctrl Pts',(-19.7839804624707,13.1082470551796,
-11.0359654109521));
#116090=CARTESIAN_POINT('Ctrl Pts',(-19.6676348175625,14.6509438328813,
-9.17118908555184));
#116091=CARTESIAN_POINT('Ctrl Pts',(-19.5512891726543,15.1415153508992,
-6.80109714485368));
#116092=CARTESIAN_POINT('Ctrl Pts',(-19.4349435277461,14.464752147301,-4.47720742608763));
#116093=CARTESIAN_POINT('Ctrl Pts',(-19.3185978828379,12.7787042472532,
-2.74078747197094));
#116094=CARTESIAN_POINT('Ctrl Pts',(-19.2022522379297,10.4757328694319,
-1.9960734567514));
#116095=CARTESIAN_POINT('Ctrl Pts',(-19.0859065930215,8.09217799182441,
-2.41650494112427));
#116096=CARTESIAN_POINT('Ctrl Pts',(-18.9695609481133,6.18298446152309,
-3.90416915817754));
#116097=CARTESIAN_POINT('Ctrl Pts',(-18.8532153032051,5.19272039089927,
-6.11268116590833));
#116098=CARTESIAN_POINT('Ctrl Pts',(-18.7368696582969,5.35195165147837,
-8.52779869403239));
#116099=CARTESIAN_POINT('Ctrl Pts',(-18.6205240133887,6.62360629674656,
-10.5871780801117));
#116100=CARTESIAN_POINT('Ctrl Pts',(-18.5041783684805,8.71158794299683,
-11.8113055188485));
#116101=CARTESIAN_POINT('Ctrl Pts',(-18.3878327235723,11.1297175009982,
-11.9151490709219));
#116102=CARTESIAN_POINT('Ctrl Pts',(-18.2714870786641,13.3149619433859,
-10.8745331189337));
#116103=CARTESIAN_POINT('Ctrl Pts',(-18.155141433756,14.7584713801457,-8.93175054934334));
#116104=CARTESIAN_POINT('Ctrl Pts',(-18.0387957888477,15.1241951719818,
-6.53918342552792));
#116105=CARTESIAN_POINT('Ctrl Pts',(-17.9224501439396,14.3268477990501,
-4.25389046706965));
#116106=CARTESIAN_POINT('Ctrl Pts',(-17.8061044990314,12.5523580402204,
-2.60806503779124));
#116107=CARTESIAN_POINT('Ctrl Pts',(-17.6897588541232,10.2133444351692,
-1.98478208598528));
#116108=CARTESIAN_POINT('Ctrl Pts',(-17.612195090851,8.64165462967066,-2.34808872059334));
#116109=CARTESIAN_POINT('Ctrl Pts',(-17.573413209215,7.94363978654326,-2.70317988908784));
#116110=CARTESIAN_POINT('Ctrl Pts',(-24.0186942488553,13.4689108860931,
-3.1420485836902));
#116111=CARTESIAN_POINT('Ctrl Pts',(-23.979908486309,12.8421276191188,-2.59950916137671));
#116112=CARTESIAN_POINT('Ctrl Pts',(-23.9023408421268,11.3198184605831,
-1.82618589485885));
#116113=CARTESIAN_POINT('Ctrl Pts',(-23.7859913163084,8.75807996724451,
-1.8712497727753));
#116114=CARTESIAN_POINT('Ctrl Pts',(-23.6696456714002,6.51616375061362,
-3.11051075077954));
#116115=CARTESIAN_POINT('Ctrl Pts',(-23.553300026492,5.11538793916249,-5.25542275061777));
#116116=CARTESIAN_POINT('Ctrl Pts',(-23.4369543815838,4.88221292331772,
-7.80654620299846));
#116117=CARTESIAN_POINT('Ctrl Pts',(-23.3206087366756,5.8707904409283,-10.1698716762644));
#116118=CARTESIAN_POINT('Ctrl Pts',(-23.2042630917674,7.85100398906855,
-11.7951115018399));
#116119=CARTESIAN_POINT('Ctrl Pts',(-23.0879174468592,10.3617409912729,
-12.3038395210299));
#116120=CARTESIAN_POINT('Ctrl Pts',(-22.971571801951,12.818406663161,-11.5776011797419));
#116121=CARTESIAN_POINT('Ctrl Pts',(-22.8552261570428,14.6489756049733,
-9.78549666579953));
#116122=CARTESIAN_POINT('Ctrl Pts',(-22.7388805121346,15.4272116972221,
-7.34480662127895));
#116123=CARTESIAN_POINT('Ctrl Pts',(-22.6225348672265,14.971912044153,-4.82383010461261));
#116124=CARTESIAN_POINT('Ctrl Pts',(-22.5061892223183,13.3890780657532,
-2.80956212377835));
#116125=CARTESIAN_POINT('Ctrl Pts',(-22.38984357741,11.0472898893152,-1.77100997906067));
#116126=CARTESIAN_POINT('Ctrl Pts',(-22.2734979325019,8.49176128907481,
-1.94999947864112));
#116127=CARTESIAN_POINT('Ctrl Pts',(-22.1571522875937,6.31765111363307,
-3.30484280688975));
#116128=CARTESIAN_POINT('Ctrl Pts',(-22.0408066426855,5.03093674561089,
-5.52009653211574));
#116129=CARTESIAN_POINT('Ctrl Pts',(-21.9244609977773,4.93174621402975,
-8.07990342631457));
#116130=CARTESIAN_POINT('Ctrl Pts',(-21.8081153528691,6.04207820373032,
-10.3883309447114));
#116131=CARTESIAN_POINT('Ctrl Pts',(-21.6917697079609,8.10569380613587,
-11.907661234399));
#116132=CARTESIAN_POINT('Ctrl Pts',(-21.5754240630527,10.6372920823065,
-12.2845768637402));
#116133=CARTESIAN_POINT('Ctrl Pts',(-21.4590784181445,13.0574428468262,
-11.4303747709233));
#116134=CARTESIAN_POINT('Ctrl Pts',(-21.3427327732363,14.7816348741085,
-9.54592758384092));
#116135=CARTESIAN_POINT('Ctrl Pts',(-21.187605246692,15.6746012107064,-6.23885106255491));
#116136=CARTESIAN_POINT('Ctrl Pts',(-20.9936958385117,13.5625235264562,
-2.09280117443452));
#116137=CARTESIAN_POINT('Ctrl Pts',(-20.7610045486953,7.97714564891089,
-1.41129517739739));
#116138=CARTESIAN_POINT('Ctrl Pts',(-20.567095140515,4.93010688283236,-4.9278498232269));
#116139=CARTESIAN_POINT('Ctrl Pts',(-20.4119676139707,5.00168009939798,
-8.35261569414545));
#116140=CARTESIAN_POINT('Ctrl Pts',(-20.2956219690625,6.22216619894035,
-10.5963610069362));
#116141=CARTESIAN_POINT('Ctrl Pts',(-20.1792763241544,8.36591711926816,
-12.0074325607462));
#116142=CARTESIAN_POINT('Ctrl Pts',(-20.0629306792461,10.9138709389455,
-12.2503040418707));
#116143=CARTESIAN_POINT('Ctrl Pts',(-19.946585034338,13.2822685479382,-11.2717506966864));
#116144=CARTESIAN_POINT('Ctrl Pts',(-19.8302393894298,14.915091271602,-9.298032204061));
#116145=CARTESIAN_POINT('Ctrl Pts',(-19.7138937445216,15.4343224865625,
-6.78947703373806));
#116146=CARTESIAN_POINT('Ctrl Pts',(-19.5975480996134,14.7180220746172,
-4.32982326707715));
#116147=CARTESIAN_POINT('Ctrl Pts',(-19.4812024547052,12.9334735073446,
-2.49195985808711));
#116148=CARTESIAN_POINT('Ctrl Pts',(-19.364856809797,10.4959601528046,-1.70373887762141));
#116149=CARTESIAN_POINT('Ctrl Pts',(-19.2485111648888,7.97315552683322,
-2.14873240541657));
#116150=CARTESIAN_POINT('Ctrl Pts',(-19.1321655199806,5.95242493012327,
-3.72330750915457));
#116151=CARTESIAN_POINT('Ctrl Pts',(-19.0158198750724,4.90430860531238,
-6.06084307922253));
#116152=CARTESIAN_POINT('Ctrl Pts',(-18.8994742301642,5.07284232130192,
-8.61705427849294));
#116153=CARTESIAN_POINT('Ctrl Pts',(-18.783128585256,6.41878835000875,-10.7967447444602));
#116154=CARTESIAN_POINT('Ctrl Pts',(-18.6667829403478,8.62875204985474,
-12.092386977931));
#116155=CARTESIAN_POINT('Ctrl Pts',(-18.5504372954396,11.1881512449122,
-12.2022971780315));
#116156=CARTESIAN_POINT('Ctrl Pts',(-18.4340916505314,13.5010599343348,
-11.1008873627179));
#116157=CARTESIAN_POINT('Ctrl Pts',(-18.3177460056232,15.0289006897138,
-9.04460542020237));
#116158=CARTESIAN_POINT('Ctrl Pts',(-18.201400360715,15.4159904448268,-6.5122620432514));
#116159=CARTESIAN_POINT('Ctrl Pts',(-18.0850547158068,14.572061211296,-4.0934598996711));
#116160=CARTESIAN_POINT('Ctrl Pts',(-17.9687090708987,12.6939039201125,
-2.35148364163229));
#116161=CARTESIAN_POINT('Ctrl Pts',(-17.8523634259905,10.218242714042,-1.69178785326283));
#116162=CARTESIAN_POINT('Ctrl Pts',(-17.7747996627183,8.55473315982364,
-2.07631923831543));
#116163=CARTESIAN_POINT('Ctrl Pts',(-17.7360177810823,7.81593956552383,
-2.45215520120238));
#116164=CARTESIAN_POINT('Ctrl Pts',(-17.734,7.81752421401937,-2.45527019889639));
#116165=CARTESIAN_POINT('Ctrl Pts',(-17.734,7.95501332932841,-2.39880616079668));
#116166=CARTESIAN_POINT('Ctrl Pts',(-17.734,8.09483307093979,-2.34855996252214));
#116167=CARTESIAN_POINT('Ctrl Pts',(-17.734,8.23654961332739,-2.304582486642));
#116168=CARTESIAN_POINT('Ctrl Pts',(-17.734,8.37832975988065,-2.26058527311788));
#116169=CARTESIAN_POINT('Ctrl Pts',(-17.734,8.52200921313304,-2.22286236353948));
#116170=CARTESIAN_POINT('Ctrl Pts',(-17.734,8.6671587240801,-2.19151622070739));
#116171=CARTESIAN_POINT('Ctrl Pts',(-17.734,8.73062405356116,-2.1778103992422));
#116172=CARTESIAN_POINT('Ctrl Pts',(-17.734,8.79437042286563,-2.16532435434159));
#116173=CARTESIAN_POINT('Ctrl Pts',(-17.734,8.85836166295589,-2.15406978045215));
#116174=CARTESIAN_POINT('Ctrl Pts',(-17.734,8.89040869116538,-2.1484334520045));
#116175=CARTESIAN_POINT('Ctrl Pts',(-17.734,8.92251712887926,-2.14310601138361));
#116176=CARTESIAN_POINT('Ctrl Pts',(-17.734,8.95468239459414,-2.13808910834503));
#116177=CARTESIAN_POINT('Ctrl Pts',(-17.734,8.98448154595258,-2.13344125452896));
#116178=CARTESIAN_POINT('Ctrl Pts',(-17.734,9.01432763175263,-2.12906034010219));
#116179=CARTESIAN_POINT('Ctrl Pts',(-17.734,9.04419731169371,-2.12495001478239));
#116180=CARTESIAN_POINT('Ctrl Pts',(-17.734,9.18914015305572,-2.10500463097011));
#116181=CARTESIAN_POINT('Ctrl Pts',(-17.734,9.33476318988617,-2.09140666587328));
#116182=CARTESIAN_POINT('Ctrl Pts',(-17.734,9.48065042336444,-2.08424512751231));
#116183=CARTESIAN_POINT('Ctrl Pts',(-17.734,9.62430709076033,-2.07719308663227));
#116184=CARTESIAN_POINT('Ctrl Pts',(-17.734,9.76822064380685,-2.07638225413068));
#116185=CARTESIAN_POINT('Ctrl Pts',(-17.734,9.91198516021645,-2.08194693812594));
#116186=CARTESIAN_POINT('Ctrl Pts',(-17.734,9.99104601795219,-2.08500714171915));
#116187=CARTESIAN_POINT('Ctrl Pts',(-17.734,10.0700615878024,-2.08999633223886));
#116188=CARTESIAN_POINT('Ctrl Pts',(-17.734,10.1489620547016,-2.09694320736949));
#116189=CARTESIAN_POINT('Ctrl Pts',(-17.734,10.1675473093435,-2.09857956578842));
#116190=CARTESIAN_POINT('Ctrl Pts',(-17.734,10.1861239058425,-2.10032440268515));
#116191=CARTESIAN_POINT('Ctrl Pts',(-17.734,10.204682003642,-2.10217705470482));
#116192=CARTESIAN_POINT('Ctrl Pts',(-17.734,10.2069686559161,-2.10240533084603));
#116193=CARTESIAN_POINT('Ctrl Pts',(-17.734,10.2092550663573,-2.10263524723068));
#116194=CARTESIAN_POINT('Ctrl Pts',(-17.734,10.2115412333789,-2.10286680408659));
#116195=CARTESIAN_POINT('Ctrl Pts',(-17.734,10.3540154766321,-2.11729745919824));
#116196=CARTESIAN_POINT('Ctrl Pts',(-17.734,10.4955450211138,-2.13809494422707));
#116197=CARTESIAN_POINT('Ctrl Pts',(-17.734,10.6357416460623,-2.16507440736953));
#116198=CARTESIAN_POINT('Ctrl Pts',(-17.734,10.7763962044387,-2.19214199530135));
#116199=CARTESIAN_POINT('Ctrl Pts',(-17.734,10.915709875811,-2.22543235084852));
#116200=CARTESIAN_POINT('Ctrl Pts',(-17.734,11.0532754223516,-2.26480926970525));
#116201=CARTESIAN_POINT('Ctrl Pts',(-17.734,11.1892331876652,-2.30372597543079));
#116202=CARTESIAN_POINT('Ctrl Pts',(-17.734,11.3234841068398,-2.34858822554395));
#116203=CARTESIAN_POINT('Ctrl Pts',(-17.734,11.4556098132251,-2.39930790770621));
#116204=CARTESIAN_POINT('Ctrl Pts',(-17.734,11.5858933052135,-2.44932041083996));
#116205=CARTESIAN_POINT('Ctrl Pts',(-17.734,11.7141110087283,-2.50502853561951));
#116206=CARTESIAN_POINT('Ctrl Pts',(-17.734,11.8398280865206,-2.56638422249516));
#116207=CARTESIAN_POINT('Ctrl Pts',(-17.734,11.8635810775125,-2.57797676905487));
#116208=CARTESIAN_POINT('Ctrl Pts',(-17.734,11.8872446880899,-2.58977102047971));
#116209=CARTESIAN_POINT('Ctrl Pts',(-17.734,11.9108158217838,-2.60176678408464));
#116210=CARTESIAN_POINT('Ctrl Pts',(-17.734,11.9371259496047,-2.61515646986953));
#116211=CARTESIAN_POINT('Ctrl Pts',(-17.734,11.9633250773611,-2.62879964621101));
#116212=CARTESIAN_POINT('Ctrl Pts',(-17.734,11.989373711485,-2.64267686049563));
#116213=CARTESIAN_POINT('Ctrl Pts',(-17.734,12.1092335086399,-2.7065312676527));
#116214=CARTESIAN_POINT('Ctrl Pts',(-17.734,12.2260636232258,-2.77541414480518));
#116215=CARTESIAN_POINT('Ctrl Pts',(-17.734,12.3395155043836,-2.84921040440292));
#116216=CARTESIAN_POINT('Ctrl Pts',(-17.734,12.3590922141296,-2.86194433124259));
#116217=CARTESIAN_POINT('Ctrl Pts',(-17.734,12.3785682723977,-2.87482464861868));
#116218=CARTESIAN_POINT('Ctrl Pts',(-17.734,12.397941804336,-2.88785087941439));
#116219=CARTESIAN_POINT('Ctrl Pts',(-17.734,12.5137183308796,-2.96569583614641));
#116220=CARTESIAN_POINT('Ctrl Pts',(-17.734,12.625836471894,-3.04874887784055));
#116221=CARTESIAN_POINT('Ctrl Pts',(-17.734,12.7340053685886,-3.13669684221413));
#116222=CARTESIAN_POINT('Ctrl Pts',(-17.734,12.8413651891065,-3.22398697790556));
#116223=CARTESIAN_POINT('Ctrl Pts',(-17.734,12.9448350524291,-3.31609977172436));
#116224=CARTESIAN_POINT('Ctrl Pts',(-17.734,13.0440889096059,-3.41275801808283));
#116225=CARTESIAN_POINT('Ctrl Pts',(-17.734,13.1288759097822,-3.49532773359962));
#116226=CARTESIAN_POINT('Ctrl Pts',(-17.734,13.2105858345264,-3.58121510518619));
#116227=CARTESIAN_POINT('Ctrl Pts',(-17.734,13.2889874920904,-3.67025872512399));
#116228=CARTESIAN_POINT('Ctrl Pts',(-17.734,13.3046808407887,-3.68808223320354));
#116229=CARTESIAN_POINT('Ctrl Pts',(-17.734,13.3202415499158,-3.70603222587404));
#116230=CARTESIAN_POINT('Ctrl Pts',(-17.734,13.3356676287495,-3.72410744241816));
#116231=CARTESIAN_POINT('Ctrl Pts',(-17.734,13.3480960124007,-3.73867016624531));
#116232=CARTESIAN_POINT('Ctrl Pts',(-17.734,13.3604375218648,-3.75331488553882));
#116233=CARTESIAN_POINT('Ctrl Pts',(-17.734,13.3726806466598,-3.76802811897179));
#116234=CARTESIAN_POINT('Ctrl Pts',(-17.734,13.4596595863362,-3.87255547327407));
#116235=CARTESIAN_POINT('Ctrl Pts',(-17.734,13.5418047089289,-3.98068713564629));
#116236=CARTESIAN_POINT('Ctrl Pts',(-17.734,13.6188521515589,-4.09212747512552));
#116237=CARTESIAN_POINT('Ctrl Pts',(-17.734,13.6955050681822,-4.20299717772693));
#116238=CARTESIAN_POINT('Ctrl Pts',(-17.734,13.7671127723516,-4.31714241929126));
#116239=CARTESIAN_POINT('Ctrl Pts',(-17.734,13.8333700251483,-4.43429573902715));
#116240=CARTESIAN_POINT('Ctrl Pts',(-17.734,13.8529952952312,-4.46899632566313));
#116241=CARTESIAN_POINT('Ctrl Pts',(-17.734,13.8721508267902,-4.50396094344829));
#116242=CARTESIAN_POINT('Ctrl Pts',(-17.734,13.89082783933,-4.53918291414616));
#116243=CARTESIAN_POINT('Ctrl Pts',(-17.734,13.9541037547201,-4.6585115505114));
#116244=CARTESIAN_POINT('Ctrl Pts',(-17.734,14.0118911506688,-4.78079380916986));
#116245=CARTESIAN_POINT('Ctrl Pts',(-17.734,14.0640355569298,-4.90562952893938));
#116246=CARTESIAN_POINT('Ctrl Pts',(-17.734,14.1069769502113,-5.00843288068094));
#116247=CARTESIAN_POINT('Ctrl Pts',(-17.734,14.1460905703569,-5.11296827640029));
#116248=CARTESIAN_POINT('Ctrl Pts',(-17.734,14.181263595494,-5.21901089821796));
#116249=CARTESIAN_POINT('Ctrl Pts',(-17.734,14.189228939926,-5.24302549474362));
#116250=CARTESIAN_POINT('Ctrl Pts',(-17.734,14.1969936498824,-5.26712264831227));
#116251=CARTESIAN_POINT('Ctrl Pts',(-17.734,14.2045469401604,-5.29126909440454));
#116252=CARTESIAN_POINT('Ctrl Pts',(-17.734,14.2441345445802,-5.41782320802469));
#116253=CARTESIAN_POINT('Ctrl Pts',(-17.734,14.2779661336648,-5.54586509835337));
#116254=CARTESIAN_POINT('Ctrl Pts',(-17.734,14.3059575691914,-5.67500275481729));
#116255=CARTESIAN_POINT('Ctrl Pts',(-17.734,14.3337111014893,-5.80304285180123));
#116256=CARTESIAN_POINT('Ctrl Pts',(-17.734,14.3557233452494,-5.93216096674691));
#116257=CARTESIAN_POINT('Ctrl Pts',(-17.734,14.3718618342398,-6.06197882817971));
#116258=CARTESIAN_POINT('Ctrl Pts',(-17.734,14.3878809810446,-6.19083670213723));
#116259=CARTESIAN_POINT('Ctrl Pts',(-17.734,14.3981129478511,-6.3203847452269));
#116260=CARTESIAN_POINT('Ctrl Pts',(-17.734,14.4023779577644,-6.45024544035567));
#116261=CARTESIAN_POINT('Ctrl Pts',(-17.734,14.404077015673,-6.50197822540308));
#116262=CARTESIAN_POINT('Ctrl Pts',(-17.734,14.4048285550272,-6.55376048351597));
#116263=CARTESIAN_POINT('Ctrl Pts',(-17.734,14.4046189505891,-6.60556761626202));
#116264=CARTESIAN_POINT('Ctrl Pts',(-17.734,14.4041999753073,-6.7091241450779));
#116265=CARTESIAN_POINT('Ctrl Pts',(-17.734,14.3999416905426,-6.8127807955209));
#116266=CARTESIAN_POINT('Ctrl Pts',(-17.734,14.3918515993157,-6.91632173312881));
#116267=CARTESIAN_POINT('Ctrl Pts',(-23.534,12.9193325810254,-3.77664721604209));
#116268=CARTESIAN_POINT('Ctrl Pts',(-23.534,12.8290342749467,-3.68176973928167));
#116269=CARTESIAN_POINT('Ctrl Pts',(-23.534,12.7344699653718,-3.59136003915295));
#116270=CARTESIAN_POINT('Ctrl Pts',(-23.534,12.6360835972834,-3.50554511160901));
#116271=CARTESIAN_POINT('Ctrl Pts',(-23.534,12.5375436323605,-3.41959621325707));
#116272=CARTESIAN_POINT('Ctrl Pts',(-23.534,12.4351690929809,-3.3382559634335));
#116273=CARTESIAN_POINT('Ctrl Pts',(-23.534,12.3293560803945,-3.26167549385162));
#116274=CARTESIAN_POINT('Ctrl Pts',(-23.534,12.2223961810545,-3.18426498338916));
#116275=CARTESIAN_POINT('Ctrl Pts',(-23.534,12.1119223277556,-3.11171743092941));
#116276=CARTESIAN_POINT('Ctrl Pts',(-23.534,11.9983009629288,-3.04422091350681));
#116277=CARTESIAN_POINT('Ctrl Pts',(-23.534,11.8876418446556,-2.97848411201814));
#116278=CARTESIAN_POINT('Ctrl Pts',(-23.534,11.7739964774381,-2.91753808376495));
#116279=CARTESIAN_POINT('Ctrl Pts',(-23.534,11.6576727871419,-2.86159294221042));
#116280=CARTESIAN_POINT('Ctrl Pts',(-23.534,11.6332495630019,-2.84984674736181));
#116281=CARTESIAN_POINT('Ctrl Pts',(-23.534,11.6087081820176,-2.83832114633447));
#116282=CARTESIAN_POINT('Ctrl Pts',(-23.534,11.5840513615887,-2.82701831535873));
#116283=CARTESIAN_POINT('Ctrl Pts',(-23.534,11.5622209636691,-2.81701113302431));
#116284=CARTESIAN_POINT('Ctrl Pts',(-23.534,11.5402959333441,-2.80717685242453));
#116285=CARTESIAN_POINT('Ctrl Pts',(-23.534,11.5183047885456,-2.79752845804063));
#116286=CARTESIAN_POINT('Ctrl Pts',(-23.534,11.3911942477278,-2.74175998216545));
#116287=CARTESIAN_POINT('Ctrl Pts',(-23.534,11.2617238431345,-2.69212530511711));
#116288=CARTESIAN_POINT('Ctrl Pts',(-23.534,11.1303326631264,-2.64879502193041));
#116289=CARTESIAN_POINT('Ctrl Pts',(-23.534,11.0033822809627,-2.60692922843141));
#116290=CARTESIAN_POINT('Ctrl Pts',(-23.534,10.8746380135545,-2.57094816886311));
#116291=CARTESIAN_POINT('Ctrl Pts',(-23.534,10.7445242523891,-2.54079174717233));
#116292=CARTESIAN_POINT('Ctrl Pts',(-23.534,10.6129949118633,-2.5103072371399));
#116293=CARTESIAN_POINT('Ctrl Pts',(-23.534,10.4800654160692,-2.48577456352108));
#116294=CARTESIAN_POINT('Ctrl Pts',(-23.534,10.3461486694481,-2.46717850660524));
#116295=CARTESIAN_POINT('Ctrl Pts',(-23.534,10.2117116901201,-2.44851020870933));
#116296=CARTESIAN_POINT('Ctrl Pts',(-23.534,10.0762789981111,-2.43582454855409));
#116297=CARTESIAN_POINT('Ctrl Pts',(-23.534,9.94025397651706,-2.4291562085726));
#116298=CARTESIAN_POINT('Ctrl Pts',(-23.534,9.92455348268286,-2.42838652495456));
#116299=CARTESIAN_POINT('Ctrl Pts',(-23.534,9.90884508947389,-2.42769706425968));
#116300=CARTESIAN_POINT('Ctrl Pts',(-23.534,9.89312941238514,-2.42708792441797));
#116301=CARTESIAN_POINT('Ctrl Pts',(-23.534,9.86982544152734,-2.42618466221429));
#116302=CARTESIAN_POINT('Ctrl Pts',(-23.534,9.84650207816375,-2.425458012161));
#116303=CARTESIAN_POINT('Ctrl Pts',(-23.534,9.82318746608169,-2.4249087042635));
#116304=CARTESIAN_POINT('Ctrl Pts',(-23.534,9.6848192673001,-2.42164865669821));
#116305=CARTESIAN_POINT('Ctrl Pts',(-23.534,9.54658084862224,-2.42462233472131));
#116306=CARTESIAN_POINT('Ctrl Pts',(-23.534,9.4089130640994,-2.43376529968541));
#116307=CARTESIAN_POINT('Ctrl Pts',(-23.534,9.26969699143324,-2.44301109149675));
#116308=CARTESIAN_POINT('Ctrl Pts',(-23.534,9.13106368650431,-2.45856549918628));
#116309=CARTESIAN_POINT('Ctrl Pts',(-23.534,8.99345056589427,-2.48041133999212));
#116310=CARTESIAN_POINT('Ctrl Pts',(-23.534,8.97031116329775,-2.48408467944715));
#116311=CARTESIAN_POINT('Ctrl Pts',(-23.534,8.94720057915598,-2.48793601825615));
#116312=CARTESIAN_POINT('Ctrl Pts',(-23.534,8.9241208670849,-2.49196541689415));
#116313=CARTESIAN_POINT('Ctrl Pts',(-23.534,8.7873871274078,-2.51583723742324));
#116314=CARTESIAN_POINT('Ctrl Pts',(-23.534,8.65173684163144,-2.54595438851017));
#116315=CARTESIAN_POINT('Ctrl Pts',(-23.534,8.51752579699817,-2.58210352084366));
#116316=CARTESIAN_POINT('Ctrl Pts',(-23.534,8.39200772104797,-2.61591124173702));
#116317=CARTESIAN_POINT('Ctrl Pts',(-23.534,8.2677479659076,-2.65499549928287));
#116318=CARTESIAN_POINT('Ctrl Pts',(-23.534,8.14504361020046,-2.69922256987843));
#116319=CARTESIAN_POINT('Ctrl Pts',(-23.534,8.12749669968016,-2.70554710861093));
#116320=CARTESIAN_POINT('Ctrl Pts',(-23.534,8.1099816141129,-2.71197687841997));
#116321=CARTESIAN_POINT('Ctrl Pts',(-23.534,8.09249924225049,-2.71851155118283));
#116322=CARTESIAN_POINT('Ctrl Pts',(-23.534,8.07453683564987,-2.72522565440019));
#116323=CARTESIAN_POINT('Ctrl Pts',(-23.534,8.05661738952652,-2.73204736696529));
#116324=CARTESIAN_POINT('Ctrl Pts',(-23.534,8.03874521119562,-2.73897465977803));
#116325=CARTESIAN_POINT('Ctrl Pts',(-23.534,7.90644077728776,-2.79025612850193));
#116326=CARTESIAN_POINT('Ctrl Pts',(-23.534,7.7766664785265,-2.84734176999563));
#116327=CARTESIAN_POINT('Ctrl Pts',(-23.534,7.64978171058123,-2.90995636965287));
#116328=CARTESIAN_POINT('Ctrl Pts',(-23.534,7.52165755880184,-2.97318257560338));
#116329=CARTESIAN_POINT('Ctrl Pts',(-23.534,7.3964789135714,-3.04204645157868));
#116330=CARTESIAN_POINT('Ctrl Pts',(-23.534,7.27461872474461,-3.11631789508779));
#116331=CARTESIAN_POINT('Ctrl Pts',(-23.534,7.1526351765545,-3.19066452375846));
#116332=CARTESIAN_POINT('Ctrl Pts',(-23.534,7.03397603466299,-3.27042992503056));
#116333=CARTESIAN_POINT('Ctrl Pts',(-23.534,6.91902974166616,-3.35543308861264));
#116334=CARTESIAN_POINT('Ctrl Pts',(-23.534,6.8844382354436,-3.3810136217932));
#116335=CARTESIAN_POINT('Ctrl Pts',(-23.534,6.85018311680615,-3.40706882775223));
#116336=CARTESIAN_POINT('Ctrl Pts',(-23.534,6.81627539023441,-3.43359460199418));
#116337=CARTESIAN_POINT('Ctrl Pts',(-23.534,6.76396915960913,-3.47451339559359));
#116338=CARTESIAN_POINT('Ctrl Pts',(-23.534,6.71248951985117,-3.51655187486384));
#116339=CARTESIAN_POINT('Ctrl Pts',(-23.534,6.66185982789805,-3.55967699429165));
#116340=CARTESIAN_POINT('Ctrl Pts',(-23.534,6.63093354887773,-3.58601923388978));
#116341=CARTESIAN_POINT('Ctrl Pts',(-23.534,6.60032442699024,-3.61276695671771));
#116342=CARTESIAN_POINT('Ctrl Pts',(-23.534,6.57003806517946,-3.63991298263474));
#116343=CARTESIAN_POINT('Ctrl Pts',(-23.534,6.54970174979597,-3.65814066372453));
#116344=CARTESIAN_POINT('Ctrl Pts',(-23.534,6.52950986024502,-3.67654895514717));
#116345=CARTESIAN_POINT('Ctrl Pts',(-23.534,6.50946759186945,-3.69513255143209));
#116346=CARTESIAN_POINT('Ctrl Pts',(-23.534,6.48629939547582,-3.71661457134924));
#116347=CARTESIAN_POINT('Ctrl Pts',(-23.534,6.46334194284684,-3.73832084889875));
#116348=CARTESIAN_POINT('Ctrl Pts',(-23.534,6.44060381946901,-3.76024083479514));
#116349=CARTESIAN_POINT('Ctrl Pts',(-23.534,6.33630358470948,-3.86078825627445));
#116350=CARTESIAN_POINT('Ctrl Pts',(-23.534,6.23656911791114,-3.96587231758902));
#116351=CARTESIAN_POINT('Ctrl Pts',(-23.534,6.14160415290407,-4.07509691447209));
#116352=CARTESIAN_POINT('Ctrl Pts',(-23.534,6.04554420161977,-4.18558091722884));
#116353=CARTESIAN_POINT('Ctrl Pts',(-23.5339999999999,5.95436378537622,
-4.30030196778979));
#116354=CARTESIAN_POINT('Ctrl Pts',(-23.534,5.86830289306953,-4.41889447743313));
#116355=CARTESIAN_POINT('Ctrl Pts',(-23.534,5.82757976366497,-4.47501123368759));
#116356=CARTESIAN_POINT('Ctrl Pts',(-23.534,5.788003413678,-4.53199543597994));
#116357=CARTESIAN_POINT('Ctrl Pts',(-23.534,5.74960209595384,-4.58981127009334));
#116358=CARTESIAN_POINT('Ctrl Pts',(-23.534,5.73602768423562,-4.61024848377764));
#116359=CARTESIAN_POINT('Ctrl Pts',(-23.534,5.72260309324962,-4.63078521650428));
#116360=CARTESIAN_POINT('Ctrl Pts',(-23.534,5.7093336961382,-4.65141296650499));
#116361=CARTESIAN_POINT('Ctrl Pts',(-23.534,5.62878693151663,-4.7766257783629));
#116362=CARTESIAN_POINT('Ctrl Pts',(-23.534,5.55390603885588,-4.90526364111016));
#116363=CARTESIAN_POINT('Ctrl Pts',(-23.534,5.48492211365497,-5.03693496093975));
#116364=CARTESIAN_POINT('Ctrl Pts',(-23.534,5.43386982584414,-5.13437972211843));
#116365=CARTESIAN_POINT('Ctrl Pts',(-23.534,5.38604780954608,-5.23348685196462));
#116366=CARTESIAN_POINT('Ctrl Pts',(-23.534,5.34156275575684,-5.33411058694693));
#116367=CARTESIAN_POINT('Ctrl Pts',(-23.534,5.29184265751413,-5.4465758210584));
#116368=CARTESIAN_POINT('Ctrl Pts',(-23.534,5.24629059068216,-5.56093558465363));
#116369=CARTESIAN_POINT('Ctrl Pts',(-23.5339999999999,5.20492644341908,
-5.67694766331998));
#116370=CARTESIAN_POINT('Ctrl Pts',(-23.5319824436158,5.20171895019276,
-8.32379158156414));
#116371=CARTESIAN_POINT('Ctrl Pts',(-23.4932005619797,5.41676778847021,
-9.12430550294336));
#116372=CARTESIAN_POINT('Ctrl Pts',(-23.4156367987076,6.2441105606237,-10.6178355852335));
#116373=CARTESIAN_POINT('Ctrl Pts',(-23.2992911537994,8.39090036149447,
-12.0161877049687));
#116374=CARTESIAN_POINT('Ctrl Pts',(-23.1829455088912,10.9421734111865,
-12.2463209198922));
#116375=CARTESIAN_POINT('Ctrl Pts',(-23.066599863983,13.3043923657925,-11.254988095828));
#116376=CARTESIAN_POINT('Ctrl Pts',(-22.9502542190748,14.9272765412854,
-9.27285603598496));
#116377=CARTESIAN_POINT('Ctrl Pts',(-22.8339085741666,15.4330667658206,
-6.76152808894962));
#116378=CARTESIAN_POINT('Ctrl Pts',(-22.7175629292584,14.7039358375933,
-4.30571513125084));
#116379=CARTESIAN_POINT('Ctrl Pts',(-22.6012172843502,12.9096844371217,
-2.47725527851035));
#116380=CARTESIAN_POINT('Ctrl Pts',(-22.484871639442,10.468080449077,-1.70188612182472));
#116381=CARTESIAN_POINT('Ctrl Pts',(-22.3685259945338,7.94764126437696,
-2.16015086439891));
#116382=CARTESIAN_POINT('Ctrl Pts',(-22.2521803496256,5.93523522075824,
-3.74534493575574));
#116383=CARTESIAN_POINT('Ctrl Pts',(-22.1358347047174,4.8994345496665,-6.08836357882409));
#116384=CARTESIAN_POINT('Ctrl Pts',(-22.0194890598092,5.08142987925019,
-8.64365526468454));
#116385=CARTESIAN_POINT('Ctrl Pts',(-21.903143414901,6.43882094024319,-10.8162231015153));
#116386=CARTESIAN_POINT('Ctrl Pts',(-21.7867977699929,8.65559788490324,
-12.1002256459208));
#116387=CARTESIAN_POINT('Ctrl Pts',(-21.6704521250846,11.2154924815527,
-12.196633040956));
#116388=CARTESIAN_POINT('Ctrl Pts',(-21.5541064801764,13.522669729074,-11.0831184026112));
#116389=CARTESIAN_POINT('Ctrl Pts',(-21.4377608352682,15.0394560589382,
-9.0187036198784));
#116390=CARTESIAN_POINT('Ctrl Pts',(-21.32141519036,15.4136427834887,-6.48460441844491));
#116391=CARTESIAN_POINT('Ctrl Pts',(-21.2050695454519,14.5560828744103,
-4.0697625184195));
#116392=CARTESIAN_POINT('Ctrl Pts',(-21.0887239005437,12.6706795512211,
-2.33877606381416));
#116393=CARTESIAN_POINT('Ctrl Pts',(-20.9723782556355,10.1876014233208,
-1.68985101778543));
#116394=CARTESIAN_POINT('Ctrl Pts',(-20.8560326107273,7.70350671639053,
-2.28420971589842));
#116395=CARTESIAN_POINT('Ctrl Pts',(-20.700905084183,5.11052115881551,-4.52263843008836));
#116396=CARTESIAN_POINT('Ctrl Pts',(-20.5069956760027,4.5360766030555,-9.14006182725829));
#116397=CARTESIAN_POINT('Ctrl Pts',(-20.2743043861863,8.77988233534782,
-12.8347906630172));
#116398=CARTESIAN_POINT('Ctrl Pts',(-20.080394978006,13.2742513752808,-11.6301196252367));
#116399=CARTESIAN_POINT('Ctrl Pts',(-19.9252674514617,15.1343798224707,
-8.75365315224294));
#116400=CARTESIAN_POINT('Ctrl Pts',(-19.8089218065535,15.3810849987625,
-6.21138539863939));
#116401=CARTESIAN_POINT('Ctrl Pts',(-19.6925761616453,14.396485337932,-3.84129168477222));
#116402=CARTESIAN_POINT('Ctrl Pts',(-19.5762305167371,12.42241195026,-2.21215263079145));
#116403=CARTESIAN_POINT('Ctrl Pts',(-19.459884871829,9.91250174166068,-1.69521825918731));
#116404=CARTESIAN_POINT('Ctrl Pts',(-19.3435392269207,7.45404862565434,
-2.41471999228771));
#116405=CARTESIAN_POINT('Ctrl Pts',(-19.2271935820125,5.61811305085138,
-4.201278060418));
#116406=CARTESIAN_POINT('Ctrl Pts',(-19.1108479371043,4.8328386716438,-6.63978700045667));
#116407=CARTESIAN_POINT('Ctrl Pts',(-18.9945022921962,5.28075752071532,
-9.1620327133916));
#116408=CARTESIAN_POINT('Ctrl Pts',(-18.878156647288,6.85772466794919,-11.1809277510202));
#116409=CARTESIAN_POINT('Ctrl Pts',(-18.7618110023798,9.1964812960346,-12.2262884221197));
#116410=CARTESIAN_POINT('Ctrl Pts',(-18.6454653574715,11.7524965873672,
-12.0547549551468));
#116411=CARTESIAN_POINT('Ctrl Pts',(-18.5291197125634,13.9306020129096,
-10.7062460945076));
#116412=CARTESIAN_POINT('Ctrl Pts',(-18.4127740676552,15.2236465040783,
-8.49476372466684));
#116413=CARTESIAN_POINT('Ctrl Pts',(-18.296428422747,15.3305499866057,-5.93523409923148));
#116414=CARTESIAN_POINT('Ctrl Pts',(-18.1800827778388,14.2264201441576,
-3.62362758976861));
#116415=CARTESIAN_POINT('Ctrl Pts',(-18.0637371329306,12.1683507297645,
-2.09819197765073));
#116416=CARTESIAN_POINT('Ctrl Pts',(-17.9473914880224,9.63554086184729,
-1.7141042706357));
#116417=CARTESIAN_POINT('Ctrl Pts',(-17.8310458431142,7.2177604705694,-2.56082133574547));
#116418=CARTESIAN_POINT('Ctrl Pts',(-17.714700198206,5.4779309504908,-4.44113880648963));
#116419=CARTESIAN_POINT('Ctrl Pts',(-17.5983545532978,4.82125271145331,
-6.91734413883624));
#116420=CARTESIAN_POINT('Ctrl Pts',(-17.4820089083896,5.40043704181473,
-9.4126399093131));
#116421=CARTESIAN_POINT('Ctrl Pts',(-17.3656593823793,7.08108558213933,
-11.3465358543532));
#116422=CARTESIAN_POINT('Ctrl Pts',(-17.2880917380051,8.67440028619388,
-11.9603779064283));
#116423=CARTESIAN_POINT('Ctrl Pts',(-17.2493059752669,9.49698545957615,
-12.0631389059803));
#116424=CARTESIAN_POINT('Ctrl Pts',(-23.6939479458674,5.47264577451099,
-8.25101021290606));
#116425=CARTESIAN_POINT('Ctrl Pts',(-23.6551660642314,5.6758713401554,-9.00751229764933));
#116426=CARTESIAN_POINT('Ctrl Pts',(-23.5776023009592,6.45772723949198,
-10.4189288773044));
#116427=CARTESIAN_POINT('Ctrl Pts',(-23.461256656051,8.48648766013054,-11.7404003289966));
#116428=CARTESIAN_POINT('Ctrl Pts',(-23.3449110111429,10.8974930521617,
-11.95788094015));
#116429=CARTESIAN_POINT('Ctrl Pts',(-23.2285653662346,13.1298384443577,
-11.0210510761709));
#116430=CARTESIAN_POINT('Ctrl Pts',(-23.1122197213265,14.6634972968383,
-9.14789560009342));
#116431=CARTESIAN_POINT('Ctrl Pts',(-22.9958740764182,15.1414794394154,
-6.77463914987075));
#116432=CARTESIAN_POINT('Ctrl Pts',(-22.8795284315101,14.4524357482022,
-4.45384550391166));
#116433=CARTESIAN_POINT('Ctrl Pts',(-22.7631827866019,12.7568313511272,
-2.72591341737859));
#116434=CARTESIAN_POINT('Ctrl Pts',(-22.6468371416937,10.4494654731035,
-1.99317365131966));
#116435=CARTESIAN_POINT('Ctrl Pts',(-22.5304914967855,8.06759871629672,
-2.42624323807267));
#116436=CARTESIAN_POINT('Ctrl Pts',(-22.4141458518773,6.16583370423474,
-3.92428416862637));
#116437=CARTESIAN_POINT('Ctrl Pts',(-22.2978002069691,5.18698081219592,
-6.13848487236893));
#116438=CARTESIAN_POINT('Ctrl Pts',(-22.1814545620609,5.35897013376373,
-8.55328795805423));
#116439=CARTESIAN_POINT('Ctrl Pts',(-22.0651089171527,6.64173254429605,
-10.6064091517207));
#116440=CARTESIAN_POINT('Ctrl Pts',(-21.9487632722445,8.73663225216978,
-11.8198179079167));
#116441=CARTESIAN_POINT('Ctrl Pts',(-21.8324176273363,11.1557851830167,
-11.9109248748051));
#116442=CARTESIAN_POINT('Ctrl Pts',(-21.7160719824281,13.3361150323902,
-10.8586306887794));
#116443=CARTESIAN_POINT('Ctrl Pts',(-21.5997263375199,14.7695092432934,
-8.90771635087327));
#116444=CARTESIAN_POINT('Ctrl Pts',(-21.4833806926117,15.1231233774711,
-6.51294059790724));
#116445=CARTESIAN_POINT('Ctrl Pts',(-21.3670350477035,14.3127116635907,
-4.23086544230325));
#116446=CARTESIAN_POINT('Ctrl Pts',(-21.2506894027953,12.5309668288262,
-2.59504771746573));
#116447=CARTESIAN_POINT('Ctrl Pts',(-21.1343437578871,10.1844070374604,
-1.98180023100471));
#116448=CARTESIAN_POINT('Ctrl Pts',(-21.0179981129789,7.83688655804795,
-2.54348139881387));
#116449=CARTESIAN_POINT('Ctrl Pts',(-20.8628705864347,5.38646198999665,
-4.6588424732551));
#116450=CARTESIAN_POINT('Ctrl Pts',(-20.6689611782544,4.84360009541132,
-9.0224023474958));
#116451=CARTESIAN_POINT('Ctrl Pts',(-20.436269888438,8.85408360854405,-12.5139969246358));
#116452=CARTESIAN_POINT('Ctrl Pts',(-20.2423604802577,13.101354589737,-11.37555807033));
#116453=CARTESIAN_POINT('Ctrl Pts',(-20.0872329537134,14.8592141479629,
-8.6572382192963));
#116454=CARTESIAN_POINT('Ctrl Pts',(-19.9708873088052,15.0923556027177,
-6.25474301688543));
#116455=CARTESIAN_POINT('Ctrl Pts',(-19.854541663897,14.16188871618,-4.01495581557319));
#116456=CARTESIAN_POINT('Ctrl Pts',(-19.7381960189888,12.2963488506932,
-2.47538597455189));
#116457=CARTESIAN_POINT('Ctrl Pts',(-19.6218503740806,9.92443219238895,
-1.986872384282));
#116458=CARTESIAN_POINT('Ctrl Pts',(-19.5055047291724,7.60114354264496,
-2.66681628847928));
#116459=CARTESIAN_POINT('Ctrl Pts',(-19.3891590842642,5.86614674533775,
-4.35515032860052));
#116460=CARTESIAN_POINT('Ctrl Pts',(-19.272813439356,5.12404634070955,-6.65959132273846));
#116461=CARTESIAN_POINT('Ctrl Pts',(-19.1564677944478,5.54733884577256,
-9.04316528580281));
#116462=CARTESIAN_POINT('Ctrl Pts',(-19.0401221495396,7.03760516418795,
-10.9510625303785));
#116463=CARTESIAN_POINT('Ctrl Pts',(-18.9237765046314,9.24777817630178,
-11.9389498186257));
#116464=CARTESIAN_POINT('Ctrl Pts',(-18.8074308597232,11.6632650840089,
-11.776847171935));
#116465=CARTESIAN_POINT('Ctrl Pts',(-18.6910852148151,13.7216194126565,
-10.5024786230275));
#116466=CARTESIAN_POINT('Ctrl Pts',(-18.5747395699068,14.9435729941127,
-8.4125823970192));
#116467=CARTESIAN_POINT('Ctrl Pts',(-18.4583939249987,15.0445989790936,
-5.99377437145986));
#116468=CARTESIAN_POINT('Ctrl Pts',(-18.3420482800905,14.0011736177956,
-3.80925877864935));
#116469=CARTESIAN_POINT('Ctrl Pts',(-18.2257026351823,12.0562557831971,
-2.36769081850622));
#116470=CARTESIAN_POINT('Ctrl Pts',(-18.1093569902741,9.66269847686509,
-2.00472005270053));
#116471=CARTESIAN_POINT('Ctrl Pts',(-17.9930113453659,7.37784638672052,
-2.80488505650165));
#116472=CARTESIAN_POINT('Ctrl Pts',(-17.8766657004577,5.73367178352352,
-4.58182365632809));
#116473=CARTESIAN_POINT('Ctrl Pts',(-17.7603200555495,5.11309737054954,
-6.92188851484443));
#116474=CARTESIAN_POINT('Ctrl Pts',(-17.6439744106413,5.66043844940817,
-9.27999422918914));
#116475=CARTESIAN_POINT('Ctrl Pts',(-17.527624884631,7.24868581215954,-11.1075655868224));
#116476=CARTESIAN_POINT('Ctrl Pts',(-17.4500572402568,8.75440090727327,
-11.687658923985));
#116477=CARTESIAN_POINT('Ctrl Pts',(-17.4112714775186,9.53176077813031,
-11.7847701775375));
#116478=CARTESIAN_POINT('Ctrl Pts',(-23.8559134481191,5.74357259882922,
-8.17822884424796));
#116479=CARTESIAN_POINT('Ctrl Pts',(-23.817131566483,5.93497489184058,-8.8907190923553));
#116480=CARTESIAN_POINT('Ctrl Pts',(-23.7395678032109,6.67134391836025,
-10.2200221693753));
#116481=CARTESIAN_POINT('Ctrl Pts',(-23.6232221583027,8.58207495876662,
-11.4646129530245));
#116482=CARTESIAN_POINT('Ctrl Pts',(-23.5068765133945,10.852812693137,-11.6694409604076));
#116483=CARTESIAN_POINT('Ctrl Pts',(-23.3905308684863,12.9552845229227,
-10.7871140565138));
#116484=CARTESIAN_POINT('Ctrl Pts',(-23.2741852235781,14.3997180523911,
-9.0229351642019));
#116485=CARTESIAN_POINT('Ctrl Pts',(-23.1578395786699,14.8498921130101,
-6.78775021079188));
#116486=CARTESIAN_POINT('Ctrl Pts',(-23.0414939337617,14.2009356588109,
-4.60197587657248));
#116487=CARTESIAN_POINT('Ctrl Pts',(-22.9251482888536,12.6039782651327,
-2.97457155624683));
#116488=CARTESIAN_POINT('Ctrl Pts',(-22.8088026439453,10.43085049713,-2.28446118081461));
#116489=CARTESIAN_POINT('Ctrl Pts',(-22.6924569990372,8.18755616821649,
-2.69233561174642));
#116490=CARTESIAN_POINT('Ctrl Pts',(-22.576111354129,6.39643218771124,-4.10322340149701));
#116491=CARTESIAN_POINT('Ctrl Pts',(-22.4597657092208,5.47452707472534,
-6.18860616591375));
#116492=CARTESIAN_POINT('Ctrl Pts',(-22.3434200643126,5.63651038827726,
-8.46292065142394));
#116493=CARTESIAN_POINT('Ctrl Pts',(-22.2270744194044,6.84464414834892,
-10.3965952019259));
#116494=CARTESIAN_POINT('Ctrl Pts',(-22.1107287744962,8.81766661943629,
-11.5394101699127));
#116495=CARTESIAN_POINT('Ctrl Pts',(-21.994383129588,11.0960778844808,-11.6252167086543));
#116496=CARTESIAN_POINT('Ctrl Pts',(-21.8780374846798,13.1495603357064,
-10.6341429749476));
#116497=CARTESIAN_POINT('Ctrl Pts',(-21.7616918397716,14.4995624276486,
-8.79672908186814));
#116498=CARTESIAN_POINT('Ctrl Pts',(-21.6453461948634,14.8326039714535,
-6.54127677736955));
#116499=CARTESIAN_POINT('Ctrl Pts',(-21.5290005499552,14.0693404527711,
-4.39196836618699));
#116500=CARTESIAN_POINT('Ctrl Pts',(-21.412654905047,12.3912541064312,-2.85131937111729));
#116501=CARTESIAN_POINT('Ctrl Pts',(-21.2963092601388,10.1812126516,-2.27374944422398));
#116502=CARTESIAN_POINT('Ctrl Pts',(-21.1799636152306,7.97026639970535,
-2.80275308172933));
#116503=CARTESIAN_POINT('Ctrl Pts',(-21.0248360886864,5.66240282117781,
-4.79504651642184));
#116504=CARTESIAN_POINT('Ctrl Pts',(-20.830926680506,5.15112358776711,-8.90474286773331));
#116505=CARTESIAN_POINT('Ctrl Pts',(-20.5982353906897,8.9282848817403,-12.1932031862544));
#116506=CARTESIAN_POINT('Ctrl Pts',(-20.4043259825093,12.9284578041932,
-11.1209965154232));
#116507=CARTESIAN_POINT('Ctrl Pts',(-20.2491984559651,14.5840484734553,
-8.56082328634967));
#116508=CARTESIAN_POINT('Ctrl Pts',(-20.1328528110569,14.8036262066728,
-6.29810063513147));
#116509=CARTESIAN_POINT('Ctrl Pts',(-20.0165071661487,13.927292094428,-4.18861994637416));
#116510=CARTESIAN_POINT('Ctrl Pts',(-19.9001615212405,12.1702857511264,
-2.73861931831233));
#116511=CARTESIAN_POINT('Ctrl Pts',(-19.7838158763323,9.93636264311722,
-2.2785265093767));
#116512=CARTESIAN_POINT('Ctrl Pts',(-19.6674702314241,7.74823845963558,
-2.91891258467084));
#116513=CARTESIAN_POINT('Ctrl Pts',(-19.5511245865159,6.1141804398241,-4.50902259678305));
#116514=CARTESIAN_POINT('Ctrl Pts',(-19.4347789416077,5.41525400977531,
-6.67939564502024));
#116515=CARTESIAN_POINT('Ctrl Pts',(-19.3184332966995,5.81392017082977,
-8.92429785821404));
#116516=CARTESIAN_POINT('Ctrl Pts',(-19.2020876517913,7.21748566042671,
-10.7211973097368));
#116517=CARTESIAN_POINT('Ctrl Pts',(-19.0857420068831,9.29907505656898,
-11.6516112151316));
#116518=CARTESIAN_POINT('Ctrl Pts',(-18.9693963619749,11.5740335806506,
-11.4989393887233));
#116519=CARTESIAN_POINT('Ctrl Pts',(-18.8530507170667,13.5126368124033,
-10.2987111515474));
#116520=CARTESIAN_POINT('Ctrl Pts',(-18.7367050721585,14.663499484147,-8.33040106937155));
#116521=CARTESIAN_POINT('Ctrl Pts',(-18.6203594272503,14.7586479715815,
-6.05231464368824));
#116522=CARTESIAN_POINT('Ctrl Pts',(-18.5040137823422,13.7759270914335,
-3.99488996753009));
#116523=CARTESIAN_POINT('Ctrl Pts',(-18.3876681374339,11.9441608366297,
-2.63718965936172));
#116524=CARTESIAN_POINT('Ctrl Pts',(-18.2713224925258,9.6898560918829,-2.29533583476536));
#116525=CARTESIAN_POINT('Ctrl Pts',(-18.1549768476175,7.53793230287164,
-3.04894877725783));
#116526=CARTESIAN_POINT('Ctrl Pts',(-18.0386312027094,5.98941261655623,
-4.72250850616656));
#116527=CARTESIAN_POINT('Ctrl Pts',(-17.9222855578012,5.40494202964576,
-6.92643289085262));
#116528=CARTESIAN_POINT('Ctrl Pts',(-17.805939912893,5.9204398570016,-9.14734854906519));
#116529=CARTESIAN_POINT('Ctrl Pts',(-17.6895903868827,7.41628604217975,
-10.8685953192918));
#116530=CARTESIAN_POINT('Ctrl Pts',(-17.6120227425084,8.83440152835267,
-11.4149399415416));
#116531=CARTESIAN_POINT('Ctrl Pts',(-17.5732369797703,9.56653609668444,
-11.5064014490947));
#116532=CARTESIAN_POINT('Ctrl Pts',(-24.0178789503708,6.01449942314746,
-8.10544747558987));
#116533=CARTESIAN_POINT('Ctrl Pts',(-23.9790970687347,6.19407844352577,
-8.77392588706126));
#116534=CARTESIAN_POINT('Ctrl Pts',(-23.9015333054626,6.88496059722852,
-10.021115461446));
#116535=CARTESIAN_POINT('Ctrl Pts',(-23.7851876605544,8.6776622574027,-11.1888255770524));
#116536=CARTESIAN_POINT('Ctrl Pts',(-23.6688420156462,10.8081323341124,
-11.3810009806654));
#116537=CARTESIAN_POINT('Ctrl Pts',(-23.552496370738,12.7807306014878,-10.5531770368568));
#116538=CARTESIAN_POINT('Ctrl Pts',(-23.4361507258298,14.135938807944,-8.89797472831037));
#116539=CARTESIAN_POINT('Ctrl Pts',(-23.3198050809216,14.558304786605,-6.800861271713));
#116540=CARTESIAN_POINT('Ctrl Pts',(-23.2034594360134,13.9494355694199,
-4.7501062492333));
#116541=CARTESIAN_POINT('Ctrl Pts',(-23.0871137911052,12.4511251791381,
-3.22322969511507));
#116542=CARTESIAN_POINT('Ctrl Pts',(-22.970768146197,10.4122355211566,-2.57574871030957));
#116543=CARTESIAN_POINT('Ctrl Pts',(-22.8544225012888,8.30751362013623,
-2.95842798542018));
#116544=CARTESIAN_POINT('Ctrl Pts',(-22.7380768563806,6.62703067118774,
-4.28216263436764));
#116545=CARTESIAN_POINT('Ctrl Pts',(-22.6217312114725,5.76207333725475,
-6.23872745945858));
#116546=CARTESIAN_POINT('Ctrl Pts',(-22.5053855665642,5.91405064279082,
-8.37255334479363));
#116547=CARTESIAN_POINT('Ctrl Pts',(-22.3890399216561,7.04755575240179,
-10.1867812521313));
#116548=CARTESIAN_POINT('Ctrl Pts',(-22.2726942767479,8.89870098670282,
-11.2590024319086));
#116549=CARTESIAN_POINT('Ctrl Pts',(-22.1563486318397,11.0363705859449,
-11.3395085425033));
#116550=CARTESIAN_POINT('Ctrl Pts',(-22.0400029869315,12.9630056390227,
-10.4096552611159));
#116551=CARTESIAN_POINT('Ctrl Pts',(-21.9236573420233,14.2296156120038,
-8.68574181286299));
#116552=CARTESIAN_POINT('Ctrl Pts',(-21.8073116971151,14.5420845654359,
-6.56961295683188));
#116553=CARTESIAN_POINT('Ctrl Pts',(-21.6909660522069,13.8259692419515,
-4.55307129007074));
#116554=CARTESIAN_POINT('Ctrl Pts',(-21.5746204072987,12.2515413840362,
-3.10759102476887));
#116555=CARTESIAN_POINT('Ctrl Pts',(-21.4582747623905,10.1780182657396,
-2.56569865744326));
#116556=CARTESIAN_POINT('Ctrl Pts',(-21.3419291174823,8.10364624136277,
-3.06202476464478));
#116557=CARTESIAN_POINT('Ctrl Pts',(-21.186801590938,5.93834365235895,-4.93125055958858));
#116558=CARTESIAN_POINT('Ctrl Pts',(-20.9928921827577,5.45864708012292,
-8.78708338797083));
#116559=CARTESIAN_POINT('Ctrl Pts',(-20.7602008929413,9.00248615493654,
-11.8724094478728));
#116560=CARTESIAN_POINT('Ctrl Pts',(-20.566291484761,12.7555610186494,-10.8664349605165));
#116561=CARTESIAN_POINT('Ctrl Pts',(-20.4111639582168,14.3088827989476,
-8.46440835340305));
#116562=CARTESIAN_POINT('Ctrl Pts',(-20.2948183133085,14.514896810628,-6.34145825337751));
#116563=CARTESIAN_POINT('Ctrl Pts',(-20.1784726684004,13.6926954726759,
-4.36228407717513));
#116564=CARTESIAN_POINT('Ctrl Pts',(-20.0621270234921,12.0442226515596,
-3.00185266207277));
#116565=CARTESIAN_POINT('Ctrl Pts',(-19.945781378584,9.94829309384551,-2.57018063447138));
#116566=CARTESIAN_POINT('Ctrl Pts',(-19.8294357336758,7.89533337662619,
-3.17100888086241));
#116567=CARTESIAN_POINT('Ctrl Pts',(-19.7130900887676,6.36221413431046,
-4.66289486496558));
#116568=CARTESIAN_POINT('Ctrl Pts',(-19.5967444438594,5.70646167884105,
-6.69919996730202));
#116569=CARTESIAN_POINT('Ctrl Pts',(-19.4803987989512,6.08050149588701,
-8.80543043062526));
#116570=CARTESIAN_POINT('Ctrl Pts',(-19.364053154043,7.39736615666546,-10.4913320890951));
#116571=CARTESIAN_POINT('Ctrl Pts',(-19.2477075091348,9.35037193683615,
-11.3642726116376));
#116572=CARTESIAN_POINT('Ctrl Pts',(-19.1313618642266,11.4848020772924,
-11.2210316055115));
#116573=CARTESIAN_POINT('Ctrl Pts',(-19.0150162193184,13.30365421215,-10.0949436800673));
#116574=CARTESIAN_POINT('Ctrl Pts',(-18.8986705744102,14.3834259741814,
-8.2482197417239));
#116575=CARTESIAN_POINT('Ctrl Pts',(-18.782324929502,14.4726969640693,-6.1108549159166));
#116576=CARTESIAN_POINT('Ctrl Pts',(-18.6659792845938,13.5506805650714,
-4.18052115641083));
#116577=CARTESIAN_POINT('Ctrl Pts',(-18.5496336396856,11.8320658900623,
-2.90668850021721));
#116578=CARTESIAN_POINT('Ctrl Pts',(-18.4332879947774,9.7170137069007,-2.58595161683019));
#116579=CARTESIAN_POINT('Ctrl Pts',(-18.3169423498692,7.69801821902275,
-3.293012498014));
#116580=CARTESIAN_POINT('Ctrl Pts',(-18.200596704961,6.24515344958894,-4.86319335600501));
#116581=CARTESIAN_POINT('Ctrl Pts',(-18.0842510600528,5.69678668874198,
-6.93097726686083));
#116582=CARTESIAN_POINT('Ctrl Pts',(-17.9679054151447,6.18044126459504,
-9.01470286894122));
#116583=CARTESIAN_POINT('Ctrl Pts',(-17.8515558891343,7.58388627219995,
-10.6296250517611));
#116584=CARTESIAN_POINT('Ctrl Pts',(-17.7739882447601,8.91440214943207,
-11.1422209590983));
#116585=CARTESIAN_POINT('Ctrl Pts',(-17.735202482022,9.6013114152386,-11.2280327206518));
#116586=CARTESIAN_POINT('Ctrl Pts',(-17.734,9.60084442449481,-11.2300936493755));
#116587=CARTESIAN_POINT('Ctrl Pts',(-17.734,9.47184184893834,-11.2265276083404));
#116588=CARTESIAN_POINT('Ctrl Pts',(-17.734,9.34319367231545,-11.2169788959015));
#116589=CARTESIAN_POINT('Ctrl Pts',(-17.734,9.21527281511486,-11.2016549822556));
#116590=CARTESIAN_POINT('Ctrl Pts',(-17.734,9.08501147085063,-11.1860506966482));
#116591=CARTESIAN_POINT('Ctrl Pts',(-17.734,8.95550358630314,-11.1644579949374));
#116592=CARTESIAN_POINT('Ctrl Pts',(-17.734,8.82713205817655,-11.1370431678773));
#116593=CARTESIAN_POINT('Ctrl Pts',(-17.734,8.77054626721239,-11.1249587929697));
#116594=CARTESIAN_POINT('Ctrl Pts',(-17.734,8.7141811982412,-11.1117424824817));
#116595=CARTESIAN_POINT('Ctrl Pts',(-17.7339999999999,8.65806956321802,
-11.0974052780753));
#116596=CARTESIAN_POINT('Ctrl Pts',(-17.7339999999999,8.63585998151805,
-11.0917304601435));
#116597=CARTESIAN_POINT('Ctrl Pts',(-17.734,8.61369010565667,-11.0858800148832));
#116598=CARTESIAN_POINT('Ctrl Pts',(-17.734,8.59156197215374,-11.0798545436473));
#116599=CARTESIAN_POINT('Ctrl Pts',(-17.734,8.56803675576561,-11.073448647974));
#116600=CARTESIAN_POINT('Ctrl Pts',(-17.734,8.54456657927922,-11.0668470333961));
#116601=CARTESIAN_POINT('Ctrl Pts',(-17.734,8.52115967302967,-11.0600525704303));
#116602=CARTESIAN_POINT('Ctrl Pts',(-17.734,8.39238352917026,-11.0226719473357));
#116603=CARTESIAN_POINT('Ctrl Pts',(-17.7339999999999,8.26546690752475,
-10.9794433217256));
#116604=CARTESIAN_POINT('Ctrl Pts',(-17.7339999999999,8.14080691439625,
-10.9305498903925));
#116605=CARTESIAN_POINT('Ctrl Pts',(-17.7339999999999,8.04196929345981,
-10.8917843625668));
#116606=CARTESIAN_POINT('Ctrl Pts',(-17.734,7.94454991934812,-10.8494567334459));
#116607=CARTESIAN_POINT('Ctrl Pts',(-17.7339999999999,7.84874780521352,
-10.8036350740797));
#116608=CARTESIAN_POINT('Ctrl Pts',(-17.7339999999999,7.8007073644388,-10.780657577885));
#116609=CARTESIAN_POINT('Ctrl Pts',(-17.734,7.75307363883164,-10.7568011656462));
#116610=CARTESIAN_POINT('Ctrl Pts',(-17.734,7.70587215411362,-10.7320725309682));
#116611=CARTESIAN_POINT('Ctrl Pts',(-17.734,7.6793174922842,-10.7181606691847));
#116612=CARTESIAN_POINT('Ctrl Pts',(-17.734,7.65289964014865,-10.7039727286759));
#116613=CARTESIAN_POINT('Ctrl Pts',(-17.734,7.6266232029969,-10.6895097288812));
#116614=CARTESIAN_POINT('Ctrl Pts',(-17.734,7.60953423118557,-10.6801036669266));
#116615=CARTESIAN_POINT('Ctrl Pts',(-17.734,7.59250626485928,-10.6705818595696));
#116616=CARTESIAN_POINT('Ctrl Pts',(-17.734,7.57555065957241,-10.660950526036));
#116617=CARTESIAN_POINT('Ctrl Pts',(-17.734,7.57223521227194,-10.6590672444767));
#116618=CARTESIAN_POINT('Ctrl Pts',(-17.734,7.56892242572952,-10.6571797172604));
#116619=CARTESIAN_POINT('Ctrl Pts',(-17.734,7.56561230852364,-10.655287949029));
#116620=CARTESIAN_POINT('Ctrl Pts',(-17.734,7.44527804479261,-10.5865155995581));
#116621=CARTESIAN_POINT('Ctrl Pts',(-17.734,7.32847088871136,-10.5121436774441));
#116622=CARTESIAN_POINT('Ctrl Pts',(-17.734,7.21544353549546,-10.4326038138175));
#116623=CARTESIAN_POINT('Ctrl Pts',(-17.734,7.10471415648964,-10.3546810857788));
#116624=CARTESIAN_POINT('Ctrl Pts',(-17.734,6.99761187192383,-10.2717977527096));
#116625=CARTESIAN_POINT('Ctrl Pts',(-17.734,6.89438670712412,-10.1843052779668));
#116626=CARTESIAN_POINT('Ctrl Pts',(-17.734,6.78794818419843,-10.0940891974518));
#116627=CARTESIAN_POINT('Ctrl Pts',(-17.734,6.68563112333944,-9.9989722894686));
#116628=CARTESIAN_POINT('Ctrl Pts',(-17.734,6.58773359226506,-9.89928785076242));
#116629=CARTESIAN_POINT('Ctrl Pts',(-17.734,6.48983606119067,-9.79960341205624));
#116630=CARTESIAN_POINT('Ctrl Pts',(-17.734,6.39635732386312,-9.69535089177204));
#116631=CARTESIAN_POINT('Ctrl Pts',(-17.734,6.3076305292093,-9.58681889811916));
#116632=CARTESIAN_POINT('Ctrl Pts',(-17.734,6.29613696047738,-9.57275978628572));
#116633=CARTESIAN_POINT('Ctrl Pts',(-17.734,6.2847217875374,-9.55862705010366));
#116634=CARTESIAN_POINT('Ctrl Pts',(-17.734,6.27339033844863,-9.54442698291117));
#116635=CARTESIAN_POINT('Ctrl Pts',(-17.734,6.18608899588886,-9.43502482960916));
#116636=CARTESIAN_POINT('Ctrl Pts',(-17.734,6.10395851094937,-9.32188720168948));
#116637=CARTESIAN_POINT('Ctrl Pts',(-17.734,6.02725312841167,-9.20538411899327));
#116638=CARTESIAN_POINT('Ctrl Pts',(-17.734,6.00879365458167,-9.17734716076432));
#116639=CARTESIAN_POINT('Ctrl Pts',(-17.734,5.99064847657934,-9.14911508036603));
#116640=CARTESIAN_POINT('Ctrl Pts',(-17.734,5.97282135213961,-9.12069264219457));
#116641=CARTESIAN_POINT('Ctrl Pts',(-17.734,5.8993219360575,-9.00350982809044));
#116642=CARTESIAN_POINT('Ctrl Pts',(-17.734,5.8312260111049,-8.88309435288586));
#116643=CARTESIAN_POINT('Ctrl Pts',(-17.734,5.76858202624986,-8.7598729906184));
#116644=CARTESIAN_POINT('Ctrl Pts',(-17.734,5.7037197407521,-8.63228820817986));
#116645=CARTESIAN_POINT('Ctrl Pts',(-17.734,5.64470175837656,-8.50169476853212));
#116646=CARTESIAN_POINT('Ctrl Pts',(-17.734,5.59162577020733,-8.36852853807731));
#116647=CARTESIAN_POINT('Ctrl Pts',(-17.734,5.5385497820381,-8.23536230762251));
#116648=CARTESIAN_POINT('Ctrl Pts',(-17.734,5.49141540954946,-8.09962248344302));
#116649=CARTESIAN_POINT('Ctrl Pts',(-17.734,5.45037050417322,-7.96171819969766));
#116650=CARTESIAN_POINT('Ctrl Pts',(-17.734,5.44370883975598,-7.93933607817511));
#116651=CARTESIAN_POINT('Ctrl Pts',(-17.734,5.43720810243115,-7.91689789280803));
#116652=CARTESIAN_POINT('Ctrl Pts',(-17.734,5.43087453779524,-7.89442610997133));
#116653=CARTESIAN_POINT('Ctrl Pts',(-17.734,5.39210005996093,-7.75685245349387));
#116654=CARTESIAN_POINT('Ctrl Pts',(-17.734,5.35952760976202,-7.61782263146663));
#116655=CARTESIAN_POINT('Ctrl Pts',(-17.734,5.33320157525561,-7.47778296854049));
#116656=CARTESIAN_POINT('Ctrl Pts',(-17.734,5.30659247764124,-7.33623756944981));
#116657=CARTESIAN_POINT('Ctrl Pts',(-17.734,5.28636445801933,-7.19365980485496));
#116658=CARTESIAN_POINT('Ctrl Pts',(-17.734,5.27260711226718,-7.05048093600343));
#116659=CARTESIAN_POINT('Ctrl Pts',(-17.734,5.26856672905835,-7.00843085541456));
#116660=CARTESIAN_POINT('Ctrl Pts',(-17.734,5.26508476885711,-6.96632877289766));
#116661=CARTESIAN_POINT('Ctrl Pts',(-17.734,5.26216428318299,-6.92418527139126));
#116662=CARTESIAN_POINT('Ctrl Pts',(-17.734,5.25225669184947,-6.78121569821777));
#116663=CARTESIAN_POINT('Ctrl Pts',(-17.734,5.24880693790302,-6.6377701872535));
#116664=CARTESIAN_POINT('Ctrl Pts',(-17.734,5.25169843615224,-6.49425035729587));
#116665=CARTESIAN_POINT('Ctrl Pts',(-17.734,5.25418827323925,-6.37066702279183));
#116666=CARTESIAN_POINT('Ctrl Pts',(-17.734,5.26138083595832,-6.24702806280391));
#116667=CARTESIAN_POINT('Ctrl Pts',(-17.734,5.27323254549849,-6.123587571864));
#116668=CARTESIAN_POINT('Ctrl Pts',(-17.734,5.27508188116906,-6.10432597063131));
#116669=CARTESIAN_POINT('Ctrl Pts',(-17.734,5.27704501035193,-6.08506650230671));
#116670=CARTESIAN_POINT('Ctrl Pts',(-17.734,5.27912085414996,-6.06581909013264));
#116671=CARTESIAN_POINT('Ctrl Pts',(-17.734,5.29479715330724,-5.9204670209976));
#116672=CARTESIAN_POINT('Ctrl Pts',(-17.734,5.31686509682758,-5.77608379440673));
#116673=CARTESIAN_POINT('Ctrl Pts',(-17.734,5.3451374958677,-5.63308999580944));
#116674=CARTESIAN_POINT('Ctrl Pts',(-17.734,5.37370011527558,-5.48862834466948));
#116675=CARTESIAN_POINT('Ctrl Pts',(-17.734,5.40859521043849,-5.3455840407847));
#116676=CARTESIAN_POINT('Ctrl Pts',(-17.734,5.44968220916162,-5.20437948138385));
#116677=CARTESIAN_POINT('Ctrl Pts',(-17.734,5.49084209471425,-5.06292443027113));
#116678=CARTESIAN_POINT('Ctrl Pts',(-17.734,5.53821592683283,-4.92331485930307));
#116679=CARTESIAN_POINT('Ctrl Pts',(-17.734,5.59171431219504,-4.78597586954203));
#116680=CARTESIAN_POINT('Ctrl Pts',(-17.734,5.62179155281002,-4.70876273847473));
#116681=CARTESIAN_POINT('Ctrl Pts',(-17.734,5.65380556167174,-4.63226736332771));
#116682=CARTESIAN_POINT('Ctrl Pts',(-17.734,5.68774754568469,-4.55656680513933));
#116683=CARTESIAN_POINT('Ctrl Pts',(-17.734,5.73801817128877,-4.44444859728045));
#116684=CARTESIAN_POINT('Ctrl Pts',(-17.734,5.7925169840286,-4.3340732964859));
#116685=CARTESIAN_POINT('Ctrl Pts',(-17.734,5.85109760638757,-4.22562345682715));
#116686=CARTESIAN_POINT('Ctrl Pts',(-23.534,5.20509380555676,-8.32288496556915));
#116687=CARTESIAN_POINT('Ctrl Pts',(-23.534,5.25448034822734,-8.46102114255292));
#116688=CARTESIAN_POINT('Ctrl Pts',(-23.534,5.30984160896072,-8.59666377487394));
#116689=CARTESIAN_POINT('Ctrl Pts',(-23.534,5.37090550416415,-8.72949042856159));
#116690=CARTESIAN_POINT('Ctrl Pts',(-23.534,5.43261983427461,-8.86373191325298));
#116691=CARTESIAN_POINT('Ctrl Pts',(-23.534,5.50015936697304,-8.99509777454744));
#116692=CARTESIAN_POINT('Ctrl Pts',(-23.534,5.57328932777698,-9.12322955613377));
#116693=CARTESIAN_POINT('Ctrl Pts',(-23.534,5.64611803491243,-9.25083350796567));
#116694=CARTESIAN_POINT('Ctrl Pts',(-23.534,5.72449172920252,-9.3752305570872));
#116695=CARTESIAN_POINT('Ctrl Pts',(-23.534,5.80821663861272,-9.49603209735779));
#116696=CARTESIAN_POINT('Ctrl Pts',(-23.534,5.89053472310169,-9.61480381617415));
#116697=CARTESIAN_POINT('Ctrl Pts',(-23.534,5.9780262364579,-9.73010029320117));
#116698=CARTESIAN_POINT('Ctrl Pts',(-23.534,6.07053600540052,-9.84151116210382));
#116699=CARTESIAN_POINT('Ctrl Pts',(-23.534,6.09530240287576,-9.87133769711567));
#116700=CARTESIAN_POINT('Ctrl Pts',(-23.534,6.12042860826526,-9.90088549058186));
#116701=CARTESIAN_POINT('Ctrl Pts',(-23.534,6.14591193093455,-9.93014609427624));
#116702=CARTESIAN_POINT('Ctrl Pts',(-23.534,6.15955451065975,-9.94581085369119));
#116703=CARTESIAN_POINT('Ctrl Pts',(-23.534,6.1732994431912,-9.9613932992639));
#116704=CARTESIAN_POINT('Ctrl Pts',(-23.534,6.18714632818517,-9.97689210391278));
#116705=CARTESIAN_POINT('Ctrl Pts',(-23.534,6.19947043338816,-9.99068646265098));
#116706=CARTESIAN_POINT('Ctrl Pts',(-23.534,6.21187374698249,-10.0044127646295));
#116707=CARTESIAN_POINT('Ctrl Pts',(-23.534,6.2243484693293,-10.0180621311511));
#116708=CARTESIAN_POINT('Ctrl Pts',(-23.534,6.32643586438779,-10.1297622743404));
#116709=CARTESIAN_POINT('Ctrl Pts',(-23.534,6.43344023196213,-10.2364692341204));
#116710=CARTESIAN_POINT('Ctrl Pts',(-23.534,6.54511720413425,-10.3377902027729));
#116711=CARTESIAN_POINT('Ctrl Pts',(-23.534,6.65173379038044,-10.4345200440534));
#116712=CARTESIAN_POINT('Ctrl Pts',(-23.534,6.76261007331512,-10.5263410649745));
#116713=CARTESIAN_POINT('Ctrl Pts',(-23.534,6.87736332873695,-10.6130492088598));
#116714=CARTESIAN_POINT('Ctrl Pts',(-23.534,6.99147784436095,-10.6992747177028));
#116715=CARTESIAN_POINT('Ctrl Pts',(-23.534,7.10942705472827,-10.7804443794051));
#116716=CARTESIAN_POINT('Ctrl Pts',(-23.534,7.23085436780316,-10.8563105129995));
#116717=CARTESIAN_POINT('Ctrl Pts',(-23.534,7.33613170341564,-10.9220863603421));
#116718=CARTESIAN_POINT('Ctrl Pts',(-23.534,7.44402406928361,-10.9838750073585));
#116719=CARTESIAN_POINT('Ctrl Pts',(-23.534,7.55430465571588,-11.0414837770386));
#116720=CARTESIAN_POINT('Ctrl Pts',(-23.534,7.58853359014114,-11.059364411006));
#116721=CARTESIAN_POINT('Ctrl Pts',(-23.534,7.62299261107083,-11.0768421517888));
#116722=CARTESIAN_POINT('Ctrl Pts',(-23.534,7.65767495108206,-11.0939106313755));
#116723=CARTESIAN_POINT('Ctrl Pts',(-23.534,7.68146530654451,-11.1056187570799));
#116724=CARTESIAN_POINT('Ctrl Pts',(-23.534,7.70536587584369,-11.1171366355578));
#116725=CARTESIAN_POINT('Ctrl Pts',(-23.534,7.72934494066839,-11.1284484864467));
#116726=CARTESIAN_POINT('Ctrl Pts',(-23.534,7.85661864731227,-11.1884884088606));
#116727=CARTESIAN_POINT('Ctrl Pts',(-23.5339999999999,7.9862331583221,-11.2427954978079));
#116728=CARTESIAN_POINT('Ctrl Pts',(-23.534,8.11783022540238,-11.2911803845139));
#116729=CARTESIAN_POINT('Ctrl Pts',(-23.534,8.24839999272988,-11.3391875592901));
#116730=CARTESIAN_POINT('Ctrl Pts',(-23.534,8.3809222148787,-11.381364838059));
#116731=CARTESIAN_POINT('Ctrl Pts',(-23.534,8.51505911926546,-11.4174776459003));
#116732=CARTESIAN_POINT('Ctrl Pts',(-23.534,8.54046938034511,-11.4243186855065));
#116733=CARTESIAN_POINT('Ctrl Pts',(-23.534,8.56593760260245,-11.430941947981));
#116734=CARTESIAN_POINT('Ctrl Pts',(-23.534,8.59146150656055,-11.4373456266197));
#116735=CARTESIAN_POINT('Ctrl Pts',(-23.534,8.72699587126349,-11.4713497710281));
#116736=CARTESIAN_POINT('Ctrl Pts',(-23.534,8.86410085374639,-11.4991663722465));
#116737=CARTESIAN_POINT('Ctrl Pts',(-23.534,9.00234645392461,-11.5207487445334));
#116738=CARTESIAN_POINT('Ctrl Pts',(-23.534,9.11948261257154,-11.5390355918611));
#116739=CARTESIAN_POINT('Ctrl Pts',(-23.534,9.23743788363359,-11.5528458391875));
#116740=CARTESIAN_POINT('Ctrl Pts',(-23.534,9.35594315836301,-11.5621227489502));
#116741=CARTESIAN_POINT('Ctrl Pts',(-23.534,9.3862114590886,-11.5644922324617));
#116742=CARTESIAN_POINT('Ctrl Pts',(-23.534,9.41651558906433,-11.5665658392786));
#116743=CARTESIAN_POINT('Ctrl Pts',(-23.534,9.44685094557672,-11.5683423557483));
#116744=CARTESIAN_POINT('Ctrl Pts',(-23.534,9.46479541432074,-11.5693932299733));
#116745=CARTESIAN_POINT('Ctrl Pts',(-23.534,9.48274095025219,-11.5703395658612));
#116746=CARTESIAN_POINT('Ctrl Pts',(-23.534,9.50068594451741,-11.5711814160656));
#116747=CARTESIAN_POINT('Ctrl Pts',(-23.534,9.6376789645452,-11.5776081443338));
#116748=CARTESIAN_POINT('Ctrl Pts',(-23.534,9.77465402965029,-11.5779506548684));
#116749=CARTESIAN_POINT('Ctrl Pts',(-23.534,9.91120575942691,-11.572220826072));
#116750=CARTESIAN_POINT('Ctrl Pts',(-23.534,10.0465379651975,-11.5665421695586));
#116751=CARTESIAN_POINT('Ctrl Pts',(-23.534,10.1814551280808,-11.5548989762821));
#116752=CARTESIAN_POINT('Ctrl Pts',(-23.534,10.315554055898,-11.5372529906654));
#116753=CARTESIAN_POINT('Ctrl Pts',(-23.534,10.4488851811598,-11.5197080396584));
#116754=CARTESIAN_POINT('Ctrl Pts',(-23.534,10.5814081302488,-11.4962287057312));
#116755=CARTESIAN_POINT('Ctrl Pts',(-23.534,10.7127070778146,-11.466730168397));
#116756=CARTESIAN_POINT('Ctrl Pts',(-23.5339999999999,10.7477535156779,
-11.4588563912274));
#116757=CARTESIAN_POINT('Ctrl Pts',(-23.534,10.7827126062386,-11.4505535095437));
#116758=CARTESIAN_POINT('Ctrl Pts',(-23.534,10.8175761048042,-11.4418193551064));
#116759=CARTESIAN_POINT('Ctrl Pts',(-23.534,10.9043442667858,-11.4200818199142));
#116760=CARTESIAN_POINT('Ctrl Pts',(-23.534,10.9905208003715,-11.3956733994087));
#116761=CARTESIAN_POINT('Ctrl Pts',(-23.534,11.0759855672366,-11.3686310737129));
#116762=CARTESIAN_POINT('Ctrl Pts',(-23.534,11.1080452454195,-11.3584869138336));
#116763=CARTESIAN_POINT('Ctrl Pts',(-23.534,11.1400046970052,-11.3479720510328));
#116764=CARTESIAN_POINT('Ctrl Pts',(-23.534,11.1718573159444,-11.3370881949364));
#116765=CARTESIAN_POINT('Ctrl Pts',(-23.534,11.1899003611931,-11.3309229904864));
#116766=CARTESIAN_POINT('Ctrl Pts',(-23.534,11.2079056979589,-11.3246405183814));
#116767=CARTESIAN_POINT('Ctrl Pts',(-23.534,11.2258644852499,-11.3182440453307));
#116768=CARTESIAN_POINT('Ctrl Pts',(-23.534,11.3524381725535,-11.2731616482488));
#116769=CARTESIAN_POINT('Ctrl Pts',(-23.534,11.4768170268761,-11.2223807678744));
#116770=CARTESIAN_POINT('Ctrl Pts',(-23.534,11.5986229667083,-11.1660898819115));
#116771=CARTESIAN_POINT('Ctrl Pts',(-23.534,11.7193673208413,-11.1102895927094));
#116772=CARTESIAN_POINT('Ctrl Pts',(-23.534,11.8375840316722,-11.0490744065899));
#116773=CARTESIAN_POINT('Ctrl Pts',(-23.534,11.9528722694146,-10.9825889536698));
#116774=CARTESIAN_POINT('Ctrl Pts',(-23.534,12.007918281115,-10.9508445269094));
#116775=CARTESIAN_POINT('Ctrl Pts',(-23.534,12.0622961454218,-10.9178981000613));
#116776=CARTESIAN_POINT('Ctrl Pts',(-23.534,12.115958959572,-10.8837627538526));
#116777=CARTESIAN_POINT('Ctrl Pts',(-23.534,12.1331643569177,-10.8728182626933));
#116778=CARTESIAN_POINT('Ctrl Pts',(-23.534,12.150294211089,-10.8617527782972));
#116779=CARTESIAN_POINT('Ctrl Pts',(-23.534,12.1673397958196,-10.8505716388401));
#116780=CARTESIAN_POINT('Ctrl Pts',(-23.534,12.2766355142431,-10.7788785471058));
#116781=CARTESIAN_POINT('Ctrl Pts',(-23.534,12.3825568873877,-10.7023781389818));
#116782=CARTESIAN_POINT('Ctrl Pts',(-23.534,12.4847306195173,-10.6212230158632));
#116783=CARTESIAN_POINT('Ctrl Pts',(-23.534,12.5574317395048,-10.5634775638721));
#116784=CARTESIAN_POINT('Ctrl Pts',(-23.534,12.6282347834107,-10.503374641833));
#116785=CARTESIAN_POINT('Ctrl Pts',(-23.534,12.6969925515033,-10.4409593113222));
#116786=CARTESIAN_POINT('Ctrl Pts',(-23.534,12.7737176242397,-10.3713116059626));
#116787=CARTESIAN_POINT('Ctrl Pts',(-23.534,12.8478962945781,-10.2987843938166));
#116788=CARTESIAN_POINT('Ctrl Pts',(-23.534,12.9193848394627,-10.2235362295063));
#116789=CARTESIAN_POINT('Ctrl Pts',(23.5308797445685,7.34306041656048,-3.78088480443338));
#116790=CARTESIAN_POINT('Ctrl Pts',(23.492093981254,7.86605497010199,-3.32818419228394));
#116791=CARTESIAN_POINT('Ctrl Pts',(23.4145263363035,9.13628619196831,-2.68291557707719));
#116792=CARTESIAN_POINT('Ctrl Pts',(23.2981768097169,11.273827201379,-2.72051676872855));
#116793=CARTESIAN_POINT('Ctrl Pts',(23.1818311648087,13.1445058509814,-3.7545693255618));
#116794=CARTESIAN_POINT('Ctrl Pts',(23.0654855199005,14.3133278040104,-5.54430636416698));
#116795=CARTESIAN_POINT('Ctrl Pts',(22.9491398749923,14.5078915515634,-7.6729906495586));
#116796=CARTESIAN_POINT('Ctrl Pts',(22.8327942300841,13.683012039168,-9.64497426174501));
#116797=CARTESIAN_POINT('Ctrl Pts',(22.7164485851759,12.0307010434993,-11.0010914771052));
#116798=CARTESIAN_POINT('Ctrl Pts',(22.6001029402677,9.93571567134801,-11.4255794825061));
#116799=CARTESIAN_POINT('Ctrl Pts',(22.4837572953595,7.88584799806227,-10.819598573941));
#116800=CARTESIAN_POINT('Ctrl Pts',(22.3674116504513,6.35840201881396,-9.32424771654229));
#116801=CARTESIAN_POINT('Ctrl Pts',(22.2510660055431,5.70903363319746,-7.28771027158123));
#116802=CARTESIAN_POINT('Ctrl Pts',(22.1347203606349,6.08894046342753,-5.18418094981214));
#116803=CARTESIAN_POINT('Ctrl Pts',(22.0183747157267,7.409673761906,-3.50345455895014));
#116804=CARTESIAN_POINT('Ctrl Pts',(21.9020290708185,9.36368649127951,-2.63687572721834));
#116805=CARTESIAN_POINT('Ctrl Pts',(21.7856834259103,11.496046351416,-2.78622644534918));
#116806=CARTESIAN_POINT('Ctrl Pts',(21.6693377810021,13.3101469114119,-3.91672197416435));
#116807=CARTESIAN_POINT('Ctrl Pts',(21.5529921360939,14.3837946056831,-5.76515297562463));
#116808=CARTESIAN_POINT('Ctrl Pts',(21.4366464911858,14.4665608124293,-7.90108278347799));
#116809=CARTESIAN_POINT('Ctrl Pts',(21.3203008462775,13.5400870289091,-9.82725897609517));
#116810=CARTESIAN_POINT('Ctrl Pts',(21.2039552013694,11.8181864808081,-11.0950041454724));
#116811=CARTESIAN_POINT('Ctrl Pts',(21.0876095564611,9.70579060275323,-11.4095065743484));
#116812=CARTESIAN_POINT('Ctrl Pts',(20.971263911553,7.68639780494903,-10.6967511237975));
#116813=CARTESIAN_POINT('Ctrl Pts',(20.8549182666448,6.24770301872872,-9.12434926157139));
#116814=CARTESIAN_POINT('Ctrl Pts',(20.6997907401005,5.50261576576667,-6.36488878700103));
#116815=CARTESIAN_POINT('Ctrl Pts',(20.5058813319202,7.26494661953086,-2.90538188427047));
#116816=CARTESIAN_POINT('Ctrl Pts',(20.2731900421038,11.9254495265014,-2.33672551939335));
#116817=CARTESIAN_POINT('Ctrl Pts',(20.0792806339235,14.4679218283246,-5.27097715185977));
#116818=CARTESIAN_POINT('Ctrl Pts',(19.9241531073792,14.4082134957746,-8.1286356409495));
#116819=CARTESIAN_POINT('Ctrl Pts',(19.807807462471,13.3898163849714,-10.0008422612073));
#116820=CARTESIAN_POINT('Ctrl Pts',(19.6914618175628,11.6010543926055,-11.1782538879465));
#116821=CARTESIAN_POINT('Ctrl Pts',(19.5751161726546,9.47501136884743,-11.3809092222496));
#116822=CARTESIAN_POINT('Ctrl Pts',(19.4587705277464,7.49879745073454,-10.5643935384525));
#116823=CARTESIAN_POINT('Ctrl Pts',(19.3424248828382,6.13635193741054,-8.91750233992758));
#116824=CARTESIAN_POINT('Ctrl Pts',(19.22607923793,5.70310051443743,-6.8243373694708));
#116825=CARTESIAN_POINT('Ctrl Pts',(19.1097335930218,6.30078881484329,-4.77197647671063));
#116826=CARTESIAN_POINT('Ctrl Pts',(18.9933879481137,7.78983506549335,-3.23844387325101));
#116827=CARTESIAN_POINT('Ctrl Pts',(18.8770423032055,9.82372176647143,-2.58074401943319));
#116828=CARTESIAN_POINT('Ctrl Pts',(18.7606966582973,11.9287765236596,-2.95205128760764));
#116829=CARTESIAN_POINT('Ctrl Pts',(18.6443510133891,13.6148953672596,-4.26589332221704));
#116830=CARTESIAN_POINT('Ctrl Pts',(18.5280053684809,14.4894546634699,-6.21635758608087));
#116831=CARTESIAN_POINT('Ctrl Pts',(18.4116597235727,14.3488283537461,-8.34928709874185));
#116832=CARTESIAN_POINT('Ctrl Pts',(18.2953140786645,13.2257568308521,-10.1680437511583));
#116833=CARTESIAN_POINT('Ctrl Pts',(18.1789684337563,11.3817398772988,-11.2491412557967));
#116834=CARTESIAN_POINT('Ctrl Pts',(18.0626227888481,9.24615026099209,-11.3408514895768));
#116835=CARTESIAN_POINT('Ctrl Pts',(17.9462771439399,7.31623493710189,-10.4218235406992));
#116836=CARTESIAN_POINT('Ctrl Pts',(17.8299314990317,6.04138851298324,-8.70604028760065));
#116837=CARTESIAN_POINT('Ctrl Pts',(17.7135858541235,5.71839679930902,-6.59302628110828));
#116838=CARTESIAN_POINT('Ctrl Pts',(17.5972402092153,6.42258013691471,-4.57475245125364));
#116839=CARTESIAN_POINT('Ctrl Pts',(17.4808945643071,7.98973446887496,-3.1212289391666));
#116840=CARTESIAN_POINT('Ctrl Pts',(17.3645489193989,10.0554518264208,-2.57077253162166));
#116841=CARTESIAN_POINT('Ctrl Pts',(17.2869851561268,11.4435020078058,-2.89162900717149));
#116842=CARTESIAN_POINT('Ctrl Pts',(17.2482032744907,12.0599591502202,-3.20523048596805));
#116843=CARTESIAN_POINT('Ctrl Pts',(23.6934845769398,7.15873664017536,-3.56793941240261));
#116844=CARTESIAN_POINT('Ctrl Pts',(23.6546988136254,7.71632743320132,-3.08529252512158));
#116845=CARTESIAN_POINT('Ctrl Pts',(23.5771311686748,9.07058481414467,-2.39733920623614));
#116846=CARTESIAN_POINT('Ctrl Pts',(23.4607816420882,11.3495247734463,-2.43742772748293));
#116847=CARTESIAN_POINT('Ctrl Pts',(23.34443599718,13.343949351418,-3.53988315706783));
#116848=CARTESIAN_POINT('Ctrl Pts',(23.2280903522717,14.5900892113502,-5.44801181329597));
#116849=CARTESIAN_POINT('Ctrl Pts',(23.1117447073636,14.7975234065203,-7.71750917374831));
#116850=CARTESIAN_POINT('Ctrl Pts',(22.9953990624555,13.9180778781628,-9.81994006658924));
#116851=CARTESIAN_POINT('Ctrl Pts',(22.8790534175472,12.1564660369653,-11.2657648240908));
#116852=CARTESIAN_POINT('Ctrl Pts',(22.7627077726391,9.9228967825145,-11.718332832608));
#116853=CARTESIAN_POINT('Ctrl Pts',(22.6463621277308,7.73742977562921,-11.072266113409));
#116854=CARTESIAN_POINT('Ctrl Pts',(22.5300164828226,6.10894280744555,-9.47799736857629));
#116855=CARTESIAN_POINT('Ctrl Pts',(22.4136708379145,5.41661851716373,-7.30674238843666));
#116856=CARTESIAN_POINT('Ctrl Pts',(22.2973251930063,5.82165629300578,-5.064063999654));
#116857=CARTESIAN_POINT('Ctrl Pts',(22.180979548098,7.22975647739126,-3.27215707673417));
#116858=CARTESIAN_POINT('Ctrl Pts',(22.0646339031898,9.31302770837495,-2.34825380712489));
#116859=CARTESIAN_POINT('Ctrl Pts',(21.9482882582816,11.586443783894,-2.50748411802901));
#116860=CARTESIAN_POINT('Ctrl Pts',(21.8319426133734,13.5205476154298,-3.71276224981039));
#116861=CARTESIAN_POINT('Ctrl Pts',(21.7155969684652,14.6652174121329,-5.68346749134442));
#116862=CARTESIAN_POINT('Ctrl Pts',(21.599251323557,14.7534586271567,-7.96068966764422));
#116863=CARTESIAN_POINT('Ctrl Pts',(21.4829056786489,13.7656983375463,-10.0142829669937));
#116864=CARTESIAN_POINT('Ctrl Pts',(21.3665600337407,11.9298935750953,-11.3658898423639));
#116865=CARTESIAN_POINT('Ctrl Pts',(21.2502143888324,9.67776210478953,-11.7011966969728));
#116866=CARTESIAN_POINT('Ctrl Pts',(21.1338687439242,7.52478589512584,-10.9412922692592));
#116867=CARTESIAN_POINT('Ctrl Pts',(21.0175230990161,5.99092103680429,-9.26487557356499));
#116868=CARTESIAN_POINT('Ctrl Pts',(20.8623955724718,5.1965460486914,-6.3228759983871));
#116869=CARTESIAN_POINT('Ctrl Pts',(20.6684861642916,7.07545559310313,-2.63452172335695));
#116870=CARTESIAN_POINT('Ctrl Pts',(20.4357948744751,12.0442521019777,-2.02824857709958));
#116871=CARTESIAN_POINT('Ctrl Pts',(20.2418854662947,14.7549096746432,-5.15660179532254));
#116872=CARTESIAN_POINT('Ctrl Pts',(20.0867579397505,14.6912516187967,-8.20329521180079));
#116873=CARTESIAN_POINT('Ctrl Pts',(19.9704122948423,13.6054872474799,-10.1993488361244));
#116874=CARTESIAN_POINT('Ctrl Pts',(19.8540666499341,11.698398137079,-11.4546465791426));
#116875=CARTESIAN_POINT('Ctrl Pts',(19.7377210050259,9.43171675847363,-11.6707076218434));
#116876=CARTESIAN_POINT('Ctrl Pts',(19.6213753601177,7.32477572375777,-10.800179191741));
#116877=CARTESIAN_POINT('Ctrl Pts',(19.5050297152095,5.87220404956978,-9.0443456688206));
#116878=CARTESIAN_POINT('Ctrl Pts',(19.3886840703013,5.41029292089868,-6.81271723615754));
#116879=CARTESIAN_POINT('Ctrl Pts',(19.2723384253932,6.04751847353379,-4.62459208261562));
#116880=CARTESIAN_POINT('Ctrl Pts',(19.155992780485,7.63506556007606,-2.98961585828608));
#116881=CARTESIAN_POINT('Ctrl Pts',(19.0396471355767,9.80349444875913,-2.28840897079557));
#116882=CARTESIAN_POINT('Ctrl Pts',(18.9233014906685,12.0477991809505,-2.68427832108942));
#116883=CARTESIAN_POINT('Ctrl Pts',(18.8069558457603,13.8454552689013,-4.08503138252743));
#116884=CARTESIAN_POINT('Ctrl Pts',(18.6906102008522,14.7778669129997,-6.16451941599185));
#116885=CARTESIAN_POINT('Ctrl Pts',(18.5742645559441,14.6279381326173,-8.4385428267131));
#116886=CARTESIAN_POINT('Ctrl Pts',(18.4579189110359,13.4305751068745,-10.3776107525164));
#116887=CARTESIAN_POINT('Ctrl Pts',(18.3415732661277,11.4645759037805,-11.5302231666757));
#116888=CARTESIAN_POINT('Ctrl Pts',(18.2252276212194,9.18771642279568,-11.6280000586831));
#116889=CARTESIAN_POINT('Ctrl Pts',(18.1088819763111,7.13013664756869,-10.6481781478091));
#116890=CARTESIAN_POINT('Ctrl Pts',(17.992536331403,5.77095876742236,-8.81889534117678));
#116891=CARTESIAN_POINT('Ctrl Pts',(17.8761906864949,5.42660105939486,-6.5661048530603));
#116892=CARTESIAN_POINT('Ctrl Pts',(17.7598450415866,6.17736632643707,-4.41432163139647));
#116893=CARTESIAN_POINT('Ctrl Pts',(17.6434993966784,7.84818836623569,-2.86464712274567));
#116894=CARTESIAN_POINT('Ctrl Pts',(17.5271537517702,10.0505535185336,-2.27777786620982));
#116895=CARTESIAN_POINT('Ctrl Pts',(17.4495899884982,11.5304236169073,-2.61985908949955));
#116896=CARTESIAN_POINT('Ctrl Pts',(17.410808106862,12.1876595758245,-2.95420539592318));
#116897=CARTESIAN_POINT('Ctrl Pts',(23.8560894093112,6.97441286379024,-3.35499402037186));
#116898=CARTESIAN_POINT('Ctrl Pts',(23.8173036459966,7.56659989630065,-2.84240085795923));
#116899=CARTESIAN_POINT('Ctrl Pts',(23.7397360010461,9.00488343632105,-2.11176283539509));
#116900=CARTESIAN_POINT('Ctrl Pts',(23.6233864744595,11.4252223455135,-2.15433868623731));
#116901=CARTESIAN_POINT('Ctrl Pts',(23.5070408295513,13.5433928518545,-3.32519698857386));
#116902=CARTESIAN_POINT('Ctrl Pts',(23.3906951846431,14.8668506186901,-5.35171726242495));
#116903=CARTESIAN_POINT('Ctrl Pts',(23.2743495397349,15.0871552614771,-7.76202769793803));
#116904=CARTESIAN_POINT('Ctrl Pts',(23.1580038948267,14.1531437171576,-9.99490587143344));
#116905=CARTESIAN_POINT('Ctrl Pts',(23.0416582499186,12.2822310304315,-11.5304381710766));
#116906=CARTESIAN_POINT('Ctrl Pts',(22.9253126050104,9.91007789368101,-12.0110861827097));
#116907=CARTESIAN_POINT('Ctrl Pts',(22.8089669601021,7.58901155319615,-11.3249336528771));
#116908=CARTESIAN_POINT('Ctrl Pts',(22.692621315194,5.85948359607716,-9.63174702061027));
#116909=CARTESIAN_POINT('Ctrl Pts',(22.5762756702858,5.12420340112999,-7.32577450529211));
#116910=CARTESIAN_POINT('Ctrl Pts',(22.4599300253776,5.55437212258404,-4.94394704949586));
#116911=CARTESIAN_POINT('Ctrl Pts',(22.3435843804694,7.04983919287652,-3.0408595945182));
#116912=CARTESIAN_POINT('Ctrl Pts',(22.2272387355612,9.2623689254704,-2.05963188703145));
#116913=CARTESIAN_POINT('Ctrl Pts',(22.110893090653,11.6768412163722,-2.22874179070883));
#116914=CARTESIAN_POINT('Ctrl Pts',(21.9945474457448,13.7309483194478,-3.50880252545644));
#116915=CARTESIAN_POINT('Ctrl Pts',(21.8782018008366,14.9466402185827,-5.60178200706422));
#116916=CARTESIAN_POINT('Ctrl Pts',(21.7618561559284,15.0403564418842,-8.02029655181046));
#116917=CARTESIAN_POINT('Ctrl Pts',(21.6455105110202,13.9913096461837,-10.2013069578923));
#116918=CARTESIAN_POINT('Ctrl Pts',(21.529164866112,12.0416006693825,-11.6367755392554));
#116919=CARTESIAN_POINT('Ctrl Pts',(21.4128192212038,9.64973360682584,-11.9928868195971));
#116920=CARTESIAN_POINT('Ctrl Pts',(21.2964735762957,7.36317398530266,-11.185833414721));
#116921=CARTESIAN_POINT('Ctrl Pts',(21.1801279313874,5.73413905487985,-9.4054018855586));
#116922=CARTESIAN_POINT('Ctrl Pts',(21.0250004048432,4.89047633161614,-6.28086320977319));
#116923=CARTESIAN_POINT('Ctrl Pts',(20.8310909966629,6.88596456667538,-2.36366156244345));
#116924=CARTESIAN_POINT('Ctrl Pts',(20.5983997068464,12.1630546774541,-1.71977163480581));
#116925=CARTESIAN_POINT('Ctrl Pts',(20.4044902986661,15.0418975209619,-5.04222643878529));
#116926=CARTESIAN_POINT('Ctrl Pts',(20.2493627721219,14.9742897418189,-8.2779547826521));
#116927=CARTESIAN_POINT('Ctrl Pts',(20.1330171272137,13.8211581099884,-10.3978554110414));
#116928=CARTESIAN_POINT('Ctrl Pts',(20.0166714823055,11.7957418815525,-11.7310392703387));
#116929=CARTESIAN_POINT('Ctrl Pts',(19.9003258373973,9.38842214809981,-11.9605060214371));
#116930=CARTESIAN_POINT('Ctrl Pts',(19.7839801924891,7.15075399678101,-11.0359648450295));
#116931=CARTESIAN_POINT('Ctrl Pts',(19.6676345475809,5.60805616172902,-9.17118899771363));
#116932=CARTESIAN_POINT('Ctrl Pts',(19.5512889026727,5.11748532735993,-6.8010971028443));
#116933=CARTESIAN_POINT('Ctrl Pts',(19.4349432577645,5.79424813222429,-4.47720768852061));
#116934=CARTESIAN_POINT('Ctrl Pts',(19.3185976128563,7.48029605465876,-2.74078784332114));
#116935=CARTESIAN_POINT('Ctrl Pts',(19.2022519679481,9.78326713104683,-1.99607392215794));
#116936=CARTESIAN_POINT('Ctrl Pts',(19.0859063230399,12.1668218382416,-2.41650535457117));
#116937=CARTESIAN_POINT('Ctrl Pts',(18.9695606781317,14.0760151705431,-3.90416944283784));
#116938=CARTESIAN_POINT('Ctrl Pts',(18.8532150332235,15.0662791625295,-6.11268124590282));
#116939=CARTESIAN_POINT('Ctrl Pts',(18.7368693883153,14.9070479114883,-8.52779855468437));
#116940=CARTESIAN_POINT('Ctrl Pts',(18.6205237434071,13.6353933828971,-10.5871777538744));
#116941=CARTESIAN_POINT('Ctrl Pts',(18.504178098499,11.5474119302623,-11.8113050775549));
#116942=CARTESIAN_POINT('Ctrl Pts',(18.3878324535907,9.12928258459928,-11.9151486277894));
#116943=CARTESIAN_POINT('Ctrl Pts',(18.2714868086826,6.94403835803548,-10.8745327549191));
#116944=CARTESIAN_POINT('Ctrl Pts',(18.1551411637744,5.50052902186147,-8.93175039475289));
#116945=CARTESIAN_POINT('Ctrl Pts',(18.0387955188662,5.13480531948069,-6.53918342501231));
#116946=CARTESIAN_POINT('Ctrl Pts',(17.922449873958,5.93215251595945,-4.2538908115393));
#116947=CARTESIAN_POINT('Ctrl Pts',(17.8061042290498,7.70664226359641,-2.60806530632473));
#116948=CARTESIAN_POINT('Ctrl Pts',(17.6897585841416,10.0456552106465,-1.98478320079797));
#116949=CARTESIAN_POINT('Ctrl Pts',(17.6121948208694,11.6173452260086,-2.34808917182759));
#116950=CARTESIAN_POINT('Ctrl Pts',(17.5734129392334,12.3153600014288,-2.70318030587831));
#116951=CARTESIAN_POINT('Ctrl Pts',(24.0186942416826,6.79008908740512,-3.14204862834109));
#116952=CARTESIAN_POINT('Ctrl Pts',(23.979908478368,7.41687235939997,-2.59950919079688));
#116953=CARTESIAN_POINT('Ctrl Pts',(23.9023408334175,8.93918205849745,-1.82618646455404));
#116954=CARTESIAN_POINT('Ctrl Pts',(23.7859913068309,11.5009199175807,-1.87124964499168));
#116955=CARTESIAN_POINT('Ctrl Pts',(23.6696456619227,13.7428363522911,-3.11051082007989));
#116956=CARTESIAN_POINT('Ctrl Pts',(23.5533000170145,15.14361202603,-5.25542271155395));
#116957=CARTESIAN_POINT('Ctrl Pts',(23.4369543721063,15.3767871164341,-7.80654622212773));
#116958=CARTESIAN_POINT('Ctrl Pts',(23.3206087271981,14.3882095561523,-10.1698716762777));
#116959=CARTESIAN_POINT('Ctrl Pts',(23.2042630822899,12.4079960238977,-11.7951115180623));
#116960=CARTESIAN_POINT('Ctrl Pts',(23.0879174373818,9.89725900484749,-12.3038395328114));
#116961=CARTESIAN_POINT('Ctrl Pts',(22.9715717924735,7.4405933307631,-11.5776011923451));
#116962=CARTESIAN_POINT('Ctrl Pts',(22.8552261475653,5.61002438470876,-9.78549667264426));
#116963=CARTESIAN_POINT('Ctrl Pts',(22.7388805026571,4.83178828509627,-7.34480662214755));
#116964=CARTESIAN_POINT('Ctrl Pts',(22.622534857749,5.28708795216229,-4.82383009933772));
#116965=CARTESIAN_POINT('Ctrl Pts',(22.5061892128408,6.86992190836178,-2.80956211230224));
#116966=CARTESIAN_POINT('Ctrl Pts',(22.3898435679325,9.21171014256585,-1.771009966938));
#116967=CARTESIAN_POINT('Ctrl Pts',(22.2734979230244,11.7672386488503,-1.94999946338866));
#116968=CARTESIAN_POINT('Ctrl Pts',(22.1571522781162,13.9413490234657,-3.30484280110248));
#116969=CARTESIAN_POINT('Ctrl Pts',(22.040806633208,15.2280630250325,-5.52009652278402));
#116970=CARTESIAN_POINT('Ctrl Pts',(21.9244609882998,15.3272542566116,-8.07990343597667));
#116971=CARTESIAN_POINT('Ctrl Pts',(21.8081153433916,14.216920954821,-10.3883309487909));
#116972=CARTESIAN_POINT('Ctrl Pts',(21.6917696984834,12.1533077636698,-11.907661236147));
#116973=CARTESIAN_POINT('Ctrl Pts',(21.5754240535752,9.62170510886214,-12.2845769422216));
#116974=CARTESIAN_POINT('Ctrl Pts',(21.459078408667,7.20156207547948,-11.4303745601828));
#116975=CARTESIAN_POINT('Ctrl Pts',(21.3427327637588,5.47735707295543,-9.54592819755221));
#116976=CARTESIAN_POINT('Ctrl Pts',(21.1876052372145,4.58440661454088,-6.23885042115928));
#116977=CARTESIAN_POINT('Ctrl Pts',(20.9936958290342,6.69647354024763,-2.09280140152994));
#116978=CARTESIAN_POINT('Ctrl Pts',(20.7610045392178,12.2818572529304,-1.41129469251204));
#116979=CARTESIAN_POINT('Ctrl Pts',(20.5670951310375,15.3288853672806,-4.92785108224806));
#116980=CARTESIAN_POINT('Ctrl Pts',(20.4119676044933,15.257327864841,-8.35261435350337));
#116981=CARTESIAN_POINT('Ctrl Pts',(20.295621959585,14.0368289724969,-10.5963619859584));
#116982=CARTESIAN_POINT('Ctrl Pts',(20.1792763146769,11.893085626026,-12.0074319615348));
#116983=CARTESIAN_POINT('Ctrl Pts',(20.0629306697686,9.345127537726,-12.2503044210308));
#116984=CARTESIAN_POINT('Ctrl Pts',(19.9465850248605,6.97673226980424,-11.2717504983181));
#116985=CARTESIAN_POINT('Ctrl Pts',(19.8302393799522,5.34390827388827,-9.29803232660665));
#116986=CARTESIAN_POINT('Ctrl Pts',(19.7138937350441,4.82467773382117,-6.78947696953105));
#116987=CARTESIAN_POINT('Ctrl Pts',(19.5975480901359,5.54097779091479,-4.3298232944256));
#116988=CARTESIAN_POINT('Ctrl Pts',(19.4812024452277,7.32552654924147,-2.49195982835622));
#116989=CARTESIAN_POINT('Ctrl Pts',(19.3648568003195,9.76303981333453,-1.70373887352032));
#116990=CARTESIAN_POINT('Ctrl Pts',(19.2485111554113,12.2858444955327,-2.14873238805294));
#116991=CARTESIAN_POINT('Ctrl Pts',(19.1321655105031,14.3065750721849,-3.72330750314826));
#116992=CARTESIAN_POINT('Ctrl Pts',(19.0158198655949,15.3546914120593,-6.0608430758138));
#116993=CARTESIAN_POINT('Ctrl Pts',(18.8994742206867,15.1861576903593,-8.61705428265562));
#116994=CARTESIAN_POINT('Ctrl Pts',(18.7831285757785,13.8402116589195,-10.7967447552324));
#116995=CARTESIAN_POINT('Ctrl Pts',(18.6667829308703,11.6302479567442,-12.0923869884339));
#116996=CARTESIAN_POINT('Ctrl Pts',(18.5504372859621,9.07084874640288,-12.2022971968956));
#116997=CARTESIAN_POINT('Ctrl Pts',(18.4340916410539,6.75794006850229,-11.1008873620291));
#116998=CARTESIAN_POINT('Ctrl Pts',(18.3177459961457,5.23009927630059,-9.04460544832903));
#116999=CARTESIAN_POINT('Ctrl Pts',(18.2014003512375,4.84300957956654,-6.51226199696434));
#117000=CARTESIAN_POINT('Ctrl Pts',(18.0850547063294,5.68693870548182,-4.09345999168212));
#117001=CARTESIAN_POINT('Ctrl Pts',(17.9687090614211,7.56509616095713,-2.35148348990379));
#117002=CARTESIAN_POINT('Ctrl Pts',(17.852363416513,10.0407569027593,-1.69178853538612));
#117003=CARTESIAN_POINT('Ctrl Pts',(17.7747996532408,11.70426683511,-2.07631925415564));
#117004=CARTESIAN_POINT('Ctrl Pts',(17.7360177716048,12.4430604270331,-2.45215521583344));
#117005=CARTESIAN_POINT('Ctrl Pts',(17.734,12.4414757859805,-2.45527019889633));
#117006=CARTESIAN_POINT('Ctrl Pts',(17.734,12.3039867051776,-2.39880617496762));
#117007=CARTESIAN_POINT('Ctrl Pts',(17.734,12.1641669931158,-2.34855999836891));
#117008=CARTESIAN_POINT('Ctrl Pts',(17.734,12.0224504771058,-2.30458254792745));
#117009=CARTESIAN_POINT('Ctrl Pts',(17.734,11.8806702982859,-2.26058534165126));
#117010=CARTESIAN_POINT('Ctrl Pts',(17.734,11.7369908080183,-2.22286244827998));
#117011=CARTESIAN_POINT('Ctrl Pts',(17.734,11.5918412576186,-2.19151632697145));
#117012=CARTESIAN_POINT('Ctrl Pts',(17.734,11.5283759217618,-2.1778105172657));
#117013=CARTESIAN_POINT('Ctrl Pts',(17.734,11.4646295457121,-2.16532448472317));
#117014=CARTESIAN_POINT('Ctrl Pts',(17.734,11.4006382986832,-2.15406992347917));
#117015=CARTESIAN_POINT('Ctrl Pts',(17.734,11.3633072808146,-2.14750427198133));
#117016=CARTESIAN_POINT('Ctrl Pts',(17.734,11.325892119771,-2.14135763815236));
#117017=CARTESIAN_POINT('Ctrl Pts',(17.734,11.2884026214455,-2.13563303349493));
#117018=CARTESIAN_POINT('Ctrl Pts',(17.734,11.2692561047234,-2.13270938170717));
#117019=CARTESIAN_POINT('Ctrl Pts',(17.734,11.250091584631,-2.12989604625388));
#117020=CARTESIAN_POINT('Ctrl Pts',(17.734,11.2309171197761,-2.12719424914615));
#117021=CARTESIAN_POINT('Ctrl Pts',(17.734,11.0859964654593,-2.10677405970945));
#117022=CARTESIAN_POINT('Ctrl Pts',(17.734,10.9403799749511,-2.09270150463882));
#117023=CARTESIAN_POINT('Ctrl Pts',(17.734,10.7944837770183,-2.0850637244268));
#117024=CARTESIAN_POINT('Ctrl Pts',(17.734,10.6507966464811,-2.07754159062285));
#117025=CARTESIAN_POINT('Ctrl Pts',(17.734,10.5068375056605,-2.07626094200616));
#117026=CARTESIAN_POINT('Ctrl Pts',(17.734,10.3630121887439,-2.08135439022795));
#117027=CARTESIAN_POINT('Ctrl Pts',(17.734,10.2786127987136,-2.08434332105241));
#117028=CARTESIAN_POINT('Ctrl Pts',(17.734,10.19425970219,-2.08952813543896));
#117029=CARTESIAN_POINT('Ctrl Pts',(17.734,10.1100377343263,-2.0969435515888));
#117030=CARTESIAN_POINT('Ctrl Pts',(17.734,10.0914524803675,-2.09857991079354));
#117031=CARTESIAN_POINT('Ctrl Pts',(17.734,10.0728758846397,-2.10032474830959));
#117032=CARTESIAN_POINT('Ctrl Pts',(17.734,10.054317787698,-2.10217740077462));
#117033=CARTESIAN_POINT('Ctrl Pts',(17.734,10.0520311372889,-2.10240567679508));
#117034=CARTESIAN_POINT('Ctrl Pts',(17.734,10.0497447287136,-2.1026355930538));
#117035=CARTESIAN_POINT('Ctrl Pts',(17.734,10.0474585635589,-2.10286714977861));
#117036=CARTESIAN_POINT('Ctrl Pts',(17.734,9.90553857679407,-2.11724167003299));
#117037=CARTESIAN_POINT('Ctrl Pts',(17.734,9.76455596495627,-2.13793360360503));
#117038=CARTESIAN_POINT('Ctrl Pts',(17.734,9.62489441371198,-2.164760150274));
#117039=CARTESIAN_POINT('Ctrl Pts',(17.734,9.48423704389368,-2.19177797631236));
#117040=CARTESIAN_POINT('Ctrl Pts',(17.734,9.34491888121941,-2.2250185138435));
#117041=CARTESIAN_POINT('Ctrl Pts',(17.734,9.20734701484862,-2.26434539663517));
#117042=CARTESIAN_POINT('Ctrl Pts',(17.734,9.07102557836913,-2.30331482618387));
#117043=CARTESIAN_POINT('Ctrl Pts',(17.734,8.93641816462683,-2.34826086893132));
#117044=CARTESIAN_POINT('Ctrl Pts',(17.734,8.80394629780779,-2.39909462202466));
#117045=CARTESIAN_POINT('Ctrl Pts',(17.734,8.6733123432917,-2.44922310853983));
#117046=CARTESIAN_POINT('Ctrl Pts',(17.734,8.54475450722417,-2.50507746121123));
#117047=CARTESIAN_POINT('Ctrl Pts',(17.734,8.41871108205256,-2.56660923674854));
#117048=CARTESIAN_POINT('Ctrl Pts',(17.734,8.3906008252741,-2.58033207876138));
#117049=CARTESIAN_POINT('Ctrl Pts',(17.734,8.36261639474796,-2.5943371237179));
#117050=CARTESIAN_POINT('Ctrl Pts',(17.734,8.33476077836578,-2.60862517191624));
#117051=CARTESIAN_POINT('Ctrl Pts',(17.734,8.31199476146196,-2.6203025996329));
#117052=CARTESIAN_POINT('Ctrl Pts',(17.734,8.28931855882506,-2.63216728051035));
#117053=CARTESIAN_POINT('Ctrl Pts',(17.734,8.2667549368276,-2.64420787330719));
#117054=CARTESIAN_POINT('Ctrl Pts',(17.734,8.14790051039562,-2.70763198805837));
#117055=CARTESIAN_POINT('Ctrl Pts',(17.734,8.0320302386953,-2.77600356607502));
#117056=CARTESIAN_POINT('Ctrl Pts',(17.734,7.91948448293877,-2.84921041197833));
#117057=CARTESIAN_POINT('Ctrl Pts',(17.734,7.89990776773299,-2.86194434018138));
#117058=CARTESIAN_POINT('Ctrl Pts',(17.734,7.88043170399221,-2.87482465916843));
#117059=CARTESIAN_POINT('Ctrl Pts',(17.734,7.86105816656312,-2.88785089183458));
#117060=CARTESIAN_POINT('Ctrl Pts',(17.734,7.74528165055071,-2.96569583060086));
#117061=CARTESIAN_POINT('Ctrl Pts',(17.734,7.63316351668275,-3.04874885969153));
#117062=CARTESIAN_POINT('Ctrl Pts',(17.734,7.52499462458606,-3.13669681545413));
#117063=CARTESIAN_POINT('Ctrl Pts',(17.734,7.41763480850288,-3.2239869427037));
#117064=CARTESIAN_POINT('Ctrl Pts',(17.734,7.31416494711279,-3.31609973202711));
#117065=CARTESIAN_POINT('Ctrl Pts',(17.734,7.214911090176,-3.41275797650577));
#117066=CARTESIAN_POINT('Ctrl Pts',(17.734,7.13012408682151,-3.49532769371153));
#117067=CARTESIAN_POINT('Ctrl Pts',(17.734,7.04841415790898,-3.58121506916121));
#117068=CARTESIAN_POINT('Ctrl Pts',(17.734,6.9700124957236,-3.67025869427777));
#117069=CARTESIAN_POINT('Ctrl Pts',(17.734,6.95431915067657,-3.68808219819647));
#117070=CARTESIAN_POINT('Ctrl Pts',(17.734,6.93875844510523,-3.70603218668507));
#117071=CARTESIAN_POINT('Ctrl Pts',(17.734,6.92333236973455,-3.72410739902025));
#117072=CARTESIAN_POINT('Ctrl Pts',(17.734,6.91090397970631,-3.7386701301976));
#117073=CARTESIAN_POINT('Ctrl Pts',(17.734,6.89856246392884,-3.75331485694984));
#117074=CARTESIAN_POINT('Ctrl Pts',(17.734,6.88631933290202,-3.7680280979283));
#117075=CARTESIAN_POINT('Ctrl Pts',(17.734,6.79919924774975,-3.87272507487817));
#117076=CARTESIAN_POINT('Ctrl Pts',(17.734,6.71692866786336,-3.98103806042148));
#117077=CARTESIAN_POINT('Ctrl Pts',(17.734,6.63977277908297,-4.09267000357134));
#117078=CARTESIAN_POINT('Ctrl Pts',(17.734,6.5632613323866,-4.20336954449987));
#117079=CARTESIAN_POINT('Ctrl Pts',(17.734,6.49177912370978,-4.31733350190904));
#117080=CARTESIAN_POINT('Ctrl Pts',(17.734,6.42562994043966,-4.43429573639373));
#117081=CARTESIAN_POINT('Ctrl Pts',(17.734,6.40600466641057,-4.46899632964889));
#117082=CARTESIAN_POINT('Ctrl Pts',(17.734,6.38684913115103,-4.5039609540058));
#117083=CARTESIAN_POINT('Ctrl Pts',(17.734,6.36817211518176,-4.5391829311905));
#117084=CARTESIAN_POINT('Ctrl Pts',(17.734,6.30473751328735,-4.6588108259421));
#117085=CARTESIAN_POINT('Ctrl Pts',(17.734,6.24681897356681,-4.78140717330271));
#117086=CARTESIAN_POINT('Ctrl Pts',(17.734,6.19457219597222,-4.90656879650459));
#117087=CARTESIAN_POINT('Ctrl Pts',(17.734,6.16656485885406,-4.97366276739923));
#117088=CARTESIAN_POINT('Ctrl Pts',(17.734,6.14018823211245,-5.04149397277722));
#117089=CARTESIAN_POINT('Ctrl Pts',(17.734,6.11547251223002,-5.11000011542525));
#117090=CARTESIAN_POINT('Ctrl Pts',(17.734,6.10242953315656,-5.14615217529696));
#117091=CARTESIAN_POINT('Ctrl Pts',(17.734,6.08984917083384,-5.1824921894001));
#117092=CARTESIAN_POINT('Ctrl Pts',(17.734,6.07773636071827,-5.2190109187711));
#117093=CARTESIAN_POINT('Ctrl Pts',(17.734,6.06903436379304,-5.24524643866015));
#117094=CARTESIAN_POINT('Ctrl Pts',(17.734,6.06057221982836,-5.27157936590157));
#117095=CARTESIAN_POINT('Ctrl Pts',(17.734,6.05236276271083,-5.29796985459013));
#117096=CARTESIAN_POINT('Ctrl Pts',(17.734,6.01297460247702,-5.42458879933058));
#117097=CARTESIAN_POINT('Ctrl Pts',(17.734,5.97934462682723,-5.55268880308997));
#117098=CARTESIAN_POINT('Ctrl Pts',(17.734,5.95155790702637,-5.68187791684614));
#117099=CARTESIAN_POINT('Ctrl Pts',(17.734,5.92387819466037,-5.81056951971318));
#117100=CARTESIAN_POINT('Ctrl Pts',(17.734,5.90199676488022,-5.9403426690094));
#117101=CARTESIAN_POINT('Ctrl Pts',(17.734,5.88604904275158,-6.07081358829993));
#117102=CARTESIAN_POINT('Ctrl Pts',(17.734,5.87037715516175,-6.19902786017957));
#117103=CARTESIAN_POINT('Ctrl Pts',(17.734,5.86043554854223,-6.32791668515105));
#117104=CARTESIAN_POINT('Ctrl Pts',(17.734,5.85640219965433,-6.45710818642194));
#117105=CARTESIAN_POINT('Ctrl Pts',(17.734,5.85485839225762,-6.50655761437785));
#117106=CARTESIAN_POINT('Ctrl Pts',(17.734,5.85418069613612,-6.55605124999239));
#117107=CARTESIAN_POINT('Ctrl Pts',(17.734,5.85438103290403,-6.60556760587704));
#117108=CARTESIAN_POINT('Ctrl Pts',(17.734,5.85480000921424,-6.70912413372275));
#117109=CARTESIAN_POINT('Ctrl Pts',(17.734,5.85905829450831,-6.81278078385137));
#117110=CARTESIAN_POINT('Ctrl Pts',(17.734,5.86714838588205,-6.9163217216595));
#117111=CARTESIAN_POINT('Ctrl Pts',(23.534,7.33966741897454,-3.77664721604216));
#117112=CARTESIAN_POINT('Ctrl Pts',(23.534,7.42781106532914,-3.68403366522651));
#117113=CARTESIAN_POINT('Ctrl Pts',(23.534,7.52001976376119,-3.59567730315303));
#117114=CARTESIAN_POINT('Ctrl Pts',(23.534,7.61588000351054,-3.5116960194841));
#117115=CARTESIAN_POINT('Ctrl Pts',(23.534,7.71428950783776,-3.42548137491161));
#117116=CARTESIAN_POINT('Ctrl Pts',(23.534,7.81654770306906,-3.34387704110181));
#117117=CARTESIAN_POINT('Ctrl Pts',(23.534,7.92225677096286,-3.26703375166838));
#117118=CARTESIAN_POINT('Ctrl Pts',(23.534,8.0288784923947,-3.18952702530023));
#117119=CARTESIAN_POINT('Ctrl Pts',(23.534,8.13901148194131,-3.11686336121957));
#117120=CARTESIAN_POINT('Ctrl Pts',(23.534,8.25229019245111,-3.04922905261281));
#117121=CARTESIAN_POINT('Ctrl Pts',(23.534,8.36548868721879,-2.98164263770322));
#117122=CARTESIAN_POINT('Ctrl Pts',(23.534,8.48182908276737,-2.91907793776718));
#117123=CARTESIAN_POINT('Ctrl Pts',(23.534,8.60098002351534,-2.86176024172565));
#117124=CARTESIAN_POINT('Ctrl Pts',(23.534,8.62551775116567,-2.84995633983295));
#117125=CARTESIAN_POINT('Ctrl Pts',(23.534,8.6501747700182,-2.83837511497645));
#117126=CARTESIAN_POINT('Ctrl Pts',(23.534,8.67494832377365,-2.82701877421198));
#117127=CARTESIAN_POINT('Ctrl Pts',(23.534,8.69677888932777,-2.81701151631264));
#117128=CARTESIAN_POINT('Ctrl Pts',(23.534,8.7187040887079,-2.80717716259871));
#117129=CARTESIAN_POINT('Ctrl Pts',(23.534,8.7406954034996,-2.7975286977491));
#117130=CARTESIAN_POINT('Ctrl Pts',(23.534,8.86780597067235,-2.74176023410807));
#117131=CARTESIAN_POINT('Ctrl Pts',(23.534,8.99727639743939,-2.69212556532351));
#117132=CARTESIAN_POINT('Ctrl Pts',(23.534,9.12866759232672,-2.6487952833054));
#117133=CARTESIAN_POINT('Ctrl Pts',(23.534,9.25547643309883,-2.60697617329764));
#117134=CARTESIAN_POINT('Ctrl Pts',(23.534,9.38407515938093,-2.57102868262552));
#117135=CARTESIAN_POINT('Ctrl Pts',(23.534,9.51404078368103,-2.54089289360577));
#117136=CARTESIAN_POINT('Ctrl Pts',(23.534,9.64599296324263,-2.51029647193366));
#117137=CARTESIAN_POINT('Ctrl Pts',(23.534,9.77935483569702,-2.48569051020119));
#117138=CARTESIAN_POINT('Ctrl Pts',(23.534,9.91370948271991,-2.46705966806736));
#117139=CARTESIAN_POINT('Ctrl Pts',(23.534,10.0310062349449,-2.45079422937997));
#117140=CARTESIAN_POINT('Ctrl Pts',(23.534,10.1490603917629,-2.43908365615736));
#117141=CARTESIAN_POINT('Ctrl Pts',(23.534,10.2676037380491,-2.43194887296395));
#117142=CARTESIAN_POINT('Ctrl Pts',(23.534,10.3041175791359,-2.42975120984852));
#117143=CARTESIAN_POINT('Ctrl Pts',(23.534,10.3406773911112,-2.4279879127063));
#117144=CARTESIAN_POINT('Ctrl Pts',(23.534,10.3772769926609,-2.42666011382119));
#117145=CARTESIAN_POINT('Ctrl Pts',(23.534,10.4011419710669,-2.42579431500428));
#117146=CARTESIAN_POINT('Ctrl Pts',(23.534,10.4250202863045,-2.42511392850644));
#117147=CARTESIAN_POINT('Ctrl Pts',(23.534,10.4488889853955,-2.42461930902246));
#117148=CARTESIAN_POINT('Ctrl Pts',(23.534,10.5881947642429,-2.42173254287793));
#117149=CARTESIAN_POINT('Ctrl Pts',(23.534,10.7273545089995,-2.42516221226969));
#117150=CARTESIAN_POINT('Ctrl Pts',(23.534,10.8659190931826,-2.43484421425681));
#117151=CARTESIAN_POINT('Ctrl Pts',(23.534,10.9998137686292,-2.44419991305517));
#117152=CARTESIAN_POINT('Ctrl Pts',(23.534,11.1331535299474,-2.45939375404953));
#117153=CARTESIAN_POINT('Ctrl Pts',(23.534,11.2655490821966,-2.48041129060109));
#117154=CARTESIAN_POINT('Ctrl Pts',(23.534,11.2886886126467,-2.48408464607836));
#117155=CARTESIAN_POINT('Ctrl Pts',(23.534,11.3117993244444,-2.48793600302252));
#117156=CARTESIAN_POINT('Ctrl Pts',(23.534,11.3348791639493,-2.49196542192025));
#117157=CARTESIAN_POINT('Ctrl Pts',(23.534,11.4716128752646,-2.51583722571738));
#117158=CARTESIAN_POINT('Ctrl Pts',(23.534,11.6072631372987,-2.54595436303442));
#117159=CARTESIAN_POINT('Ctrl Pts',(23.534,11.741474161821,-2.58210348353803));
#117160=CARTESIAN_POINT('Ctrl Pts',(23.534,11.8669921985643,-2.61591118787352));
#117161=CARTESIAN_POINT('Ctrl Pts',(23.534,11.9912519180839,-2.65499542884546));
#117162=CARTESIAN_POINT('Ctrl Pts',(23.534,12.1139562411199,-2.69922248208064));
#117163=CARTESIAN_POINT('Ctrl Pts',(23.534,12.1324792825538,-2.70589885271947));
#117164=CARTESIAN_POINT('Ctrl Pts',(23.534,12.1509668598302,-2.71269248793648));
#117165=CARTESIAN_POINT('Ctrl Pts',(23.534,12.1694179272643,-2.71960300224709));
#117166=CARTESIAN_POINT('Ctrl Pts',(23.534,12.1864042738565,-2.725964931801));
#117167=CARTESIAN_POINT('Ctrl Pts',(23.534,12.2033501584913,-2.73242235622137));
#117168=CARTESIAN_POINT('Ctrl Pts',(23.534,12.2202547019028,-2.73897459134067));
#117169=CARTESIAN_POINT('Ctrl Pts',(23.534,12.3523840941254,-2.79018821024404));
#117170=CARTESIAN_POINT('Ctrl Pts',(23.534,12.4819900441372,-2.84719066756166));
#117171=CARTESIAN_POINT('Ctrl Pts',(23.534,12.6087145787098,-2.90970780354203));
#117172=CARTESIAN_POINT('Ctrl Pts',(23.534,12.7371473048454,-2.97306764330177));
#117173=CARTESIAN_POINT('Ctrl Pts',(23.534,12.8626211666375,-3.04209197613929));
#117174=CARTESIAN_POINT('Ctrl Pts',(23.534,12.9847605797071,-3.11654906624453));
#117175=CARTESIAN_POINT('Ctrl Pts',(23.534,13.1066107532543,-3.19082983379632));
#117176=CARTESIAN_POINT('Ctrl Pts',(23.534,13.2251430159563,-3.27051793770692));
#117177=CARTESIAN_POINT('Ctrl Pts',(23.534,13.339970121412,-3.35543295399967));
#117178=CARTESIAN_POINT('Ctrl Pts',(23.534,13.3745616920472,-3.38101353249137));
#117179=CARTESIAN_POINT('Ctrl Pts',(23.534,13.4088168737746,-3.40706878536305));
#117180=CARTESIAN_POINT('Ctrl Pts',(23.534,13.442724662023,-3.43359460806598));
#117181=CARTESIAN_POINT('Ctrl Pts',(23.534,13.5222654936816,-3.49581883757828));
#117182=CARTESIAN_POINT('Ctrl Pts',(23.534,13.5998952497886,-3.56063180043892));
#117183=CARTESIAN_POINT('Ctrl Pts',(23.534,13.6755304223662,-3.62791906475953));
#117184=CARTESIAN_POINT('Ctrl Pts',(23.534,13.6988785584492,-3.64869025031349));
#117185=CARTESIAN_POINT('Ctrl Pts',(23.534,13.7220365683719,-3.66969729110703));
#117186=CARTESIAN_POINT('Ctrl Pts',(23.534,13.7450018328666,-3.69093701222324));
#117187=CARTESIAN_POINT('Ctrl Pts',(23.534,13.7616807918054,-3.70636276255376));
#117188=CARTESIAN_POINT('Ctrl Pts',(23.534,13.778252633284,-3.72190625726443));
#117189=CARTESIAN_POINT('Ctrl Pts',(23.534,13.794710755701,-3.73756042625356));
#117190=CARTESIAN_POINT('Ctrl Pts',(23.534,13.8994714966307,-3.83720376954566));
#117191=CARTESIAN_POINT('Ctrl Pts',(23.534,13.9997005890966,-3.94139578034812));
#117192=CARTESIAN_POINT('Ctrl Pts',(23.534,14.0951974348198,-4.04973935219095));
#117193=CARTESIAN_POINT('Ctrl Pts',(23.534,14.1919272854663,-4.15948179911159));
#117194=CARTESIAN_POINT('Ctrl Pts',(23.5339999999999,14.2838024902753,-4.27348416760674));
#117195=CARTESIAN_POINT('Ctrl Pts',(23.534,14.3705861834528,-4.39137862116285));
#117196=CARTESIAN_POINT('Ctrl Pts',(23.534,14.3939765840125,-4.42315415861089));
#117197=CARTESIAN_POINT('Ctrl Pts',(23.534,14.4169969315181,-4.45521265895928));
#117198=CARTESIAN_POINT('Ctrl Pts',(23.5339999999999,14.4396421540893,-4.48754739858326));
#117199=CARTESIAN_POINT('Ctrl Pts',(23.5339999999999,14.4633057306723,-4.52133622909603));
#117200=CARTESIAN_POINT('Ctrl Pts',(23.534,14.486559687685,-4.55542670188665));
#117201=CARTESIAN_POINT('Ctrl Pts',(23.534,14.5093979973546,-4.58981135573279));
#117202=CARTESIAN_POINT('Ctrl Pts',(23.534,14.5229724195575,-4.6102485866559));
#117203=CARTESIAN_POINT('Ctrl Pts',(23.534,14.5363970207432,-4.63078533674386));
#117204=CARTESIAN_POINT('Ctrl Pts',(23.534,14.5496664278029,-4.65141310427564));
#117205=CARTESIAN_POINT('Ctrl Pts',(23.534,14.6302131840669,-4.77662591568344));
#117206=CARTESIAN_POINT('Ctrl Pts',(23.5339999999999,14.7050940684627,-4.90526377791117));
#117207=CARTESIAN_POINT('Ctrl Pts',(23.5339999999999,14.7740779860328,-5.03693509762848));
#117208=CARTESIAN_POINT('Ctrl Pts',(23.5339999999999,14.825130242171,-5.1343798090488));
#117209=CARTESIAN_POINT('Ctrl Pts',(23.534,14.8729522304357,-5.23348688766521));
#117210=CARTESIAN_POINT('Ctrl Pts',(23.534,14.917437260214,-5.33411057035729));
#117211=CARTESIAN_POINT('Ctrl Pts',(23.534,14.9671573568045,-5.44657580299122));
#117212=CARTESIAN_POINT('Ctrl Pts',(23.5339999999999,15.012709422787,-5.56093556570213));
#117213=CARTESIAN_POINT('Ctrl Pts',(23.5339999999999,15.0540735698273,-5.67694764394986));
#117214=CARTESIAN_POINT('Ctrl Pts',(23.531982455913,15.0572810292372,-8.32379157603815));
#117215=CARTESIAN_POINT('Ctrl Pts',(23.4932005742769,14.8422321918575,-9.12430549407578));
#117216=CARTESIAN_POINT('Ctrl Pts',(23.4156368110048,14.0148884746517,-10.6178353680082));
#117217=CARTESIAN_POINT('Ctrl Pts',(23.2992911660966,11.8680998485746,-12.016187756466));
#117218=CARTESIAN_POINT('Ctrl Pts',(23.1829455211884,9.31682643229098,-12.2463209197506));
#117219=CARTESIAN_POINT('Ctrl Pts',(23.0665998762802,6.95460769844995,-11.2549881116262));
#117220=CARTESIAN_POINT('Ctrl Pts',(22.950254231372,5.33172340411622,-9.27285604389766));
#117221=CARTESIAN_POINT('Ctrl Pts',(22.8339085864638,4.82593323769868,-6.76152808689128));
#117222=CARTESIAN_POINT('Ctrl Pts',(22.7175629415556,5.55506413782101,-4.30571512371993));
#117223=CARTESIAN_POINT('Ctrl Pts',(22.6012172966474,7.34931555885556,-2.4772552638758));
#117224=CARTESIAN_POINT('Ctrl Pts',(22.4848716517392,9.79091954839253,-1.70188610485324));
#117225=CARTESIAN_POINT('Ctrl Pts',(22.368526006831,12.3113587413642,-2.16015085039805));
#117226=CARTESIAN_POINT('Ctrl Pts',(22.2521803619228,14.3237647967067,-3.74534492265297));
#117227=CARTESIAN_POINT('Ctrl Pts',(22.1358347170146,15.359565457441,-6.08836358180601));
#117228=CARTESIAN_POINT('Ctrl Pts',(22.0194890721064,15.1775701554181,-8.64365525823664));
#117229=CARTESIAN_POINT('Ctrl Pts',(21.9031434271982,13.820179034717,-10.8162231363412));
#117230=CARTESIAN_POINT('Ctrl Pts',(21.78679778229,11.6034021905309,-12.1002256175434));
#117231=CARTESIAN_POINT('Ctrl Pts',(21.6704521373819,9.04350737951443,-12.1966331433727));
#117232=CARTESIAN_POINT('Ctrl Pts',(21.5541064924736,6.7363305172835,-11.0831182499555));
#117233=CARTESIAN_POINT('Ctrl Pts',(21.4377608475655,5.21954344324481,-9.0187039421408));
#117234=CARTESIAN_POINT('Ctrl Pts',(21.3214152026572,4.84535809285406,-6.48460381961909));
#117235=CARTESIAN_POINT('Ctrl Pts',(21.2050695577491,5.702915485133,-4.06976362634162));
#117236=CARTESIAN_POINT('Ctrl Pts',(21.0887239128409,7.58832332776442,-2.33877399674752));
#117237=CARTESIAN_POINT('Ctrl Pts',(20.9723782679327,10.071393582989,-1.68985471831868));
#117238=CARTESIAN_POINT('Ctrl Pts',(20.8560326230245,12.5555012697233,-2.28420337620227));
#117239=CARTESIAN_POINT('Ctrl Pts',(20.7009050964802,15.1484711142166,-4.52264463641619));
#117240=CARTESIAN_POINT('Ctrl Pts',(20.5069956882999,15.7229262950689,-9.1400595208437));
#117241=CARTESIAN_POINT('Ctrl Pts',(20.2743043984835,11.4791149812055,-12.8347932160127));
#117242=CARTESIAN_POINT('Ctrl Pts',(20.0803949903032,6.98475583574678,-11.6301128262941));
#117243=CARTESIAN_POINT('Ctrl Pts',(19.9252674637589,5.12461279872623,-8.75366018950281));
#117244=CARTESIAN_POINT('Ctrl Pts',(19.8089218188507,4.87791935403154,-6.21138096196604));
#117245=CARTESIAN_POINT('Ctrl Pts',(19.6925761739425,5.8625122183247,-3.84129425176305));
#117246=CARTESIAN_POINT('Ctrl Pts',(19.5762305290343,7.83658937295929,-2.21215115848727));
#117247=CARTESIAN_POINT('Ctrl Pts',(19.4598848841261,10.3464975445664,-1.69521904474282));
#117248=CARTESIAN_POINT('Ctrl Pts',(19.3435392392179,12.8049517620754,-2.41471954357795));
#117249=CARTESIAN_POINT('Ctrl Pts',(19.2271935943097,14.6408867640296,-4.20127828341279));
#117250=CARTESIAN_POINT('Ctrl Pts',(19.1108479494016,15.426161448925,-6.63978687694656));
#117251=CARTESIAN_POINT('Ctrl Pts',(18.9945023044933,14.9782424407922,-9.16203278420036));
#117252=CARTESIAN_POINT('Ctrl Pts',(18.8781566595852,13.4012753699925,-11.1809277310132));
#117253=CARTESIAN_POINT('Ctrl Pts',(18.761811014677,11.0625186928061,-12.2262884555702));
#117254=CARTESIAN_POINT('Ctrl Pts',(18.6454653697688,8.50650341460799,-12.0547549625971));
#117255=CARTESIAN_POINT('Ctrl Pts',(18.5291197248606,6.32839797170798,-10.7062461100025));
#117256=CARTESIAN_POINT('Ctrl Pts',(18.4127740799524,5.03535348126381,-8.49476372842595));
#117257=CARTESIAN_POINT('Ctrl Pts',(18.2964284350442,4.92844999693276,-5.93523409438871));
#117258=CARTESIAN_POINT('Ctrl Pts',(18.180082790136,6.03257984190088,-3.62362758376954));
#117259=CARTESIAN_POINT('Ctrl Pts',(18.0637371452278,8.09064926616096,-2.09819195226243));
#117260=CARTESIAN_POINT('Ctrl Pts',(17.9473915003196,10.6234591356293,-1.71410427383802));
#117261=CARTESIAN_POINT('Ctrl Pts',(17.8310458554114,13.0412395447846,-2.56082128275623));
#117262=CARTESIAN_POINT('Ctrl Pts',(17.7147002105032,14.7810690563125,-4.44113887229518));
#117263=CARTESIAN_POINT('Ctrl Pts',(17.598354565595,15.4377473099555,-6.91734398378451));
#117264=CARTESIAN_POINT('Ctrl Pts',(17.4820089206868,14.8585629802715,-9.41264012447143));
#117265=CARTESIAN_POINT('Ctrl Pts',(17.365659393706,13.177914321498,-11.3465348850005));
#117266=CARTESIAN_POINT('Ctrl Pts',(17.2880917483612,11.5845996678674,-11.9603779011799));
#117267=CARTESIAN_POINT('Ctrl Pts',(17.2493059846525,10.7620144760327,-12.0631388925593));
#117268=CARTESIAN_POINT('Ctrl Pts',(23.6939479204724,14.7863542679684,-8.25101022431757));
#117269=CARTESIAN_POINT('Ctrl Pts',(23.6551660388364,14.5831287004702,-9.00751231596158));
#117270=CARTESIAN_POINT('Ctrl Pts',(23.5776022755642,13.8012718976441,-10.4189287174808));
#117271=CARTESIAN_POINT('Ctrl Pts',(23.4612566306561,11.7725125602348,-11.740400440692));
#117272=CARTESIAN_POINT('Ctrl Pts',(23.3449109857478,9.36150678970984,-11.9578810059372));
#117273=CARTESIAN_POINT('Ctrl Pts',(23.2285653408397,7.12916157645969,-11.0210511445653));
#117274=CARTESIAN_POINT('Ctrl Pts',(23.1122196959314,5.59550259128015,-9.14789563612996));
#117275=CARTESIAN_POINT('Ctrl Pts',(22.9958740510233,5.11752049727005,-6.77463914492913));
#117276=CARTESIAN_POINT('Ctrl Pts',(22.879528406115,5.80656417108524,-4.45384546294059));
#117277=CARTESIAN_POINT('Ctrl Pts',(22.7631827612069,7.5021686101377,-2.72591334671949));
#117278=CARTESIAN_POINT('Ctrl Pts',(22.6468371162987,9.80953452025079,-1.99317356870946));
#117279=CARTESIAN_POINT('Ctrl Pts',(22.5304914713905,12.1914013165442,-2.42624316402794));
#117280=CARTESIAN_POINT('Ctrl Pts',(22.4141458264823,14.0931663649717,-3.92428411534862));
#117281=CARTESIAN_POINT('Ctrl Pts',(22.2978001815741,15.0720192602376,-6.138484863732));
#117282=CARTESIAN_POINT('Ctrl Pts',(22.1814545366659,14.9000299624285,-8.55328797261369));
#117283=CARTESIAN_POINT('Ctrl Pts',(22.0651088917577,13.6172674784149,-10.6064092325833));
#117284=CARTESIAN_POINT('Ctrl Pts',(21.9487632468495,11.5223678376368,-11.8198179451847));
#117285=CARTESIAN_POINT('Ctrl Pts',(21.8324176019413,9.10321467204312,-11.9109250368877));
#117286=CARTESIAN_POINT('Ctrl Pts',(21.7160719570331,6.92288515778683,-10.8586305958217));
#117287=CARTESIAN_POINT('Ctrl Pts',(21.5997263121249,5.48949022456477,-8.90771668078325));
#117288=CARTESIAN_POINT('Ctrl Pts',(21.4833806672167,5.13587738429453,-6.5129400255285));
#117289=CARTESIAN_POINT('Ctrl Pts',(21.3670350223085,5.94628673052317,-4.23086645249341));
#117290=CARTESIAN_POINT('Ctrl Pts',(21.2506893774004,7.72803585994387,-2.59504570547613));
#117291=CARTESIAN_POINT('Ctrl Pts',(21.1343437324921,10.0745882426698,-1.98180366136159));
#117292=CARTESIAN_POINT('Ctrl Pts',(21.017998087584,12.4221210194767,-2.54347534841603));
#117293=CARTESIAN_POINT('Ctrl Pts',(20.8628705610397,14.8725307709244,-4.65884830723382));
#117294=CARTESIAN_POINT('Ctrl Pts',(20.6689611528594,15.4154027136581,-9.02240019477693));
#117295=CARTESIAN_POINT('Ctrl Pts',(20.436269863043,11.4049138725019,-12.5139994105841));
#117296=CARTESIAN_POINT('Ctrl Pts',(20.2423604548627,7.15765218531772,-11.3755517033679));
#117297=CARTESIAN_POINT('Ctrl Pts',(20.0872329283184,5.39977881602929,-8.65724489168638));
#117298=CARTESIAN_POINT('Ctrl Pts',(19.9708872834102,5.16664844477492,-6.25473881422892));
#117299=CARTESIAN_POINT('Ctrl Pts',(19.854541638502,6.09710892081693,-4.01495820174247));
#117300=CARTESIAN_POINT('Ctrl Pts',(19.7381959935938,7.96265237096534,-2.47538452303399));
#117301=CARTESIAN_POINT('Ctrl Pts',(19.6218503486856,10.3345671358076,-1.98687305999249));
#117302=CARTESIAN_POINT('Ctrl Pts',(19.5055047037774,12.6578568573851,-2.66681580682442));
#117303=CARTESIAN_POINT('Ctrl Pts',(19.3891590588692,14.3928531364073,-4.3551505041687));
#117304=CARTESIAN_POINT('Ctrl Pts',(19.272813413961,15.1349538397841,-6.65959120149271));
#117305=CARTESIAN_POINT('Ctrl Pts',(19.1564677690528,14.7116611787767,-9.04316537988491));
#117306=CARTESIAN_POINT('Ctrl Pts',(19.0401221241446,13.2213949127782,-10.9510625640058));
#117307=CARTESIAN_POINT('Ctrl Pts',(18.9237764792364,11.0112218248761,-11.9389499159064));
#117308=CARTESIAN_POINT('Ctrl Pts',(18.8074308343282,8.59573489746441,-11.7768472424898));
#117309=CARTESIAN_POINT('Ctrl Pts',(18.69108518942,6.53738052504534,-10.5024786842401));
#117310=CARTESIAN_POINT('Ctrl Pts',(18.5747395445119,5.31542692802643,-8.41258241935363));
#117311=CARTESIAN_POINT('Ctrl Pts',(18.4583938996037,5.21440093999774,-5.99377435350435));
#117312=CARTESIAN_POINT('Ctrl Pts',(18.3420482546954,6.25782631755088,-3.80925873055534));
#117313=CARTESIAN_POINT('Ctrl Pts',(18.2257026097873,8.20274418733385,-2.36769073292162));
#117314=CARTESIAN_POINT('Ctrl Pts',(18.1093569648791,10.5963015269569,-2.0047199893085));
#117315=CARTESIAN_POINT('Ctrl Pts',(17.9930113199709,12.8811536643759,-2.8048849506466));
#117316=CARTESIAN_POINT('Ctrl Pts',(17.8766656750627,14.5253282813535,-4.58182368636311));
#117317=CARTESIAN_POINT('Ctrl Pts',(17.7603200301545,15.1459027163813,-6.92188836727878));
#117318=CARTESIAN_POINT('Ctrl Pts',(17.6439743852463,14.5985616308853,-9.27999446283346));
#117319=CARTESIAN_POINT('Ctrl Pts',(17.5276248582655,13.0103141350797,-11.1075647253793));
#117320=CARTESIAN_POINT('Ctrl Pts',(17.4500572129207,11.5045990675973,-11.6876589813532));
#117321=CARTESIAN_POINT('Ctrl Pts',(17.411271449212,10.7272391689664,-11.7847702284737));
#117322=CARTESIAN_POINT('Ctrl Pts',(23.8559133850319,14.5154275066996,-8.17822887259699));
#117323=CARTESIAN_POINT('Ctrl Pts',(23.8171315033958,14.324025209083,-8.89071913784739));
#117324=CARTESIAN_POINT('Ctrl Pts',(23.7395677401237,13.5876553206365,-10.2200220669534));
#117325=CARTESIAN_POINT('Ctrl Pts',(23.6232220952155,11.6769252718951,-11.4646131249179));
#117326=CARTESIAN_POINT('Ctrl Pts',(23.5068764503073,9.40618714712869,-11.6694410921238));
#117327=CARTESIAN_POINT('Ctrl Pts',(23.3905308053991,7.30371545446943,-10.7871141775044));
#117328=CARTESIAN_POINT('Ctrl Pts',(23.2741851604909,5.85928177844407,-9.02293522836227));
#117329=CARTESIAN_POINT('Ctrl Pts',(23.1578395155828,5.40910775684145,-6.78775020296697));
#117330=CARTESIAN_POINT('Ctrl Pts',(23.0414938706745,6.05806420434945,-4.60197580216125));
#117331=CARTESIAN_POINT('Ctrl Pts',(22.9251482257664,7.65502166141984,-2.97457142956318));
#117332=CARTESIAN_POINT('Ctrl Pts',(22.8088025808582,9.82814949210905,-2.28446103256568));
#117333=CARTESIAN_POINT('Ctrl Pts',(22.69245693595,12.0714438917243,-2.69233547765782));
#117334=CARTESIAN_POINT('Ctrl Pts',(22.5761112910418,13.8625679332368,-4.10322330804428));
#117335=CARTESIAN_POINT('Ctrl Pts',(22.4597656461336,14.7844730630341,-6.188606145658));
#117336=CARTESIAN_POINT('Ctrl Pts',(22.3434200012254,14.6224897694389,-8.46292068699072));
#117337=CARTESIAN_POINT('Ctrl Pts',(22.2270743563172,13.4143559221128,-10.3965953288256));
#117338=CARTESIAN_POINT('Ctrl Pts',(22.110728711409,11.4413334847428,-11.5394102728262));
#117339=CARTESIAN_POINT('Ctrl Pts',(21.9943830665008,9.1629219645718,-11.6252169304027));
#117340=CARTESIAN_POINT('Ctrl Pts',(21.8780374215926,7.10943979829016,-10.6341429416881));
#117341=CARTESIAN_POINT('Ctrl Pts',(21.7616917766844,5.75943700588474,-8.79672941942568));
#117342=CARTESIAN_POINT('Ctrl Pts',(21.6453461317762,5.42639667573499,-6.5412762314379));
#117343=CARTESIAN_POINT('Ctrl Pts',(21.529000486868,6.18965797591334,-4.39196927864519));
#117344=CARTESIAN_POINT('Ctrl Pts',(21.4126548419598,7.86774839212332,-2.85131741420474));
#117345=CARTESIAN_POINT('Ctrl Pts',(21.2963091970516,10.0777829023506,-2.2737526044045));
#117346=CARTESIAN_POINT('Ctrl Pts',(21.1799635521434,12.2887407692301,-2.80274732062977));
#117347=CARTESIAN_POINT('Ctrl Pts',(21.0248360255992,14.5965904276323,-4.79505197805147));
#117348=CARTESIAN_POINT('Ctrl Pts',(20.8309266174188,15.1078791322475,-8.90474086871017));
#117349=CARTESIAN_POINT('Ctrl Pts',(20.5982353276024,11.3307127637984,-12.1932056051556));
#117350=CARTESIAN_POINT('Ctrl Pts',(20.4043259194221,7.33054853488867,-11.1209905804417));
#117351=CARTESIAN_POINT('Ctrl Pts',(20.2491983928779,5.67494483333233,-8.56082959386996));
#117352=CARTESIAN_POINT('Ctrl Pts',(20.1328527479697,5.45537753551829,-6.29809666649179));
#117353=CARTESIAN_POINT('Ctrl Pts',(20.0165071030615,6.33170562330916,-4.18862215172188));
#117354=CARTESIAN_POINT('Ctrl Pts',(19.9001614581533,8.08871536897138,-2.73861788758071));
#117355=CARTESIAN_POINT('Ctrl Pts',(19.7838158132451,10.3226367270489,-2.27852707524217));
#117356=CARTESIAN_POINT('Ctrl Pts',(19.6674701683369,12.510761952695,-2.91891207007088));
#117357=CARTESIAN_POINT('Ctrl Pts',(19.5511245234287,14.1448195087852,-4.50902272492462));
#117358=CARTESIAN_POINT('Ctrl Pts',(19.4347788785205,14.843746230643,-6.67939552603887));
#117359=CARTESIAN_POINT('Ctrl Pts',(19.3184332336123,14.4450799167611,-8.92429797556946));
#117360=CARTESIAN_POINT('Ctrl Pts',(19.2020875887041,13.0415144555639,-10.7211973969982));
#117361=CARTESIAN_POINT('Ctrl Pts',(19.0857419437959,10.959924956946,-11.6516113762426));
#117362=CARTESIAN_POINT('Ctrl Pts',(18.9693962988877,8.68496638032083,-11.4989395223824));
#117363=CARTESIAN_POINT('Ctrl Pts',(18.8530506539795,6.7463630783827,-10.2987112584779));
#117364=CARTESIAN_POINT('Ctrl Pts',(18.7367050090713,5.59550037478904,-8.33040111028128));
#117365=CARTESIAN_POINT('Ctrl Pts',(18.6203593641631,5.50035188306271,-6.05231461262));
#117366=CARTESIAN_POINT('Ctrl Pts',(18.5040137192549,6.48307279320089,-3.99488987734113));
#117367=CARTESIAN_POINT('Ctrl Pts',(18.3876680743467,8.31483910850671,-2.63718951358079));
#117368=CARTESIAN_POINT('Ctrl Pts',(18.2713224294385,10.5691439182845,-2.29533570477897));
#117369=CARTESIAN_POINT('Ctrl Pts',(18.1549767845304,12.7210677839672,-3.04894861853697));
#117370=CARTESIAN_POINT('Ctrl Pts',(18.0386311396222,14.2695875063947,-4.72250850043103));
#117371=CARTESIAN_POINT('Ctrl Pts',(17.922285494714,14.8540581228072,-6.92643275077305));
#117372=CARTESIAN_POINT('Ctrl Pts',(17.8059398498058,14.3385602814992,-9.14734880119549));
#117373=CARTESIAN_POINT('Ctrl Pts',(17.6895903228249,12.8427139486614,-10.8685945657582));
#117374=CARTESIAN_POINT('Ctrl Pts',(17.6120226774801,11.4245984673272,-11.4149400615265));
#117375=CARTESIAN_POINT('Ctrl Pts',(17.5732369137714,10.6924638619,-11.5064015643881));
#117376=CARTESIAN_POINT('Ctrl Pts',(24.0178788495913,14.2445007454307,-8.1054475208764));
#117377=CARTESIAN_POINT('Ctrl Pts',(23.9790969679552,14.0649217176957,-8.77392595973318));
#117378=CARTESIAN_POINT('Ctrl Pts',(23.9015332046831,13.374038743629,-10.0211154164259));
#117379=CARTESIAN_POINT('Ctrl Pts',(23.7851875597749,11.5813379835554,-11.1888258091439));
#117380=CARTESIAN_POINT('Ctrl Pts',(23.6688419148667,9.45086750454755,-11.3810011783102));
#117381=CARTESIAN_POINT('Ctrl Pts',(23.5524962699585,7.47826933247917,-10.5531772104435));
#117382=CARTESIAN_POINT('Ctrl Pts',(23.4361506250503,6.123060965608,-8.89797482059457));
#117383=CARTESIAN_POINT('Ctrl Pts',(23.3198049801421,5.70069501641282,-6.80086126100482));
#117384=CARTESIAN_POINT('Ctrl Pts',(23.2034593352339,6.30956423761369,-4.75010614138192));
#117385=CARTESIAN_POINT('Ctrl Pts',(23.0871136903257,7.80787471270198,-3.22322951240687));
#117386=CARTESIAN_POINT('Ctrl Pts',(22.9707680454175,9.84676446396732,-2.5757484964219));
#117387=CARTESIAN_POINT('Ctrl Pts',(22.8544224005093,11.9514864669044,-2.95842779128772));
#117388=CARTESIAN_POINT('Ctrl Pts',(22.7380767556011,13.6319695015019,-4.28216250073993));
#117389=CARTESIAN_POINT('Ctrl Pts',(22.6217311106929,14.4969268658308,-6.238727427584));
#117390=CARTESIAN_POINT('Ctrl Pts',(22.5053854657848,14.3449495764493,-8.37255340136776));
#117391=CARTESIAN_POINT('Ctrl Pts',(22.3890398208766,13.2114443658107,-10.1867814250677));
#117392=CARTESIAN_POINT('Ctrl Pts',(22.2726941759684,11.3602991318489,-11.2590026004677));
#117393=CARTESIAN_POINT('Ctrl Pts',(22.1563485310602,9.22262925710048,-11.3395088239177));
#117394=CARTESIAN_POINT('Ctrl Pts',(22.040002886152,7.29599443879349,-10.4096552875544));
#117395=CARTESIAN_POINT('Ctrl Pts',(21.9236572412438,6.02938378720469,-8.68574215806813));
#117396=CARTESIAN_POINT('Ctrl Pts',(21.8073115963356,5.71691596717546,-6.56961243734728));
#117397=CARTESIAN_POINT('Ctrl Pts',(21.6909659514274,6.43302922130351,-4.55307210479699));
#117398=CARTESIAN_POINT('Ctrl Pts',(21.5746203065192,8.00746092430277,-3.10758912293336));
#117399=CARTESIAN_POINT('Ctrl Pts',(21.458274661611,10.0809775620313,-2.56570154744741));
#117400=CARTESIAN_POINT('Ctrl Pts',(21.3419290167028,12.1553605189835,-3.06201929284352));
#117401=CARTESIAN_POINT('Ctrl Pts',(21.1868014901586,14.3206500843401,-4.93125564886911));
#117402=CARTESIAN_POINT('Ctrl Pts',(20.9928920819782,14.8003555508367,-8.7870815426434));
#117403=CARTESIAN_POINT('Ctrl Pts',(20.7602007921619,11.2565116550948,-11.8724117997271));
#117404=CARTESIAN_POINT('Ctrl Pts',(20.5662913839815,7.50344488445961,-10.8664294575155));
#117405=CARTESIAN_POINT('Ctrl Pts',(20.4111638574373,5.95011085063539,-8.46441429605354));
#117406=CARTESIAN_POINT('Ctrl Pts',(20.294818212529,5.74410662626167,-6.34145451875465));
#117407=CARTESIAN_POINT('Ctrl Pts',(20.1784725676209,6.56630232580139,-4.36228610170129));
#117408=CARTESIAN_POINT('Ctrl Pts',(20.0621269227127,8.21477836697742,-3.00185125212742));
#117409=CARTESIAN_POINT('Ctrl Pts',(19.9457812778045,10.31070631829,-2.57018109049185));
#117410=CARTESIAN_POINT('Ctrl Pts',(19.8294356328963,12.3636670480047,-3.17100833331735));
#117411=CARTESIAN_POINT('Ctrl Pts',(19.7130899879881,13.896785881163,-4.66289494568054));
#117412=CARTESIAN_POINT('Ctrl Pts',(19.5967443430799,14.5525386215021,-6.69919985058501));
#117413=CARTESIAN_POINT('Ctrl Pts',(19.4803986981717,14.1784986547455,-8.80543057125401));
#117414=CARTESIAN_POINT('Ctrl Pts',(19.3640530532635,12.8616339983496,-10.4913322299906));
#117415=CARTESIAN_POINT('Ctrl Pts',(19.2477074083553,10.9086280890158,-11.3642728365788));
#117416=CARTESIAN_POINT('Ctrl Pts',(19.1313617634471,8.77419786317726,-11.221031802275));
#117417=CARTESIAN_POINT('Ctrl Pts',(19.0150161185389,6.95534563172006,-10.0949438327155));
#117418=CARTESIAN_POINT('Ctrl Pts',(18.8986704736307,5.87557382155166,-8.24821980120896));
#117419=CARTESIAN_POINT('Ctrl Pts',(18.7823248287225,5.78630282612769,-6.11085487173564));
#117420=CARTESIAN_POINT('Ctrl Pts',(18.6659791838143,6.70831926885089,-4.18052102412694));
#117421=CARTESIAN_POINT('Ctrl Pts',(18.5496335389061,8.42693402967958,-2.90668829423997));
#117422=CARTESIAN_POINT('Ctrl Pts',(18.4332878939979,10.5419863096122,-2.58595142024945));
#117423=CARTESIAN_POINT('Ctrl Pts',(18.3169422490897,12.5609819035585,-3.29301228642734));
#117424=CARTESIAN_POINT('Ctrl Pts',(18.2005966041815,14.0138467314357,-4.86319331449896));
#117425=CARTESIAN_POINT('Ctrl Pts',(18.0842509592733,14.5622135292331,-6.93097713426731));
#117426=CARTESIAN_POINT('Ctrl Pts',(17.9679053143652,14.078558932113,-9.01470313955753));
#117427=CARTESIAN_POINT('Ctrl Pts',(17.8515557873843,12.6751137622431,-10.629624406137));
#117428=CARTESIAN_POINT('Ctrl Pts',(17.7739881420395,11.3445978670571,-11.1422211416999));
#117429=CARTESIAN_POINT('Ctrl Pts',(17.7352023783309,10.6576885548338,-11.2280329003024));
#117430=CARTESIAN_POINT('Ctrl Pts',(17.734,10.6581555755053,-11.2300936493755));
#117431=CARTESIAN_POINT('Ctrl Pts',(17.734,10.7871580301293,-11.2265276116833));
#117432=CARTESIAN_POINT('Ctrl Pts',(17.734,10.9158060854873,-11.2169788999138));
#117433=CARTESIAN_POINT('Ctrl Pts',(17.734,11.0437268225087,-11.2016549886172));
#117434=CARTESIAN_POINT('Ctrl Pts',(17.734,11.1739880982412,-11.1860506989516));
#117435=CARTESIAN_POINT('Ctrl Pts',(17.7339999999999,11.3034959147556,-11.1644579899712));
#117436=CARTESIAN_POINT('Ctrl Pts',(17.734,11.4318673763278,-11.1370431572385));
#117437=CARTESIAN_POINT('Ctrl Pts',(17.734,11.4884530911241,-11.1249587898316));
#117438=CARTESIAN_POINT('Ctrl Pts',(17.734,11.5448180845801,-11.1117424890276));
#117439=CARTESIAN_POINT('Ctrl Pts',(17.734,11.6009296449061,-11.0974052968746));
#117440=CARTESIAN_POINT('Ctrl Pts',(17.7339999999999,11.6231422455803,-11.0917297048534));
#117441=CARTESIAN_POINT('Ctrl Pts',(17.734,11.6453151296432,-11.0858784376901));
#117442=CARTESIAN_POINT('Ctrl Pts',(17.734,11.6674462597462,-11.0798520970063));
#117443=CARTESIAN_POINT('Ctrl Pts',(17.734,11.6909691969026,-11.0734467651264));
#117444=CARTESIAN_POINT('Ctrl Pts',(17.7339999999999,11.7144371000566,-11.0668457533736));
#117445=CARTESIAN_POINT('Ctrl Pts',(17.7339999999999,11.7378417469922,-11.0600519299264));
#117446=CARTESIAN_POINT('Ctrl Pts',(17.7339999999999,11.8666178352729,-11.0226712332466));
#117447=CARTESIAN_POINT('Ctrl Pts',(17.734,11.9935344010332,-10.9794425381218));
#117448=CARTESIAN_POINT('Ctrl Pts',(17.734,12.1181943387372,-10.9305490461558));
#117449=CARTESIAN_POINT('Ctrl Pts',(17.734,12.2170317257716,-10.8917835447612));
#117450=CARTESIAN_POINT('Ctrl Pts',(17.7339999999999,12.3144508717194,-10.8494559613376));
#117451=CARTESIAN_POINT('Ctrl Pts',(17.734,12.4102527649422,-10.8036343689628));
#117452=CARTESIAN_POINT('Ctrl Pts',(17.734,12.4582931021382,-10.7806569029182));
#117453=CARTESIAN_POINT('Ctrl Pts',(17.7339999999999,12.5059267258685,-10.7568005259236));
#117454=CARTESIAN_POINT('Ctrl Pts',(17.7339999999999,12.5531281105939,-10.7320719318602));
#117455=CARTESIAN_POINT('Ctrl Pts',(17.7339999999999,12.5796828219838,-10.7181600374899));
#117456=CARTESIAN_POINT('Ctrl Pts',(17.734,12.6061007231861,-10.703972063894));
#117457=CARTESIAN_POINT('Ctrl Pts',(17.734,12.6323772088884,-10.6895090305751));
#117458=CARTESIAN_POINT('Ctrl Pts',(17.734,12.6494661520011,-10.6801029799934));
#117459=CARTESIAN_POINT('Ctrl Pts',(17.734,12.6664940896698,-10.6705811847365));
#117460=CARTESIAN_POINT('Ctrl Pts',(17.734,12.683449666574,-10.6609498639215));
#117461=CARTESIAN_POINT('Ctrl Pts',(17.734,12.6867649951574,-10.6590666491319));
#117462=CARTESIAN_POINT('Ctrl Pts',(17.7339999999999,12.6900776631735,-10.6571791889994));
#117463=CARTESIAN_POINT('Ctrl Pts',(17.7339999999999,12.6933876620448,-10.6552874881657));
#117464=CARTESIAN_POINT('Ctrl Pts',(17.734,12.813721983353,-10.5865150973585));
#117465=CARTESIAN_POINT('Ctrl Pts',(17.7339999999999,12.9305291947834,-10.5121431425042));
#117466=CARTESIAN_POINT('Ctrl Pts',(17.7339999999999,13.0435566004255,-10.4326032510522));
#117467=CARTESIAN_POINT('Ctrl Pts',(17.7339999999999,13.1542860408063,-10.3546804887062));
#117468=CARTESIAN_POINT('Ctrl Pts',(17.734,13.2613883832878,-10.2717971251544));
#117469=CARTESIAN_POINT('Ctrl Pts',(17.734,13.3646136018083,-10.1843046204669));
#117470=CARTESIAN_POINT('Ctrl Pts',(17.734,13.4710521658324,-10.0940885211912));
#117471=CARTESIAN_POINT('Ctrl Pts',(17.734,13.5733692644385,-9.99897159633853));
#117472=CARTESIAN_POINT('Ctrl Pts',(17.734,13.6712668291686,-9.89928713892356));
#117473=CARTESIAN_POINT('Ctrl Pts',(17.734,13.7691643938987,-9.79960268150859));
#117474=CARTESIAN_POINT('Ctrl Pts',(17.734,13.8626431607924,-9.69535014068121));
#117475=CARTESIAN_POINT('Ctrl Pts',(17.734,13.9513699801085,-9.58681812087919));
#117476=CARTESIAN_POINT('Ctrl Pts',(17.734,13.9628634835586,-9.57275908941993));
#117477=CARTESIAN_POINT('Ctrl Pts',(17.734,13.9742785921472,-9.55862643429634));
#117478=CARTESIAN_POINT('Ctrl Pts',(17.734,13.9856099775934,-9.5444264491211));
#117479=CARTESIAN_POINT('Ctrl Pts',(17.734,14.0729113490609,-9.43502427702995));
#117480=CARTESIAN_POINT('Ctrl Pts',(17.734,14.155041858068,-9.32188662452608));
#117481=CARTESIAN_POINT('Ctrl Pts',(17.734,14.2317472591746,-9.20538350790436));
#117482=CARTESIAN_POINT('Ctrl Pts',(17.734,14.2502066068323,-9.17734673993373));
#117483=CARTESIAN_POINT('Ctrl Pts',(17.734,14.2683516627921,-9.14911485201464));
#117484=CARTESIAN_POINT('Ctrl Pts',(17.734,14.2861786693898,-9.12069260839312));
#117485=CARTESIAN_POINT('Ctrl Pts',(17.734,14.3596274174382,-9.00359060367398));
#117486=CARTESIAN_POINT('Ctrl Pts',(17.734,14.4276801174427,-8.88326038142567));
#117487=CARTESIAN_POINT('Ctrl Pts',(17.734,14.4902884333848,-8.76012784854764));
#117488=CARTESIAN_POINT('Ctrl Pts',(17.734,14.5537529998899,-8.63531131732177));
#117489=CARTESIAN_POINT('Ctrl Pts',(17.734,14.6116236543302,-8.50761468832594));
#117490=CARTESIAN_POINT('Ctrl Pts',(17.734,14.6638094340167,-8.37744644945232));
#117491=CARTESIAN_POINT('Ctrl Pts',(17.734,14.7100740696579,-8.26204746184093));
#117492=CARTESIAN_POINT('Ctrl Pts',(17.734,14.7518702709579,-8.14470509092101));
#117493=CARTESIAN_POINT('Ctrl Pts',(17.734,14.7891046475072,-8.02568745899151));
#117494=CARTESIAN_POINT('Ctrl Pts',(17.734,14.7957588699923,-8.0044176036614));
#117495=CARTESIAN_POINT('Ctrl Pts',(17.734,14.802267320164,-7.98309421356168));
#117496=CARTESIAN_POINT('Ctrl Pts',(17.734,14.8086293625773,-7.9617187827321));
#117497=CARTESIAN_POINT('Ctrl Pts',(17.734,14.8141582507119,-7.94314261517331));
#117498=CARTESIAN_POINT('Ctrl Pts',(17.734,14.8195767038318,-7.92452645243315));
#117499=CARTESIAN_POINT('Ctrl Pts',(17.734,14.8248800133524,-7.90588690657763));
#117500=CARTESIAN_POINT('Ctrl Pts',(17.734,14.8642211214105,-7.76761468527757));
#117501=CARTESIAN_POINT('Ctrl Pts',(17.734,14.8972903477015,-7.62785672464364));
#117502=CARTESIAN_POINT('Ctrl Pts',(17.734,14.9240435546541,-7.48706785777855));
#117503=CARTESIAN_POINT('Ctrl Pts',(17.734,14.9507706801502,-7.34641624469049));
#117504=CARTESIAN_POINT('Ctrl Pts',(17.734,14.9711943919531,-7.20473499473391));
#117505=CARTESIAN_POINT('Ctrl Pts',(17.734,14.9852278277044,-7.06244825044858));
#117506=CARTESIAN_POINT('Ctrl Pts',(17.734,14.9897675457622,-7.01641948644057));
#117507=CARTESIAN_POINT('Ctrl Pts',(17.734,14.9936381823968,-6.9703271759923));
#117508=CARTESIAN_POINT('Ctrl Pts',(17.734,14.9968357553433,-6.92418521713769));
#117509=CARTESIAN_POINT('Ctrl Pts',(17.7339999999999,15.0067323514289,-6.78137429866482));
#117510=CARTESIAN_POINT('Ctrl Pts',(17.734,15.010185425558,-6.63808849971123));
#117511=CARTESIAN_POINT('Ctrl Pts',(17.734,15.0073112040798,-6.49472810706362));
#117512=CARTESIAN_POINT('Ctrl Pts',(17.734,15.0056440306924,-6.41157284806938));
#117513=CARTESIAN_POINT('Ctrl Pts',(17.734,15.0018470671246,-6.32839227527476));
#117514=CARTESIAN_POINT('Ctrl Pts',(17.734,14.9959350165701,-6.24526375434569));
#117515=CARTESIAN_POINT('Ctrl Pts',(17.734,14.9930494071184,-6.20468960101485));
#117516=CARTESIAN_POINT('Ctrl Pts',(17.734,14.9896598294849,-6.16412784684823));
#117517=CARTESIAN_POINT('Ctrl Pts',(17.734,14.9857674896188,-6.12358750933691));
#117518=CARTESIAN_POINT('Ctrl Pts',(17.734,14.9839181537182,-6.10432590727623));
#117519=CARTESIAN_POINT('Ctrl Pts',(17.734,14.9819550242892,-6.08506643814876));
#117520=CARTESIAN_POINT('Ctrl Pts',(17.734,14.9798791802301,-6.06581902520355));
#117521=CARTESIAN_POINT('Ctrl Pts',(17.734,14.9642028796882,-5.92046695568585));
#117522=CARTESIAN_POINT('Ctrl Pts',(17.734,14.9421349343852,-5.77608373015697));
#117523=CARTESIAN_POINT('Ctrl Pts',(17.734,14.9138625332143,-5.63308993321275));
#117524=CARTESIAN_POINT('Ctrl Pts',(17.734,14.8852999124013,-5.48862828752365));
#117525=CARTESIAN_POINT('Ctrl Pts',(17.734,14.8504048158092,-5.34558398961965));
#117526=CARTESIAN_POINT('Ctrl Pts',(17.734,14.809317815667,-5.20437943584449));
#117527=CARTESIAN_POINT('Ctrl Pts',(17.734,14.7681579286984,-5.06292439038676));
#117528=CARTESIAN_POINT('Ctrl Pts',(17.734,14.7207840951756,-4.92331482471784));
#117529=CARTESIAN_POINT('Ctrl Pts',(17.734,14.6672857084543,-4.78597583902191));
#117530=CARTESIAN_POINT('Ctrl Pts',(17.734,14.6372084702442,-4.70876271837517));
#117531=CARTESIAN_POINT('Ctrl Pts',(17.734,14.6051944642096,-4.63226735310747));
#117532=CARTESIAN_POINT('Ctrl Pts',(17.734,14.5712524834494,-4.55656680407633));
#117533=CARTESIAN_POINT('Ctrl Pts',(17.734,14.5209818578362,-4.44444859901506));
#117534=CARTESIAN_POINT('Ctrl Pts',(17.734,14.4664830452091,-4.33407329976893));
#117535=CARTESIAN_POINT('Ctrl Pts',(17.734,14.4079024230562,-4.22562346067728));
#117536=CARTESIAN_POINT('Ctrl Pts',(23.534,15.0539061944433,-8.32288496556903));
#117537=CARTESIAN_POINT('Ctrl Pts',(23.534,15.0045196831565,-8.46102105477097));
#117538=CARTESIAN_POINT('Ctrl Pts',(23.534,14.9491584466399,-8.59666359933272));
#117539=CARTESIAN_POINT('Ctrl Pts',(23.534,14.8880945730865,-8.72949016701654));
#117540=CARTESIAN_POINT('Ctrl Pts',(23.534,14.8263802252152,-8.86373165101629));
#117541=CARTESIAN_POINT('Ctrl Pts',(23.534,14.7588406646494,-8.9950975097176));
#117542=CARTESIAN_POINT('Ctrl Pts',(23.534,14.6857106710858,-9.12322928795019));
#117543=CARTESIAN_POINT('Ctrl Pts',(23.534,14.6128819085607,-9.25083327632891));
#117544=CARTESIAN_POINT('Ctrl Pts',(23.534,14.5345081505571,-9.37523035923853));
#117545=CARTESIAN_POINT('Ctrl Pts',(23.534,14.4507831744512,-9.49603193130466));
#117546=CARTESIAN_POINT('Ctrl Pts',(23.534,14.3684650046213,-9.61480370990148));
#117547=CARTESIAN_POINT('Ctrl Pts',(23.534,14.2809734005509,-9.73010024311516));
#117548=CARTESIAN_POINT('Ctrl Pts',(23.534,14.1884635407854,-9.84151116501367));
#117549=CARTESIAN_POINT('Ctrl Pts',(23.534,14.1636970862179,-9.87133775368768));
#117550=CARTESIAN_POINT('Ctrl Pts',(23.534,14.1385708227766,-9.90088559984928));
#117551=CARTESIAN_POINT('Ctrl Pts',(23.534,14.1130874412093,-9.9301462552455));
#117552=CARTESIAN_POINT('Ctrl Pts',(23.534,14.0994446628436,-9.94581123421829));
#117553=CARTESIAN_POINT('Ctrl Pts',(23.534,14.0856995289216,-9.96139389704753));
#117554=CARTESIAN_POINT('Ctrl Pts',(23.534,14.0718524398192,-9.97689291659844));
#117555=CARTESIAN_POINT('Ctrl Pts',(23.534,14.0595282691968,-9.99068733649516));
#117556=CARTESIAN_POINT('Ctrl Pts',(23.534,14.0471248899774,-10.0044136985475));
#117557=CARTESIAN_POINT('Ctrl Pts',(23.534,14.0346501013912,-10.0180631245397));
#117558=CARTESIAN_POINT('Ctrl Pts',(23.534,13.9325629744592,-10.129762867921));
#117559=CARTESIAN_POINT('Ctrl Pts',(23.534,13.8255589167938,-10.2364694610508));
#117560=CARTESIAN_POINT('Ctrl Pts',(23.534,13.7138822995671,-10.3377901011926));
#117561=CARTESIAN_POINT('Ctrl Pts',(23.534,13.6072656917372,-10.4345199558688));
#117562=CARTESIAN_POINT('Ctrl Pts',(23.534,13.4963893994937,-10.5263409917788));
#117563=CARTESIAN_POINT('Ctrl Pts',(23.534,13.3816361432654,-10.6130491512947));
#117564=CARTESIAN_POINT('Ctrl Pts',(23.534,13.2675216549448,-10.6992746544448));
#117565=CARTESIAN_POINT('Ctrl Pts',(23.534,13.1495724821822,-10.7804443135787));
#117566=CARTESIAN_POINT('Ctrl Pts',(23.534,13.028145213054,-10.8563104469597));
#117567=CARTESIAN_POINT('Ctrl Pts',(23.534,12.9228679009085,-10.9220863032608));
#117568=CARTESIAN_POINT('Ctrl Pts',(23.534,12.8149755625505,-10.9838749598991));
#117569=CARTESIAN_POINT('Ctrl Pts',(23.534,12.7046950051531,-11.0414837392859));
#117570=CARTESIAN_POINT('Ctrl Pts',(23.534,12.6704660549416,-11.0593643892202));
#117571=CARTESIAN_POINT('Ctrl Pts',(23.534,12.6360070180388,-11.0768421453942));
#117572=CARTESIAN_POINT('Ctrl Pts',(23.534,12.6013246618057,-11.0939106397649));
#117573=CARTESIAN_POINT('Ctrl Pts',(23.534,12.5775343548302,-11.1056187462719));
#117574=CARTESIAN_POINT('Ctrl Pts',(23.534,12.5536338344587,-11.1171366062184));
#117575=CARTESIAN_POINT('Ctrl Pts',(23.534,12.5296548188552,-11.1284484392924));
#117576=CARTESIAN_POINT('Ctrl Pts',(23.534,12.4026030627483,-11.1883836877031));
#117577=CARTESIAN_POINT('Ctrl Pts',(23.534,12.2732186532335,-11.2426060623178));
#117578=CARTESIAN_POINT('Ctrl Pts',(23.534,12.1418579788867,-11.2909272251374));
#117579=CARTESIAN_POINT('Ctrl Pts',(23.534,12.0110656904146,-11.3390393066126));
#117580=CARTESIAN_POINT('Ctrl Pts',(23.534,11.8783134757111,-11.381301368659));
#117581=CARTESIAN_POINT('Ctrl Pts',(23.534,11.7439408942886,-11.4174776418709));
#117582=CARTESIAN_POINT('Ctrl Pts',(23.534,11.7185306168275,-11.4243186888322));
#117583=CARTESIAN_POINT('Ctrl Pts',(23.534,11.6930623778329,-11.4309419582457));
#117584=CARTESIAN_POINT('Ctrl Pts',(23.534,11.6675384567621,-11.4373456433974));
#117585=CARTESIAN_POINT('Ctrl Pts',(23.534,11.5320041155766,-11.4713497936919));
#117586=CARTESIAN_POINT('Ctrl Pts',(23.534,11.394899148674,-11.4991663992332));
#117587=CARTESIAN_POINT('Ctrl Pts',(23.534,11.2566535581235,-11.5207487746459));
#117588=CARTESIAN_POINT('Ctrl Pts',(23.534,11.1395174117289,-11.5390356239828));
#117589=CARTESIAN_POINT('Ctrl Pts',(23.534,11.0215621487013,-11.5528458727715));
#117590=CARTESIAN_POINT('Ctrl Pts',(23.534,10.9030568789718,-11.5621227836795));
#117591=CARTESIAN_POINT('Ctrl Pts',(23.534,10.8727885717626,-11.5644922680911));
#117592=CARTESIAN_POINT('Ctrl Pts',(23.534,10.842484435087,-11.5665658756357));
#117593=CARTESIAN_POINT('Ctrl Pts',(23.534,10.8121490716819,-11.5683423926637));
#117594=CARTESIAN_POINT('Ctrl Pts',(23.534,10.7942046025595,-11.5693932670024));
#117595=CARTESIAN_POINT('Ctrl Pts',(23.5339999999999,10.7762590661863,-11.5703396029876));
#117596=CARTESIAN_POINT('Ctrl Pts',(23.5339999999999,10.7583140714215,-11.5711814532735));
#117597=CARTESIAN_POINT('Ctrl Pts',(23.534,10.621315610092,-11.5776084372518));
#117598=CARTESIAN_POINT('Ctrl Pts',(23.534,10.4843351016943,-11.5779507199327));
#117599=CARTESIAN_POINT('Ctrl Pts',(23.534,10.3477779769602,-11.5722201804618));
#117600=CARTESIAN_POINT('Ctrl Pts',(23.534,10.2117250436855,-11.566510799089));
#117601=CARTESIAN_POINT('Ctrl Pts',(23.5339999999999,10.0760915866747,-11.5547732226133));
#117602=CARTESIAN_POINT('Ctrl Pts',(23.534,9.94128731876771,-11.5369684475271));
#117603=CARTESIAN_POINT('Ctrl Pts',(23.534,9.80868446685906,-11.5194544326471));
#117604=CARTESIAN_POINT('Ctrl Pts',(23.5339999999999,9.67688326966917,-11.4960695457184));
#117605=CARTESIAN_POINT('Ctrl Pts',(23.534,9.54629292155958,-11.4667302088915));
#117606=CARTESIAN_POINT('Ctrl Pts',(23.534,9.5112464654664,-11.4588564280586));
#117607=CARTESIAN_POINT('Ctrl Pts',(23.534,9.47628735692625,-11.4505535423215));
#117608=CARTESIAN_POINT('Ctrl Pts',(23.534,9.44142384068047,-11.4418193834442));
#117609=CARTESIAN_POINT('Ctrl Pts',(23.534,9.35465567581842,-11.4200818475038));
#117610=CARTESIAN_POINT('Ctrl Pts',(23.534,9.26847914064438,-11.395673426388));
#117611=CARTESIAN_POINT('Ctrl Pts',(23.534,9.18301437324066,-11.3686311001959));
#117612=CARTESIAN_POINT('Ctrl Pts',(23.5339999999999,9.15095469784314,-11.3584869410757));
#117613=CARTESIAN_POINT('Ctrl Pts',(23.534,9.11899524917182,-11.347972079119));
#117614=CARTESIAN_POINT('Ctrl Pts',(23.534,9.08714263326125,-11.3370882239502));
#117615=CARTESIAN_POINT('Ctrl Pts',(23.534,9.06138445712602,-11.3282868037072));
#117616=CARTESIAN_POINT('Ctrl Pts',(23.534,9.03570611702107,-11.3192474074339));
#117617=CARTESIAN_POINT('Ctrl Pts',(23.534,9.01012249912345,-11.3099758408373));
#117618=CARTESIAN_POINT('Ctrl Pts',(23.534,8.8838168776646,-11.2642023702683));
#117619=CARTESIAN_POINT('Ctrl Pts',(23.534,8.75972821615212,-11.2127431096887));
#117620=CARTESIAN_POINT('Ctrl Pts',(23.534,8.63823633729656,-11.1557838964956));
#117621=CARTESIAN_POINT('Ctrl Pts',(23.534,8.51762503020503,-11.0992375230357));
#117622=CARTESIAN_POINT('Ctrl Pts',(23.534,8.39957237065447,-11.0372701273009));
#117623=CARTESIAN_POINT('Ctrl Pts',(23.534,8.28448331249122,-10.970024793541));
#117624=CARTESIAN_POINT('Ctrl Pts',(23.534,8.2674356587266,-10.9600640276305));
#117625=CARTESIAN_POINT('Ctrl Pts',(23.534,8.25045309991395,-10.9499873953753));
#117626=CARTESIAN_POINT('Ctrl Pts',(23.534,8.23353702790624,-10.939795299223));
#117627=CARTESIAN_POINT('Ctrl Pts',(23.534,8.20315452082413,-10.9214895463633));
#117628=CARTESIAN_POINT('Ctrl Pts',(23.534,8.17298647883074,-10.902811329405));
#117629=CARTESIAN_POINT('Ctrl Pts',(23.534,8.14304114129206,-10.8837628607093));
#117630=CARTESIAN_POINT('Ctrl Pts',(23.5339999999999,8.12583577094011,-10.8728183870288));
#117631=CARTESIAN_POINT('Ctrl Pts',(23.534,8.1087059434679,-10.8617529204478));
#117632=CARTESIAN_POINT('Ctrl Pts',(23.534,8.09166038518002,-10.8505717991687));
#117633=CARTESIAN_POINT('Ctrl Pts',(23.534,7.98236466033434,-10.778878708561));
#117634=CARTESIAN_POINT('Ctrl Pts',(23.534,7.87644328077352,-10.7023783007895));
#117635=CARTESIAN_POINT('Ctrl Pts',(23.5339999999999,7.77426954147455,-10.6212231772217));
#117636=CARTESIAN_POINT('Ctrl Pts',(23.5339999999999,7.70156836402741,-10.5634776833234));
#117637=CARTESIAN_POINT('Ctrl Pts',(23.534,7.63076526501317,-10.5033747155762));
#117638=CARTESIAN_POINT('Ctrl Pts',(23.534,7.56200744420826,-10.4409593356367));
#117639=CARTESIAN_POINT('Ctrl Pts',(23.534,7.48528237325109,-10.3713116301304));
#117640=CARTESIAN_POINT('Ctrl Pts',(23.534,7.41110370365363,-10.298784417752));
#117641=CARTESIAN_POINT('Ctrl Pts',(23.5339999999999,7.33961515870573,-10.2235362531339));
#117642=CARTESIAN_POINT('Ctrl Pts',(-17.1175857387455,20.5721719462546,
-0.00214206224876584));
#117643=CARTESIAN_POINT('Ctrl Pts',(-16.6641680440313,20.0337688721201,
-0.0445526553076215));
#117644=CARTESIAN_POINT('Ctrl Pts',(-16.3459143283547,18.477787514409,-0.129355183926955));
#117645=CARTESIAN_POINT('Ctrl Pts',(-18.0613963234494,16.802775720219,-0.256549648106768));
#117646=CARTESIAN_POINT('Ctrl Pts',(-20.3933471209293,17.343653714663,-0.383725454788201));
#117647=CARTESIAN_POINT('Ctrl Pts',(-21.203092243631,19.5945946034862,-0.510901261469636));
#117648=CARTESIAN_POINT('Ctrl Pts',(-19.7475288885744,21.4952120560344,
-0.638077068151069));
#117649=CARTESIAN_POINT('Ctrl Pts',(-17.3621513494713,21.2993774656764,
-0.765252874832505));
#117650=CARTESIAN_POINT('Ctrl Pts',(-16.2353413405934,19.188016346975,-0.892428681513937));
#117651=CARTESIAN_POINT('Ctrl Pts',(-17.4009051420832,17.0975180849442,
-1.01960448819538));
#117652=CARTESIAN_POINT('Ctrl Pts',(-19.7894957664261,16.9461241370553,
-1.14678029487681));
#117653=CARTESIAN_POINT('Ctrl Pts',(-21.2097371145961,18.8725531087288,
-1.27395610155824));
#117654=CARTESIAN_POINT('Ctrl Pts',(-20.358641983851,21.1095172903669,-1.40113190823968));
#117655=CARTESIAN_POINT('Ctrl Pts',(-18.0170393638344,21.6046935058561,
-1.52830771492111));
#117656=CARTESIAN_POINT('Ctrl Pts',(-16.333203267628,19.9038128993918,-1.65548352160254));
#117657=CARTESIAN_POINT('Ctrl Pts',(-16.8519493500829,17.5673150993311,
-1.78265932828398));
#117658=CARTESIAN_POINT('Ctrl Pts',(-19.0973599935785,16.7387984392048,
-1.90983513496541));
#117659=CARTESIAN_POINT('Ctrl Pts',(-21.0094104459781,18.1783720950554,
-2.03701094164685));
#117660=CARTESIAN_POINT('Ctrl Pts',(-20.8339130159653,20.5653183707664,
-2.16418674832828));
#117661=CARTESIAN_POINT('Ctrl Pts',(-18.7318757426636,21.7097612836464,
-2.29136255500972));
#117662=CARTESIAN_POINT('Ctrl Pts',(-16.6317873365857,20.561745973449,-2.41853836169115));
#117663=CARTESIAN_POINT('Ctrl Pts',(-16.4603485748086,18.1745049842297,
-2.54571416837258));
#117664=CARTESIAN_POINT('Ctrl Pts',(-18.3748438750272,16.7381838840222,
-2.67288997505402));
#117665=CARTESIAN_POINT('Ctrl Pts',(-20.6188426291484,17.5705180670209,
-2.80006578173545));
#117666=CARTESIAN_POINT('Ctrl Pts',(-21.1336152570428,19.9078926156331,
-2.92724158841689));
#117667=CARTESIAN_POINT('Ctrl Pts',(-19.4468898237851,21.6059114372621,
-3.05441739509832));
#117668=CARTESIAN_POINT('Ctrl Pts',(-17.1061322239997,21.1067476633747,
-3.18159320177976));
#117669=CARTESIAN_POINT('Ctrl Pts',(-16.2588422718968,18.8683530700484,
-3.30876900846119));
#117670=CARTESIAN_POINT('Ctrl Pts',(-17.6823559096772,16.9443157687486,
-3.43594481514263));
#117671=CARTESIAN_POINT('Ctrl Pts',(-20.0706877279544,17.0998205628843,
-3.56312062182406));
#117672=CARTESIAN_POINT('Ctrl Pts',(-21.2326915200203,19.1922014562322,
-3.6902964285055));
#117673=CARTESIAN_POINT('Ctrl Pts',(-20.102300928759,21.3018288465973,-3.81747223518693));
#117674=CARTESIAN_POINT('Ctrl Pts',(-17.7165791616921,21.4932505417456,
-3.94464804186836));
#117675=CARTESIAN_POINT('Ctrl Pts',(-16.264277865515,19.590849017254,-4.0718238485498));
#117676=CARTESIAN_POINT('Ctrl Pts',(-17.0777933394838,17.3399595955375,
-4.19899965523123));
#117677=CARTESIAN_POINT('Ctrl Pts',(-19.4107756286979,16.8056336150422,
-4.32617546191267));
#117678=CARTESIAN_POINT('Ctrl Pts',(-21.1228582840144,18.4780819988752,
-4.4533512685941));
#117679=CARTESIAN_POINT('Ctrl Pts',(-20.6433117330145,20.8229371587163,
-4.58052707527553));
#117680=CARTESIAN_POINT('Ctrl Pts',(-18.4120901722247,21.6889400235399,
-4.70770288195697));
#117681=CARTESIAN_POINT('Ctrl Pts',(-16.4762008984415,20.281586715068,-4.8348786886384));
#117682=CARTESIAN_POINT('Ctrl Pts',(-16.6117021655217,17.8920365436271,
-4.96205449531983));
#117683=CARTESIAN_POINT('Ctrl Pts',(-18.6942799710763,16.7125534793035,
-5.08923030200127));
#117684=CARTESIAN_POINT('Ctrl Pts',(-20.8132984378653,17.8252400266391,
-5.21640610868271));
#117685=CARTESIAN_POINT('Ctrl Pts',(-21.0246896437286,20.2092753395693,
-5.34358191536413));
#117686=CARTESIAN_POINT('Ctrl Pts',(-19.1345152777048,21.6774549884001,
-5.47075772204558));
#117687=CARTESIAN_POINT('Ctrl Pts',(-16.8768930031683,20.8828152708351,
-5.59793352872701));
#117688=CARTESIAN_POINT('Ctrl Pts',(-16.3230511331653,18.5543888068372,
-5.72510933540844));
#117689=CARTESIAN_POINT('Ctrl Pts',(-17.98110520812,16.8283623586792,-5.85228514208988));
#117690=CARTESIAN_POINT('Ctrl Pts',(-20.3298935247037,17.288258063263,-5.97946094877131));
#117691=CARTESIAN_POINT('Ctrl Pts',(-21.2145485846948,19.5121501559794,
-6.10663675545275));
#117692=CARTESIAN_POINT('Ctrl Pts',(-19.8234542784371,21.4597556720715,
-6.23381256213418));
#117693=CARTESIAN_POINT('Ctrl Pts',(-17.4328532908717,21.3442674325558,
-6.36098836881561));
#117694=CARTESIAN_POINT('Ctrl Pts',(-16.235973650659,19.2716387291798,-6.48816417549706));
#117695=CARTESIAN_POINT('Ctrl Pts',(-17.3308781409654,17.1433777554452,
-6.61533998217847));
#117696=CARTESIAN_POINT('Ctrl Pts',(-19.7130598493718,16.9120318599802,
-6.74251578885992));
#117697=CARTESIAN_POINT('Ctrl Pts',(-21.1970149132871,18.7898465429281,
-6.86969159554135));
#117698=CARTESIAN_POINT('Ctrl Pts',(-20.4213066662076,21.054043383008,-6.99686740222279));
#117699=CARTESIAN_POINT('Ctrl Pts',(-18.0975992789452,21.6273623113514,
-7.12404320890422));
#117700=CARTESIAN_POINT('Ctrl Pts',(-16.3577500537671,19.9838187953891,
-7.25121901558565));
#117701=CARTESIAN_POINT('Ctrl Pts',(-16.7979626675525,17.6312620012014,
-7.37839482226709));
#117702=CARTESIAN_POINT('Ctrl Pts',(-19.0143693698296,16.7280167713133,
-7.50557062894852));
#117703=CARTESIAN_POINT('Ctrl Pts',(-20.9735545769736,18.1027545424254,
-7.63274643562996));
#117704=CARTESIAN_POINT('Ctrl Pts',(-20.8780874621779,20.4942387353917,
-7.75992224231139));
#117705=CARTESIAN_POINT('Ctrl Pts',(-18.8155531779101,21.7084310354144,
-7.88709804899282));
#117706=CARTESIAN_POINT('Ctrl Pts',(-16.6781989146708,20.6313853684961,
-8.01427385567426));
#117707=CARTESIAN_POINT('Ctrl Pts',(-16.4269145498154,18.2512242850411,
-8.1414496623557));
#117708=CARTESIAN_POINT('Ctrl Pts',(-18.2922378916319,16.7515978496617,
-8.26862546903713));
#117709=CARTESIAN_POINT('Ctrl Pts',(-20.5628505490274,17.5083202395048,
-8.39580127571856));
#117710=CARTESIAN_POINT('Ctrl Pts',(-21.155606338957,19.8271456293778,-8.5229770824));
#117711=CARTESIAN_POINT('Ctrl Pts',(-19.5266886147337,21.5806956466073,
-8.65015288908143));
#117712=CARTESIAN_POINT('Ctrl Pts',(-17.1705282862964,21.160196987974,-8.77732869576286));
#117713=CARTESIAN_POINT('Ctrl Pts',(-16.2487562151834,18.9514310736836,
-8.9045045024443));
#117714=CARTESIAN_POINT('Ctrl Pts',(-17.6070410650139,16.9808035386242,
-9.03168030912573));
#117715=CARTESIAN_POINT('Ctrl Pts',(-19.9992407907343,17.0562428352734,
-9.15885611580717));
#117716=CARTESIAN_POINT('Ctrl Pts',(-21.2306606206557,19.1085380912468,
-9.2860319224886));
#117717=CARTESIAN_POINT('Ctrl Pts',(-20.1715492913599,21.2548357889979,
-9.41320772917003));
#117718=CARTESIAN_POINT('Ctrl Pts',(-17.7935757116131,21.5260410050991,
-9.54038353585147));
#117719=CARTESIAN_POINT('Ctrl Pts',(-16.278383047147,19.6733397866716,-9.66755934253291));
#117720=CARTESIAN_POINT('Ctrl Pts',(-17.0160665241465,17.3964705100163,
-9.79473514921434));
#117721=CARTESIAN_POINT('Ctrl Pts',(-19.3298473382647,16.7843194180195,
-9.92191095589577));
#117722=CARTESIAN_POINT('Ctrl Pts',(-21.0969752019817,18.3984971432064,
-10.0490867625772));
#117723=CARTESIAN_POINT('Ctrl Pts',(-20.696219980662,20.7580958098868,-10.1762625692586));
#117724=CARTESIAN_POINT('Ctrl Pts',(-18.4952497161921,21.6983300945914,
-10.3034383759401));
#117725=CARTESIAN_POINT('Ctrl Pts',(-16.5133180186021,20.356593398625,-10.4306141826215));
#117726=CARTESIAN_POINT('Ctrl Pts',(-16.5687242078764,17.9638458629654,
-10.5577899893029));
#117727=CARTESIAN_POINT('Ctrl Pts',(-18.6106365442519,16.7152848409195,
-10.6849657959844));
#117728=CARTESIAN_POINT('Ctrl Pts',(-20.7657271944765,17.7563875757774,
-10.8121416026658));
#117729=CARTESIAN_POINT('Ctrl Pts',(-21.0568342469805,20.1320069264304,
-10.9393174093472));
#117730=CARTESIAN_POINT('Ctrl Pts',(-19.2168850492326,21.6626595862203,
-11.0664932160287));
#117731=CARTESIAN_POINT('Ctrl Pts',(-16.93391879004,20.9440667428082,-11.1936690227101));
#117732=CARTESIAN_POINT('Ctrl Pts',(-16.3024153153455,18.6354927291228,
-11.3208448293915));
#117733=CARTESIAN_POINT('Ctrl Pts',(-17.9017398676552,16.8549109164576,
-11.448020636073));
#117734=CARTESIAN_POINT('Ctrl Pts',(-20.2646114355015,17.2358946025617,
-11.5751964427544));
#117735=CARTESIAN_POINT('Ctrl Pts',(-21.2232420117351,19.428914901949,-11.7023722494359));
#117736=CARTESIAN_POINT('Ctrl Pts',(-19.8981475419851,21.4220118041223,
-11.8295480561173));
#117737=CARTESIAN_POINT('Ctrl Pts',(-17.5050199576091,21.3866426068827,
-11.9567238627987));
#117738=CARTESIAN_POINT('Ctrl Pts',(-16.2394052830226,19.3552563534375,
-12.0838996694802));
#117739=CARTESIAN_POINT('Ctrl Pts',(-17.2624264292529,17.1915238492725,
-12.2110754761616));
#117740=CARTESIAN_POINT('Ctrl Pts',(-19.635524990487,16.880535370574,-12.338251282843));
#117741=CARTESIAN_POINT('Ctrl Pts',(-21.1815303279007,18.707603544426,-12.4654270895244));
#117742=CARTESIAN_POINT('Ctrl Pts',(-20.48207850033,20.9965067219594,-12.5926028962059));
#117743=CARTESIAN_POINT('Ctrl Pts',(-18.1788731466945,21.6473183031405,
-12.7197787028873));
#117744=CARTESIAN_POINT('Ctrl Pts',(-16.3849622259084,20.0629590561579,
-12.8469545095688));
#117745=CARTESIAN_POINT('Ctrl Pts',(-16.7461476651242,17.6969802536931,
-12.9741303162502));
#117746=CARTESIAN_POINT('Ctrl Pts',(-18.9310642415578,16.7200205978014,
-13.1013061229316));
#117747=CARTESIAN_POINT('Ctrl Pts',(-20.9351866075484,18.0283799358088,
-13.2284819296131));
#117748=CARTESIAN_POINT('Ctrl Pts',(-20.9198568821621,20.4217197810322,
-13.3556577362945));
#117749=CARTESIAN_POINT('Ctrl Pts',(-18.8991391369708,21.7042993729031,
-13.4828335429759));
#117750=CARTESIAN_POINT('Ctrl Pts',(-16.7269164832995,20.6994315417472,
-13.6100093496574));
#117751=CARTESIAN_POINT('Ctrl Pts',(-16.3960683825486,18.3290201535185,
-13.7371851563388));
#117752=CARTESIAN_POINT('Ctrl Pts',(-18.2101274324079,16.7677705325936,
-13.8643609630202));
#117753=CARTESIAN_POINT('Ctrl Pts',(-20.5048070478343,17.4480323040911,
-13.9915367697017));
#117754=CARTESIAN_POINT('Ctrl Pts',(-21.1748811055536,19.7457075144692,
-14.1187125763831));
#117755=CARTESIAN_POINT('Ctrl Pts',(-19.6055982470946,21.5528217680131,
-14.2458883830645));
#117756=CARTESIAN_POINT('Ctrl Pts',(-17.2366780944146,21.2114598992563,
-14.373064189746));
#117757=CARTESIAN_POINT('Ctrl Pts',(-16.2414578558307,19.0348002354761,
-14.5002399964274));
#117758=CARTESIAN_POINT('Ctrl Pts',(-17.5329903299092,17.0197929194559,
-14.6274158031088));
#117759=CARTESIAN_POINT('Ctrl Pts',(-19.926374633229,17.0150820981853,-14.7545916097903));
#117760=CARTESIAN_POINT('Ctrl Pts',(-21.2258292176773,19.0249896577937,
-14.8817674164717));
#117761=CARTESIAN_POINT('Ctrl Pts',(-20.2391851552704,21.2055501612724,
-15.0089432231531));
#117762=CARTESIAN_POINT('Ctrl Pts',(-17.8716271352296,21.5562346875283,
-15.1361190298346));
#117763=CARTESIAN_POINT('Ctrl Pts',(-16.2952426937192,19.7553119496581,
-15.263294836516));
#117764=CARTESIAN_POINT('Ctrl Pts',(-16.956266714372,17.4550167817861,-15.3904706431974));
#117765=CARTESIAN_POINT('Ctrl Pts',(-19.2482506860169,16.7657272280153,
-15.5176464498789));
#117766=CARTESIAN_POINT('Ctrl Pts',(-21.0684415712385,18.3198236717957,
-15.6448222565603));
#117767=CARTESIAN_POINT('Ctrl Pts',(-20.7469272066334,20.6915190840625,
-15.7719980632418));
#117768=CARTESIAN_POINT('Ctrl Pts',(-18.5786770662948,21.7049301280797,
-15.8991738699232));
#117769=CARTESIAN_POINT('Ctrl Pts',(-16.5529260772022,20.4303150703446,
-16.0263496766046));
#117770=CARTESIAN_POINT('Ctrl Pts',(-16.5281750395616,18.0370541147968,
-16.153525483286));
#117771=CARTESIAN_POINT('Ctrl Pts',(-18.5271314941858,16.7208156456237,
-16.2807012899675));
#117772=CARTESIAN_POINT('Ctrl Pts',(-20.7158769631869,17.689166763319,-16.4078770966489));
#117773=CARTESIAN_POINT('Ctrl Pts',(-21.0863733276212,20.0537054200458,
-16.5350529033304));
#117774=CARTESIAN_POINT('Ctrl Pts',(-19.2987131687179,21.6451141580778,
-16.6622287100118));
#117775=CARTESIAN_POINT('Ctrl Pts',(-16.9929637275681,21.0033742342365,
-16.7894045166932));
#117776=CARTESIAN_POINT('Ctrl Pts',(-16.2845070054764,18.7172421977746,
-16.9165803233747));
#117777=CARTESIAN_POINT('Ctrl Pts',(-17.8233080731787,16.884102298789,-17.0437561300561));
#117778=CARTESIAN_POINT('Ctrl Pts',(-20.1976124598239,17.1857466171053,
-17.1709319367376));
#117779=CARTESIAN_POINT('Ctrl Pts',(-21.2291432566148,19.3454352128261,
-17.2981077434189));
#117780=CARTESIAN_POINT('Ctrl Pts',(-19.9715349815179,21.3817878447692,
-17.4252835501004));
#117781=CARTESIAN_POINT('Ctrl Pts',(-17.5785651709616,21.4265773634257,
-17.5524593567818));
#117782=CARTESIAN_POINT('Ctrl Pts',(-16.245635101675,19.4387121653785,-17.6796351634633));
#117783=CARTESIAN_POINT('Ctrl Pts',(-17.195625381257,17.2419351890085,-17.8068109701447));
#117784=CARTESIAN_POINT('Ctrl Pts',(-19.5569788912398,16.8516529627759,
-17.9339867768261));
#117785=CARTESIAN_POINT('Ctrl Pts',(-21.1633003483382,18.6259252056079,
-18.0611625835076));
#117786=CARTESIAN_POINT('Ctrl Pts',(-20.5408895152254,20.9369672584502,
-18.188338390189));
#117787=CARTESIAN_POINT('Ctrl Pts',(-18.2607697000954,21.6645414772881,
-18.3155141968704));
#117788=CARTESIAN_POINT('Ctrl Pts',(-16.4148093131604,20.1411436746453,
-18.4426900035519));
#117789=CARTESIAN_POINT('Ctrl Pts',(-16.696562436159,17.7643967817956,-18.5698658102333));
#117790=CARTESIAN_POINT('Ctrl Pts',(-18.8475380664095,16.7148185552248,
-18.6970416169147));
#117791=CARTESIAN_POINT('Ctrl Pts',(-20.8943495675715,17.955331873938,-18.8242174235962));
#117792=CARTESIAN_POINT('Ctrl Pts',(-20.9591744271437,20.3478427623818,
-18.9513932302776));
#117793=CARTESIAN_POINT('Ctrl Pts',(-18.9825398592484,21.6973709774882,
-19.078569036959));
#117794=CARTESIAN_POINT('Ctrl Pts',(-16.77788539751,20.7658081409326,-19.2057448436405));
#117795=CARTESIAN_POINT('Ctrl Pts',(-16.3678446716688,18.4078053400529,
-19.3329206503219));
#117796=CARTESIAN_POINT('Ctrl Pts',(-18.1286046027284,16.7866837825795,
-19.4600964570034));
#117797=CARTESIAN_POINT('Ctrl Pts',(-20.4447772293123,17.3897218945994,
-19.5872722636848));
#117798=CARTESIAN_POINT('Ctrl Pts',(-21.1914179431377,19.6636696077008,
-19.7144480703662));
#117799=CARTESIAN_POINT('Ctrl Pts',(-19.683530194942,21.5223210888799,-19.8416238770476));
#117800=CARTESIAN_POINT('Ctrl Pts',(-17.3045074731465,21.2604788559019,
-19.9687996837291));
#117801=CARTESIAN_POINT('Ctrl Pts',(-16.2369553322288,19.118367116143,-20.0959754904105));
#117802=CARTESIAN_POINT('Ctrl Pts',(-17.4602868598787,17.0612400309757,
-20.223151297092));
#117803=CARTESIAN_POINT('Ctrl Pts',(-19.8521708105233,16.9763848025611,
-20.3503271037734));
#117804=CARTESIAN_POINT('Ctrl Pts',(-21.2182030751438,18.9416493308234,
-20.4775029104549));
#117805=CARTESIAN_POINT('Ctrl Pts',(-20.305131989166,21.154028290157,-20.6046787171362));
#117806=CARTESIAN_POINT('Ctrl Pts',(-17.9506471621875,21.5837957108187,
-20.7318545238177));
#117807=CARTESIAN_POINT('Ctrl Pts',(-16.3148354273652,19.8366774312875,
-20.8590303304991));
#117808=CARTESIAN_POINT('Ctrl Pts',(-16.8984657403956,17.5155252757358,
-20.9862061371806));
#117809=CARTESIAN_POINT('Ctrl Pts',(-19.1660680401668,16.7498922826988,
-21.113381943862));
#117810=CARTESIAN_POINT('Ctrl Pts',(-21.0373070469929,18.2421221167019,
-21.2405577505435));
#117811=CARTESIAN_POINT('Ctrl Pts',(-20.7953425225475,20.6233350697589,
-21.3677335572248));
#117812=CARTESIAN_POINT('Ctrl Pts',(-18.6623441810672,21.7086297969706,
-21.4949093639063));
#117813=CARTESIAN_POINT('Ctrl Pts',(-16.5948543422637,20.502867400276,-21.6220851705877));
#117814=CARTESIAN_POINT('Ctrl Pts',(-16.4903436183303,18.1111966683195,
-21.7492609772692));
#117815=CARTESIAN_POINT('Ctrl Pts',(-18.4433885098623,16.7298792897364,
-21.8764367839506));
#117816=CARTESIAN_POINT('Ctrl Pts',(-20.6647168984764,17.6222041838633,
-22.003612590632));
#117817=CARTESIAN_POINT('Ctrl Pts',(-21.1114420608105,19.9774734447106,
-22.1307883973135));
#117818=CARTESIAN_POINT('Ctrl Pts',(-19.9599075668543,21.0705044715179,
-22.2155722684344));
#117819=CARTESIAN_POINT('Ctrl Pts',(-19.2802415985968,21.2523731445725,
-22.2579642039949));
#117820=CARTESIAN_POINT('Ctrl Pts',(-17.0028273852109,20.6688092100886,
0.0844763361257092));
#117821=CARTESIAN_POINT('Ctrl Pts',(-16.5172190142843,20.092181868941,0.0420657430668536));
#117822=CARTESIAN_POINT('Ctrl Pts',(-16.1763706746349,18.4257326299315,
-0.0427367855524801));
#117823=CARTESIAN_POINT('Ctrl Pts',(-18.01364439973,16.6318023132686,-0.169931249732292));
#117824=CARTESIAN_POINT('Ctrl Pts',(-20.5111535200096,17.2110802832593,
-0.297107056413726));
#117825=CARTESIAN_POINT('Ctrl Pts',(-21.3783870101994,19.6218281451444,
-0.424282863095161));
#117826=CARTESIAN_POINT('Ctrl Pts',(-19.8194850134989,21.6573811366705,
-0.551458669776596));
#117827=CARTESIAN_POINT('Ctrl Pts',(-17.2647560862599,21.4476431456228,
-0.678634476458029));
#117828=CARTESIAN_POINT('Ctrl Pts',(-16.057947487624,19.1863846079818,-0.805810283139464));
#117829=CARTESIAN_POINT('Ctrl Pts',(-17.3062612289062,16.947470098725,-0.932986089820897));
#117830=CARTESIAN_POINT('Ctrl Pts',(-19.8644313564054,16.7853278416859,
-1.06016189650233));
#117831=CARTESIAN_POINT('Ctrl Pts',(-21.3855036379843,18.848524857474,-1.18733770318377));
#117832=CARTESIAN_POINT('Ctrl Pts',(-20.4739844697589,21.2443037270014,
-1.3145135098652));
#117833=CARTESIAN_POINT('Ctrl Pts',(-17.9661382896929,21.774635291315,-1.44168931654664));
#117834=CARTESIAN_POINT('Ctrl Pts',(-16.1627571841069,19.9529995896776,
-1.56886512322807));
#117835=CARTESIAN_POINT('Ctrl Pts',(-16.7183319730092,17.4506206494911,
-1.69604092990951));
#117836=CARTESIAN_POINT('Ctrl Pts',(-19.1231569662995,16.5632829246964,
-1.82321673659094));
#117837=CARTESIAN_POINT('Ctrl Pts',(-21.1709546507375,18.1050600233756,
-1.95039254327237));
#117838=CARTESIAN_POINT('Ctrl Pts',(-20.9829976696055,20.6614690606707,
-2.07756834995381));
#117839=CARTESIAN_POINT('Ctrl Pts',(-18.7317249296694,21.8871624224887,
-2.20474415663524));
#117840=CARTESIAN_POINT('Ctrl Pts',(-16.4825394180193,20.6576430387449,
-2.33191996331668));
#117841=CARTESIAN_POINT('Ctrl Pts',(-16.2989292528432,18.1009183645693,
-2.45909576999811));
#117842=CARTESIAN_POINT('Ctrl Pts',(-18.3493453586185,16.5626247387795,
-2.58627157667954));
#117843=CARTESIAN_POINT('Ctrl Pts',(-20.7526582245547,17.4540510138992,
-2.71344738336098));
#117844=CARTESIAN_POINT('Ctrl Pts',(-21.3039774609752,19.9573689479556,
-2.84062319004241));
#117845=CARTESIAN_POINT('Ctrl Pts',(-19.4975018880252,21.7759396905319,
-2.96779899672385));
#117846=CARTESIAN_POINT('Ctrl Pts',(-16.9905607209365,21.2413374685879,
-3.09497480340528));
#117847=CARTESIAN_POINT('Ctrl Pts',(-16.0831168824194,18.8440266343892,
-3.22215061008672));
#117848=CARTESIAN_POINT('Ctrl Pts',(-17.6076937718807,16.7833910871266,
-3.34932641676815));
#117849=CARTESIAN_POINT('Ctrl Pts',(-20.1655867192137,16.9499360425438,
-3.47650222344959));
#117850=CARTESIAN_POINT('Ctrl Pts',(-21.4100877059499,19.1908668417195,
-3.60367803013102));
#117851=CARTESIAN_POINT('Ctrl Pts',(-20.1994443192179,21.4502685638837,
-3.73085383681246));
#117852=CARTESIAN_POINT('Ctrl Pts',(-17.6443467253329,21.6552803634332,
-3.85802964349388));
#117853=CARTESIAN_POINT('Ctrl Pts',(-16.0889383794468,19.6178166386469,
-3.98520545017533));
#117854=CARTESIAN_POINT('Ctrl Pts',(-16.9602098993781,17.2071238978084,
-4.11238125685675));
#117855=CARTESIAN_POINT('Ctrl Pts',(-19.4588237428005,16.6348631061435,
-4.23955706353819));
#117856=CARTESIAN_POINT('Ctrl Pts',(-21.2924567898383,18.4260480215086,
-4.36673287021963));
#117857=CARTESIAN_POINT('Ctrl Pts',(-20.7788645279368,20.9373776575228,
-4.49390867690106));
#117858=CARTESIAN_POINT('Ctrl Pts',(-18.3892359802594,21.8648629438428,
-4.62108448358249));
#117859=CARTESIAN_POINT('Ctrl Pts',(-16.3159070222257,20.3575936964975,
-4.74826029026393));
#117860=CARTESIAN_POINT('Ctrl Pts',(-16.4610282875234,17.7983958982468,
-4.87543609694536));
#117861=CARTESIAN_POINT('Ctrl Pts',(-18.6914600224833,16.535174687256,-5.0026119036268));
#117862=CARTESIAN_POINT('Ctrl Pts',(-20.9609195464861,17.7268571202586,
-5.12978771030823));
#117863=CARTESIAN_POINT('Ctrl Pts',(-21.1873186048029,20.280148529128,-5.25696351698966));
#117864=CARTESIAN_POINT('Ctrl Pts',(-19.1629501133386,21.8525625213641,
-5.38413932367111));
#117865=CARTESIAN_POINT('Ctrl Pts',(-16.7450465165327,21.0015068541093,
-5.51131513035253));
#117866=CARTESIAN_POINT('Ctrl Pts',(-16.1518842924324,18.5077722795978,
-5.63849093703398));
#117867=CARTESIAN_POINT('Ctrl Pts',(-17.9276529658501,16.6592054913206,
-5.7656667437154));
#117868=CARTESIAN_POINT('Ctrl Pts',(-20.4431949955591,17.1517517825272,
-5.89284255039684));
#117869=CARTESIAN_POINT('Ctrl Pts',(-21.390656701448,19.5335305019064,-6.02001835707826));
#117870=CARTESIAN_POINT('Ctrl Pts',(-19.9008007744696,21.6194075042871,
-6.14719416375971));
#117871=CARTESIAN_POINT('Ctrl Pts',(-17.3404775567387,21.4957201041125,
-6.27436997044113));
#117872=CARTESIAN_POINT('Ctrl Pts',(-16.0586246889428,19.2759438141371,
-6.40154577712258));
#117873=CARTESIAN_POINT('Ctrl Pts',(-17.2312626165228,16.9965856055586,
-6.528721583804));
#117874=CARTESIAN_POINT('Ctrl Pts',(-19.7825688230421,16.7488151618222,
-6.65589739048545));
#117875=CARTESIAN_POINT('Ctrl Pts',(-21.3718782159412,18.7599464866879,
-6.78307319716687));
#117876=CARTESIAN_POINT('Ctrl Pts',(-20.5410980709011,21.1848914144791,
-6.91024900384832));
#117877=CARTESIAN_POINT('Ctrl Pts',(-18.0524176069647,21.7989134830039,
-7.03742481052974));
#117878=CARTESIAN_POINT('Ctrl Pts',(-16.189046684864,20.0386855548983,-7.16460061721119));
#117879=CARTESIAN_POINT('Ctrl Pts',(-16.6605124717835,17.5191075021328,
-7.2917764238926));
#117880=CARTESIAN_POINT('Ctrl Pts',(-19.0342743706914,16.551735805469,-7.41895223057406));
#117881=CARTESIAN_POINT('Ctrl Pts',(-21.1325531716193,18.024073954737,-7.54612803725548));
#117882=CARTESIAN_POINT('Ctrl Pts',(-21.0303083085858,20.5853430815951,
-7.67330384393691));
#117883=CARTESIAN_POINT('Ctrl Pts',(-18.8213430973923,21.8857377324416,
-7.80047965061835));
#117884=CARTESIAN_POINT('Ctrl Pts',(-16.5322460154652,20.7322265267193,
-7.92765545729978));
#117885=CARTESIAN_POINT('Ctrl Pts',(-16.2631215580847,18.1830844006987,
-8.05483126398122));
#117886=CARTESIAN_POINT('Ctrl Pts',(-18.2608747111494,16.5769910373997,
-8.18200707066265));
#117887=CARTESIAN_POINT('Ctrl Pts',(-20.6926909512673,17.3874374122526,
-8.30918287734408));
#117888=CARTESIAN_POINT('Ctrl Pts',(-21.3275298136684,19.8708892783049,
-8.43635868402552));
#117889=CARTESIAN_POINT('Ctrl Pts',(-19.5829660446433,21.7489336888602,
-8.56353449070696));
#117890=CARTESIAN_POINT('Ctrl Pts',(-17.0595286224332,21.2985814618163,
-8.69071029738838));
#117891=CARTESIAN_POINT('Ctrl Pts',(-16.0723147597259,18.9330028134741,
-8.81788610406983));
#117892=CARTESIAN_POINT('Ctrl Pts',(-17.5270319021526,16.8224693293182,
-8.94506191075126));
#117893=CARTESIAN_POINT('Ctrl Pts',(-20.0890673614655,16.90326448658,-9.07223771743269));
#117894=CARTESIAN_POINT('Ctrl Pts',(-21.4079126215994,19.1012637431849,
-9.19941352411413));
#117895=CARTESIAN_POINT('Ctrl Pts',(-20.2736090131502,21.3999392044174,
-9.32658933079555));
#117896=CARTESIAN_POINT('Ctrl Pts',(-17.726809694048,21.6903988064862,-9.453765137477));
#117897=CARTESIAN_POINT('Ctrl Pts',(-16.1040449673761,19.7061638924493,
-9.58094094415843));
#117898=CARTESIAN_POINT('Ctrl Pts',(-16.894100749718,17.2676468404274,-9.70811675083986));
#117899=CARTESIAN_POINT('Ctrl Pts',(-19.3721498971671,16.6120356942131,
-9.83529255752129));
#117900=CARTESIAN_POINT('Ctrl Pts',(-21.2647361220149,18.3408129886411,
-9.96246836420274));
#117901=CARTESIAN_POINT('Ctrl Pts',(-20.8355290301125,20.8679328560937,
-10.0896441708842));
#117902=CARTESIAN_POINT('Ctrl Pts',(-18.4782994886839,21.8749196689318,
-10.2168199775656));
#117903=CARTESIAN_POINT('Ctrl Pts',(-16.3556592958241,20.4379255270265,
-10.3439957842471));
#117904=CARTESIAN_POINT('Ctrl Pts',(-16.4149990825736,17.875303365661,-10.4711715909285));
#117905=CARTESIAN_POINT('Ctrl Pts',(-18.6018782776321,16.5380999636187,
-10.59834739761));
#117906=CARTESIAN_POINT('Ctrl Pts',(-20.9099709525642,17.65311644607,-10.7255232042914));
#117907=CARTESIAN_POINT('Ctrl Pts',(-21.2217453345073,20.1973943960938,
-10.8526990109728));
#117908=CARTESIAN_POINT('Ctrl Pts',(-19.2511677789294,21.8367167102424,
-10.9798748176543));
#117909=CARTESIAN_POINT('Ctrl Pts',(-16.806120885236,21.0671069131022,-11.1070506243357));
#117910=CARTESIAN_POINT('Ctrl Pts',(-16.1297834216659,18.5946342261783,
-11.2342264310171));
#117911=CARTESIAN_POINT('Ctrl Pts',(-17.8426530328072,16.6876388807614,
-11.3614022376985));
#117912=CARTESIAN_POINT('Ctrl Pts',(-20.3732781631159,17.0956707447917,
-11.48857804438));
#117913=CARTESIAN_POINT('Ctrl Pts',(-21.3999673238431,19.4443859083351,
-11.6157538510614));
#117914=CARTESIAN_POINT('Ctrl Pts',(-19.9807969335377,21.5789839865442,
-11.7429296577429));
#117915=CARTESIAN_POINT('Ctrl Pts',(-17.4177677416566,21.5411037307608,
-11.8701054644243));
#117916=CARTESIAN_POINT('Ctrl Pts',(-16.062299952218,19.3654979245523,-11.9972812711057));
#117917=CARTESIAN_POINT('Ctrl Pts',(-17.157951132213,17.0481498617898,-12.1244570777871));
#117918=CARTESIAN_POINT('Ctrl Pts',(-19.6995293277776,16.7150825592159,
-12.2516328844686));
#117919=CARTESIAN_POINT('Ctrl Pts',(-21.3552942926149,18.671864594454,-12.37880869115));
#117920=CARTESIAN_POINT('Ctrl Pts',(-20.6061844398505,21.1232699017635,
-12.5059844978315));
#117921=CARTESIAN_POINT('Ctrl Pts',(-18.1394615643946,21.8202862630607,
-12.6331603045129));
#117922=CARTESIAN_POINT('Ctrl Pts',(-16.2181908023896,20.1234444285697,
-12.7603361111943));
#117923=CARTESIAN_POINT('Ctrl Pts',(-16.605018830463,17.5894914635544,-12.8875119178758));
#117924=CARTESIAN_POINT('Ctrl Pts',(-18.9450549421127,16.5431719385577,
-13.0146877245572));
#117925=CARTESIAN_POINT('Ctrl Pts',(-21.091461243921,17.9444190758505,-13.1418635312386));
#117926=CARTESIAN_POINT('Ctrl Pts',(-21.0750431749784,20.5076755981723,
-13.2690393379201));
#117927=CARTESIAN_POINT('Ctrl Pts',(-18.9108632945195,21.8813127399352,
-13.3962151446015));
#117928=CARTESIAN_POINT('Ctrl Pts',(-16.5844223187131,20.8051036811079,
-13.5233909512829));
#117929=CARTESIAN_POINT('Ctrl Pts',(-16.2300854476496,18.2664034360971,
-13.6505667579644));
#117930=CARTESIAN_POINT('Ctrl Pts',(-18.1729347679036,16.5943119101923,
-13.7777425646458));
#117931=CARTESIAN_POINT('Ctrl Pts',(-20.6305266149702,17.3228692967068,
-13.9049183713272));
#117932=CARTESIAN_POINT('Ctrl Pts',(-21.3481730045189,19.7836694128848,
-14.0320941780087));
#117933=CARTESIAN_POINT('Ctrl Pts',(-19.6674779162968,21.7190808866133,
-14.1592699846901));
#117934=CARTESIAN_POINT('Ctrl Pts',(-17.1303747780463,21.3534838159302,
-14.2864457913715));
#117935=CARTESIAN_POINT('Ctrl Pts',(-16.0644982487317,19.0222908216738,
-14.413621598053));
#117936=CARTESIAN_POINT('Ctrl Pts',(-17.447723888241,16.8642267859192,-14.5407974047344));
#117937=CARTESIAN_POINT('Ctrl Pts',(-20.0110280249899,16.859181516911,-14.6679732114158));
#117938=CARTESIAN_POINT('Ctrl Pts',(-21.4027382101088,19.0117837358195,
-14.7951490180973));
#117939=CARTESIAN_POINT('Ctrl Pts',(-20.3460467280269,21.3471545123578,
-14.9223248247787));
#117940=CARTESIAN_POINT('Ctrl Pts',(-17.8104024278843,21.7227361085096,
-15.0495006314601));
#117941=CARTESIAN_POINT('Ctrl Pts',(-16.1221015752275,19.7939557210286,
-15.1766764381416));
#117942=CARTESIAN_POINT('Ctrl Pts',(-16.8300554146003,17.3303496418165,
-15.303852244823));
#117943=CARTESIAN_POINT('Ctrl Pts',(-19.284760238949,16.5921235399122,-15.4310280515045));
#117944=CARTESIAN_POINT('Ctrl Pts',(-21.2341767280976,18.2565540443337,
-15.5582038581859));
#117945=CARTESIAN_POINT('Ctrl Pts',(-20.8898362476853,20.7966294734819,
-15.6853796648673));
#117946=CARTESIAN_POINT('Ctrl Pts',(-18.5676498163098,21.8819882759749,
-15.8125554715487));
#117947=CARTESIAN_POINT('Ctrl Pts',(-16.3980793536131,20.5168811154897,
-15.9397312782302));
#117948=CARTESIAN_POINT('Ctrl Pts',(-16.3715711003901,17.9537090836658,
-16.0669070849116));
#117949=CARTESIAN_POINT('Ctrl Pts',(-18.5124447336848,16.5440234313033,
-16.1940828915931));
#117950=CARTESIAN_POINT('Ctrl Pts',(-20.8565815725531,17.5811232494858,
-16.3212586982745));
#117951=CARTESIAN_POINT('Ctrl Pts',(-21.253381560874,20.1135338247049,-16.4484345049559));
#117952=CARTESIAN_POINT('Ctrl Pts',(-19.338805337548,21.8179256333241,-16.5756103116374));
#117953=CARTESIAN_POINT('Ctrl Pts',(-16.8693577554744,21.1306249774212,
-16.7027861183188));
#117954=CARTESIAN_POINT('Ctrl Pts',(-16.1106037000031,18.6821875500976,
-16.8299619250002));
#117955=CARTESIAN_POINT('Ctrl Pts',(-17.7586529234411,16.7189027237572,
-16.9571377316817));
#117956=CARTESIAN_POINT('Ctrl Pts',(-20.3015225527551,17.0419624713682,
-17.0843135383631));
#117957=CARTESIAN_POINT('Ctrl Pts',(-21.4062875313382,19.354979525847,-17.2114893450445));
#117958=CARTESIAN_POINT('Ctrl Pts',(-20.0593945607884,21.5359043017382,
-17.338665151726));
#117959=CARTESIAN_POINT('Ctrl Pts',(-17.4965343439791,21.5838736806199,
-17.4658409584074));
#117960=CARTESIAN_POINT('Ctrl Pts',(-16.0689720607886,19.4548787346826,
-17.5930167650888));
#117961=CARTESIAN_POINT('Ctrl Pts',(-17.0864075015351,17.1021401864965,
-17.7201925717703));
#117962=CARTESIAN_POINT('Ctrl Pts',(-19.6154067985012,16.684149626596,-17.8473683784517));
#117963=CARTESIAN_POINT('Ctrl Pts',(-21.3357700641153,18.584387450276,-17.9745441851331));
#117964=CARTESIAN_POINT('Ctrl Pts',(-20.6691707799709,21.0595033963588,
-18.1017199918146));
#117965=CARTESIAN_POINT('Ctrl Pts',(-18.2271724154379,21.8387322073577,
-18.228895798496));
#117966=CARTESIAN_POINT('Ctrl Pts',(-16.2501569024917,20.207179813531,-18.3560716051774));
#117967=CARTESIAN_POINT('Ctrl Pts',(-16.5519132667841,17.6616942707386,
-18.4832474118589));
#117968=CARTESIAN_POINT('Ctrl Pts',(-18.8555987732945,16.537600573676,-18.6104232185403));
#117969=CARTESIAN_POINT('Ctrl Pts',(-21.0477249524445,17.8661849205939,
-18.7375990252217));
#117970=CARTESIAN_POINT('Ctrl Pts',(-21.1171520939507,20.4285536338248,
-18.8647748319032));
#117971=CARTESIAN_POINT('Ctrl Pts',(-19.0001851038609,21.8738924587027,
-18.9919506385846));
#117972=CARTESIAN_POINT('Ctrl Pts',(-16.639009803247,20.8761927289634,-19.119126445266));
#117973=CARTESIAN_POINT('Ctrl Pts',(-16.1998579765528,18.3507820268139,
-19.2463022519475));
#117974=CARTESIAN_POINT('Ctrl Pts',(-18.0856241733337,16.6145679183314,
-19.3734780586289));
#117975=CARTESIAN_POINT('Ctrl Pts',(-20.5662349414884,17.2604191027876,
-19.5006538653103));
#117976=CARTESIAN_POINT('Ctrl Pts',(-21.3658838853536,19.695807173002,-19.6278296719918));
#117977=CARTESIAN_POINT('Ctrl Pts',(-19.7509426921062,21.6864147924606,
-19.7550054786732));
#117978=CARTESIAN_POINT('Ctrl Pts',(-17.2030197464517,21.4059829044279,
-19.8821812853547));
#117979=CARTESIAN_POINT('Ctrl Pts',(-16.059676065617,19.1117905859247,-20.0093570920361));
#117980=CARTESIAN_POINT('Ctrl Pts',(-17.3698587893405,16.908616461354,-20.1365328987175));
#117981=CARTESIAN_POINT('Ctrl Pts',(-19.9315560549264,16.8177368822917,
-20.2637087053989));
#117982=CARTESIAN_POINT('Ctrl Pts',(-21.3945706447594,18.9225266095884,
-20.3908845120804));
#117983=CARTESIAN_POINT('Ctrl Pts',(-20.4166754991338,21.2919748133934,
-20.5180603187618));
#117984=CARTESIAN_POINT('Ctrl Pts',(-17.8950325316693,21.7522538440923,
-20.6452361254433));
#117985=CARTESIAN_POINT('Ctrl Pts',(-16.1430853073993,19.881097796524,-20.7724119321247));
#117986=CARTESIAN_POINT('Ctrl Pts',(-16.7681508238931,17.395153974591,-20.8995877388061));
#117987=CARTESIAN_POINT('Ctrl Pts',(-19.1967429841419,16.5751643826307,
-21.0267635454876));
#117988=CARTESIAN_POINT('Ctrl Pts',(-21.2008317885977,18.1733360181572,
-21.153939352169));
#117989=CARTESIAN_POINT('Ctrl Pts',(-20.9416888395956,20.7236046919281,
-21.2811151588505));
#117990=CARTESIAN_POINT('Ctrl Pts',(-18.6572569308498,21.8859506052002,
-21.4082909655318));
#117991=CARTESIAN_POINT('Ctrl Pts',(-16.4429843423899,20.5945843440041,
-21.5354667722133));
#117992=CARTESIAN_POINT('Ctrl Pts',(-16.3310538134642,18.033115434702,-21.6626425788947));
#117993=CARTESIAN_POINT('Ctrl Pts',(-18.4227563631869,16.5537305545665,
-21.7898183855762));
#117994=CARTESIAN_POINT('Ctrl Pts',(-20.8017893666684,17.50940661932,-21.9169941922576));
#117995=CARTESIAN_POINT('Ctrl Pts',(-21.2802300646426,20.0318897120323,
-22.0441699989391));
#117996=CARTESIAN_POINT('Ctrl Pts',(-20.0469416504615,21.2025211683863,
-22.12895387006));
#117997=CARTESIAN_POINT('Ctrl Pts',(-19.3190223666151,21.3973017229923,
-22.1713458056205));
#117998=CARTESIAN_POINT('Ctrl Pts',(-16.8880690316762,20.7654464739225,
0.171094734500185));
#117999=CARTESIAN_POINT('Ctrl Pts',(-16.3702699845374,20.1505948657621,
0.128684141441329));
#118000=CARTESIAN_POINT('Ctrl Pts',(-16.006827020915,18.3736777454539,0.043881612821995));
#118001=CARTESIAN_POINT('Ctrl Pts',(-17.9658924760107,16.4608289063181,
-0.0833128513578171));
#118002=CARTESIAN_POINT('Ctrl Pts',(-20.6289599190898,17.0785068518555,
-0.210488658039252));
#118003=CARTESIAN_POINT('Ctrl Pts',(-21.5536817767679,19.6490616868026,
-0.337664464720685));
#118004=CARTESIAN_POINT('Ctrl Pts',(-19.8914411384235,21.8195502173065,
-0.46484027140212));
#118005=CARTESIAN_POINT('Ctrl Pts',(-17.1673608230486,21.5959088255693,
-0.592016078083554));
#118006=CARTESIAN_POINT('Ctrl Pts',(-15.8805536346544,19.1847528689885,
-0.719191884764988));
#118007=CARTESIAN_POINT('Ctrl Pts',(-17.2116173157294,16.7974221125058,
-0.846367691446423));
#118008=CARTESIAN_POINT('Ctrl Pts',(-19.9393669463845,16.6245315463164,
-0.973543498127856));
#118009=CARTESIAN_POINT('Ctrl Pts',(-21.5612701613726,18.8244966062191,
-1.10071930480929));
#118010=CARTESIAN_POINT('Ctrl Pts',(-20.5893269556668,21.379090163636,-1.22789511149073));
#118011=CARTESIAN_POINT('Ctrl Pts',(-17.9152372155514,21.9445770767739,
-1.35507091817216));
#118012=CARTESIAN_POINT('Ctrl Pts',(-15.9923111005858,20.0021862799634,
-1.4822467248536));
#118013=CARTESIAN_POINT('Ctrl Pts',(-16.5847145959355,17.3339261996511,
-1.60942253153503));
#118014=CARTESIAN_POINT('Ctrl Pts',(-19.1489539390206,16.3877674101879,
-1.73659833821646));
#118015=CARTESIAN_POINT('Ctrl Pts',(-21.332498855497,18.0317479516957,-1.8637741448979));
#118016=CARTESIAN_POINT('Ctrl Pts',(-21.1320823232458,20.7576197505752,
-1.99094995157933));
#118017=CARTESIAN_POINT('Ctrl Pts',(-18.7315741166753,22.064563561331,-2.11812575826077));
#118018=CARTESIAN_POINT('Ctrl Pts',(-16.3332914994529,20.7535401040407,
-2.2453015649422));
#118019=CARTESIAN_POINT('Ctrl Pts',(-16.1375099308779,18.0273317449088,
-2.37247737162363));
#118020=CARTESIAN_POINT('Ctrl Pts',(-18.3238468422098,16.387065593537,-2.49965317830507));
#118021=CARTESIAN_POINT('Ctrl Pts',(-20.8864738199611,17.3375839607775,
-2.62682898498651));
#118022=CARTESIAN_POINT('Ctrl Pts',(-21.4743396649076,20.006845280278,-2.75400479166794));
#118023=CARTESIAN_POINT('Ctrl Pts',(-19.5481139522653,21.9459679438018,
-2.88118059834937));
#118024=CARTESIAN_POINT('Ctrl Pts',(-16.8749892178732,21.3759272738012,
-3.00835640503081));
#118025=CARTESIAN_POINT('Ctrl Pts',(-15.9073914929419,18.8197001987301,
-3.13553221171224));
#118026=CARTESIAN_POINT('Ctrl Pts',(-17.5330316340844,16.6224664055047,
-3.26270801839368));
#118027=CARTESIAN_POINT('Ctrl Pts',(-20.2604857104729,16.8000515222033,
-3.38988382507511));
#118028=CARTESIAN_POINT('Ctrl Pts',(-21.5874838918795,19.1895322272068,
-3.51705963175655));
#118029=CARTESIAN_POINT('Ctrl Pts',(-20.2965877096769,21.5987082811702,
-3.64423543843798));
#118030=CARTESIAN_POINT('Ctrl Pts',(-17.5721142889738,21.8173101851209,
-3.77141124511941));
#118031=CARTESIAN_POINT('Ctrl Pts',(-15.9135988933785,19.64478426004,-3.89858705180085));
#118032=CARTESIAN_POINT('Ctrl Pts',(-16.8426264592725,17.0742882000792,
-4.02576285848228));
#118033=CARTESIAN_POINT('Ctrl Pts',(-19.5068718569032,16.4640925972449,
-4.15293866516372));
#118034=CARTESIAN_POINT('Ctrl Pts',(-21.4620552956622,18.3740140441421,
-4.28011447184515));
#118035=CARTESIAN_POINT('Ctrl Pts',(-20.914417322859,21.0518181563291,-4.40729027852659));
#118036=CARTESIAN_POINT('Ctrl Pts',(-18.3663817882941,22.0407858641459,
-4.53446608520802));
#118037=CARTESIAN_POINT('Ctrl Pts',(-16.15561314601,20.4336006779268,-4.66164189188945));
#118038=CARTESIAN_POINT('Ctrl Pts',(-16.3103544095251,17.7047552528665,
-4.78881769857089));
#118039=CARTESIAN_POINT('Ctrl Pts',(-18.6886400738904,16.3577958952085,
-4.91599350525232));
#118040=CARTESIAN_POINT('Ctrl Pts',(-21.1085406551067,17.628474213878,-5.04316931193375));
#118041=CARTESIAN_POINT('Ctrl Pts',(-21.3499475658771,20.3510217186868,
-5.1703451186152));
#118042=CARTESIAN_POINT('Ctrl Pts',(-19.1913849489723,22.0276700543283,
-5.29752092529662));
#118043=CARTESIAN_POINT('Ctrl Pts',(-16.613200029897,21.1201984373834,-5.42469673197806));
#118044=CARTESIAN_POINT('Ctrl Pts',(-15.9807174516997,18.4611557523585,
-5.5518725386595));
#118045=CARTESIAN_POINT('Ctrl Pts',(-17.8742007235803,16.4900486239617,
-5.67904834534092));
#118046=CARTESIAN_POINT('Ctrl Pts',(-20.5564964664144,17.0152455017915,
-5.80622415202237));
#118047=CARTESIAN_POINT('Ctrl Pts',(-21.5667648182011,19.5549108478334,
-5.93339995870379));
#118048=CARTESIAN_POINT('Ctrl Pts',(-19.9781472705019,21.7790593365027,
-6.06057576538524));
#118049=CARTESIAN_POINT('Ctrl Pts',(-17.2481018226055,21.6471727756692,
-6.18775157206665));
#118050=CARTESIAN_POINT('Ctrl Pts',(-15.8812757272267,19.2802488990946,
-6.31492737874811));
#118051=CARTESIAN_POINT('Ctrl Pts',(-17.1316470920802,16.849793455672,-6.44210318542952));
#118052=CARTESIAN_POINT('Ctrl Pts',(-19.8520777967125,16.5855984636642,
-6.56927899211098));
#118053=CARTESIAN_POINT('Ctrl Pts',(-21.5467415185955,18.7300464304477,
-6.6964547987924));
#118054=CARTESIAN_POINT('Ctrl Pts',(-20.6608894755945,21.3157394459503,
-6.82363060547384));
#118055=CARTESIAN_POINT('Ctrl Pts',(-18.0072359349844,21.9704646546564,
-6.95080641215527));
#118056=CARTESIAN_POINT('Ctrl Pts',(-16.020343315961,20.0935523144076,-7.07798221883671));
#118057=CARTESIAN_POINT('Ctrl Pts',(-16.5230622760143,17.4069530030642,
-7.20515802551813));
#118058=CARTESIAN_POINT('Ctrl Pts',(-19.0541793715532,16.3754548396247,
-7.33233383219958));
#118059=CARTESIAN_POINT('Ctrl Pts',(-21.291551766265,17.9453933670485,-7.459509638881));
#118060=CARTESIAN_POINT('Ctrl Pts',(-21.1825291549937,20.6764474277986,
-7.58668544556244));
#118061=CARTESIAN_POINT('Ctrl Pts',(-18.8271330168744,22.0630444294688,
-7.71386125224388));
#118062=CARTESIAN_POINT('Ctrl Pts',(-16.3862931162597,20.8330676849425,
-7.84103705892531));
#118063=CARTESIAN_POINT('Ctrl Pts',(-16.099328566354,18.1149445163563,-7.96821286560675));
#118064=CARTESIAN_POINT('Ctrl Pts',(-18.2295115306668,16.4023842251376,
-8.09538867228817));
#118065=CARTESIAN_POINT('Ctrl Pts',(-20.8225313535071,17.2665545850003,
-8.22256447896962));
#118066=CARTESIAN_POINT('Ctrl Pts',(-21.4994532883798,19.9146329272319,
-8.34974028565105));
#118067=CARTESIAN_POINT('Ctrl Pts',(-19.6392434745528,21.917171731113,-8.47691609233248));
#118068=CARTESIAN_POINT('Ctrl Pts',(-16.9485289585702,21.4369659356584,
-8.60409189901392));
#118069=CARTESIAN_POINT('Ctrl Pts',(-15.8958733042685,18.9145745532647,
-8.73126770569535));
#118070=CARTESIAN_POINT('Ctrl Pts',(-17.4470227392911,16.6641351200123,
-8.85844351237678));
#118071=CARTESIAN_POINT('Ctrl Pts',(-20.1788939321968,16.7502861378866,
-8.98561931905823));
#118072=CARTESIAN_POINT('Ctrl Pts',(-21.5851646225432,19.093989395123,-9.11279512573965));
#118073=CARTESIAN_POINT('Ctrl Pts',(-20.3756687349405,21.5450426198368,
-9.23997093242109));
#118074=CARTESIAN_POINT('Ctrl Pts',(-17.6600436764829,21.8547566078734,
-9.36714673910252));
#118075=CARTESIAN_POINT('Ctrl Pts',(-15.9297068876053,19.738987998227,-9.49432254578396));
#118076=CARTESIAN_POINT('Ctrl Pts',(-16.7721349752896,17.1388231708385,
-9.62149835246539));
#118077=CARTESIAN_POINT('Ctrl Pts',(-19.4144524560694,16.4397519704066,
-9.74867415914682));
#118078=CARTESIAN_POINT('Ctrl Pts',(-21.432497042048,18.2831288340757,-9.87584996582827));
#118079=CARTESIAN_POINT('Ctrl Pts',(-20.974838079563,20.9777699023008,-10.0030257725097));
#118080=CARTESIAN_POINT('Ctrl Pts',(-18.4613492611758,22.0515092432722,
-10.1302015791911));
#118081=CARTESIAN_POINT('Ctrl Pts',(-16.1980005730462,20.5192576554282,
-10.2573773858725));
#118082=CARTESIAN_POINT('Ctrl Pts',(-16.2612739572708,17.7867608683564,
-10.384553192554));
#118083=CARTESIAN_POINT('Ctrl Pts',(-18.5931200110123,16.3609150863178,
-10.5117289992354));
#118084=CARTESIAN_POINT('Ctrl Pts',(-21.0542147106519,17.5498453163626,
-10.6389048059168));
#118085=CARTESIAN_POINT('Ctrl Pts',(-21.3866564220343,20.2627818657572,
-10.7660806125983));
#118086=CARTESIAN_POINT('Ctrl Pts',(-19.2854505086261,22.0107738342645,
-10.8932564192797));
#118087=CARTESIAN_POINT('Ctrl Pts',(-16.6783229804319,21.1901470833962,
-11.0204322259611));
#118088=CARTESIAN_POINT('Ctrl Pts',(-15.9571515279862,18.5537757232337,
-11.1476080326426));
#118089=CARTESIAN_POINT('Ctrl Pts',(-17.7835661979594,16.5203668450652,
-11.274783839324));
#118090=CARTESIAN_POINT('Ctrl Pts',(-20.4819448907301,16.9554468870216,
-11.4019596460055));
#118091=CARTESIAN_POINT('Ctrl Pts',(-21.5766926359512,19.4598569147211,
-11.5291354526869));
#118092=CARTESIAN_POINT('Ctrl Pts',(-20.0634463250904,21.735956168966,-11.6563112593683));
#118093=CARTESIAN_POINT('Ctrl Pts',(-17.330515525704,21.6955648546388,-11.7834870660497));
#118094=CARTESIAN_POINT('Ctrl Pts',(-15.8851946214135,19.3757394956669,
-11.9106628727312));
#118095=CARTESIAN_POINT('Ctrl Pts',(-17.053475835173,16.9047758743069,-12.0378386794126));
#118096=CARTESIAN_POINT('Ctrl Pts',(-19.7635336650682,16.5496297478578,
-12.165014486094));
#118097=CARTESIAN_POINT('Ctrl Pts',(-21.5290582573291,18.6361256444822,
-12.2921902927755));
#118098=CARTESIAN_POINT('Ctrl Pts',(-20.7302903793709,21.2500330815675,
-12.4193660994569));
#118099=CARTESIAN_POINT('Ctrl Pts',(-18.1000499820946,21.9932542229807,
-12.5465419061383));
#118100=CARTESIAN_POINT('Ctrl Pts',(-16.0514193788707,20.1839298009815,
-12.6737177128198));
#118101=CARTESIAN_POINT('Ctrl Pts',(-16.4638899958019,17.4820026734157,
-12.8008935195012));
#118102=CARTESIAN_POINT('Ctrl Pts',(-18.9590456426675,16.3663232793141,
-12.9280693261827));
#118103=CARTESIAN_POINT('Ctrl Pts',(-21.2477358802935,17.8604582158923,
-13.0552451328641));
#118104=CARTESIAN_POINT('Ctrl Pts',(-21.2302294677946,20.5936314153126,
-13.1824209395455));
#118105=CARTESIAN_POINT('Ctrl Pts',(-18.9225874520683,22.0583261069674,
-13.309596746227));
#118106=CARTESIAN_POINT('Ctrl Pts',(-16.4419281541264,20.9107758204687,
-13.4367725529084));
#118107=CARTESIAN_POINT('Ctrl Pts',(-16.0641025127507,18.2037867186756,
-13.5639483595899));
#118108=CARTESIAN_POINT('Ctrl Pts',(-18.1357421033992,16.4208532877909,
-13.6911241662712));
#118109=CARTESIAN_POINT('Ctrl Pts',(-20.756246182106,17.1977062893226,-13.8182999729527));
#118110=CARTESIAN_POINT('Ctrl Pts',(-21.5214649034841,19.8216313113002,
-13.9454757796341));
#118111=CARTESIAN_POINT('Ctrl Pts',(-19.7293575854992,21.8853400052135,
-14.0726515863156));
#118112=CARTESIAN_POINT('Ctrl Pts',(-17.0240714616778,21.495507732604,-14.199827392997));
#118113=CARTESIAN_POINT('Ctrl Pts',(-15.8875386416327,19.0097814078715,
-14.3270031996784));
#118114=CARTESIAN_POINT('Ctrl Pts',(-17.3624574465728,16.7086606523826,
-14.4541790063599));
#118115=CARTESIAN_POINT('Ctrl Pts',(-20.0956814167509,16.7032809356367,
-14.5813548130413));
#118116=CARTESIAN_POINT('Ctrl Pts',(-21.5796472025402,18.9985778138453,
-14.7085306197227));
#118117=CARTESIAN_POINT('Ctrl Pts',(-20.4529083007835,21.4887588634431,
-14.8357064264042));
#118118=CARTESIAN_POINT('Ctrl Pts',(-17.749177720539,21.8892375294908,-14.9628822330856));
#118119=CARTESIAN_POINT('Ctrl Pts',(-15.9489604567358,19.8325994923992,
-15.090058039767));
#118120=CARTESIAN_POINT('Ctrl Pts',(-16.7038441148285,17.2056825018467,
-15.2172338464485));
#118121=CARTESIAN_POINT('Ctrl Pts',(-19.321269791881,16.4185198518092,-15.3444096531299));
#118122=CARTESIAN_POINT('Ctrl Pts',(-21.3999118849568,18.1932844168717,
-15.4715854598113));
#118123=CARTESIAN_POINT('Ctrl Pts',(-21.0327452887372,20.9017398629015,
-15.5987612664928));
#118124=CARTESIAN_POINT('Ctrl Pts',(-18.5566225663247,22.05904642387,-15.7259370731742));
#118125=CARTESIAN_POINT('Ctrl Pts',(-16.2432326300242,20.6034471606347,
-15.8531128798556));
#118126=CARTESIAN_POINT('Ctrl Pts',(-16.2149671612184,17.8703640525348,
-15.9802886865371));
#118127=CARTESIAN_POINT('Ctrl Pts',(-18.4977579731839,16.367231216983,-16.1074644932185));
#118128=CARTESIAN_POINT('Ctrl Pts',(-20.9972861819192,17.4730797356526,
-16.2346402999));
#118129=CARTESIAN_POINT('Ctrl Pts',(-21.4203897941269,20.1733622293642,
-16.3618161065814));
#118130=CARTESIAN_POINT('Ctrl Pts',(-19.378897506378,21.9907371085704,-16.4889919132628));
#118131=CARTESIAN_POINT('Ctrl Pts',(-16.7457517833806,21.2578757206061,
-16.6161677199442));
#118132=CARTESIAN_POINT('Ctrl Pts',(-15.9367003945299,18.6471329024206,
-16.7433435266257));
#118133=CARTESIAN_POINT('Ctrl Pts',(-17.6939977737036,16.5537031487253,
-16.8705193333071));
#118134=CARTESIAN_POINT('Ctrl Pts',(-20.4054326456863,16.8981783256312,
-16.9976951399886));
#118135=CARTESIAN_POINT('Ctrl Pts',(-21.5834318060615,19.364523838868,-17.12487094667));
#118136=CARTESIAN_POINT('Ctrl Pts',(-20.1472541400588,21.6900207587073,
-17.2520467533514));
#118137=CARTESIAN_POINT('Ctrl Pts',(-17.4145035169965,21.7411699978141,
-17.3792225600329));
#118138=CARTESIAN_POINT('Ctrl Pts',(-15.8923090199021,19.4710453039867,
-17.5063983667143));
#118139=CARTESIAN_POINT('Ctrl Pts',(-16.9771896218132,16.9623451839844,
-17.6335741733957));
#118140=CARTESIAN_POINT('Ctrl Pts',(-19.6738347057625,16.5166462904161,
-17.7607499800772));
#118141=CARTESIAN_POINT('Ctrl Pts',(-21.5082397798925,18.542849694944,-17.8879257867586));
#118142=CARTESIAN_POINT('Ctrl Pts',(-20.7974520447164,21.1820395342675,
-18.01510159344));
#118143=CARTESIAN_POINT('Ctrl Pts',(-18.1935751307804,22.0129229374273,
-18.1422774001214));
#118144=CARTESIAN_POINT('Ctrl Pts',(-16.085504491823,20.2732159524167,-18.2694532068029));
#118145=CARTESIAN_POINT('Ctrl Pts',(-16.4072640974092,17.5589917596816,
-18.3966290134843));
#118146=CARTESIAN_POINT('Ctrl Pts',(-18.8636594801795,16.3603825921271,
-18.5238048201658));
#118147=CARTESIAN_POINT('Ctrl Pts',(-21.2011003373174,17.7770379672497,
-18.6509806268472));
#118148=CARTESIAN_POINT('Ctrl Pts',(-21.2751297607577,20.5092645052679,
-18.7781564335287));
#118149=CARTESIAN_POINT('Ctrl Pts',(-19.0178303484736,22.0504139399173,
-18.90533224021));
#118150=CARTESIAN_POINT('Ctrl Pts',(-16.5001342089838,20.9865773169943,
-19.0325080468915));
#118151=CARTESIAN_POINT('Ctrl Pts',(-16.0318712814367,18.2937587135751,
-19.1596838535729));
#118152=CARTESIAN_POINT('Ctrl Pts',(-18.042643743939,16.4424520540833,-19.2868596602544));
#118153=CARTESIAN_POINT('Ctrl Pts',(-20.6876926536642,17.1311163109758,
-19.4140354669358));
#118154=CARTESIAN_POINT('Ctrl Pts',(-21.5403498275698,19.7279447383034,
-19.5412112736172));
#118155=CARTESIAN_POINT('Ctrl Pts',(-19.8183551892704,21.8505084960413,
-19.6683870802987));
#118156=CARTESIAN_POINT('Ctrl Pts',(-17.1015320197568,21.5514869529538,
-19.7955628869801));
#118157=CARTESIAN_POINT('Ctrl Pts',(-15.8823967990051,19.1052140557062,
-19.9227386936616));
#118158=CARTESIAN_POINT('Ctrl Pts',(-17.2794307188022,16.7559928917323,
-20.049914500343));
#118159=CARTESIAN_POINT('Ctrl Pts',(-20.0109412993294,16.6590889620223,
-20.1770903070244));
#118160=CARTESIAN_POINT('Ctrl Pts',(-21.5709382143749,18.9034038883535,
-20.3042661137059));
#118161=CARTESIAN_POINT('Ctrl Pts',(-20.5282190091016,21.4299213366298,
-20.4314419203873));
#118162=CARTESIAN_POINT('Ctrl Pts',(-17.839417901151,21.920711977366,-20.5586177270687));
#118163=CARTESIAN_POINT('Ctrl Pts',(-15.9713351874334,19.9255181617605,
-20.6857935337502));
#118164=CARTESIAN_POINT('Ctrl Pts',(-16.6378359073908,17.2747826734461,
-20.8129693404316));
#118165=CARTESIAN_POINT('Ctrl Pts',(-19.227417928117,16.4004364825627,-20.940145147113));
#118166=CARTESIAN_POINT('Ctrl Pts',(-21.3643565302024,18.1045499196127,
-21.0673209537945));
#118167=CARTESIAN_POINT('Ctrl Pts',(-21.0880351566437,20.8238743140973,
-21.1944967604759));
#118168=CARTESIAN_POINT('Ctrl Pts',(-18.6521696806325,22.0632714134299,
-21.3216725671574));
#118169=CARTESIAN_POINT('Ctrl Pts',(-16.2911143425161,20.6863012877323,
-21.4488483738387));
#118170=CARTESIAN_POINT('Ctrl Pts',(-16.171764008598,17.9550342010845,-21.5760241805202));
#118171=CARTESIAN_POINT('Ctrl Pts',(-18.4021242165115,16.3775818193965,
-21.7031999872016));
#118172=CARTESIAN_POINT('Ctrl Pts',(-20.9388618348603,17.3966090547766,
-21.8303757938831));
#118173=CARTESIAN_POINT('Ctrl Pts',(-21.4490180684747,20.086305979354,-21.9575516005645));
#118174=CARTESIAN_POINT('Ctrl Pts',(-20.1339757340687,21.3345378652548,
-22.0423354716855));
#118175=CARTESIAN_POINT('Ctrl Pts',(-19.3578031346334,21.5422303014122,
-22.0847274072459));
#118176=CARTESIAN_POINT('Ctrl Pts',(-16.7733106781415,20.8620837377565,
0.257713132874659));
#118177=CARTESIAN_POINT('Ctrl Pts',(-16.2233209547904,20.2090078625832,
0.215302539815803));
#118178=CARTESIAN_POINT('Ctrl Pts',(-15.8372833671953,18.3216228609763,
0.13050001119647));
#118179=CARTESIAN_POINT('Ctrl Pts',(-17.9181405522913,16.2898554993676,
0.00330554701665787));
#118180=CARTESIAN_POINT('Ctrl Pts',(-20.7467663181702,16.9459334204518,
-0.123870259664777));
#118181=CARTESIAN_POINT('Ctrl Pts',(-21.7289765433362,19.6762952284609,
-0.251046066346211));
#118182=CARTESIAN_POINT('Ctrl Pts',(-19.9633972633481,21.9817192979427,
-0.378221873027645));
#118183=CARTESIAN_POINT('Ctrl Pts',(-17.0699655598372,21.7441745055157,
-0.50539767970908));
#118184=CARTESIAN_POINT('Ctrl Pts',(-15.703159781685,19.1831211299953,-0.632573486390514));
#118185=CARTESIAN_POINT('Ctrl Pts',(-17.1169734025524,16.6473741262867,
-0.759749293071947));
#118186=CARTESIAN_POINT('Ctrl Pts',(-20.0143025363638,16.4637352509469,
-0.886925099753383));
#118187=CARTESIAN_POINT('Ctrl Pts',(-21.7370366847608,18.8004683549644,
-1.01410090643482));
#118188=CARTESIAN_POINT('Ctrl Pts',(-20.7046694415748,21.5138766002705,
-1.14127671311625));
#118189=CARTESIAN_POINT('Ctrl Pts',(-17.8643361414099,22.1145188622328,
-1.26845251979769));
#118190=CARTESIAN_POINT('Ctrl Pts',(-15.8218650170646,20.0513729702491,
-1.39562832647912));
#118191=CARTESIAN_POINT('Ctrl Pts',(-16.4510972188617,17.217231749811,-1.52280413316055));
#118192=CARTESIAN_POINT('Ctrl Pts',(-19.1747509117416,16.2122518956796,
-1.64997993984199));
#118193=CARTESIAN_POINT('Ctrl Pts',(-21.4940430602564,17.9584358800158,
-1.77715574652343));
#118194=CARTESIAN_POINT('Ctrl Pts',(-21.281166976886,20.8537704404796,-1.90433155320486));
#118195=CARTESIAN_POINT('Ctrl Pts',(-18.7314233036813,22.2419647001733,
-2.03150735988629));
#118196=CARTESIAN_POINT('Ctrl Pts',(-16.1840435808866,20.8494371693366,
-2.15868316656773));
#118197=CARTESIAN_POINT('Ctrl Pts',(-15.9760906089126,17.9537451252482,
-2.28585897324916));
#118198=CARTESIAN_POINT('Ctrl Pts',(-18.2983483258012,16.2115064482945,
-2.4130347799306));
#118199=CARTESIAN_POINT('Ctrl Pts',(-21.0202894153674,17.2211169076559,
-2.54021058661203));
#118200=CARTESIAN_POINT('Ctrl Pts',(-21.64470186884,20.0563216126004,-2.66738639329346));
#118201=CARTESIAN_POINT('Ctrl Pts',(-19.5987260165054,22.1159961970718,
-2.7945621999749));
#118202=CARTESIAN_POINT('Ctrl Pts',(-16.75941771481,21.5105170790144,-2.92173800665633));
#118203=CARTESIAN_POINT('Ctrl Pts',(-15.7316661034645,18.7953737630709,
-3.04891381333777));
#118204=CARTESIAN_POINT('Ctrl Pts',(-17.4583694962879,16.4615417238828,
-3.1760896200192));
#118205=CARTESIAN_POINT('Ctrl Pts',(-20.3553847017321,16.6501670018626,
-3.30326542670064));
#118206=CARTESIAN_POINT('Ctrl Pts',(-21.7648800778091,19.1881976126941,
-3.43044123338207));
#118207=CARTESIAN_POINT('Ctrl Pts',(-20.3937311001358,21.7471479984566,
-3.5576170400635));
#118208=CARTESIAN_POINT('Ctrl Pts',(-17.4998818526146,21.9793400068086,
-3.68479284674494));
#118209=CARTESIAN_POINT('Ctrl Pts',(-15.7382594073102,19.671751881433,-3.81196865342637));
#118210=CARTESIAN_POINT('Ctrl Pts',(-16.7250430191669,16.9414525023501,
-3.93914446010781));
#118211=CARTESIAN_POINT('Ctrl Pts',(-19.5549199710057,16.2933220883461,
-4.06632026678924));
#118212=CARTESIAN_POINT('Ctrl Pts',(-21.6316538014862,18.3219800667756,
-4.19349607347067));
#118213=CARTESIAN_POINT('Ctrl Pts',(-21.0499701177813,21.1662586551355,
-4.32067188015211));
#118214=CARTESIAN_POINT('Ctrl Pts',(-18.3435275963289,22.2167087844487,
-4.44784768683354));
#118215=CARTESIAN_POINT('Ctrl Pts',(-15.995319269794,20.5096076593562,-4.57502349351498));
#118216=CARTESIAN_POINT('Ctrl Pts',(-16.1596805315267,17.6111146074862,
-4.70219930019641));
#118217=CARTESIAN_POINT('Ctrl Pts',(-18.6858201252975,16.180417103161,-4.82937510687785));
#118218=CARTESIAN_POINT('Ctrl Pts',(-21.2561617637276,17.5300913074975,
-4.95655091355928));
#118219=CARTESIAN_POINT('Ctrl Pts',(-21.5125765269513,20.4218949082454,
-5.08372672024072));
#118220=CARTESIAN_POINT('Ctrl Pts',(-19.2198197846062,22.2027775872924,
-5.21090252692215));
#118221=CARTESIAN_POINT('Ctrl Pts',(-16.4813535432613,21.2388900206576,
-5.33807833360358));
#118222=CARTESIAN_POINT('Ctrl Pts',(-15.8095506109669,18.4145392251191,
-5.46525414028503));
#118223=CARTESIAN_POINT('Ctrl Pts',(-17.8207484813105,16.3208917566031,
-5.59242994696645));
#118224=CARTESIAN_POINT('Ctrl Pts',(-20.6697979372697,16.8787392210558,
-5.71960575364789));
#118225=CARTESIAN_POINT('Ctrl Pts',(-21.7428729349543,19.5762911937604,
-5.84678156032932));
#118226=CARTESIAN_POINT('Ctrl Pts',(-20.0554937665343,21.9387111687183,
-5.97395736701076));
#118227=CARTESIAN_POINT('Ctrl Pts',(-17.1557260884723,21.7986254472259,
-6.10113317369219));
#118228=CARTESIAN_POINT('Ctrl Pts',(-15.7039267655104,19.284553984052,-6.22830898037363));
#118229=CARTESIAN_POINT('Ctrl Pts',(-17.0320315676376,16.7030013057854,
-6.35548478705506));
#118230=CARTESIAN_POINT('Ctrl Pts',(-19.9215867703828,16.4223817655062,
-6.48266059373649));
#118231=CARTESIAN_POINT('Ctrl Pts',(-21.7216048212496,18.7001463742074,
-6.60983640041793));
#118232=CARTESIAN_POINT('Ctrl Pts',(-20.7806808802879,21.4465874774214,
-6.73701220709936));
#118233=CARTESIAN_POINT('Ctrl Pts',(-17.9620542630039,22.1420158263089,
-6.8641880137808));
#118234=CARTESIAN_POINT('Ctrl Pts',(-15.8516399470578,20.1484190739168,
-6.99136382046223));
#118235=CARTESIAN_POINT('Ctrl Pts',(-16.3856120802451,17.2947985039956,
-7.11853962714367));
#118236=CARTESIAN_POINT('Ctrl Pts',(-19.0740843724149,16.1991738737805,
-7.2457154338251));
#118237=CARTESIAN_POINT('Ctrl Pts',(-21.4505503609105,17.86671277936,-7.37289124050654));
#118238=CARTESIAN_POINT('Ctrl Pts',(-21.3347500014016,20.7675517740021,
-7.50006704718796));
#118239=CARTESIAN_POINT('Ctrl Pts',(-18.8329229363566,22.240351126496,-7.62724285386941));
#118240=CARTESIAN_POINT('Ctrl Pts',(-16.2403402170543,20.9339088431657,
-7.75441866055083));
#118241=CARTESIAN_POINT('Ctrl Pts',(-15.9355355746231,18.0468046320139,
-7.88159446723227));
#118242=CARTESIAN_POINT('Ctrl Pts',(-18.1981483501842,16.2277774128756,
-8.0087702739137));
#118243=CARTESIAN_POINT('Ctrl Pts',(-20.952371755747,17.145671757748,-8.13594608059513));
#118244=CARTESIAN_POINT('Ctrl Pts',(-21.6713767630913,19.958376576159,-8.26312188727658));
#118245=CARTESIAN_POINT('Ctrl Pts',(-19.6955209044624,22.0854097733659,
-8.390297693958));
#118246=CARTESIAN_POINT('Ctrl Pts',(-16.8375292947071,21.5753504095007,
-8.51747350063944));
#118247=CARTESIAN_POINT('Ctrl Pts',(-15.719431848811,18.8961462930551,-8.64464930732087));
#118248=CARTESIAN_POINT('Ctrl Pts',(-17.3670135764298,16.5058009107065,
-8.77182511400231));
#118249=CARTESIAN_POINT('Ctrl Pts',(-20.268720502928,16.5973077891932,-8.89900092068374));
#118250=CARTESIAN_POINT('Ctrl Pts',(-21.7624166234869,19.0867150470611,
-9.02617672736517));
#118251=CARTESIAN_POINT('Ctrl Pts',(-20.4777284567308,21.6901460352563,
-9.15335253404662));
#118252=CARTESIAN_POINT('Ctrl Pts',(-17.5932776589179,22.0191144092604,
-9.28052834072804));
#118253=CARTESIAN_POINT('Ctrl Pts',(-15.7553688078344,19.7718121040047,
-9.40770414740949));
#118254=CARTESIAN_POINT('Ctrl Pts',(-16.6501692008611,17.0099995012495,
-9.53487995409091));
#118255=CARTESIAN_POINT('Ctrl Pts',(-19.4567550149717,16.2674682466002,
-9.66205576077236));
#118256=CARTESIAN_POINT('Ctrl Pts',(-21.6002579620812,18.2254446795103,
-9.78923156745378));
#118257=CARTESIAN_POINT('Ctrl Pts',(-21.1141471290137,21.0876069485077,
-9.91640737413522));
#118258=CARTESIAN_POINT('Ctrl Pts',(-18.4443990336675,22.2280988176125,
-10.0435831808167));
#118259=CARTESIAN_POINT('Ctrl Pts',(-16.0403418502683,20.6005897838297,
-10.1707589874981));
#118260=CARTESIAN_POINT('Ctrl Pts',(-16.1075488319678,17.698218371052,-10.2979347941796));
#118261=CARTESIAN_POINT('Ctrl Pts',(-18.5843617443927,16.183730209017,-10.425110600861));
#118262=CARTESIAN_POINT('Ctrl Pts',(-21.1984584687395,17.4465741866552,
-10.5522864075424));
#118263=CARTESIAN_POINT('Ctrl Pts',(-21.5515675095613,20.3281693354206,
-10.6794622142238));
#118264=CARTESIAN_POINT('Ctrl Pts',(-19.3197332383227,22.1848309582866,
-10.8066380209053));
#118265=CARTESIAN_POINT('Ctrl Pts',(-16.5505250756278,21.3131872536903,
-10.9338138275867));
#118266=CARTESIAN_POINT('Ctrl Pts',(-15.7845196343066,18.5129172202892,
-11.0609896342681));
#118267=CARTESIAN_POINT('Ctrl Pts',(-17.7244793631115,16.3530948093689,
-11.1881654409496));
#118268=CARTESIAN_POINT('Ctrl Pts',(-20.5906116183444,16.8152230292517,
-11.315341247631));
#118269=CARTESIAN_POINT('Ctrl Pts',(-21.7534179480593,19.4753279211071,
-11.4425170543125));
#118270=CARTESIAN_POINT('Ctrl Pts',(-20.1460957166432,21.8929283513879,
-11.5696928609939));
#118271=CARTESIAN_POINT('Ctrl Pts',(-17.2432633097514,21.8500259785168,
-11.6968686676753));
#118272=CARTESIAN_POINT('Ctrl Pts',(-15.7080892906089,19.3859810667816,
-11.8240444743568));
#118273=CARTESIAN_POINT('Ctrl Pts',(-16.9490005381331,16.7614018868241,
-11.9512202810382));
#118274=CARTESIAN_POINT('Ctrl Pts',(-19.8275380023589,16.3841769364998,
-12.0783960877196));
#118275=CARTESIAN_POINT('Ctrl Pts',(-21.7028222220433,18.6003866945102,
-12.205571894401));
#118276=CARTESIAN_POINT('Ctrl Pts',(-20.8543963188915,21.3767962613715,
-12.3327477010825));
#118277=CARTESIAN_POINT('Ctrl Pts',(-18.0606383997947,22.1662221829007,
-12.4599235077639));
#118278=CARTESIAN_POINT('Ctrl Pts',(-15.8846479553519,20.2444151733933,
-12.5870993144454));
#118279=CARTESIAN_POINT('Ctrl Pts',(-16.3227611611408,17.3745138832769,
-12.7142751211268));
#118280=CARTESIAN_POINT('Ctrl Pts',(-18.9730363432223,16.1894746200704,
-12.8414509278082));
#118281=CARTESIAN_POINT('Ctrl Pts',(-21.4040105166661,17.776497355934,-12.9686267344897));
#118282=CARTESIAN_POINT('Ctrl Pts',(-21.385415760611,20.6795872324527,-13.0958025411711));
#118283=CARTESIAN_POINT('Ctrl Pts',(-18.934311609617,22.2353394739996,-13.2229783478525));
#118284=CARTESIAN_POINT('Ctrl Pts',(-16.2994339895399,21.0164479598295,
-13.350154154534));
#118285=CARTESIAN_POINT('Ctrl Pts',(-15.8981195778519,18.1411700012542,
-13.4773299612154));
#118286=CARTESIAN_POINT('Ctrl Pts',(-18.0985494388948,16.2473946653896,
-13.6045057678968));
#118287=CARTESIAN_POINT('Ctrl Pts',(-20.881965749242,17.0725432819383,-13.7316815745783));
#118288=CARTESIAN_POINT('Ctrl Pts',(-21.6947568024494,19.8595932097158,
-13.8588573812597));
#118289=CARTESIAN_POINT('Ctrl Pts',(-19.7912372547015,22.0515991238136,
-13.9860331879411));
#118290=CARTESIAN_POINT('Ctrl Pts',(-16.9177681453095,21.6375316492779,
-14.1132089946226));
#118291=CARTESIAN_POINT('Ctrl Pts',(-15.7105790345338,18.9972719940692,
-14.240384801304));
#118292=CARTESIAN_POINT('Ctrl Pts',(-17.2771910049047,16.5530945188459,
-14.3675606079854));
#118293=CARTESIAN_POINT('Ctrl Pts',(-20.1803348085118,16.5473803543624,
-14.4947364146669));
#118294=CARTESIAN_POINT('Ctrl Pts',(-21.7565561949717,18.9853718918711,
-14.6219122213483));
#118295=CARTESIAN_POINT('Ctrl Pts',(-20.55976987354,21.6303632145285,-14.7490880280298));
#118296=CARTESIAN_POINT('Ctrl Pts',(-17.6879530131938,22.0557389504721,
-14.8762638347112));
#118297=CARTESIAN_POINT('Ctrl Pts',(-15.7758193382441,19.8712432637697,
-15.0034396413926));
#118298=CARTESIAN_POINT('Ctrl Pts',(-16.5776328150568,17.081015361877,-15.130615448074));
#118299=CARTESIAN_POINT('Ctrl Pts',(-19.3577793448131,16.2449161637061,
-15.2577912547555));
#118300=CARTESIAN_POINT('Ctrl Pts',(-21.5656470418159,18.1300147894097,
-15.3849670614369));
#118301=CARTESIAN_POINT('Ctrl Pts',(-21.1756543297891,21.0068502523211,
-15.5121428681183));
#118302=CARTESIAN_POINT('Ctrl Pts',(-18.5455953163398,22.2361045717652,
-15.6393186747998));
#118303=CARTESIAN_POINT('Ctrl Pts',(-16.0883859064352,20.6900132057797,
-15.7664944814812));
#118304=CARTESIAN_POINT('Ctrl Pts',(-16.0583632220467,17.7870190214039,
-15.8936702881626));
#118305=CARTESIAN_POINT('Ctrl Pts',(-18.4830712126828,16.1904390026627,
-16.0208460948441));
#118306=CARTESIAN_POINT('Ctrl Pts',(-21.1379907912855,17.3650362218196,
-16.1480219015255));
#118307=CARTESIAN_POINT('Ctrl Pts',(-21.5873980273797,20.2331906340233,
-16.2751977082069));
#118308=CARTESIAN_POINT('Ctrl Pts',(-19.418989675208,22.1635485838168,-16.4023735148884));
#118309=CARTESIAN_POINT('Ctrl Pts',(-16.622145811287,21.3851264637907,-16.5295493215698));
#118310=CARTESIAN_POINT('Ctrl Pts',(-15.7627970890565,18.6120782547437,
-16.6567251282513));
#118311=CARTESIAN_POINT('Ctrl Pts',(-17.629342623966,16.3885035736934,-16.7839009349327));
#118312=CARTESIAN_POINT('Ctrl Pts',(-20.5093427386175,16.7543941798941,
-16.9110767416142));
#118313=CARTESIAN_POINT('Ctrl Pts',(-21.7605760807848,19.374068151889,-17.0382525482955));
#118314=CARTESIAN_POINT('Ctrl Pts',(-20.2351137193294,21.8441372156765,
-17.165428354977));
#118315=CARTESIAN_POINT('Ctrl Pts',(-17.3324726900139,21.8984663150084,
-17.2926041616584));
#118316=CARTESIAN_POINT('Ctrl Pts',(-15.7156459790158,19.4872118732907,
-17.4197799683399));
#118317=CARTESIAN_POINT('Ctrl Pts',(-16.8679717420912,16.8225501814725,
-17.5469557750213));
#118318=CARTESIAN_POINT('Ctrl Pts',(-19.7322626130239,16.3491429542363,
-17.6741315817028));
#118319=CARTESIAN_POINT('Ctrl Pts',(-21.6807094956696,18.501311939612,-17.8013073883841));
#118320=CARTESIAN_POINT('Ctrl Pts',(-20.925733309462,21.3045756721762,-17.9284831950656));
#118321=CARTESIAN_POINT('Ctrl Pts',(-18.1599778461229,22.1871136674968,
-18.055659001747));
#118322=CARTESIAN_POINT('Ctrl Pts',(-15.9208520811544,20.3392520913025,
-18.1828348084285));
#118323=CARTESIAN_POINT('Ctrl Pts',(-16.2626149280343,17.4562892486245,
-18.3100106151099));
#118324=CARTESIAN_POINT('Ctrl Pts',(-18.8717201870645,16.1831646105782,
-18.4371864217913));
#118325=CARTESIAN_POINT('Ctrl Pts',(-21.3544757221902,17.6878910139056,
-18.5643622284728));
#118326=CARTESIAN_POINT('Ctrl Pts',(-21.4331074275647,20.5899753767109,
-18.6915380351542));
#118327=CARTESIAN_POINT('Ctrl Pts',(-19.0354755930861,22.226935421132,-18.8187138418356));
#118328=CARTESIAN_POINT('Ctrl Pts',(-16.3612586147209,21.0969619050252,
-18.9458896485171));
#118329=CARTESIAN_POINT('Ctrl Pts',(-15.8638845863206,18.2367354003361,
-19.0730654551985));
#118330=CARTESIAN_POINT('Ctrl Pts',(-17.9996633145444,16.2703361898353,
-19.20024126188));
#118331=CARTESIAN_POINT('Ctrl Pts',(-20.8091503658403,17.0018135191641,
-19.3274170685614));
#118332=CARTESIAN_POINT('Ctrl Pts',(-21.7148157697857,19.7600823036045,
-19.4545928752428));
#118333=CARTESIAN_POINT('Ctrl Pts',(-19.8857676864347,22.0146021996221,
-19.5817686819242));
#118334=CARTESIAN_POINT('Ctrl Pts',(-17.000044293062,21.6969910014797,-19.7089444886057));
#118335=CARTESIAN_POINT('Ctrl Pts',(-15.7051175323933,19.0986375254879,
-19.8361202952871));
#118336=CARTESIAN_POINT('Ctrl Pts',(-17.1890026482639,16.6033693221106,
-19.9632961019685));
#118337=CARTESIAN_POINT('Ctrl Pts',(-20.0903265437325,16.500441041753,-20.09047190865));
#118338=CARTESIAN_POINT('Ctrl Pts',(-21.7473057839905,18.8842811671185,
-20.2176477153314));
#118339=CARTESIAN_POINT('Ctrl Pts',(-20.6397625190695,21.5678678598662,
-20.3448235220129));
#118340=CARTESIAN_POINT('Ctrl Pts',(-17.7838032706328,22.0891701106396,
-20.4719993286943));
#118341=CARTESIAN_POINT('Ctrl Pts',(-15.7995850674674,19.9699385269971,
-20.5991751353757));
#118342=CARTESIAN_POINT('Ctrl Pts',(-16.5075209908883,17.1544113723013,
-20.7263509420572));
#118343=CARTESIAN_POINT('Ctrl Pts',(-19.2580928720921,16.2257085824946,
-20.8535267487386));
#118344=CARTESIAN_POINT('Ctrl Pts',(-21.5278812718072,18.035763821068,-20.98070255542));
#118345=CARTESIAN_POINT('Ctrl Pts',(-21.2343814736919,20.9241439362665,
-21.1078783621014));
#118346=CARTESIAN_POINT('Ctrl Pts',(-18.6470824304151,22.2405922216597,
-21.2350541687829));
#118347=CARTESIAN_POINT('Ctrl Pts',(-16.1392443426422,20.7780182314605,
-21.3622299754643));
#118348=CARTESIAN_POINT('Ctrl Pts',(-16.0124742037318,17.8769529674671,
-21.4894057821458));
#118349=CARTESIAN_POINT('Ctrl Pts',(-18.381492069836,16.2014330842265,-21.6165815888272));
#118350=CARTESIAN_POINT('Ctrl Pts',(-21.0759343030523,17.2838114902333,
-21.7437573955087));
#118351=CARTESIAN_POINT('Ctrl Pts',(-21.6178060723068,20.1407222466758,
-21.87093320219));
#118352=CARTESIAN_POINT('Ctrl Pts',(-20.221009817676,21.4665545621232,-21.955717073311));
#118353=CARTESIAN_POINT('Ctrl Pts',(-19.3965839026516,21.687158879832,-21.9981090088715));
#118354=CARTESIAN_POINT('Ctrl Pts',(-17.1140743056112,20.5739122292573,
2.77555756156289E-16));
#118355=CARTESIAN_POINT('Ctrl Pts',(-17.0603911325521,20.522111673172,4.45182444894629E-15));
#118356=CARTESIAN_POINT('Ctrl Pts',(-17.0098645202578,20.4674385257497,
-9.9671288295164E-15));
#118357=CARTESIAN_POINT('Ctrl Pts',(-16.9624881995608,20.410264093257,4.69416172599324E-15));
#118358=CARTESIAN_POINT('Ctrl Pts',(-16.9134245654303,20.3510533863855,
1.9877615930799E-14));
#118359=CARTESIAN_POINT('Ctrl Pts',(-16.8677391100127,20.2891596196004,
4.01703270921356E-15));
#118360=CARTESIAN_POINT('Ctrl Pts',(-16.8254532095188,20.2249455930833,
3.11556336285435E-15));
#118361=CARTESIAN_POINT('Ctrl Pts',(-16.7853187213443,20.1639986330379,
2.25995876655715E-15));
#118362=CARTESIAN_POINT('Ctrl Pts',(-16.7482466106952,20.1009605704099,
1.9879857987986E-14));
#118363=CARTESIAN_POINT('Ctrl Pts',(-16.7142836213594,20.0361088469222,
1.85268467234323E-14));
#118364=CARTESIAN_POINT('Ctrl Pts',(-16.6991853089609,20.0072788881953,
1.79420105219681E-14));
#118365=CARTESIAN_POINT('Ctrl Pts',(-16.6847018341336,19.9780901364722,
-8.23592356720746E-15));
#118366=CARTESIAN_POINT('Ctrl Pts',(-16.6708392964776,19.9485654278612,
1.03597685985335E-14));
#118367=CARTESIAN_POINT('Ctrl Pts',(-16.6640109607001,19.9340223024153,
1.9174859491606E-14));
#118368=CARTESIAN_POINT('Ctrl Pts',(-16.657333302533,19.9193976511972,3.18705451808171E-15));
#118369=CARTESIAN_POINT('Ctrl Pts',(-16.6508071688394,19.9046941363876,
-4.62824223390612E-15));
#118370=CARTESIAN_POINT('Ctrl Pts',(-16.6447949816305,19.8911485536865,
-1.19254541885051E-14));
#118371=CARTESIAN_POINT('Ctrl Pts',(-16.6389109256811,19.8775346474983,
3.85423458197671E-15));
#118372=CARTESIAN_POINT('Ctrl Pts',(-16.6331636045017,19.8638740397009,
6.02989880249538E-15));
#118373=CARTESIAN_POINT('Ctrl Pts',(-16.6020948019513,19.790027683611,1.85394696934408E-14));
#118374=CARTESIAN_POINT('Ctrl Pts',(-16.5749612060018,19.7146929635301,
8.98167354597479E-15));
#118375=CARTESIAN_POINT('Ctrl Pts',(-16.5517844460822,19.6382510185693,
1.35030875370035E-14));
#118376=CARTESIAN_POINT('Ctrl Pts',(-16.5281813102644,19.5604027940833,
1.81076806245845E-14));
#118377=CARTESIAN_POINT('Ctrl Pts',(-16.5086814210928,19.4814054223285,
2.71946254420182E-14));
#118378=CARTESIAN_POINT('Ctrl Pts',(-16.4933485190229,19.4016259047529,
7.14706072102445E-15));
#118379=CARTESIAN_POINT('Ctrl Pts',(-16.4794162838085,19.3291342786354,
-1.10691507889412E-14));
#118380=CARTESIAN_POINT('Ctrl Pts',(-16.4689247639322,19.2559959244269,
1.02006884852949E-14));
#118381=CARTESIAN_POINT('Ctrl Pts',(-16.4619555680579,19.1824703462648,
1.64729341278758E-14));
#118382=CARTESIAN_POINT('Ctrl Pts',(-16.4592976470201,19.1544290650995,
1.9131180430237E-14));
#118383=CARTESIAN_POINT('Ctrl Pts',(-16.4571524088489,19.1263313551069,
2.39160590086535E-14));
#118384=CARTESIAN_POINT('Ctrl Pts',(-16.4555257409501,19.0981913259617,
-4.73232564246473E-15));
#118385=CARTESIAN_POINT('Ctrl Pts',(-16.4546322610198,19.0827348512285,
-2.03445886243926E-14));
#118386=CARTESIAN_POINT('Ctrl Pts',(-16.453895246137,19.0672656072016,-8.75022012521963E-16));
#118387=CARTESIAN_POINT('Ctrl Pts',(-16.4533157740873,19.051785924702,1.26981758441502E-14));
#118388=CARTESIAN_POINT('Ctrl Pts',(-16.4528680721876,19.0398262740765,
2.31564174349633E-14));
#118389=CARTESIAN_POINT('Ctrl Pts',(-16.452514580052,19.0278636904617,5.25880506684687E-15));
#118390=CARTESIAN_POINT('Ctrl Pts',(-16.4522557186358,19.0159077924821,
5.49560397189452E-15));
#118391=CARTESIAN_POINT('Ctrl Pts',(-16.4504488747983,18.9324560332097,
7.08905735160161E-15));
#118392=CARTESIAN_POINT('Ctrl Pts',(-16.4532438607103,18.8492105138102,
6.08038579602206E-16));
#118393=CARTESIAN_POINT('Ctrl Pts',(-16.4606969184041,18.7665518702536,
4.14945855453652E-15));
#118394=CARTESIAN_POINT('Ctrl Pts',(-16.4681357553308,18.6840509430821,
7.10329836543544E-15));
#118395=CARTESIAN_POINT('Ctrl Pts',(-16.4802145308229,18.6021336503298,
7.4706047686461E-15));
#118396=CARTESIAN_POINT('Ctrl Pts',(-16.4970385284052,18.5211628277987,
4.55191440096314E-15));
#118397=CARTESIAN_POINT('Ctrl Pts',(-16.5134762563069,18.4420510505752,
2.05501660863705E-15));
#118398=CARTESIAN_POINT('Ctrl Pts',(-16.5344435942651,18.3638418295306,
-1.67546161971538E-14));
#118399=CARTESIAN_POINT('Ctrl Pts',(-16.5596748813382,18.2867616450374,
-2.91433543964104E-15));
#118400=CARTESIAN_POINT('Ctrl Pts',(-16.5700722924092,18.2549981301094,
2.76440958040333E-15));
#118401=CARTESIAN_POINT('Ctrl Pts',(-16.581194395652,18.2234264109971,1.53541667197338E-14));
#118402=CARTESIAN_POINT('Ctrl Pts',(-16.5930250854222,18.1920628114276,
1.10467190950203E-14));
#118403=CARTESIAN_POINT('Ctrl Pts',(-16.5995763500233,18.1746951647716,
8.82295792525399E-15));
#118404=CARTESIAN_POINT('Ctrl Pts',(-16.6063471420461,18.1573861965041,
1.49165270495576E-14));
#118405=CARTESIAN_POINT('Ctrl Pts',(-16.6133223339605,18.1401687566555,
1.25455201782643E-14));
#118406=CARTESIAN_POINT('Ctrl Pts',(-16.6442815008621,18.0637496988806,
1.85388435652528E-15));
#118407=CARTESIAN_POINT('Ctrl Pts',(-16.6792965711232,17.9890373934243,
2.44510841382609E-16));
#118408=CARTESIAN_POINT('Ctrl Pts',(-16.7180395276146,17.9162554524269,
3.63598040564739E-15));
#118409=CARTESIAN_POINT('Ctrl Pts',(-16.7588464280445,17.8395962170884,
7.20812288916674E-15));
#118410=CARTESIAN_POINT('Ctrl Pts',(-16.8037890252177,17.7650776476886,
-8.42604220156098E-15));
#118411=CARTESIAN_POINT('Ctrl Pts',(-16.8525445311818,17.692966664072,-1.04360964314765E-14));
#118412=CARTESIAN_POINT('Ctrl Pts',(-16.9013000371459,17.6208556804554,
-1.2446150661392E-14));
#118413=CARTESIAN_POINT('Ctrl Pts',(-16.9538690505405,17.5511513968607,
1.86312228584609E-14));
#118414=CARTESIAN_POINT('Ctrl Pts',(-17.0099820350415,17.4841394296583,
-2.55351295663786E-15));
#118415=CARTESIAN_POINT('Ctrl Pts',(-17.0318957421493,17.4579693616242,
-1.0746443255118E-14));
#118416=CARTESIAN_POINT('Ctrl Pts',(-17.0543504737559,17.4322101781547,
-7.53714155281239E-18));
#118417=CARTESIAN_POINT('Ctrl Pts',(-17.0773320757735,17.4068801208169,
7.21644966006352E-16));
#118418=CARTESIAN_POINT('Ctrl Pts',(-17.0864638250902,17.3968152117818,
1.04464455640109E-15));
#118419=CARTESIAN_POINT('Ctrl Pts',(-17.0956795264284,17.3868172601505,
1.08622188611639E-14));
#118420=CARTESIAN_POINT('Ctrl Pts',(-17.1049759845535,17.376889953632,9.32587340685131E-15));
#118421=CARTESIAN_POINT('Ctrl Pts',(-17.1654855522993,17.3122742668584,
-1.28932407812809E-15));
#118422=CARTESIAN_POINT('Ctrl Pts',(-17.2292149096655,17.2508596682763,
-5.87214431812852E-15));
#118423=CARTESIAN_POINT('Ctrl Pts',(-17.2958559710253,17.1929205201455,
-8.43769498715119E-15));
#118424=CARTESIAN_POINT('Ctrl Pts',(-17.3510488277484,17.1449346832427,
-1.05625121434475E-14));
#118425=CARTESIAN_POINT('Ctrl Pts',(-17.4082400420401,17.099332805993,-4.53394044041895E-15));
#118426=CARTESIAN_POINT('Ctrl Pts',(-17.467277750751,17.0562847197858,6.7168492989822E-15));
#118427=CARTESIAN_POINT('Ctrl Pts',(-17.4867746862249,17.042068284606,1.03075517856999E-14));
#118428=CARTESIAN_POINT('Ctrl Pts',(-17.5064731567169,17.0281304980274,
1.80459611682673E-14));
#118429=CARTESIAN_POINT('Ctrl Pts',(-17.5263681208433,17.0144778848536,
3.1641356201817E-15));
#118430=CARTESIAN_POINT('Ctrl Pts',(-17.5422931383847,17.0035495864712,
-8.70945017928273E-15));
#118431=CARTESIAN_POINT('Ctrl Pts',(-17.5583454202066,16.9928032530657,
3.52998690900286E-15));
#118432=CARTESIAN_POINT('Ctrl Pts',(-17.5745064361378,16.9822524120729,
5.10702591327572E-15));
#118433=CARTESIAN_POINT('Ctrl Pts',(-17.6490341987622,16.9335964008203,
1.25639560294472E-14));
#118434=CARTESIAN_POINT('Ctrl Pts',(-17.7259441000136,16.8890440749741,
4.67377112410806E-15));
#118435=CARTESIAN_POINT('Ctrl Pts',(-17.8049552753632,16.8488860377447,
8.13238365537927E-15));
#118436=CARTESIAN_POINT('Ctrl Pts',(-17.8827964927913,16.8093226406223,
1.16249942035744E-14));
#118437=CARTESIAN_POINT('Ctrl Pts',(-17.9626778959223,16.774023635519,1.251775654464E-14));
#118438=CARTESIAN_POINT('Ctrl Pts',(-18.0443633532837,16.7433042678249,
-2.16493489801906E-14));
#118439=CARTESIAN_POINT('Ctrl Pts',(-18.0530581203136,16.7400344355435,
-2.53480777024185E-14));
#118440=CARTESIAN_POINT('Ctrl Pts',(-18.0617733522417,16.7368165315127,
1.30580969649654E-14));
#118441=CARTESIAN_POINT('Ctrl Pts',(-18.0705086335888,16.7336504254972,
-1.0769163338864E-14));
#118442=CARTESIAN_POINT('Ctrl Pts',(-19.3965839091051,16.7348410960496,
-0.00189100554319391));
#118443=CARTESIAN_POINT('Ctrl Pts',(-20.2210098321597,16.9554454159071,
-0.044282941103672));
#118444=CARTESIAN_POINT('Ctrl Pts',(-21.6178061486211,18.2812774518108,
-0.129066812224628));
#118445=CARTESIAN_POINT('Ctrl Pts',(-21.0759342831862,21.1381886893359,
-0.256242618906062));
#118446=CARTESIAN_POINT('Ctrl Pts',(-18.3814920744256,22.2205668231227,
-0.383418425587496));
#118447=CARTESIAN_POINT('Ctrl Pts',(-16.012474196746,20.5450470987711,-0.510594232268932));
#118448=CARTESIAN_POINT('Ctrl Pts',(-16.139244329641,17.6439817266502,-0.637770038950364));
#118449=CARTESIAN_POINT('Ctrl Pts',(-18.647082433769,16.1814077892925,-0.764945845631801));
#118450=CARTESIAN_POINT('Ctrl Pts',(-21.2343814795738,17.4978560455519,
-0.892121652313232));
#118451=CARTESIAN_POINT('Ctrl Pts',(-21.5278812831845,20.386236189992,-1.01929745899467));
#118452=CARTESIAN_POINT('Ctrl Pts',(-19.2580928727389,22.1962914237501,
-1.14647326567611));
#118453=CARTESIAN_POINT('Ctrl Pts',(-16.5075209839662,21.267588636987,-1.27364907235753));
#118454=CARTESIAN_POINT('Ctrl Pts',(-15.7995850569884,18.4520614691495,
-1.40082487903898));
#118455=CARTESIAN_POINT('Ctrl Pts',(-17.7838032676266,16.3328298801955,
-1.52800068572041));
#118456=CARTESIAN_POINT('Ctrl Pts',(-20.6397625254543,16.8541321316718,
-1.65517649240185));
#118457=CARTESIAN_POINT('Ctrl Pts',(-21.747305794399,19.5377188342137,-1.78235229908328));
#118458=CARTESIAN_POINT('Ctrl Pts',(-20.0903265483327,21.9215589674176,
-1.90952810576472));
#118459=CARTESIAN_POINT('Ctrl Pts',(-17.1890026429968,21.8186306868887,
-2.03670391244613));
#118460=CARTESIAN_POINT('Ctrl Pts',(-15.7051175219999,19.3233624748623,
-2.16387971912758));
#118461=CARTESIAN_POINT('Ctrl Pts',(-17.0000442871287,16.7250089900212,
-2.29105552580901));
#118462=CARTESIAN_POINT('Ctrl Pts',(-19.8857676903764,16.4073977907608,
-2.41823133249045));
#118463=CARTESIAN_POINT('Ctrl Pts',(-21.714815780002,18.6619176945194,-2.54540713917187));
#118464=CARTESIAN_POINT('Ctrl Pts',(-20.8091503729495,21.4201864884025,
-2.67258294585332));
#118465=CARTESIAN_POINT('Ctrl Pts',(-17.9996633120291,22.1516638202427,
-2.79975875253474));
#118466=CARTESIAN_POINT('Ctrl Pts',(-15.8638845764857,20.1852646030015,
-2.92693455921619));
#118467=CARTESIAN_POINT('Ctrl Pts',(-16.3612586065906,17.3250380885132,
-3.05411036589761));
#118468=CARTESIAN_POINT('Ctrl Pts',(-19.0354755941188,16.1950645685336,
-3.18128617257904));
#118469=CARTESIAN_POINT('Ctrl Pts',(-21.4331074368131,17.832024618564,-3.30846197926049));
#118470=CARTESIAN_POINT('Ctrl Pts',(-21.3544757311695,20.7341089913131,
-3.43563778594193));
#118471=CARTESIAN_POINT('Ctrl Pts',(-18.8717201875366,22.2388353997967,
-3.56281359262336));
#118472=CARTESIAN_POINT('Ctrl Pts',(-16.2626149195662,20.9657107573881,
-3.68998939930478));
#118473=CARTESIAN_POINT('Ctrl Pts',(-15.9208520715149,18.0827479048318,
-3.81716520598622));
#118474=CARTESIAN_POINT('Ctrl Pts',(-18.1599778441558,16.2348863223055,
-3.94434101266766));
#118475=CARTESIAN_POINT('Ctrl Pts',(-20.9257333169718,17.11742432065,-4.0715168193491));
#118476=CARTESIAN_POINT('Ctrl Pts',(-21.6807095057666,19.9206880628195,
-4.19869262603053));
#118477=CARTESIAN_POINT('Ctrl Pts',(-19.7322626164446,22.0728570555698,
-4.32586843271195));
#118478=CARTESIAN_POINT('Ctrl Pts',(-16.8679717356974,21.5994498267117,
-4.4530442393934));
#118479=CARTESIAN_POINT('Ctrl Pts',(-15.7156459686732,18.934788125763,-4.58022004607482));
#118480=CARTESIAN_POINT('Ctrl Pts',(-17.3324726852114,16.5235336757831,
-4.70739585275626));
#118481=CARTESIAN_POINT('Ctrl Pts',(-20.2351137244727,16.5778627753009,
-4.8345716594377));
#118482=CARTESIAN_POINT('Ctrl Pts',(-21.7605760911555,19.0479318475521,
-4.96174746611912));
#118483=CARTESIAN_POINT('Ctrl Pts',(-20.5093427447009,21.6676058285233,
-5.08892327280056));
#118484=CARTESIAN_POINT('Ctrl Pts',(-17.6293426201811,22.033496435978,-5.216099079482));
#118485=CARTESIAN_POINT('Ctrl Pts',(-15.7627970788757,19.8099217473088,
-5.34327488616344));
#118486=CARTESIAN_POINT('Ctrl Pts',(-16.6221458040505,17.0368735287597,
-5.47045069284487));
#118487=CARTESIAN_POINT('Ctrl Pts',(-19.4189896775549,16.2584514060663,
-5.59762649952629));
#118488=CARTESIAN_POINT('Ctrl Pts',(-21.5873980371568,18.1888093624738,
-5.72480230620775));
#118489=CARTESIAN_POINT('Ctrl Pts',(-21.1379907995229,21.0569637845056,
-5.85197811288917));
#118490=CARTESIAN_POINT('Ctrl Pts',(-18.4830712118232,22.2315610076874,
-5.9791539195706));
#118491=CARTESIAN_POINT('Ctrl Pts',(-16.0583632128787,20.6349809834757,
-6.10632972625204));
#118492=CARTESIAN_POINT('Ctrl Pts',(-16.0883858973698,17.7319867891525,
-6.23350553293348));
#118493=CARTESIAN_POINT('Ctrl Pts',(-18.545595315694,16.1858954178693,-6.36068133961492));
#118494=CARTESIAN_POINT('Ctrl Pts',(-21.1756543381554,17.4151497415253,
-6.48785714629634));
#118495=CARTESIAN_POINT('Ctrl Pts',(-21.5656470515186,20.2919852142942,
-6.61503295297777));
#118496=CARTESIAN_POINT('Ctrl Pts',(-19.3577793469507,22.1770838464573,
-6.74220875965922));
#118497=CARTESIAN_POINT('Ctrl Pts',(-16.577632807668,21.3409846454216,-6.86938456634065));
#118498=CARTESIAN_POINT('Ctrl Pts',(-15.7758193281077,18.5507567339681,
-6.99656037302208));
#118499=CARTESIAN_POINT('Ctrl Pts',(-17.6879530096092,16.3662610397804,
-7.12373617970353));
#118500=CARTESIAN_POINT('Ctrl Pts',(-20.5597698797958,16.7916367771814,
-7.25091198638494));
#118501=CARTESIAN_POINT('Ctrl Pts',(-21.7565562053286,19.4366281089017,
-7.3780877930664));
#118502=CARTESIAN_POINT('Ctrl Pts',(-20.1803348134679,21.8746196547645,
-7.50526359974781));
#118503=CARTESIAN_POINT('Ctrl Pts',(-17.277190999913,21.8689054902615,-7.63243940642925));
#118504=CARTESIAN_POINT('Ctrl Pts',(-15.710579024174,19.4247280066634,-7.75961521311068));
#118505=CARTESIAN_POINT('Ctrl Pts',(-16.917768139086,16.7844683424076,-7.88679101979213));
#118506=CARTESIAN_POINT('Ctrl Pts',(-19.7912372583239,16.3704008664529,
-8.01396682647355));
#118507=CARTESIAN_POINT('Ctrl Pts',(-21.6947568125944,18.5624067880616,
-8.14114263315499));
#118508=CARTESIAN_POINT('Ctrl Pts',(-20.8819657566022,21.3494567253891,
-8.26831843983642));
#118509=CARTESIAN_POINT('Ctrl Pts',(-18.0985494367176,22.1746053447652,
-8.39549424651787));
#118510=CARTESIAN_POINT('Ctrl Pts',(-15.8981195681347,20.2808300024119,
-8.52267005319928));
#118511=CARTESIAN_POINT('Ctrl Pts',(-16.2994339811977,17.4055520339842,
-8.64984585988073));
#118512=CARTESIAN_POINT('Ctrl Pts',(-18.9343116103032,16.1866605156374,
-8.77702166656217));
#118513=CARTESIAN_POINT('Ctrl Pts',(-21.385415769696,17.7424127625149,-8.9041974732436));
#118514=CARTESIAN_POINT('Ctrl Pts',(-21.404010525815,20.6455026489812,-9.03137327992503));
#118515=CARTESIAN_POINT('Ctrl Pts',(-18.9730363440416,22.2325253902829,
-9.15854908660645));
#118516=CARTESIAN_POINT('Ctrl Pts',(-16.3227611528787,21.0474861230161,
-9.28572489328791));
#118517=CARTESIAN_POINT('Ctrl Pts',(-15.8846479455884,18.1775848230658,
-9.41290069996933));
#118518=CARTESIAN_POINT('Ctrl Pts',(-18.0606383974872,16.2557778069732,
-9.54007650665076));
#118519=CARTESIAN_POINT('Ctrl Pts',(-20.8543963261569,17.0452037312071,
-9.6672523133322));
#118520=CARTESIAN_POINT('Ctrl Pts',(-21.7028222322161,19.8216133075818,
-9.79442812001363));
#118521=CARTESIAN_POINT('Ctrl Pts',(-19.8275380061061,22.0378230731863,
-9.92160392669508));
#118522=CARTESIAN_POINT('Ctrl Pts',(-16.9490005320169,21.6605981215696,
-10.0487797333765));
#118523=CARTESIAN_POINT('Ctrl Pts',(-15.7080892802405,19.0360189326189,
-10.175955540058));
#118524=CARTESIAN_POINT('Ctrl Pts',(-17.2432633046432,16.5719740124406,
-10.3031313467394));
#118525=CARTESIAN_POINT('Ctrl Pts',(-20.1460957214815,16.5290716394223,
-10.4303071534208));
#118526=CARTESIAN_POINT('Ctrl Pts',(-21.7534179584053,18.9466720779869,
-10.5574829601022));
#118527=CARTESIAN_POINT('Ctrl Pts',(-20.5906116247063,21.6067769789573,
-10.6846587667837));
#118528=CARTESIAN_POINT('Ctrl Pts',(-17.7244793596526,22.0689052004239,
-10.8118345734651));
#118529=CARTESIAN_POINT('Ctrl Pts',(-15.7845196242002,19.9090827821031,
-10.9390103801465));
#118530=CARTESIAN_POINT('Ctrl Pts',(-16.5505250681459,17.1088127391066,
-11.066186186828));
#118531=CARTESIAN_POINT('Ctrl Pts',(-19.3197332403295,16.2371690315234,
-11.1933619935094));
#118532=CARTESIAN_POINT('Ctrl Pts',(-21.5515675192157,18.0938306607512,
-11.3205378001909));
#118533=CARTESIAN_POINT('Ctrl Pts',(-21.1984584771842,20.9754258193904,
-11.4477136068723));
#118534=CARTESIAN_POINT('Ctrl Pts',(-18.5843617438802,22.2382698013562,
-11.5748894135537));
#118535=CARTESIAN_POINT('Ctrl Pts',(-16.1075488229684,20.7237816341318,
-11.7020652202351));
#118536=CARTESIAN_POINT('Ctrl Pts',(-16.0403418410383,17.821410211409,-11.8292410269166));
#118537=CARTESIAN_POINT('Ctrl Pts',(-18.4443990326749,16.1939011720493,
-11.956416833598));
#118538=CARTESIAN_POINT('Ctrl Pts',(-21.1141471371691,17.3343930450618,
-12.0835926402795));
#118539=CARTESIAN_POINT('Ctrl Pts',(-21.6002579719026,20.1965553238665,
-12.2107684469609));
#118540=CARTESIAN_POINT('Ctrl Pts',(-19.4567550174485,22.1545317634858,
-12.3379442536423));
#118541=CARTESIAN_POINT('Ctrl Pts',(-16.650169193721,21.4120005062924,-12.4651200603238));
#118542=CARTESIAN_POINT('Ctrl Pts',(-15.7553687976281,18.6501878940739,
-12.5922958670052));
#118543=CARTESIAN_POINT('Ctrl Pts',(-17.593277655009,16.4028855811176,-12.7194716736866));
#118544=CARTESIAN_POINT('Ctrl Pts',(-20.4777284627055,16.7318539562487,
-12.8466474803681));
#118545=CARTESIAN_POINT('Ctrl Pts',(-21.7624166338639,19.3352849533645,
-12.9738232870495));
#118546=CARTESIAN_POINT('Ctrl Pts',(-20.268720508187,21.8246922197625,-13.1009990937309));
#118547=CARTESIAN_POINT('Ctrl Pts',(-17.3670135717459,21.9161990985631,
-13.2281749004124));
#118548=CARTESIAN_POINT('Ctrl Pts',(-15.7194318384815,19.5258537080241,
-13.3553507070938));
#118549=CARTESIAN_POINT('Ctrl Pts',(-16.8375292882087,16.846649582398,-13.4825265137753));
#118550=CARTESIAN_POINT('Ctrl Pts',(-19.6955209077569,16.3365902167848,
-13.6097023204567));
#118551=CARTESIAN_POINT('Ctrl Pts',(-21.6713767731562,18.4636234212799,
-13.7368781271381));
#118552=CARTESIAN_POINT('Ctrl Pts',(-20.9523717633484,21.2763282493288,
-13.8640539338195));
#118553=CARTESIAN_POINT('Ctrl Pts',(-18.1981483483483,22.1942225973466,
-13.991229740501));
#118554=CARTESIAN_POINT('Ctrl Pts',(-15.9355355650342,20.3751953719755,
-14.1184055471824));
#118555=CARTESIAN_POINT('Ctrl Pts',(-16.2403402085095,17.4880911509308,
-14.2455813538639));
#118556=CARTESIAN_POINT('Ctrl Pts',(-18.8329229366954,16.181648863124,-14.3727571605453));
#118557=CARTESIAN_POINT('Ctrl Pts',(-21.334750010313,17.6544482206642,-14.4999329672267));
#118558=CARTESIAN_POINT('Ctrl Pts',(-21.450550370219,20.555287225246,-14.6271087739081));
#118559=CARTESIAN_POINT('Ctrl Pts',(-19.0740843735804,22.2228261365397,
-14.7542845805896));
#118560=CARTESIAN_POINT('Ctrl Pts',(-16.3856120721985,21.1272015025705,
-14.881460387271));
#118561=CARTESIAN_POINT('Ctrl Pts',(-15.8516399371812,18.2735809228713,
-15.0086361939525));
#118562=CARTESIAN_POINT('Ctrl Pts',(-17.9620542603586,16.2799841636479,
-15.1358120006339));
#118563=CARTESIAN_POINT('Ctrl Pts',(-20.7806808873008,16.9754125149182,
-15.2629878073153));
#118564=CARTESIAN_POINT('Ctrl Pts',(-21.7216048314868,19.7218536275428,
-15.3901636139968));
#118565=CARTESIAN_POINT('Ctrl Pts',(-19.9215867744523,21.999618244049,-15.5173394206782));
#118566=CARTESIAN_POINT('Ctrl Pts',(-17.0320315618059,21.7189987028083,
-15.6445152273596));
#118567=CARTESIAN_POINT('Ctrl Pts',(-15.7039267551279,19.1374460156962,
-15.771691034041));
#118568=CARTESIAN_POINT('Ctrl Pts',(-17.1557260830642,16.6233745439076,
-15.8988668407225));
#118569=CARTESIAN_POINT('Ctrl Pts',(-20.0554937710623,16.483288821935,-16.0260426474039));
#118570=CARTESIAN_POINT('Ctrl Pts',(-21.7428729452643,18.8457088049877,
-16.1532184540854));
#118571=CARTESIAN_POINT('Ctrl Pts',(-20.669797943903,21.5432607869357,-16.2803942607668));
#118572=CARTESIAN_POINT('Ctrl Pts',(-17.8207484781814,22.1011082533001,
-16.4075700674482));
#118573=CARTESIAN_POINT('Ctrl Pts',(-15.8095506009463,20.0074607776102,
-16.5347458741296));
#118574=CARTESIAN_POINT('Ctrl Pts',(-16.4813535355424,17.1831099723939,
-16.6619216808111));
#118575=CARTESIAN_POINT('Ctrl Pts',(-19.2198197862706,16.2192224024562,
-16.7890974874925));
#118576=CARTESIAN_POINT('Ctrl Pts',(-21.5125765364721,18.0001050876052,
-16.916273294174));
#118577=CARTESIAN_POINT('Ctrl Pts',(-21.2561617723699,20.891908698262,-17.0434491008554));
#118578=CARTESIAN_POINT('Ctrl Pts',(-18.6858201251326,22.2415829072234,
-17.1706249075368));
#118579=CARTESIAN_POINT('Ctrl Pts',(-16.1596805227059,20.8108853979961,
-17.2978007142183));
#118580=CARTESIAN_POINT('Ctrl Pts',(-15.9953192604098,17.9123923361942,
-17.4249765208997));
#118581=CARTESIAN_POINT('Ctrl Pts',(-18.3435275949907,16.2052912052522,
-17.5521523275811));
#118582=CARTESIAN_POINT('Ctrl Pts',(-21.0499701257169,17.2557413381646,
-17.6793281342626));
#118583=CARTESIAN_POINT('Ctrl Pts',(-21.6316538114152,20.1000199362705,
-17.806503940944));
#118584=CARTESIAN_POINT('Ctrl Pts',(-19.5549199738189,22.1286779216513,
-17.9336797476255));
#118585=CARTESIAN_POINT('Ctrl Pts',(-16.7250430122834,21.4805475054267,
-18.0608555543069));
#118586=CARTESIAN_POINT('Ctrl Pts',(-15.7382593970452,18.7502481169883,
-18.1880313609883));
#118587=CARTESIAN_POINT('Ctrl Pts',(-17.4998818483857,16.4426599837058,
-18.3152071676697));
#118588=CARTESIAN_POINT('Ctrl Pts',(-20.3937311058227,16.6748519928531,
-18.4423829743512));
#118589=CARTESIAN_POINT('Ctrl Pts',(-21.7648800881945,19.2338023873838,
-18.5695587810326));
#118590=CARTESIAN_POINT('Ctrl Pts',(-20.355384707288,21.7718330069121,-18.6967345877141));
#118591=CARTESIAN_POINT('Ctrl Pts',(-17.458369491917,21.9604582855383,-18.8239103943955));
#118592=CARTESIAN_POINT('Ctrl Pts',(-15.7316660931769,19.6266262383536,
-18.9510862010769));
#118593=CARTESIAN_POINT('Ctrl Pts',(-16.7594177080439,16.911482913106,-19.0782620077583));
#118594=CARTESIAN_POINT('Ctrl Pts',(-19.5987260194682,16.3060037929748,
-19.2054378144398));
#118595=CARTESIAN_POINT('Ctrl Pts',(-21.6447018788134,18.3656783845019,
-19.3326136211212));
#118596=CARTESIAN_POINT('Ctrl Pts',(-21.0202894232019,21.2008830991641,
-19.4597894278026));
#118597=CARTESIAN_POINT('Ctrl Pts',(-18.298348324308,22.2104935619801,-19.5869652344841));
#118598=CARTESIAN_POINT('Ctrl Pts',(-15.9760905994637,20.468254879066,-19.7141410411655));
#118599=CARTESIAN_POINT('Ctrl Pts',(-16.1840435721468,17.5725628250383,
-19.841316847847));
#118600=CARTESIAN_POINT('Ctrl Pts',(-18.7314233036762,16.1800352894614,
-19.9684926545284));
#118601=CARTESIAN_POINT('Ctrl Pts',(-21.2811669856061,17.5682295538539,
-20.0956684612098));
#118602=CARTESIAN_POINT('Ctrl Pts',(-21.4940430697286,20.4635641243438,
-20.2228442678912));
#118603=CARTESIAN_POINT('Ctrl Pts',(-19.1747509132239,22.2097481144726,
-20.3500200745727));
#118604=CARTESIAN_POINT('Ctrl Pts',(-16.4510972110931,21.2047682572431,
-20.4771958812541));
#118605=CARTESIAN_POINT('Ctrl Pts',(-15.821865006984,18.370627026472,-20.6043716879356));
#118606=CARTESIAN_POINT('Ctrl Pts',(-17.8643361386242,16.3074811285329,
-20.731547494617));
#118607=CARTESIAN_POINT('Ctrl Pts',(-20.7046694479571,16.9081233905683,
-20.8587233012984));
#118608=CARTESIAN_POINT('Ctrl Pts',(-21.7370366957551,19.6215316486842,
-20.9858991079799));
#118609=CARTESIAN_POINT('Ctrl Pts',(-20.0143025394107,21.9582647545422,
-21.1130749146613));
#118610=CARTESIAN_POINT('Ctrl Pts',(-17.1169733995614,21.7746258892963,
-21.2402507213427));
#118611=CARTESIAN_POINT('Ctrl Pts',(-15.7031597664495,19.2388788584707,
-21.3674265280241));
#118612=CARTESIAN_POINT('Ctrl Pts',(-17.0699655633607,16.6778255053829,
-21.4946023347056));
#118613=CARTESIAN_POINT('Ctrl Pts',(-19.9633972500118,16.4402806602733,
-21.621778141387));
#118614=CARTESIAN_POINT('Ctrl Pts',(-21.7289765870023,18.7457048218335,
-21.7489539480685));
#118615=CARTESIAN_POINT('Ctrl Pts',(-20.7467662613402,21.4760665062299,
-21.8761297547499));
#118616=CARTESIAN_POINT('Ctrl Pts',(-17.9181406714293,22.1321446364483,
-22.0033055614313));
#118617=CARTESIAN_POINT('Ctrl Pts',(-15.8372831342433,20.1003769378317,
-22.1305000254672));
#118618=CARTESIAN_POINT('Ctrl Pts',(-16.2233209291158,18.2129921341989,
-22.2153025539425));
#118619=CARTESIAN_POINT('Ctrl Pts',(-16.7733106534418,17.5599162528134,
-22.2577131468574));
#118620=CARTESIAN_POINT('Ctrl Pts',(-19.3578031414673,16.879769673048,0.0847273919817681));
#118621=CARTESIAN_POINT('Ctrl Pts',(-20.133975749406,17.0874621114807,0.04233545642129));
#118622=CARTESIAN_POINT('Ctrl Pts',(-21.4490181436218,18.3356937357163,
-0.0424484146996662));
#118623=CARTESIAN_POINT('Ctrl Pts',(-20.9388618188364,21.0253911164874,
-0.1696242213811));
#118624=CARTESIAN_POINT('Ctrl Pts',(-18.402124220429,22.0444180968188,-0.296800028062535));
#118625=CARTESIAN_POINT('Ctrl Pts',(-16.1717639989072,20.466965862803,-0.423975834743969));
#118626=CARTESIAN_POINT('Ctrl Pts',(-16.291114327307,17.7356986710373,-0.551151641425403));
#118627=CARTESIAN_POINT('Ctrl Pts',(-18.6521696836906,16.3587285934148,
-0.678327448106839));
#118628=CARTESIAN_POINT('Ctrl Pts',(-21.0880351650422,17.5981256668252,
-0.80550325478827));
#118629=CARTESIAN_POINT('Ctrl Pts',(-21.3643565441105,20.3174500921447,
-0.932679061469707));
#118630=CARTESIAN_POINT('Ctrl Pts',(-19.2274179293257,22.0215635267321,
-1.05985486815114));
#118631=CARTESIAN_POINT('Ctrl Pts',(-16.6378358983264,21.1472173376516,
-1.18703067483258));
#118632=CARTESIAN_POINT('Ctrl Pts',(-15.9713351742103,18.4964818337432,
-1.31420648151401));
#118633=CARTESIAN_POINT('Ctrl Pts',(-17.8394178972337,16.5012880107125,
-1.44138228819545));
#118634=CARTESIAN_POINT('Ctrl Pts',(-20.5282190172933,16.9920786527069,
-1.56855809487688));
#118635=CARTESIAN_POINT('Ctrl Pts',(-21.5709382276219,19.5185961132746,
-1.69573390155831));
#118636=CARTESIAN_POINT('Ctrl Pts',(-20.0109413052122,21.7629110497128,
-1.82290970823975));
#118637=CARTESIAN_POINT('Ctrl Pts',(-17.2794307120758,21.6660071197238,
-1.95008551492118));
#118638=CARTESIAN_POINT('Ctrl Pts',(-15.8823967857546,19.316785944752,-2.07726132160262));
#118639=CARTESIAN_POINT('Ctrl Pts',(-17.101532012187,16.8705130362003,-2.20443712828405));
#118640=CARTESIAN_POINT('Ctrl Pts',(-19.8183551942992,16.5714914916967,
-2.33161293496548));
#118641=CARTESIAN_POINT('Ctrl Pts',(-21.5403498405985,18.6940552593023,
-2.45878874164692));
#118642=CARTESIAN_POINT('Ctrl Pts',(-20.6876926627317,21.2908836986755,
-2.58596454832835));
#118643=CARTESIAN_POINT('Ctrl Pts',(-18.0426437407308,21.9795479587692,
-2.71314035500979));
#118644=CARTESIAN_POINT('Ctrl Pts',(-16.0318712688937,20.128241290682,-2.84031616169122));
#118645=CARTESIAN_POINT('Ctrl Pts',(-16.5001341986149,17.4354226747645,
-2.96749196837266));
#118646=CARTESIAN_POINT('Ctrl Pts',(-19.0178303497907,16.3715860469025,
-3.09466777505409));
#118647=CARTESIAN_POINT('Ctrl Pts',(-21.275129772553,17.9127354887059,-3.22184358173553));
#118648=CARTESIAN_POINT('Ctrl Pts',(-21.2011003487691,20.6449620394061,
-3.34901938841696));
#118649=CARTESIAN_POINT('Ctrl Pts',(-18.8636594807816,22.0616174211049,
-3.4761951950984));
#118650=CARTESIAN_POINT('Ctrl Pts',(-16.4072640866091,20.8630082479868,
-3.60337100177983));
#118651=CARTESIAN_POINT('Ctrl Pts',(-16.0855044795293,18.1487840426529,
-3.73054680846126));
#118652=CARTESIAN_POINT('Ctrl Pts',(-18.1935751282717,16.4090770495669,
-3.8577226151427));
#118653=CARTESIAN_POINT('Ctrl Pts',(-20.7974520542944,17.2399604565832,
-3.98489842182413));
#118654=CARTESIAN_POINT('Ctrl Pts',(-21.50823979277,19.8791503081571,-4.11207422850556));
#118655=CARTESIAN_POINT('Ctrl Pts',(-19.6738347101252,21.9053537220903,
-4.239250035187));
#118656=CARTESIAN_POINT('Ctrl Pts',(-16.9771896136586,21.4596548264534,
-4.36642584186844));
#118657=CARTESIAN_POINT('Ctrl Pts',(-15.8923090067117,18.9509546948064,
-4.49360164854987));
#118658=CARTESIAN_POINT('Ctrl Pts',(-17.4145035108715,16.6808299904415,
-4.62077745523131));
#118659=CARTESIAN_POINT('Ctrl Pts',(-20.1472541466187,16.7319792297855,
-4.74795326191273));
#118660=CARTESIAN_POINT('Ctrl Pts',(-21.5834318192879,19.0574761604191,
-4.87512906859417));
#118661=CARTESIAN_POINT('Ctrl Pts',(-20.4054326534448,21.5238216851043,
-5.00230487527561));
#118662=CARTESIAN_POINT('Ctrl Pts',(-17.6939977688763,21.8682968636094,
-5.12948068195703));
#118663=CARTESIAN_POINT('Ctrl Pts',(-15.9367003815454,19.7748671001969,
-5.25665648863848));
#118664=CARTESIAN_POINT('Ctrl Pts',(-16.7457517741515,17.164124269893,-5.38383229531991));
#118665=CARTESIAN_POINT('Ctrl Pts',(-19.3788975093713,16.4312628785266,
-5.51100810200134));
#118666=CARTESIAN_POINT('Ctrl Pts',(-21.4203898065964,18.2486377661686,
-5.63818390868278));
#118667=CARTESIAN_POINT('Ctrl Pts',(-20.9972861924251,20.9489202724142,
-5.76535971536421));
#118668=CARTESIAN_POINT('Ctrl Pts',(-18.4977579720875,22.0547687962171,
-5.89253552204564));
#118669=CARTESIAN_POINT('Ctrl Pts',(-16.2149671495256,20.5516359536883,
-6.01971132872709));
#118670=CARTESIAN_POINT('Ctrl Pts',(-16.2432326184625,17.8185528329019,
-6.14688713540851));
#118671=CARTESIAN_POINT('Ctrl Pts',(-18.5566225655012,16.36295356291,-6.27406294208995));
#118672=CARTESIAN_POINT('Ctrl Pts',(-21.0327452994073,17.5202601292503,
-6.40123874877139));
#118673=CARTESIAN_POINT('Ctrl Pts',(-21.3999118973314,20.2287155878522,
-6.52841455545281));
#118674=CARTESIAN_POINT('Ctrl Pts',(-19.3212697946072,22.0034801611529,
-6.65559036213426));
#118675=CARTESIAN_POINT('Ctrl Pts',(-16.703844105405,21.2163175074616,-6.78276616881569));
#118676=CARTESIAN_POINT('Ctrl Pts',(-15.9489604438082,18.5894005047157,
-6.90994197549712));
#118677=CARTESIAN_POINT('Ctrl Pts',(-17.7491777159676,16.5327624580774,
-7.03711778217856));
#118678=CARTESIAN_POINT('Ctrl Pts',(-20.4529083087621,16.9332411259839,
-7.16429358885998));
#118679=CARTESIAN_POINT('Ctrl Pts',(-21.5796472157492,19.4234221871405,
-7.29146939554142));
#118680=CARTESIAN_POINT('Ctrl Pts',(-20.0956814230716,21.7187190760035,
-7.41864520222286));
#118681=CARTESIAN_POINT('Ctrl Pts',(-17.3624574402067,21.7133393592328,
-7.54582100890429));
#118682=CARTESIAN_POINT('Ctrl Pts',(-15.8875386284201,19.4122185930627,
-7.67299681558573));
#118683=CARTESIAN_POINT('Ctrl Pts',(-17.0240714537406,16.9264922567919,
-7.80017262226716));
#118684=CARTESIAN_POINT('Ctrl Pts',(-19.7293575901193,16.5366599823727,
-7.9273484289486));
#118685=CARTESIAN_POINT('Ctrl Pts',(-21.5214649164229,18.6003686858652,
-8.05452423563003));
#118686=CARTESIAN_POINT('Ctrl Pts',(-20.756246191493,21.2242937200225,-8.18170004231146));
#118687=CARTESIAN_POINT('Ctrl Pts',(-18.1357421006224,22.0011467251603,
-8.3088758489929));
#118688=CARTESIAN_POINT('Ctrl Pts',(-16.0641025003577,20.2182132859998,
-8.43605165567432));
#118689=CARTESIAN_POINT('Ctrl Pts',(-16.4419281434871,17.5112241716414,
-8.56322746235577));
#118690=CARTESIAN_POINT('Ctrl Pts',(-18.9225874529435,16.3636738798159,
-8.6904032690372));
#118691=CARTESIAN_POINT('Ctrl Pts',(-21.2302294793815,17.8283685782694,
-8.81757907571863));
#118692=CARTESIAN_POINT('Ctrl Pts',(-21.2477358919618,20.5615417903766,
-8.94475488240009));
#118693=CARTESIAN_POINT('Ctrl Pts',(-18.9590456437123,22.0556767338902,
-9.07193068908149));
#118694=CARTESIAN_POINT('Ctrl Pts',(-16.4638899852646,20.9399973346102,
-9.19910649576295));
#118695=CARTESIAN_POINT('Ctrl Pts',(-16.0514193664187,18.2380701945025,
-9.32628230244436));
#118696=CARTESIAN_POINT('Ctrl Pts',(-18.1000499791517,16.4287457641048,
-9.45345810912581));
#118697=CARTESIAN_POINT('Ctrl Pts',(-20.7302903886372,17.1719669089676,
-9.58063391580724));
#118698=CARTESIAN_POINT('Ctrl Pts',(-21.5290582703031,19.7858743581861,
-9.70780972248867));
#118699=CARTESIAN_POINT('Ctrl Pts',(-19.7635336698473,21.8723702644956,
-9.83498552917011));
#118700=CARTESIAN_POINT('Ctrl Pts',(-17.0534758273726,21.5172241363981,
-9.96216133585154));
#118701=CARTESIAN_POINT('Ctrl Pts',(-15.88519460819,19.0462605035686,-10.089337142533));
#118702=CARTESIAN_POINT('Ctrl Pts',(-17.3305155191891,16.7264351338286,
-10.2165129492144));
#118703=CARTESIAN_POINT('Ctrl Pts',(-20.0634463312613,16.6860438193137,
-10.3436887558959));
#118704=CARTESIAN_POINT('Ctrl Pts',(-21.5766926491464,18.9621430841235,
-10.4708645625773));
#118705=CARTESIAN_POINT('Ctrl Pts',(-20.4819448988438,21.466553123448,-10.5980403692588));
#118706=CARTESIAN_POINT('Ctrl Pts',(-17.7835661935479,21.9016331674242,
-10.7252161759402));
#118707=CARTESIAN_POINT('Ctrl Pts',(-15.9571515150968,19.8682242798172,
-10.8523919826216));
#118708=CARTESIAN_POINT('Ctrl Pts',(-16.6783229708898,17.2318529074172,
-10.9795677893031));
#118709=CARTESIAN_POINT('Ctrl Pts',(-19.2854505111856,16.4112261527396,
-11.1067435959845));
#118710=CARTESIAN_POINT('Ctrl Pts',(-21.3866564343474,18.1592181293605,
-11.2339194026659));
#118711=CARTESIAN_POINT('Ctrl Pts',(-21.0542147214219,20.8721546913479,
-11.3610952093473));
#118712=CARTESIAN_POINT('Ctrl Pts',(-18.5931200103587,22.0610849269117,
-11.4882710160288));
#118713=CARTESIAN_POINT('Ctrl Pts',(-16.261273945793,20.6352391382547,-11.6154468227102));
#118714=CARTESIAN_POINT('Ctrl Pts',(-16.1980005612746,17.9027423384994,
-11.7426226293916));
#118715=CARTESIAN_POINT('Ctrl Pts',(-18.4613492599099,16.3704907435428,
-11.8697984360731));
#118716=CARTESIAN_POINT('Ctrl Pts',(-20.9748380899644,17.4442300894981,
-11.9969742427545));
#118717=CARTESIAN_POINT('Ctrl Pts',(-21.4324970545739,20.138871170231,-12.124150049436));
#118718=CARTESIAN_POINT('Ctrl Pts',(-19.4144524592281,21.9822480424568,
-12.2513258561174));
#118719=CARTESIAN_POINT('Ctrl Pts',(-16.7721349661832,21.2831768387803,
-12.3785016627988));
#118720=CARTESIAN_POINT('Ctrl Pts',(-15.9297068745883,18.6830119993224,
-12.5056774694802));
#118721=CARTESIAN_POINT('Ctrl Pts',(-17.6600436714977,16.5672433798551,
-12.6328532761617));
#118722=CARTESIAN_POINT('Ctrl Pts',(-20.3756687425606,16.8769573693289,
-12.7600290828431));
#118723=CARTESIAN_POINT('Ctrl Pts',(-21.5851646357777,19.3280106054199,
-12.8872048895246));
#118724=CARTESIAN_POINT('Ctrl Pts',(-20.1788939389038,21.6717138735354,
-13.014380696206));
#118725=CARTESIAN_POINT('Ctrl Pts',(-17.4470227333175,21.7578648918097,
-13.1415565028874));
#118726=CARTESIAN_POINT('Ctrl Pts',(-15.8958732910946,19.5074254481115,
-13.2687323095689));
#118727=CARTESIAN_POINT('Ctrl Pts',(-16.9485289502823,16.9850340540092,
-13.3959081162503));
#118728=CARTESIAN_POINT('Ctrl Pts',(-19.6392434787545,16.5048282563255,
-13.5230839229317));
#118729=CARTESIAN_POINT('Ctrl Pts',(-21.4994533012164,18.5073670695018,
-13.6502597296132));
#118730=CARTESIAN_POINT('Ctrl Pts',(-20.8225313632018,21.1554454240253,
-13.7774355362946));
#118731=CARTESIAN_POINT('Ctrl Pts',(-18.2295115283253,22.0196157878994,
-13.904611342976));
#118732=CARTESIAN_POINT('Ctrl Pts',(-16.0993285541244,20.3070554887315,
-14.0317871496575));
#118733=CARTESIAN_POINT('Ctrl Pts',(-16.3862931053621,17.5889323075283,
-14.1589629563389));
#118734=CARTESIAN_POINT('Ctrl Pts',(-18.8271330173065,16.3589555572926,
-14.2861387630203));
#118735=CARTESIAN_POINT('Ctrl Pts',(-21.1825291663591,17.745552565399,-14.4133145697018));
#118736=CARTESIAN_POINT('Ctrl Pts',(-21.2915517781366,20.476606638826,-14.5404903763832));
#118737=CARTESIAN_POINT('Ctrl Pts',(-19.0541793730395,22.0465451735372,
-14.6676661830647));
#118738=CARTESIAN_POINT('Ctrl Pts',(-16.5230622657518,21.0150470053099,
-14.7948419897461));
#118739=CARTESIAN_POINT('Ctrl Pts',(-16.0203433033647,18.328447681496,-14.9220177964275));
#118740=CARTESIAN_POINT('Ctrl Pts',(-18.0072359316107,16.4515353325348,
-15.0491936031089));
#118741=CARTESIAN_POINT('Ctrl Pts',(-20.6608894845385,17.1062605442799,
-15.1763694097904));
#118742=CARTESIAN_POINT('Ctrl Pts',(-21.5467415316516,19.6919535717847,
-15.3035452164718));
#118743=CARTESIAN_POINT('Ctrl Pts',(-19.8520778019026,21.8364015485223,
-15.4307210231533));
#118744=CARTESIAN_POINT('Ctrl Pts',(-17.1316470846427,21.5722065552882,
-15.5578968298347));
#118745=CARTESIAN_POINT('Ctrl Pts',(-15.8812757139849,19.1417511005842,
-15.6850726365161));
#118746=CARTESIAN_POINT('Ctrl Pts',(-17.2481018157082,16.7748272130226,
-15.8122484431975));
#118747=CARTESIAN_POINT('Ctrl Pts',(-19.9781472762768,16.6429406515769,
-15.939424249879));
#118748=CARTESIAN_POINT('Ctrl Pts',(-21.5667648313502,18.8670891505701,
-16.0666000565604));
#118749=CARTESIAN_POINT('Ctrl Pts',(-20.5564964748742,21.4067545084005,
-16.1937758632419));
#118750=CARTESIAN_POINT('Ctrl Pts',(-17.8742007195895,21.9319513886684,
-16.3209516699233));
#118751=CARTESIAN_POINT('Ctrl Pts',(-15.9807174389196,19.9608442511223,
-16.4481274766047));
#118752=CARTESIAN_POINT('Ctrl Pts',(-16.6132000200527,17.3018015537547,
-16.5753032832862));
#118753=CARTESIAN_POINT('Ctrl Pts',(-19.1913849510953,16.3943299325974,
-16.7024790899676));
#118754=CARTESIAN_POINT('Ctrl Pts',(-21.3499475780197,18.0709782760213,
-16.829654896649));
#118755=CARTESIAN_POINT('Ctrl Pts',(-21.1085406661289,20.7935257934676,
-16.9568307033305));
#118756=CARTESIAN_POINT('Ctrl Pts',(-18.6886400736801,22.0642041180355,
-17.0840065100119));
#118757=CARTESIAN_POINT('Ctrl Pts',(-16.3103543982751,20.7172447541254,
-17.2111823166934));
#118758=CARTESIAN_POINT('Ctrl Pts',(-16.1556131340415,17.9883993163983,
-17.3383581233747));
#118759=CARTESIAN_POINT('Ctrl Pts',(-18.3663817865876,16.381214122719,-17.4655339300562));
#118760=CARTESIAN_POINT('Ctrl Pts',(-20.9144173329799,17.3701818351261,
-17.5927097367376));
#118761=CARTESIAN_POINT('Ctrl Pts',(-21.4620553083253,20.0479859597428,
-17.7198855434191));
#118762=CARTESIAN_POINT('Ctrl Pts',(-19.5068718604908,21.9579074155056,
-17.8470613501005));
#118763=CARTESIAN_POINT('Ctrl Pts',(-16.8426264504933,21.347711809839,-17.9742371567819));
#118764=CARTESIAN_POINT('Ctrl Pts',(-15.9135988802868,18.7772157379466,
-18.1014129634634));
#118765=CARTESIAN_POINT('Ctrl Pts',(-17.5721142835804,16.6046898027813,
-18.2285887701448));
#118766=CARTESIAN_POINT('Ctrl Pts',(-20.2965877169299,16.8232917077465,
-18.3557645768262));
#118767=CARTESIAN_POINT('Ctrl Pts',(-21.5874839051248,19.2324677728927,
-18.4829403835077));
#118768=CARTESIAN_POINT('Ctrl Pts',(-20.2604857175586,21.6219484889878,
-18.6101161901891));
#118769=CARTESIAN_POINT('Ctrl Pts',(-17.5330316285098,21.7995336065107,
-18.7372919968706));
#118770=CARTESIAN_POINT('Ctrl Pts',(-15.9073914798215,19.6022998030865,
-18.864467803552));
#118771=CARTESIAN_POINT('Ctrl Pts',(-16.874989209244,17.0460727161496,-18.9916436102334));
#118772=CARTESIAN_POINT('Ctrl Pts',(-19.5481139560441,16.4760320435035,
-19.1188194169148));
#118773=CARTESIAN_POINT('Ctrl Pts',(-21.4743396776274,18.4151547160267,
-19.2459952235963));
#118774=CARTESIAN_POINT('Ctrl Pts',(-20.8864738299528,21.08441604792,-19.3731710302777));
#118775=CARTESIAN_POINT('Ctrl Pts',(-18.3238468403057,22.0349344195679,
-19.5003468369591));
#118776=CARTESIAN_POINT('Ctrl Pts',(-16.1375099188267,20.3946682605915,
-19.6275226436406));
#118777=CARTESIAN_POINT('Ctrl Pts',(-16.3332914883073,17.6684598887888,
-19.754698450322));
#118778=CARTESIAN_POINT('Ctrl Pts',(-18.7315741166677,16.3574364254427,
-19.8818742570035));
#118779=CARTESIAN_POINT('Ctrl Pts',(-21.1320823343698,17.6643802422104,
-20.0090500636849));
#118780=CARTESIAN_POINT('Ctrl Pts',(-21.3324988675726,20.390252053842,-20.1362258703664));
#118781=CARTESIAN_POINT('Ctrl Pts',(-19.1489539409205,22.0342326028009,
-20.2634016770477));
#118782=CARTESIAN_POINT('Ctrl Pts',(-16.5847145860095,21.0880738092713,
-20.3905774837292));
#118783=CARTESIAN_POINT('Ctrl Pts',(-15.9923110877633,18.4198137159881,
-20.5177532904106));
#118784=CARTESIAN_POINT('Ctrl Pts',(-17.9152372119337,16.4774229112103,
-20.6449290970921));
#118785=CARTESIAN_POINT('Ctrl Pts',(-20.5893269639303,17.0429098251043,
-20.7721049037735));
#118786=CARTESIAN_POINT('Ctrl Pts',(-21.5612701751591,19.5975033976856,
-20.8992807104549));
#118787=CARTESIAN_POINT('Ctrl Pts',(-19.9393669507179,21.7974684619948,
-21.0264565171363));
#118788=CARTESIAN_POINT('Ctrl Pts',(-17.2116173110634,21.6245779050981,
-21.1536323238178));
#118789=CARTESIAN_POINT('Ctrl Pts',(-15.8805536168431,19.2372471201844,
-21.2808081304992));
#118790=CARTESIAN_POINT('Ctrl Pts',(-17.1673608244619,16.8260911817933,
-21.4079839371807));
#118791=CARTESIAN_POINT('Ctrl Pts',(-19.8914411272743,16.6024497401849,
-21.535159743862));
#118792=CARTESIAN_POINT('Ctrl Pts',(-21.5536818213048,18.7729383600156,
-21.6623355505436));
#118793=CARTESIAN_POINT('Ctrl Pts',(-20.628959867889,21.3434930817089,-21.7895113572249));
#118794=CARTESIAN_POINT('Ctrl Pts',(-17.9658925872421,21.9611712248908,
-21.9166871639064));
#118795=CARTESIAN_POINT('Ctrl Pts',(-16.0068267982834,20.0483220661474,
-22.0438816279422));
#118796=CARTESIAN_POINT('Ctrl Pts',(-16.370269957493,18.2714051300663,-22.1286841564175));
#118797=CARTESIAN_POINT('Ctrl Pts',(-16.8880690061789,17.6565535153103,
-22.1710947493324));
#118798=CARTESIAN_POINT('Ctrl Pts',(-19.3190223738293,17.0246982500464,
0.17134578950673));
#118799=CARTESIAN_POINT('Ctrl Pts',(-20.0469416666524,17.2194788070544,
0.128953853946252));
#118800=CARTESIAN_POINT('Ctrl Pts',(-21.2802301386225,18.3901100196218,
0.0441699828252958));
#118801=CARTESIAN_POINT('Ctrl Pts',(-20.8017893544867,20.9125935436388,
-0.0830058238561385));
#118802=CARTESIAN_POINT('Ctrl Pts',(-18.4227563664326,21.868269370515,-0.210181630537573));
#118803=CARTESIAN_POINT('Ctrl Pts',(-16.3310538010686,20.388884626835,-0.337357437219007));
#118804=CARTESIAN_POINT('Ctrl Pts',(-16.4429843249731,17.8274156154244,
-0.464533243900441));
#118805=CARTESIAN_POINT('Ctrl Pts',(-18.6572569336122,16.5360493975372,
-0.591709050581877));
#118806=CARTESIAN_POINT('Ctrl Pts',(-20.9416888505105,17.6983952880986,
-0.718884857263309));
#118807=CARTESIAN_POINT('Ctrl Pts',(-21.2008318050364,20.2486639942973,
-0.846060663944745));
#118808=CARTESIAN_POINT('Ctrl Pts',(-19.1967429859123,21.846835629714,-0.973236470626179));
#118809=CARTESIAN_POINT('Ctrl Pts',(-16.7681508126867,21.0268460383161,
-1.10041227730761));
#118810=CARTESIAN_POINT('Ctrl Pts',(-16.1430852914322,18.540902198337,-1.22758808398905));
#118811=CARTESIAN_POINT('Ctrl Pts',(-17.8950325268407,16.6697461412296,
-1.35476389067048));
#118812=CARTESIAN_POINT('Ctrl Pts',(-20.4166755091321,17.130025173742,-1.48193969735192));
#118813=CARTESIAN_POINT('Ctrl Pts',(-21.3945706608446,19.4994733923354,
-1.60911550403335));
#118814=CARTESIAN_POINT('Ctrl Pts',(-19.9315560620918,21.6042631320078,
-1.73629131071478));
#118815=CARTESIAN_POINT('Ctrl Pts',(-17.3698587811547,21.5133835525588,
-1.86346711739622));
#118816=CARTESIAN_POINT('Ctrl Pts',(-16.0596760495093,19.3102094146417,
-1.99064292407765));
#118817=CARTESIAN_POINT('Ctrl Pts',(-17.2030197372453,17.0160170823794,
-2.11781873075909));
#118818=CARTESIAN_POINT('Ctrl Pts',(-19.750942698222,16.7355851926327,-2.24499453744052));
#118819=CARTESIAN_POINT('Ctrl Pts',(-21.365883901195,18.7261928240851,-2.37217034412196));
#118820=CARTESIAN_POINT('Ctrl Pts',(-20.5662349525139,21.1615809089484,
-2.49934615080339));
#118821=CARTESIAN_POINT('Ctrl Pts',(-18.0856241694325,21.8074320972958,
-2.62652195748482));
#118822=CARTESIAN_POINT('Ctrl Pts',(-16.1998579613017,20.0712179783623,
-2.75369776416626));
#118823=CARTESIAN_POINT('Ctrl Pts',(-16.6390097906391,17.5458072610157,
-2.8808735708477));
#118824=CARTESIAN_POINT('Ctrl Pts',(-19.0001851054626,16.5481075252713,
-3.00804937752912));
#118825=CARTESIAN_POINT('Ctrl Pts',(-21.1171521082928,17.9934463588478,
-3.13522518421057));
#118826=CARTESIAN_POINT('Ctrl Pts',(-21.0477249663689,20.5558150874991,
-3.26240099089199));
#118827=CARTESIAN_POINT('Ctrl Pts',(-18.8555987740266,21.8843994424129,
-3.38957679757343));
#118828=CARTESIAN_POINT('Ctrl Pts',(-16.5519132536521,20.7603057385855,
-3.51675260425486));
#118829=CARTESIAN_POINT('Ctrl Pts',(-16.2501568875435,18.214820180474,-3.64392841093631));
#118830=CARTESIAN_POINT('Ctrl Pts',(-18.2271724123875,16.5832677768282,
-3.77110421761772));
#118831=CARTESIAN_POINT('Ctrl Pts',(-20.6691707916169,17.3624965925164,
-3.89828002429917));
#118832=CARTESIAN_POINT('Ctrl Pts',(-21.3357700797732,19.8376125534949,
-4.0254558309806));
#118833=CARTESIAN_POINT('Ctrl Pts',(-19.6154068038058,21.7378503886108,
-4.15263163766203));
#118834=CARTESIAN_POINT('Ctrl Pts',(-17.0864074916199,21.3198598261951,
-4.27980744434348));
#118835=CARTESIAN_POINT('Ctrl Pts',(-16.06897204475,18.9671212638499,-4.4069832510249));
#118836=CARTESIAN_POINT('Ctrl Pts',(-17.4965343365317,16.8381263050999,
-4.53415905770634));
#118837=CARTESIAN_POINT('Ctrl Pts',(-20.0593945687647,16.8860956842701,
-4.66133486438777));
#118838=CARTESIAN_POINT('Ctrl Pts',(-21.4062875474204,19.0670204732863,
-4.7885106710692));
#118839=CARTESIAN_POINT('Ctrl Pts',(-20.3015225621888,21.3800375416853,
-4.91568647775065));
#118840=CARTESIAN_POINT('Ctrl Pts',(-17.7586529175715,21.7030972912407,
-5.04286228443207));
#118841=CARTESIAN_POINT('Ctrl Pts',(-16.1106036842152,19.7398124530851,
-5.17003809111352));
#118842=CARTESIAN_POINT('Ctrl Pts',(-16.8693577442526,17.2913750110263,
-5.29721389779494));
#118843=CARTESIAN_POINT('Ctrl Pts',(-19.3388053411876,16.604074350987,-5.42438970447638));
#118844=CARTESIAN_POINT('Ctrl Pts',(-21.253381576036,18.3084661698633,-5.55156551115781));
#118845=CARTESIAN_POINT('Ctrl Pts',(-20.8565815853272,20.8408767603229,
-5.67874131783925));
#118846=CARTESIAN_POINT('Ctrl Pts',(-18.5124447323517,21.877976584747,-5.80591712452068));
#118847=CARTESIAN_POINT('Ctrl Pts',(-16.3715710861727,20.468290923901,-5.93309293120211));
#118848=CARTESIAN_POINT('Ctrl Pts',(-16.3980793395551,17.9051188766514,
-6.06026873788356));
#118849=CARTESIAN_POINT('Ctrl Pts',(-18.5676498153085,16.5400117079507,
-6.18744454456498));
#118850=CARTESIAN_POINT('Ctrl Pts',(-20.8898362606593,17.6253705169753,
-6.31462035124643));
#118851=CARTESIAN_POINT('Ctrl Pts',(-21.2341767431441,20.1654459614101,
-6.44179615792784));
#118852=CARTESIAN_POINT('Ctrl Pts',(-19.2847602422637,21.8298764758485,
-6.56897196460929));
#118853=CARTESIAN_POINT('Ctrl Pts',(-16.8300554031422,21.0916503695018,
-6.69614777129072));
#118854=CARTESIAN_POINT('Ctrl Pts',(-16.1221015595086,18.6280442754634,
-6.82332357797216));
#118855=CARTESIAN_POINT('Ctrl Pts',(-17.8104024223259,16.6992638763745,
-6.95049938465359));
#118856=CARTESIAN_POINT('Ctrl Pts',(-20.3460467377283,17.0748454747864,
-7.07767519133502));
#118857=CARTESIAN_POINT('Ctrl Pts',(-21.4027382261697,19.4102162653792,
-7.20485099801646));
#118858=CARTESIAN_POINT('Ctrl Pts',(-20.0110280326754,21.5628184972425,
-7.33202680469789));
#118859=CARTESIAN_POINT('Ctrl Pts',(-17.4477238805002,21.5577732282041,
-7.45920261137933));
#118860=CARTESIAN_POINT('Ctrl Pts',(-16.0644982326662,19.3997091794621,
-7.58637841806076));
#118861=CARTESIAN_POINT('Ctrl Pts',(-17.1303747683952,17.0685161711762,
-7.7135542247422));
#118862=CARTESIAN_POINT('Ctrl Pts',(-19.6674779219145,16.7029190982927,
-7.84073003142363));
#118863=CARTESIAN_POINT('Ctrl Pts',(-21.3481730202512,18.6383305836686,
-7.96790583810506));
#118864=CARTESIAN_POINT('Ctrl Pts',(-20.6305266263839,21.0991307146561,
-8.0950816447865));
#118865=CARTESIAN_POINT('Ctrl Pts',(-18.1729347645271,21.8276881055553,
-8.22225745146793));
#118866=CARTESIAN_POINT('Ctrl Pts',(-16.2300854325808,20.1555965695878,
-8.34943325814937));
#118867=CARTESIAN_POINT('Ctrl Pts',(-16.5844223057765,17.6168963092987,
-8.4766090648308));
#118868=CARTESIAN_POINT('Ctrl Pts',(-18.9108632955837,16.5406872439944,
-8.60378487151224));
#118869=CARTESIAN_POINT('Ctrl Pts',(-21.075043189067,17.9143243940239,-8.73096067819366));
#118870=CARTESIAN_POINT('Ctrl Pts',(-21.0914612581086,20.4775809317719,
-8.85813648487511));
#118871=CARTESIAN_POINT('Ctrl Pts',(-18.945054943383,21.8788280774976,-8.98531229155654));
#118872=CARTESIAN_POINT('Ctrl Pts',(-16.6050188176507,20.8325085462043,
-9.11248809823798));
#118873=CARTESIAN_POINT('Ctrl Pts',(-16.218190787249,18.2985555659393,-9.23966390491941));
#118874=CARTESIAN_POINT('Ctrl Pts',(-18.1394615608164,16.6017137212363,
-9.36683971160084));
#118875=CARTESIAN_POINT('Ctrl Pts',(-20.6061844511175,17.2987300867281,
-9.49401551828229));
#118876=CARTESIAN_POINT('Ctrl Pts',(-21.3552943083903,19.7501354087903,
-9.62119132496371));
#118877=CARTESIAN_POINT('Ctrl Pts',(-19.6995293335885,21.7069174558048,
-9.74836713164515));
#118878=CARTESIAN_POINT('Ctrl Pts',(-17.1579511227282,21.3738501512268,
-9.87554293832658));
#118879=CARTESIAN_POINT('Ctrl Pts',(-16.0622999361394,19.0565020745182,
-10.002718745008));
#118880=CARTESIAN_POINT('Ctrl Pts',(-17.4177677337352,16.8808962552165,
-10.1298945516894));
#118881=CARTESIAN_POINT('Ctrl Pts',(-19.980796941041,16.8430159992049,-10.2570703583709));
#118882=CARTESIAN_POINT('Ctrl Pts',(-21.3999673398873,18.9776140902601,
-10.3842461650523));
#118883=CARTESIAN_POINT('Ctrl Pts',(-20.3732781729815,21.3263292679386,
-10.5114219717337));
#118884=CARTESIAN_POINT('Ctrl Pts',(-17.8426530274432,21.7343611344247,
-10.6385977784151));
#118885=CARTESIAN_POINT('Ctrl Pts',(-16.1297834059933,19.8273657775314,
-10.7657735850966));
#118886=CARTESIAN_POINT('Ctrl Pts',(-16.8061208736337,17.3548930757276,
-10.892949391778));
#118887=CARTESIAN_POINT('Ctrl Pts',(-19.2511677820415,16.5852832739556,
-11.0201251984594));
#118888=CARTESIAN_POINT('Ctrl Pts',(-21.221745349479,18.2246055979698,-11.1473010051409));
#118889=CARTESIAN_POINT('Ctrl Pts',(-20.9099709656597,20.7688835633054,
-11.2744768118223));
#118890=CARTESIAN_POINT('Ctrl Pts',(-18.6018782768372,21.8839000524673,
-11.4016526185037));
#118891=CARTESIAN_POINT('Ctrl Pts',(-16.4149990686176,20.5466966423776,
-11.5288284251852));
#118892=CARTESIAN_POINT('Ctrl Pts',(-16.3556592815108,17.9840744655897,
-11.6560042318666));
#118893=CARTESIAN_POINT('Ctrl Pts',(-18.4782994871448,16.5470803150364,
-11.783180038548));
#118894=CARTESIAN_POINT('Ctrl Pts',(-20.8355290427597,17.5540671339344,
-11.9103558452295));
#118895=CARTESIAN_POINT('Ctrl Pts',(-21.2647361372453,20.0811870165956,
-12.0375316519109));
#118896=CARTESIAN_POINT('Ctrl Pts',(-19.3721499010078,21.8099643214279,
-12.1647074585924));
#118897=CARTESIAN_POINT('Ctrl Pts',(-16.8941007386454,21.1543531712681,
-12.2918832652738));
#118898=CARTESIAN_POINT('Ctrl Pts',(-16.1040449515487,18.7158361045709,
-12.4190590719552));
#118899=CARTESIAN_POINT('Ctrl Pts',(-17.7268096879864,16.7316011785925,
-12.5462348786367));
#118900=CARTESIAN_POINT('Ctrl Pts',(-20.2736090224157,17.0220607824092,
-12.6734106853181));
#118901=CARTESIAN_POINT('Ctrl Pts',(-21.4079126376915,19.3207362574753,
-12.8005864919995));
#118902=CARTESIAN_POINT('Ctrl Pts',(-20.0890673696206,21.5187355273081,
-12.9277622986809));
#118903=CARTESIAN_POINT('Ctrl Pts',(-17.5270318948891,21.5995306850564,
-13.0549381053624));
#118904=CARTESIAN_POINT('Ctrl Pts',(-16.0723147437075,19.4889971881991,
-13.1821139120438));
#118905=CARTESIAN_POINT('Ctrl Pts',(-17.0595286123559,17.1234185256205,
-13.3092897187253));
#118906=CARTESIAN_POINT('Ctrl Pts',(-19.5829660497523,16.6730662958661,
-13.4364655254067));
#118907=CARTESIAN_POINT('Ctrl Pts',(-21.3275298292767,18.5511107177236,
-13.5636413320881));
#118908=CARTESIAN_POINT('Ctrl Pts',(-20.6926909630551,21.0345625987219,
-13.6908171387696));
#118909=CARTESIAN_POINT('Ctrl Pts',(-18.2608747083023,21.8450089784522,
-13.817992945451));
#118910=CARTESIAN_POINT('Ctrl Pts',(-16.2631215432146,20.2389156054877,
-13.9451687521324));
#118911=CARTESIAN_POINT('Ctrl Pts',(-16.5322460022147,17.6897734641258,
-14.0723445588139));
#118912=CARTESIAN_POINT('Ctrl Pts',(-18.8213430979177,16.5362622514614,
-14.1995203654953));
#118913=CARTESIAN_POINT('Ctrl Pts',(-21.0303083224052,17.8366569101336,
-14.3266961721767));
#118914=CARTESIAN_POINT('Ctrl Pts',(-21.1325531860542,20.3979260524059,
-14.4538719788582));
#118915=CARTESIAN_POINT('Ctrl Pts',(-19.0342743724987,21.8702642105349,
-14.5810477855396));
#118916=CARTESIAN_POINT('Ctrl Pts',(-16.6605124593049,20.9028925080494,
-14.708223592221));
#118917=CARTESIAN_POINT('Ctrl Pts',(-16.1890466695481,18.3833144401207,
-14.8353993989025));
#118918=CARTESIAN_POINT('Ctrl Pts',(-18.0524176028627,16.6230865014217,
-14.9625752055839));
#118919=CARTESIAN_POINT('Ctrl Pts',(-20.5410980817764,17.2371085736416,
-15.0897510122653));
#118920=CARTESIAN_POINT('Ctrl Pts',(-21.3718782318164,19.6620535160264,
-15.2169268189468));
#118921=CARTESIAN_POINT('Ctrl Pts',(-19.7825688293528,21.6731848529956,
-15.3441026256282));
#118922=CARTESIAN_POINT('Ctrl Pts',(-17.2312626074793,21.4254144077681,
-15.4712784323096));
#118923=CARTESIAN_POINT('Ctrl Pts',(-16.0586246728421,19.1460561854722,
-15.5984542389911));
#118924=CARTESIAN_POINT('Ctrl Pts',(-17.3404775483521,16.9262798821378,
-15.7256300456725));
#118925=CARTESIAN_POINT('Ctrl Pts',(-19.9008007814914,16.8025924812187,
-15.852805852354));
#118926=CARTESIAN_POINT('Ctrl Pts',(-21.3906567174362,18.8884694961524,
-15.9799816590354));
#118927=CARTESIAN_POINT('Ctrl Pts',(-20.4431950058454,21.2702482298655,
-16.1071574657168));
#118928=CARTESIAN_POINT('Ctrl Pts',(-17.9276529609976,21.7627945240366,
-16.2343332723983));
#118929=CARTESIAN_POINT('Ctrl Pts',(-16.1518842768929,19.9142277246345,
-16.3615090790797));
#118930=CARTESIAN_POINT('Ctrl Pts',(-16.7450465045628,17.4204931351153,
-16.4886848857611));
#118931=CARTESIAN_POINT('Ctrl Pts',(-19.1629501159199,16.5694374627385,
-16.6158606924426));
#118932=CARTESIAN_POINT('Ctrl Pts',(-21.1873186195673,18.1418514644375,
-16.743036499124));
#118933=CARTESIAN_POINT('Ctrl Pts',(-20.960919559888,20.6951428886731,-16.8702123058054));
#118934=CARTESIAN_POINT('Ctrl Pts',(-18.6914600222275,21.8868253288476,
-16.9973881124868));
#118935=CARTESIAN_POINT('Ctrl Pts',(-16.4610282738444,20.6236041102547,
-17.1245639191683));
#118936=CARTESIAN_POINT('Ctrl Pts',(-16.3159070076732,18.0644062966023,
-17.2517397258497));
#118937=CARTESIAN_POINT('Ctrl Pts',(-18.3892359781844,16.5571370401859,
-17.3789155325312));
#118938=CARTESIAN_POINT('Ctrl Pts',(-20.7788645402429,17.4846223320876,
-17.5060913392126));
#118939=CARTESIAN_POINT('Ctrl Pts',(-21.2924568052356,19.9959519832151,
-17.633267145894));
#118940=CARTESIAN_POINT('Ctrl Pts',(-19.4588237471628,21.78713690936,-17.7604429525755));
#118941=CARTESIAN_POINT('Ctrl Pts',(-16.9602098887033,21.2148761142513,
-17.8876187592569));
#118942=CARTESIAN_POINT('Ctrl Pts',(-16.0889383635284,18.8041833589049,
-18.0147945659385));
#118943=CARTESIAN_POINT('Ctrl Pts',(-17.6443467187751,16.7667196218568,
-18.1419703726198));
#118944=CARTESIAN_POINT('Ctrl Pts',(-20.199444328037,16.97173142264,-18.2691461793012));
#118945=CARTESIAN_POINT('Ctrl Pts',(-21.410087722055,19.2311331584014,-18.3963219859826));
#118946=CARTESIAN_POINT('Ctrl Pts',(-20.1655867278293,21.4720639710636,
-18.5234977926641));
#118947=CARTESIAN_POINT('Ctrl Pts',(-17.6076937651026,21.638608927483,-18.6506735993455));
#118948=CARTESIAN_POINT('Ctrl Pts',(-16.083116866466,19.5779733678196,-18.777849406027));
#118949=CARTESIAN_POINT('Ctrl Pts',(-16.9905607104441,17.1806625191931,
-18.9050252127085));
#118950=CARTESIAN_POINT('Ctrl Pts',(-19.4975018926199,16.6460602940324,
-19.0322010193898));
#118951=CARTESIAN_POINT('Ctrl Pts',(-21.3039774764415,18.4646310475516,
-19.1593768260712));
#118952=CARTESIAN_POINT('Ctrl Pts',(-20.7526582367037,20.9679489966759,
-19.2865526327527));
#118953=CARTESIAN_POINT('Ctrl Pts',(-18.3493453563032,21.8593752771558,
-19.4137284394341));
#118954=CARTESIAN_POINT('Ctrl Pts',(-16.2989292381897,20.3210816421169,
-19.5409042461156));
#118955=CARTESIAN_POINT('Ctrl Pts',(-16.4825394044677,17.7643569525393,
-19.668080052797));
#118956=CARTESIAN_POINT('Ctrl Pts',(-18.7317249296591,16.5348375614239,
-19.7952558594784));
#118957=CARTESIAN_POINT('Ctrl Pts',(-20.9829976831335,17.760530930567,-19.9224316661598));
#118958=CARTESIAN_POINT('Ctrl Pts',(-21.1709546654166,20.31693998334,-20.0496074728413));
#118959=CARTESIAN_POINT('Ctrl Pts',(-19.1231569686169,21.8587170911293,
-20.1767832795227));
#118960=CARTESIAN_POINT('Ctrl Pts',(-16.7183319609261,20.9713793612995,
-20.3039590862042));
#118961=CARTESIAN_POINT('Ctrl Pts',(-16.1627571685425,18.4690004055044,
-20.4311348928856));
#118962=CARTESIAN_POINT('Ctrl Pts',(-17.9661382852434,16.6473646938876,
-20.558310699567));
#118963=CARTESIAN_POINT('Ctrl Pts',(-20.4739844799035,17.1776962596402,
-20.6854865062485));
#118964=CARTESIAN_POINT('Ctrl Pts',(-21.3855036545633,19.573475146687,-20.8126623129299));
#118965=CARTESIAN_POINT('Ctrl Pts',(-19.8644313620253,21.6366721694472,
-20.9398381196113));
#118966=CARTESIAN_POINT('Ctrl Pts',(-17.3062612225653,21.4745299209001,
-21.0670139262928));
#118967=CARTESIAN_POINT('Ctrl Pts',(-16.0579474672366,19.2356153818981,
-21.1941897329742));
#118968=CARTESIAN_POINT('Ctrl Pts',(-17.2647560855632,16.9743568582036,
-21.3213655396557));
#118969=CARTESIAN_POINT('Ctrl Pts',(-19.8194850045369,16.7646188200965,
-21.448541346337));
#118970=CARTESIAN_POINT('Ctrl Pts',(-21.3783870556072,18.8001718981978,
-21.5757171530185));
#118971=CARTESIAN_POINT('Ctrl Pts',(-20.5111534744378,21.210919657188,-21.7028929596999));
#118972=CARTESIAN_POINT('Ctrl Pts',(-18.013644503055,21.7901978133332,-21.8300687663814));
#118973=CARTESIAN_POINT('Ctrl Pts',(-16.1763704623236,19.996267194463,-21.9572632304172));
#118974=CARTESIAN_POINT('Ctrl Pts',(-16.5172189858702,18.3298181259339,
-22.0420657588926));
#118975=CARTESIAN_POINT('Ctrl Pts',(-17.0028273589161,17.7531907778071,
-22.0844763518074));
#118976=CARTESIAN_POINT('Ctrl Pts',(-19.2802416061914,17.1696268270448,
0.257964187031692));
#118977=CARTESIAN_POINT('Ctrl Pts',(-19.9599075838988,17.3514955026281,
0.215572251471214));
#118978=CARTESIAN_POINT('Ctrl Pts',(-21.1114421336233,18.4445263035272,
0.130788380350257));
#118979=CARTESIAN_POINT('Ctrl Pts',(-20.664716890137,20.7997959707902,0.00361257366882362));
#118980=CARTESIAN_POINT('Ctrl Pts',(-18.4433885124361,21.6921206442111,
-0.123563233012611));
#118981=CARTESIAN_POINT('Ctrl Pts',(-16.4903436032298,20.310803390867,-0.250739039694045));
#118982=CARTESIAN_POINT('Ctrl Pts',(-16.5948543226392,17.9191325598114,
-0.37791484637548));
#118983=CARTESIAN_POINT('Ctrl Pts',(-18.6623441835338,16.7133702016597,
-0.505090653056915));
#118984=CARTESIAN_POINT('Ctrl Pts',(-20.7953425359789,17.7986649093718,
-0.632266459738347));
#118985=CARTESIAN_POINT('Ctrl Pts',(-21.0373070659623,20.1798778964501,
-0.759442266419783));
#118986=CARTESIAN_POINT('Ctrl Pts',(-19.1660680424989,21.6721077326961,
-0.886618073101216));
#118987=CARTESIAN_POINT('Ctrl Pts',(-16.8984657270469,20.9064747389806,
-1.01379387978265));
#118988=CARTESIAN_POINT('Ctrl Pts',(-16.3148354086541,18.5853225629306,
-1.14096968646408));
#118989=CARTESIAN_POINT('Ctrl Pts',(-17.9506471564477,16.8382042717466,
-1.26814549314552));
#118990=CARTESIAN_POINT('Ctrl Pts',(-20.305132000971,17.2679716947772,-1.39532129982695));
#118991=CARTESIAN_POINT('Ctrl Pts',(-21.2182030940675,19.4803506713964,
-1.52249710650838));
#118992=CARTESIAN_POINT('Ctrl Pts',(-19.8521708189713,21.445615214303,-1.64967291318982));
#118993=CARTESIAN_POINT('Ctrl Pts',(-17.4602868502336,21.3607599853939,
-1.77684871987125));
#118994=CARTESIAN_POINT('Ctrl Pts',(-16.236955313264,19.3036328845313,-1.90402452655269));
#118995=CARTESIAN_POINT('Ctrl Pts',(-17.3045074623036,17.1615211285584,
-2.03120033323412));
#118996=CARTESIAN_POINT('Ctrl Pts',(-19.6835302021449,16.8996788935686,
-2.15837613991555));
#118997=CARTESIAN_POINT('Ctrl Pts',(-21.1914179617914,18.758330388868,-2.28555194659699));
#118998=CARTESIAN_POINT('Ctrl Pts',(-20.444777242296,21.0322781192214,-2.41272775327842));
#118999=CARTESIAN_POINT('Ctrl Pts',(-18.1286045981342,21.6353162358223,
-2.53990355995986));
#119000=CARTESIAN_POINT('Ctrl Pts',(-16.3678446537097,20.0141946660428,
-2.66707936664131));
#119001=CARTESIAN_POINT('Ctrl Pts',(-16.7778853826632,17.6561918472671,
-2.79425517332272));
#119002=CARTESIAN_POINT('Ctrl Pts',(-18.9825398611346,16.7246290036402,
-2.92143098000418));
#119003=CARTESIAN_POINT('Ctrl Pts',(-20.9591744440326,18.0741572289896,
-3.04860678668559));
#119004=CARTESIAN_POINT('Ctrl Pts',(-20.8943495839686,20.4666681355921,
-3.17578259336703));
#119005=CARTESIAN_POINT('Ctrl Pts',(-18.8475380672715,21.7071814637211,
-3.30295840004846));
#119006=CARTESIAN_POINT('Ctrl Pts',(-16.696562420695,20.6576032291843,-3.4301342067299));
#119007=CARTESIAN_POINT('Ctrl Pts',(-16.4148092955578,18.2808563182951,
-3.55731001341133));
#119008=CARTESIAN_POINT('Ctrl Pts',(-18.2607696965035,16.7574585040896,
-3.68448582009278));
#119009=CARTESIAN_POINT('Ctrl Pts',(-20.5408895289395,17.4850327284497,
-3.8116616267742));
#119010=CARTESIAN_POINT('Ctrl Pts',(-21.1633003667766,19.7960747988325,
-3.93883743345564));
#119011=CARTESIAN_POINT('Ctrl Pts',(-19.5569788974863,21.5703470551314,
-4.06601324013707));
#119012=CARTESIAN_POINT('Ctrl Pts',(-17.1956253695811,21.1800648259367,
-4.19318904681852));
#119013=CARTESIAN_POINT('Ctrl Pts',(-16.2456350827884,18.9832878328934,
-4.32036485349995));
#119014=CARTESIAN_POINT('Ctrl Pts',(-17.5785651621917,16.9954226197583,
-4.44754066018137));
#119015=CARTESIAN_POINT('Ctrl Pts',(-19.9715349909106,17.0402121387546,
-4.57471646686281));
#119016=CARTESIAN_POINT('Ctrl Pts',(-21.2291432755529,19.0765647861535,
-4.70189227354424));
#119017=CARTESIAN_POINT('Ctrl Pts',(-20.1976124709327,21.2362533982663,
-4.82906808022569));
#119018=CARTESIAN_POINT('Ctrl Pts',(-17.8233080662669,21.5378977188721,
-4.95624388690712));
#119019=CARTESIAN_POINT('Ctrl Pts',(-16.2845069868849,19.7047578059733,
-5.08341969358855));
#119020=CARTESIAN_POINT('Ctrl Pts',(-16.9929637143536,17.4186257521595,
-5.21059550026999));
#119021=CARTESIAN_POINT('Ctrl Pts',(-19.298713173004,16.7768858234474,-5.33777130695141));
#119022=CARTESIAN_POINT('Ctrl Pts',(-21.0863733454756,18.368294573558,-5.46494711363286));
#119023=CARTESIAN_POINT('Ctrl Pts',(-20.7158769782294,20.7328332482315,
-5.59212292031427));
#119024=CARTESIAN_POINT('Ctrl Pts',(-18.5271314926159,21.7011843732767,
-5.71929872699574));
#119025=CARTESIAN_POINT('Ctrl Pts',(-16.5281750228197,20.3849458941136,
-5.84647453367714));
#119026=CARTESIAN_POINT('Ctrl Pts',(-16.5529260606478,17.9916849204009,
-5.9736503403586));
#119027=CARTESIAN_POINT('Ctrl Pts',(-18.5786770651157,16.7170698529915,
-6.10082614704002));
#119028=CARTESIAN_POINT('Ctrl Pts',(-20.7469272219113,17.7304809047003,
-6.22800195372147));
#119029=CARTESIAN_POINT('Ctrl Pts',(-21.0684415889569,20.1021763349681,
-6.35517776040288));
#119030=CARTESIAN_POINT('Ctrl Pts',(-19.2482506899202,21.6562727905442,
-6.48235356708434));
#119031=CARTESIAN_POINT('Ctrl Pts',(-16.9562667008792,20.9669832315418,
-6.60952937376576));
#119032=CARTESIAN_POINT('Ctrl Pts',(-16.2952426752091,18.6666880462109,
-6.7367051804472));
#119033=CARTESIAN_POINT('Ctrl Pts',(-17.8716271286841,16.8657652946716,
-6.86388098712864));
#119034=CARTESIAN_POINT('Ctrl Pts',(-20.2391851666945,17.2164498235889,
-6.99105679381006));
#119035=CARTESIAN_POINT('Ctrl Pts',(-21.2258292365902,19.397010343618,-7.11823260049151));
#119036=CARTESIAN_POINT('Ctrl Pts',(-19.9263746422792,21.4069179184816,
-7.24540840717293));
#119037=CARTESIAN_POINT('Ctrl Pts',(-17.5329903207938,21.4022070971754,
-7.37258421385437));
#119038=CARTESIAN_POINT('Ctrl Pts',(-16.2414578369124,19.3871997658614,
-7.49976002053581));
#119039=CARTESIAN_POINT('Ctrl Pts',(-17.2366780830498,17.2105400855604,
-7.62693582721722));
#119040=CARTESIAN_POINT('Ctrl Pts',(-19.6055982537098,16.8691782142126,
-7.75411163389868));
#119041=CARTESIAN_POINT('Ctrl Pts',(-21.1748811240797,18.6762924814722,
-7.88128744058011));
#119042=CARTESIAN_POINT('Ctrl Pts',(-20.5048070612748,20.9739677092896,
-8.00846324726155));
#119043=CARTESIAN_POINT('Ctrl Pts',(-18.2101274284319,21.6542294859505,
-8.13563905394297));
#119044=CARTESIAN_POINT('Ctrl Pts',(-16.3960683648039,20.0929798531758,
-8.26281486062441));
#119045=CARTESIAN_POINT('Ctrl Pts',(-16.7269164680658,17.7225684469559,
-8.38999066730585));
#119046=CARTESIAN_POINT('Ctrl Pts',(-18.899139138224,16.717700608173,-8.51716647398728));
#119047=CARTESIAN_POINT('Ctrl Pts',(-20.9198568987526,18.0002802097783,
-8.64434228066872));
#119048=CARTESIAN_POINT('Ctrl Pts',(-20.9351866242553,20.3936200731671,
-8.77151808735015));
#119049=CARTESIAN_POINT('Ctrl Pts',(-18.9310642430538,21.7019794211049,
-8.89869389403158));
#119050=CARTESIAN_POINT('Ctrl Pts',(-16.7461476500366,20.7250197577984,
-9.02586970071301));
#119051=CARTESIAN_POINT('Ctrl Pts',(-16.3849622080794,18.3590409373758,
-9.15304550739446));
#119052=CARTESIAN_POINT('Ctrl Pts',(-18.1788731424809,16.774681678368,-9.28022131407588));
#119053=CARTESIAN_POINT('Ctrl Pts',(-20.4820785135977,17.4254932644886,
-9.40739712075733));
#119054=CARTESIAN_POINT('Ctrl Pts',(-21.1815303464774,19.7143964593946,
-9.53457292743875));
#119055=CARTESIAN_POINT('Ctrl Pts',(-19.6355249973296,21.5414646471141,
-9.66174873412019));
#119056=CARTESIAN_POINT('Ctrl Pts',(-17.2624264180838,21.2304761660553,
-9.78892454080163));
#119057=CARTESIAN_POINT('Ctrl Pts',(-16.2394052640888,19.0667436454676,
-9.91610034748306));
#119058=CARTESIAN_POINT('Ctrl Pts',(-17.5050199482811,17.0353573766044,
-10.0432761541645));
#119059=CARTESIAN_POINT('Ctrl Pts',(-19.8981475508207,16.9999881790961,
-10.1704519608459));
#119060=CARTESIAN_POINT('Ctrl Pts',(-21.2232420306283,18.9930850963969,
-10.2976277675273));
#119061=CARTESIAN_POINT('Ctrl Pts',(-20.264611447119,21.1861054124292,-10.4248035742088));
#119062=CARTESIAN_POINT('Ctrl Pts',(-17.9017398613385,21.5670891014251,
-10.5519793808902));
#119063=CARTESIAN_POINT('Ctrl Pts',(-16.30241529689,19.7865072752454,-10.6791551875716));
#119064=CARTESIAN_POINT('Ctrl Pts',(-16.9339187763774,17.477933244038,-10.8063309942531));
#119065=CARTESIAN_POINT('Ctrl Pts',(-19.2168850528976,16.7593403951717,
-10.9335068009345));
#119066=CARTESIAN_POINT('Ctrl Pts',(-21.0568342646105,18.289993066579,-11.0606826076159));
#119067=CARTESIAN_POINT('Ctrl Pts',(-20.7657272098974,20.6656124352628,
-11.1878584142974));
#119068=CARTESIAN_POINT('Ctrl Pts',(-18.6106365433157,21.7067151780229,
-11.3150342209788));
#119069=CARTESIAN_POINT('Ctrl Pts',(-16.5687241914422,20.4581541465005,
-11.4422100276602));
#119070=CARTESIAN_POINT('Ctrl Pts',(-16.5133180017472,18.0654065926801,
-11.5693858343417));
#119071=CARTESIAN_POINT('Ctrl Pts',(-18.4952497143798,16.7236698865299,
-11.6965616410231));
#119072=CARTESIAN_POINT('Ctrl Pts',(-20.696219995555,17.6639041783707,-11.8237374477046));
#119073=CARTESIAN_POINT('Ctrl Pts',(-21.0969752199166,20.0235028629602,
-11.950913254386));
#119074=CARTESIAN_POINT('Ctrl Pts',(-19.3298473427874,21.6376806003988,
-12.0780890610674));
#119075=CARTESIAN_POINT('Ctrl Pts',(-17.0160665111076,21.0255295037559,
-12.2052648677489));
#119076=CARTESIAN_POINT('Ctrl Pts',(-16.278383028509,18.7486602098194,-12.3324406744303));
#119077=CARTESIAN_POINT('Ctrl Pts',(-17.7935757044751,16.8959589773299,
-12.4596164811117));
#119078=CARTESIAN_POINT('Ctrl Pts',(-20.1715493022707,17.1671641954894,
-12.5867922877931));
#119079=CARTESIAN_POINT('Ctrl Pts',(-21.2306606396052,19.3134619095308,
-12.7139680944746));
#119080=CARTESIAN_POINT('Ctrl Pts',(-19.9992408003375,21.365757181081,-12.841143901156));
#119081=CARTESIAN_POINT('Ctrl Pts',(-17.6070410564606,21.4411964783031,
-12.9683197078375));
#119082=CARTESIAN_POINT('Ctrl Pts',(-16.2487561963206,19.4705689282866,
-13.0954955145189));
#119083=CARTESIAN_POINT('Ctrl Pts',(-17.1705282744295,17.2618029972318,
-13.2226713212003));
#119084=CARTESIAN_POINT('Ctrl Pts',(-19.52668862075,16.8413043354067,-13.3498471278818));
#119085=CARTESIAN_POINT('Ctrl Pts',(-21.1556063573368,18.5948543659455,
-13.4770229345632));
#119086=CARTESIAN_POINT('Ctrl Pts',(-20.5628505629085,20.9136797734184,
-13.6041987412446));
#119087=CARTESIAN_POINT('Ctrl Pts',(-18.2922378882792,21.670402169005,-13.7313745479261));
#119088=CARTESIAN_POINT('Ctrl Pts',(-16.4269145323048,20.1707757222437,
-13.8585503546075));
#119089=CARTESIAN_POINT('Ctrl Pts',(-16.6781988990673,17.7906146207234,
-13.9857261612889));
#119090=CARTESIAN_POINT('Ctrl Pts',(-18.8155531785289,16.7135689456302,
-14.1129019679704));
#119091=CARTESIAN_POINT('Ctrl Pts',(-20.8780874784513,17.9277612548684,
-14.2400777746518));
#119092=CARTESIAN_POINT('Ctrl Pts',(-20.9735545939718,20.3192454659859,
-14.3672535813332));
#119093=CARTESIAN_POINT('Ctrl Pts',(-19.0143693719578,21.6939832475324,
-14.4944293880147));
#119094=CARTESIAN_POINT('Ctrl Pts',(-16.7979626528582,20.7907380107889,
-14.6216051946961));
#119095=CARTESIAN_POINT('Ctrl Pts',(-16.3577500357315,18.4381811987453,
-14.7487810013775));
#119096=CARTESIAN_POINT('Ctrl Pts',(-18.0975992741149,16.7946376703086,
-14.875956808059));
#119097=CARTESIAN_POINT('Ctrl Pts',(-20.4213066790141,17.3679566030033,
-15.0031326147404));
#119098=CARTESIAN_POINT('Ctrl Pts',(-21.1970149319813,19.6321534602683,
-15.1303084214219));
#119099=CARTESIAN_POINT('Ctrl Pts',(-19.713059856803,21.5099681574688,-15.2574842281033));
#119100=CARTESIAN_POINT('Ctrl Pts',(-17.3308781303159,21.2786222602481,
-15.3846600347847));
#119101=CARTESIAN_POINT('Ctrl Pts',(-16.2359736316991,19.1503612703603,
-15.5118358414661));
#119102=CARTESIAN_POINT('Ctrl Pts',(-17.432853280996,17.0777325512529,-15.6390116481476));
#119103=CARTESIAN_POINT('Ctrl Pts',(-19.8234542867059,16.9622443108606,
-15.766187454829));
#119104=CARTESIAN_POINT('Ctrl Pts',(-21.2145486035221,18.9098498417347,
-15.8933632615105));
#119105=CARTESIAN_POINT('Ctrl Pts',(-20.3298935368166,21.1337419513304,
-16.0205390681919));
#119106=CARTESIAN_POINT('Ctrl Pts',(-17.9811052024058,21.5936376594049,
-16.1477148748733));
#119107=CARTESIAN_POINT('Ctrl Pts',(-16.3230511148663,19.8676111981466,
-16.2748906815548));
#119108=CARTESIAN_POINT('Ctrl Pts',(-16.8768929890729,17.5391847164761,
-16.4020664882362));
#119109=CARTESIAN_POINT('Ctrl Pts',(-19.1345152807445,16.7445449928796,
-16.5292422949176));
#119110=CARTESIAN_POINT('Ctrl Pts',(-21.0246896611148,18.2127246528537,
-16.656418101599));
#119111=CARTESIAN_POINT('Ctrl Pts',(-20.8132984536472,20.5967599838785,
-16.7835939082805));
#119112=CARTESIAN_POINT('Ctrl Pts',(-18.6942799707749,21.7094465396596,
-16.9107697149619));
#119113=CARTESIAN_POINT('Ctrl Pts',(-16.6117021494137,20.5299634663839,
-17.0379455216434));
#119114=CARTESIAN_POINT('Ctrl Pts',(-16.4762008813049,18.1404132768064,
-17.1651213283248));
#119115=CARTESIAN_POINT('Ctrl Pts',(-18.4120901697813,16.7330599576527,
-17.2922971350062));
#119116=CARTESIAN_POINT('Ctrl Pts',(-20.6433117475059,17.5990628290491,
-17.4194729416877));
#119117=CARTESIAN_POINT('Ctrl Pts',(-21.1228583021457,19.9439180066875,
-17.5466487483691));
#119118=CARTESIAN_POINT('Ctrl Pts',(-19.4107756338348,21.6163664032144,
-17.6738245550505));
#119119=CARTESIAN_POINT('Ctrl Pts',(-17.0777933269134,21.0820404186637,
-17.801000361732));
#119120=CARTESIAN_POINT('Ctrl Pts',(-16.2642778467699,18.8311509798632,
-17.9281761684134));
#119121=CARTESIAN_POINT('Ctrl Pts',(-17.7165791539697,16.9287494409323,
-18.0553519750948));
#119122=CARTESIAN_POINT('Ctrl Pts',(-20.1023009391443,17.1201711375333,
-18.1825277817763));
#119123=CARTESIAN_POINT('Ctrl Pts',(-21.2326915389853,19.2297985439103,
-18.3097035884577));
#119124=CARTESIAN_POINT('Ctrl Pts',(-20.0706877380999,21.3221794531393,
-18.4368793951392));
#119125=CARTESIAN_POINT('Ctrl Pts',(-17.6823559016955,21.4776842484555,
-18.5640552018205));
#119126=CARTESIAN_POINT('Ctrl Pts',(-16.2588422531106,19.5536469325526,
-18.691231008502));
#119127=CARTESIAN_POINT('Ctrl Pts',(-17.1061322116441,17.3152523222366,
-18.8184068151834));
#119128=CARTESIAN_POINT('Ctrl Pts',(-19.4468898291958,16.8160885445611,
-18.9455826218649));
#119129=CARTESIAN_POINT('Ctrl Pts',(-21.1336152752557,18.5141073790766,
-19.0727584285463));
#119130=CARTESIAN_POINT('Ctrl Pts',(-20.6188426434545,20.8514819454316,
-19.1999342352277));
#119131=CARTESIAN_POINT('Ctrl Pts',(-18.3748438723008,21.6838161347437,
-19.3271100419092));
#119132=CARTESIAN_POINT('Ctrl Pts',(-16.4603485575527,20.2474950236424,
-19.4542858485906));
#119133=CARTESIAN_POINT('Ctrl Pts',(-16.6317873206282,17.8602540162898,
-19.5814616552721));
#119134=CARTESIAN_POINT('Ctrl Pts',(-18.7318757426506,16.712238697405,-19.7086374619535));
#119135=CARTESIAN_POINT('Ctrl Pts',(-20.833913031897,17.8566816189236,-19.8358132686349));
#119136=CARTESIAN_POINT('Ctrl Pts',(-21.0094104632606,20.243627912838,-19.9629890753163));
#119137=CARTESIAN_POINT('Ctrl Pts',(-19.0973599963134,21.6832015794576,
-20.0901648819978));
#119138=CARTESIAN_POINT('Ctrl Pts',(-16.8519493358426,20.8546849133278,
-20.2173406886792));
#119139=CARTESIAN_POINT('Ctrl Pts',(-16.3332032493219,18.5181870950206,
-20.3445164953606));
#119140=CARTESIAN_POINT('Ctrl Pts',(-18.0170393585529,16.817306476565,-20.4716923020421));
#119141=CARTESIAN_POINT('Ctrl Pts',(-20.3586419958767,17.3124826941761,
-20.5988681087235));
#119142=CARTESIAN_POINT('Ctrl Pts',(-21.2097371339674,19.5494468956883,
-20.726043915405));
#119143=CARTESIAN_POINT('Ctrl Pts',(-19.7894957733326,21.4758758768998,
-20.8532197220864));
#119144=CARTESIAN_POINT('Ctrl Pts',(-17.4009051340672,21.3244819367018,
-20.9803955287679));
#119145=CARTESIAN_POINT('Ctrl Pts',(-16.2353413176302,19.2339836436119,
-21.1075713354492));
#119146=CARTESIAN_POINT('Ctrl Pts',(-17.3621513466646,17.1226225346138,
-21.2347471421307));
#119147=CARTESIAN_POINT('Ctrl Pts',(-19.7475288817995,16.9267879000082,
-21.3619229488121));
#119148=CARTESIAN_POINT('Ctrl Pts',(-21.2030922899096,18.82740543638,-21.4890987554935));
#119149=CARTESIAN_POINT('Ctrl Pts',(-20.3933470809866,21.078346232667,-21.616274562175));
#119150=CARTESIAN_POINT('Ctrl Pts',(-18.0613964188678,21.6192244017756,
-21.7434503688564));
#119151=CARTESIAN_POINT('Ctrl Pts',(-16.3459141263638,19.9442123227787,
-21.8706448328923));
#119152=CARTESIAN_POINT('Ctrl Pts',(-16.6641680142473,18.3882311218014,
-21.9554473613676));
#119153=CARTESIAN_POINT('Ctrl Pts',(-17.1175857116532,17.849828040304,-21.9978579542825));
#119154=CARTESIAN_POINT('Ctrl Pts',(-19.3957372685685,16.7380050975816,
1.23230418924702E-15));
#119155=CARTESIAN_POINT('Ctrl Pts',(-19.4773890628972,16.7675693190178,
-4.67334893926385E-15));
#119156=CARTESIAN_POINT('Ctrl Pts',(-19.5571491449815,16.8015339789002,
-1.47154927005622E-14));
#119157=CARTESIAN_POINT('Ctrl Pts',(-19.6348154881073,16.8395812463466,
-1.46480050311482E-14));
#119158=CARTESIAN_POINT('Ctrl Pts',(-19.7143271339384,16.8785324925657,
-1.45789138978149E-14));
#119159=CARTESIAN_POINT('Ctrl Pts',(-19.791645087401,16.921763301817,-1.99347487809546E-15));
#119160=CARTESIAN_POINT('Ctrl Pts',(-19.8665231354225,16.9689790854406,
-1.5404344466674E-15));
#119161=CARTESIAN_POINT('Ctrl Pts',(-19.9365885602911,17.0131601775965,
-1.1165122004366E-15));
#119162=CARTESIAN_POINT('Ctrl Pts',(-20.0045177778059,17.0608314259461,
-4.38762558481736E-15));
#119163=CARTESIAN_POINT('Ctrl Pts',(-20.0700782293505,17.1117789745462,
-6.47398801234544E-15));
#119164=CARTESIAN_POINT('Ctrl Pts',(-20.0997466327889,17.1348345269478,
-7.67905425978548E-15));
#119165=CARTESIAN_POINT('Ctrl Pts',(-20.1289294943527,17.1585613303937,
-2.17441215594909E-14));
#119166=CARTESIAN_POINT('Ctrl Pts',(-20.1576028725501,17.1829408480985,
-1.05609965217468E-14));
#119167=CARTESIAN_POINT('Ctrl Pts',(-20.1753080913464,17.197994696729,-3.771524073573E-15));
#119168=CARTESIAN_POINT('Ctrl Pts',(-20.192819023282,17.213297426603,2.39813803353757E-14));
#119169=CARTESIAN_POINT('Ctrl Pts',(-20.2101297182957,17.228844786453,1.88737914186277E-14));
#119170=CARTESIAN_POINT('Ctrl Pts',(-20.2222917522923,17.2397679480536,
1.53214174626332E-14));
#119171=CARTESIAN_POINT('Ctrl Pts',(-20.2343567224894,17.2508136607941,
1.04616494884397E-14));
#119172=CARTESIAN_POINT('Ctrl Pts',(-20.2463056670645,17.2619643610397,
1.13103970633688E-14));
#119173=CARTESIAN_POINT('Ctrl Pts',(-20.309737445094,17.3211586052181,1.46542491453268E-14));
#119174=CARTESIAN_POINT('Ctrl Pts',(-20.3700068842138,17.3834001964164,
1.3331333505949E-14));
#119175=CARTESIAN_POINT('Ctrl Pts',(-20.4268834249918,17.4484109388489,
4.71844785465692E-16));
#119176=CARTESIAN_POINT('Ctrl Pts',(-20.4830375676453,17.5125959693487,
-1.22243134931973E-14));
#119177=CARTESIAN_POINT('Ctrl Pts',(-20.5358849034902,17.5794810921953,
4.32698449193755E-15));
#119178=CARTESIAN_POINT('Ctrl Pts',(-20.5851610289878,17.6488247163806,
4.9960036108132E-15));
#119179=CARTESIAN_POINT('Ctrl Pts',(-20.6305982574028,17.712766068494,5.61290224501695E-15));
#119180=CARTESIAN_POINT('Ctrl Pts',(-20.6729989034471,17.7787984983198,
1.74504747378125E-14));
#119181=CARTESIAN_POINT('Ctrl Pts',(-20.7121179763249,17.8467438133767,
-5.41233724504764E-16));
#119182=CARTESIAN_POINT('Ctrl Pts',(-20.7284900279032,17.8751801775537,
-7.96914155170017E-15));
#119183=CARTESIAN_POINT('Ctrl Pts',(-20.7442868194365,17.9039516828061,
1.02457455428025E-15));
#119184=CARTESIAN_POINT('Ctrl Pts',(-20.7594882783128,17.9330455001009,
1.22540866343002E-14));
#119185=CARTESIAN_POINT('Ctrl Pts',(-20.7693449710067,17.9519100590029,
1.96618582104559E-14));
#119186=CARTESIAN_POINT('Ctrl Pts',(-20.7789513429732,17.970910128766,2.31589035439596E-14));
#119187=CARTESIAN_POINT('Ctrl Pts',(-20.7883016221878,17.9900422154472,
2.25791607633141E-14));
#119188=CARTESIAN_POINT('Ctrl Pts',(-20.7942275728048,18.0021676074567,
2.21995283693054E-14));
#119189=CARTESIAN_POINT('Ctrl Pts',(-20.8000468301417,18.0143382523374,
-7.82794172139843E-16));
#119190=CARTESIAN_POINT('Ctrl Pts',(-20.8057567255896,18.0265495880407,
-6.80011602582908E-16));
#119191=CARTESIAN_POINT('Ctrl Pts',(-20.8408822594586,18.1016699978184,
-4.24130062536125E-16));
#119192=CARTESIAN_POINT('Ctrl Pts',(-20.8718943559605,18.1783721483409,
-2.22042397420453E-14));
#119193=CARTESIAN_POINT('Ctrl Pts',(-20.8985462175416,18.2564274689474,
-7.57727214306669E-15));
#119194=CARTESIAN_POINT('Ctrl Pts',(-20.9251980791227,18.3344827895539,
7.49378466576201E-15));
#119195=CARTESIAN_POINT('Ctrl Pts',(-20.9474901778909,18.4138920100306,
4.88674281099961E-16));
#119196=CARTESIAN_POINT('Ctrl Pts',(-20.9651214076632,18.4944358221201,
-7.63278329429795E-15));
#119197=CARTESIAN_POINT('Ctrl Pts',(-20.9829513884047,18.5758875777237,
-1.55637816228118E-14));
#119198=CARTESIAN_POINT('Ctrl Pts',(-20.9960140913518,18.658500875996,1.15461163552663E-14));
#119199=CARTESIAN_POINT('Ctrl Pts',(-21.0043852377911,18.741883902842,4.69069227904129E-15));
#119200=CARTESIAN_POINT('Ctrl Pts',(-21.0073021823588,18.7709389037262,
2.30190453493397E-15));
#119201=CARTESIAN_POINT('Ctrl Pts',(-21.00964903562,18.8000872405097,2.61472081366534E-15));
#119202=CARTESIAN_POINT('Ctrl Pts',(-21.0114276099525,18.8293118127927,
5.68989300120393E-15));
#119203=CARTESIAN_POINT('Ctrl Pts',(-21.0124180861908,18.8455867830844,
7.40243597734682E-15));
#119204=CARTESIAN_POINT('Ctrl Pts',(-21.0132324466529,18.861889846349,1.06678997328114E-14));
#119205=CARTESIAN_POINT('Ctrl Pts',(-21.0138703004904,18.8781994766446,
7.41073868937292E-15));
#119206=CARTESIAN_POINT('Ctrl Pts',(-21.0156561554122,18.9238629685382,
-1.7086186600829E-15));
#119207=CARTESIAN_POINT('Ctrl Pts',(-21.0160589030104,18.9695495775744,
-5.36082417604155E-15));
#119208=CARTESIAN_POINT('Ctrl Pts',(-21.0151046780539,19.0152032729735,
-5.27355936696949E-16));
#119209=CARTESIAN_POINT('Ctrl Pts',(-21.0142961185276,19.0538877886947,
3.56826822819105E-15));
#119210=CARTESIAN_POINT('Ctrl Pts',(-21.0125130883006,19.0925470966385,
8.8757475914889E-15));
#119211=CARTESIAN_POINT('Ctrl Pts',(-21.0097683504117,19.1311426359222,
5.16253706450698E-15));
#119212=CARTESIAN_POINT('Ctrl Pts',(-21.0039587339496,19.2128354202505,
-2.62298544613293E-15));
#119213=CARTESIAN_POINT('Ctrl Pts',(-20.9938436162584,19.2942438410435,
-1.34729324233074E-14));
#119214=CARTESIAN_POINT('Ctrl Pts',(-20.9795069236666,19.3749917573276,
2.08166817117217E-15));
#119215=CARTESIAN_POINT('Ctrl Pts',(-20.9654095554313,19.4543917376786,
1.73766137054392E-14));
#119216=CARTESIAN_POINT('Ctrl Pts',(-20.9472298872587,19.5331539565538,
-1.43672378246897E-15));
#119217=CARTESIAN_POINT('Ctrl Pts',(-20.9250049246735,19.6108953906176,
-1.52655665885959E-15));
#119218=CARTESIAN_POINT('Ctrl Pts',(-20.9157258007275,19.6433531461548,
-1.56406270150217E-15));
#119219=CARTESIAN_POINT('Ctrl Pts',(-20.9057410485004,19.6756325821129,
-2.56785656981742E-15));
#119220=CARTESIAN_POINT('Ctrl Pts',(-20.8950514018658,19.7077039335531,
4.57966997657877E-15));
#119221=CARTESIAN_POINT('Ctrl Pts',(-20.8895107318069,19.72432719368,8.10553462204269E-15));
#119222=CARTESIAN_POINT('Ctrl Pts',(-20.8837798046829,19.7408965824585,
-8.47385102258745E-15));
#119223=CARTESIAN_POINT('Ctrl Pts',(-20.8778666060763,19.757386588617,-4.9960036108132E-15));
#119224=CARTESIAN_POINT('Ctrl Pts',(-20.8511334429462,19.8319367693201,
1.07200736924069E-14));
#119225=CARTESIAN_POINT('Ctrl Pts',(-20.8206474027028,19.9049627949995,
1.69200158934511E-14));
#119226=CARTESIAN_POINT('Ctrl Pts',(-20.7864673380873,19.9761054066943,
1.74860126378462E-14));
#119227=CARTESIAN_POINT('Ctrl Pts',(-20.7601551358713,20.0308717977514,
1.79217233645422E-14));
#119228=CARTESIAN_POINT('Ctrl Pts',(-20.7316529099465,20.0845216847886,
1.90313142705558E-16));
#119229=CARTESIAN_POINT('Ctrl Pts',(-20.7009723060731,20.1368764894501,
-6.60582699651968E-15));
#119230=CARTESIAN_POINT('Ctrl Pts',(-20.6917380360057,20.1526342759514,
-8.36889325698314E-15));
#119231=CARTESIAN_POINT('Ctrl Pts',(-20.6823063437492,20.1682746386422,
-7.8227685048287E-15));
#119232=CARTESIAN_POINT('Ctrl Pts',(-20.6726773354748,20.1837924272005,
6.38378239159465E-15));
#119233=CARTESIAN_POINT('Ctrl Pts',(-20.6644524181989,20.1970474295393,
1.8695920822413E-14));
#119234=CARTESIAN_POINT('Ctrl Pts',(-20.6560858012134,20.2102092325172,
-1.06494413537713E-14));
#119235=CARTESIAN_POINT('Ctrl Pts',(-20.64758209464,20.2232683236723,-1.08524300657109E-14));
#119236=CARTESIAN_POINT('Ctrl Pts',(-20.6064305700017,20.2864644731141,
-1.1070441092253E-14));
#119237=CARTESIAN_POINT('Ctrl Pts',(-20.5620419244788,20.3473056726972,
-5.11924385313933E-15));
#119238=CARTESIAN_POINT('Ctrl Pts',(-20.5144495335262,20.4054521925719,
-8.82627304576999E-15));
#119239=CARTESIAN_POINT('Ctrl Pts',(-20.4703173116583,20.4593712133354,
-1.25884914482375E-14));
#119240=CARTESIAN_POINT('Ctrl Pts',(-20.4234297145935,20.5109732585207,
9.12964091805133E-15));
#119241=CARTESIAN_POINT('Ctrl Pts',(-20.3737907847676,20.5599542646918,
6.32827124036339E-15));
#119242=CARTESIAN_POINT('Ctrl Pts',(-20.3682022242118,20.5654687534213,
6.19434691003275E-15));
#119243=CARTESIAN_POINT('Ctrl Pts',(-20.3625787693224,20.5709499818026,
2.24934943646516E-15));
#119244=CARTESIAN_POINT('Ctrl Pts',(-20.3569207886222,20.5763978007994,
-2.27595720048157E-15));
#119245=CARTESIAN_POINT('Ctrl Pts',(20.3504145334569,20.5721720813046,-0.0021418961558211));
#119246=CARTESIAN_POINT('Ctrl Pts',(20.8038322552136,20.0337689331937,-0.0445524877679966));
#119247=CARTESIAN_POINT('Ctrl Pts',(21.1220877011301,18.4777891502142,-0.12935501494065));
#119248=CARTESIAN_POINT('Ctrl Pts',(19.4066027174179,16.8027744939582,-0.256549477673783));
#119249=CARTESIAN_POINT('Ctrl Pts',(17.0746532806956,17.3436542441791,-0.383725284355217));
#119250=CARTESIAN_POINT('Ctrl Pts',(16.2649072910693,19.5945942026566,-0.510901091036651));
#119251=CARTESIAN_POINT('Ctrl Pts',(17.7204711796095,21.4952124979738,-0.638076897718085));
#119252=CARTESIAN_POINT('Ctrl Pts',(20.1058486786829,21.2993774626889,-0.765252704399521));
#119253=CARTESIAN_POINT('Ctrl Pts',(21.2326588902647,19.1880164416469,-0.892428511080953));
#119254=CARTESIAN_POINT('Ctrl Pts',(20.06709493847,17.0975178673283,-1.01960431776238));
#119255=CARTESIAN_POINT('Ctrl Pts',(17.6785041641668,16.9461239968056,-1.14678012444382));
#119256=CARTESIAN_POINT('Ctrl Pts',(16.2582626906796,18.8725530643131,-1.27395593112525));
#119257=CARTESIAN_POINT('Ctrl Pts',(17.1093578952725,21.1095174457448,-1.40113173780669));
#119258=CARTESIAN_POINT('Ctrl Pts',(19.4509606892502,21.6046936825495,-1.52830754448812));
#119259=CARTESIAN_POINT('Ctrl Pts',(21.1347969163821,19.9038129555627,-1.65548335116956));
#119260=CARTESIAN_POINT('Ctrl Pts',(20.6160507930577,17.5673149720866,-1.78265915785099));
#119261=CARTESIAN_POINT('Ctrl Pts',(18.3706399789337,16.7387982516159,-1.90983496453243));
#119262=CARTESIAN_POINT('Ctrl Pts',(16.4585893803026,18.1783720157104,-2.03701077121386));
#119263=CARTESIAN_POINT('Ctrl Pts',(16.6340868238919,20.5653184744001,-2.16418657789529));
#119264=CARTESIAN_POINT('Ctrl Pts',(18.7361242574646,21.709761474113,-2.29136238457673));
#119265=CARTESIAN_POINT('Ctrl Pts',(20.8362128238147,20.5617460765933,-2.41853819125816));
#119266=CARTESIAN_POINT('Ctrl Pts',(21.0076515986441,18.1745049051026,-2.54571399793959));
#119267=CARTESIAN_POINT('Ctrl Pts',(19.0931561523786,16.7381836953926,-2.67288980462103));
#119268=CARTESIAN_POINT('Ctrl Pts',(16.84915722705,17.5705179418497,-2.80006561130246));
#119269=CARTESIAN_POINT('Ctrl Pts',(16.3343845598861,19.9078926688087,-2.9272414179839));
#119270=CARTESIAN_POINT('Ctrl Pts',(18.021110121826,21.605911619971,-3.05441722466533));
#119271=CARTESIAN_POINT('Ctrl Pts',(20.3618679001945,21.1067478080081,-3.18159303134677));
#119272=CARTESIAN_POINT('Ctrl Pts',(21.2091579169385,18.8683530439058,-3.3087688380282));
#119273=CARTESIAN_POINT('Ctrl Pts',(19.7856441705552,16.9443155958186,-3.43594464470964));
#119274=CARTESIAN_POINT('Ctrl Pts',(17.3973121700664,17.0998204018171,-3.56312045139107));
#119275=CARTESIAN_POINT('Ctrl Pts',(16.2353082893486,19.1922014547983,-3.69029625807251));
#119276=CARTESIAN_POINT('Ctrl Pts',(17.3656989668499,21.3018290061115,-3.81747206475393));
#119277=CARTESIAN_POINT('Ctrl Pts',(19.7514209159292,21.4932507158639,-3.94464787143538));
#119278=CARTESIAN_POINT('Ctrl Pts',(21.2037223229058,19.5908490462334,-4.0718236781168));
#119279=CARTESIAN_POINT('Ctrl Pts',(20.390206786872,17.3399594527915,-4.19899948479825));
#119280=CARTESIAN_POINT('Ctrl Pts',(18.0572243196692,16.8056334315311,-4.32617529147967));
#119281=CARTESIAN_POINT('Ctrl Pts',(16.345141533734,18.4780819429591,-4.45335109816111));
#119282=CARTESIAN_POINT('Ctrl Pts',(16.8246881213196,20.8229372816948,-4.58052690484254));
#119283=CARTESIAN_POINT('Ctrl Pts',(19.0559098523345,21.6889402125877,-4.70770271152398));
#119284=CARTESIAN_POINT('Ctrl Pts',(20.9917992738112,20.2815867967456,-4.83487851820542));
#119285=CARTESIAN_POINT('Ctrl Pts',(20.8562979963933,17.8920364430003,-4.96205432488684));
#119286=CARTESIAN_POINT('Ctrl Pts',(18.7737200319539,16.7125532886911,-5.0892301315683));
#119287=CARTESIAN_POINT('Ctrl Pts',(16.6547014035,17.8252399209163,-5.21640593824971));
#119288=CARTESIAN_POINT('Ctrl Pts',(16.4433101815092,20.2092754157301,-5.34358174493116));
#119289=CARTESIAN_POINT('Ctrl Pts',(18.3334846917389,21.6774551765717,-5.47075755161258));
#119290=CARTESIAN_POINT('Ctrl Pts',(20.5911071385146,20.8828153983818,-5.59793335829403));
#119291=CARTESIAN_POINT('Ctrl Pts',(21.1449490507717,18.5543887567427,-5.72510916497545));
#119292=CARTESIAN_POINT('Ctrl Pts',(19.48689484932,16.8283621769022,-5.85228497165689));
#119293=CARTESIAN_POINT('Ctrl Pts',(17.1381063535418,17.2882579165725,-5.97946077833832));
#119294=CARTESIAN_POINT('Ctrl Pts',(16.2534512260582,19.5121501789549,-6.10663658501977));
#119295=CARTESIAN_POINT('Ctrl Pts',(17.6445456384458,21.4597558436343,-6.23381239170119));
#119296=CARTESIAN_POINT('Ctrl Pts',(20.0351468083957,21.3442675953078,-6.36098819838263));
#119297=CARTESIAN_POINT('Ctrl Pts',(21.2320265399213,19.271638733806,-6.48816400506407));
#119298=CARTESIAN_POINT('Ctrl Pts',(20.1371219660819,17.1433775977014,-6.6153398117455));
#119299=CARTESIAN_POINT('Ctrl Pts',(17.7549400759333,16.9120316845865,-6.74251561842693));
#119300=CARTESIAN_POINT('Ctrl Pts',(16.2709848988036,18.7898465107973,-6.86969142510836));
#119301=CARTESIAN_POINT('Ctrl Pts',(17.0466932050637,21.0540435236181,-6.99686723178981));
#119302=CARTESIAN_POINT('Ctrl Pts',(19.3704007696072,21.6273624957014,-7.12404303847125));
#119303=CARTESIAN_POINT('Ctrl Pts',(21.1102501275226,19.9838188543493,-7.25121884515265));
#119304=CARTESIAN_POINT('Ctrl Pts',(20.6700374801522,17.6312618806795,-7.37839465183411));
#119305=CARTESIAN_POINT('Ctrl Pts',(18.4536306087803,16.7280165818806,-7.50557045851553));
#119306=CARTESIAN_POINT('Ctrl Pts',(16.4944452521654,18.1027544578749,-7.63274626519699));
#119307=CARTESIAN_POINT('Ctrl Pts',(16.5899123742445,20.494238833293,-7.75992207187839));
#119308=CARTESIAN_POINT('Ctrl Pts',(18.6524468158679,21.7084312259493,-7.88709787855984));
#119309=CARTESIAN_POINT('Ctrl Pts',(20.7898012421711,20.6313854768606,-8.01427368524127));
#119310=CARTESIAN_POINT('Ctrl Pts',(21.0410856261975,18.2512242118175,-8.14144949192272));
#119311=CARTESIAN_POINT('Ctrl Pts',(19.175762142071,16.7515976620282,-8.26862529860413));
#119312=CARTESIAN_POINT('Ctrl Pts',(16.9051493114451,17.5083201096033,-8.39580110528559));
#119313=CARTESIAN_POINT('Ctrl Pts',(16.3123934762929,19.827145676385,-8.52297691196702));
#119314=CARTESIAN_POINT('Ctrl Pts',(17.9413113247901,21.580695827397,-8.65015271864845));
#119315=CARTESIAN_POINT('Ctrl Pts',(20.2974718329846,21.1601971366828,-8.77732852532987));
#119316=CARTESIAN_POINT('Ctrl Pts',(21.2192439744216,18.9514310538806,-8.90450433201132));
#119317=CARTESIAN_POINT('Ctrl Pts',(19.8609590209642,16.9808033684772,-9.03168013869275));
#119318=CARTESIAN_POINT('Ctrl Pts',(17.4687591127375,17.0562426708819,-9.1588559453742));
#119319=CARTESIAN_POINT('Ctrl Pts',(16.2373391888682,19.1085380834297,-9.28603175205561));
#119320=CARTESIAN_POINT('Ctrl Pts',(17.296450598966,21.2548359449271,-9.41320755873705));
#119321=CARTESIAN_POINT('Ctrl Pts',(19.6744243601341,21.526041181719,-9.54038336541849));
#119322=CARTESIAN_POINT('Ctrl Pts',(21.1896171401977,19.6733398219446,-9.66755917209992));
#119323=CARTESIAN_POINT('Ctrl Pts',(20.4519336069186,17.3964703715815,-9.79473497878134));
#119324=CARTESIAN_POINT('Ctrl Pts',(18.1381526162766,16.7843192328824,-9.9219107854628));
#119325=CARTESIAN_POINT('Ctrl Pts',(16.3710246177412,18.3984970812188,-10.0490865921442));
#119326=CARTESIAN_POINT('Ctrl Pts',(16.7717798696356,20.7580959279184,-10.1762623988257));
#119327=CARTESIAN_POINT('Ctrl Pts',(18.9727503020227,21.6983302843557,-10.3034382055071));
#119328=CARTESIAN_POINT('Ctrl Pts',(20.9546821508189,20.356593486025,-10.4306140121885));
#119329=CARTESIAN_POINT('Ctrl Pts',(20.8992759573175,17.9638457678171,-10.5577898188699));
#119330=CARTESIAN_POINT('Ctrl Pts',(18.8573634651597,16.7152846505155,-10.6849656255514));
#119331=CARTESIAN_POINT('Ctrl Pts',(16.7022726505182,17.7563874648017,-10.8121414322328));
#119332=CARTESIAN_POINT('Ctrl Pts',(16.411165575805,20.1320069966963,-10.9393172389142));
#119333=CARTESIAN_POINT('Ctrl Pts',(18.2511149139269,21.6626597732632,-11.0664930455957));
#119334=CARTESIAN_POINT('Ctrl Pts',(20.5340813472922,20.9440668750279,-11.1936688522771));
#119335=CARTESIAN_POINT('Ctrl Pts',(21.1655848701657,18.635492685216,-11.3208446589586));
#119336=CARTESIAN_POINT('Ctrl Pts',(19.5662601958398,16.854910736706,-11.44802046564));
#119337=CARTESIAN_POINT('Ctrl Pts',(17.2033884477244,17.2358944518762,-11.5751962723214));
#119338=CARTESIAN_POINT('Ctrl Pts',(16.2447577983548,19.4289149185742,-11.7023720790029));
#119339=CARTESIAN_POINT('Ctrl Pts',(17.5698523691992,21.4220119728056,-11.8295478856843));
#119340=CARTESIAN_POINT('Ctrl Pts',(19.9629801361526,21.3866427728676,-11.9567236923657));
#119341=CARTESIAN_POINT('Ctrl Pts',(21.2285949072958,19.3552563644432,-12.0838994990471));
#119342=CARTESIAN_POINT('Ctrl Pts',(20.2055736830169,17.191523695202,-12.2110753057286));
#119343=CARTESIAN_POINT('Ctrl Pts',(17.8324749407335,16.8805351927773,-12.33825111241));
#119344=CARTESIAN_POINT('Ctrl Pts',(16.2864694853713,18.7076035060207,-12.4654269190915));
#119345=CARTESIAN_POINT('Ctrl Pts',(16.9859213663049,20.9965068581799,-12.5926027257729));
#119346=CARTESIAN_POINT('Ctrl Pts',(19.2891268956574,21.647318489013,-12.7197785324543));
#119347=CARTESIAN_POINT('Ctrl Pts',(21.0830379533052,20.0629591211559,-12.8469543391357));
#119348=CARTESIAN_POINT('Ctrl Pts',(20.7218524865336,17.6969801381849,-12.9741301458172));
#119349=CARTESIAN_POINT('Ctrl Pts',(18.5369357434076,16.7200204077588,-13.1013059524986));
#119350=CARTESIAN_POINT('Ctrl Pts',(16.5328132245178,18.0283798455839,-13.2284817591801));
#119351=CARTESIAN_POINT('Ctrl Pts',(16.5481429510737,20.4217198734009,-13.3556575658615));
#119352=CARTESIAN_POINT('Ctrl Pts',(18.5688608504302,21.7042995631227,-13.4828333725429));
#119353=CARTESIAN_POINT('Ctrl Pts',(20.7410836698255,20.6994316553031,-13.6100091792244));
#119354=CARTESIAN_POINT('Ctrl Pts',(21.0719317958176,18.3290200862303,-13.7371849859058));
#119355=CARTESIAN_POINT('Ctrl Pts',(19.2578726075595,16.7677703461939,-13.8643607925872));
#119356=CARTESIAN_POINT('Ctrl Pts',(16.9631928170665,17.4480321695901,-13.9915365992687));
#119357=CARTESIAN_POINT('Ctrl Pts',(16.2931187082259,19.7457075552633,-14.1187124059501));
#119358=CARTESIAN_POINT('Ctrl Pts',(17.862401686409,21.5528219466762,-14.2458882126315));
#119359=CARTESIAN_POINT('Ctrl Pts',(20.2313220198197,21.211460051876,-14.373064019313));
#119360=CARTESIAN_POINT('Ctrl Pts',(21.2265423343311,19.0348002220335,-14.5002398259944));
#119361=CARTESIAN_POINT('Ctrl Pts',(19.9350097617186,17.0197927522835,-14.6274156326758));
#119362=CARTESIAN_POINT('Ctrl Pts',(17.5416252758018,17.0150819306535,-14.7545914393573));
#119363=CARTESIAN_POINT('Ctrl Pts',(16.2421705922151,19.0249896436024,-14.8817672460387));
#119364=CARTESIAN_POINT('Ctrl Pts',(17.2288147298954,21.2055503134414,-15.0089430527202));
#119365=CARTESIAN_POINT('Ctrl Pts',(19.5963729305628,21.5562348664518,-15.1361188594016));
#119366=CARTESIAN_POINT('Ctrl Pts',(21.1727574923393,19.7553119911849,-15.263294666083));
#119367=CARTESIAN_POINT('Ctrl Pts',(20.5117334212554,17.455016647818,-15.3904704727644));
#119368=CARTESIAN_POINT('Ctrl Pts',(18.2197492747497,16.7657270414598,-15.5176462794459));
#119369=CARTESIAN_POINT('Ctrl Pts',(16.3995582506614,18.3198236038057,-15.6448220861273));
#119370=CARTESIAN_POINT('Ctrl Pts',(16.7210726397956,20.6915191970147,-15.7719978928088));
#119371=CARTESIAN_POINT('Ctrl Pts',(18.8893229455551,21.7049303183475,-15.8991736994902));
#119372=CARTESIAN_POINT('Ctrl Pts',(20.915074089197,20.4303151633691,-16.0263495061716));
#119373=CARTESIAN_POINT('Ctrl Pts',(20.9398251287258,18.0370540252336,-16.153525312853));
#119374=CARTESIAN_POINT('Ctrl Pts',(18.9408685215966,16.7208154556417,-16.2807011195345));
#119375=CARTESIAN_POINT('Ctrl Pts',(16.7521228856109,17.6891666472147,-16.4078769262159));
#119376=CARTESIAN_POINT('Ctrl Pts',(16.3816264929107,20.0537054843378,-16.5350527328974));
#119377=CARTESIAN_POINT('Ctrl Pts',(18.1692867881987,21.6451143437821,-16.6622285395788));
#119378=CARTESIAN_POINT('Ctrl Pts',(20.4750364052595,21.003374370981,-16.7894043462602));
#119379=CARTESIAN_POINT('Ctrl Pts',(21.1834931814011,18.7172421601046,-16.9165801529417));
#119380=CARTESIAN_POINT('Ctrl Pts',(19.6446919963,16.8841021212645,-17.0437559596231));
#119381=CARTESIAN_POINT('Ctrl Pts',(17.2703874285137,17.1857464625939,-17.1709317663045));
#119382=CARTESIAN_POINT('Ctrl Pts',(16.2388565530248,19.3454352230824,-17.298107572986));
#119383=CARTESIAN_POINT('Ctrl Pts',(17.4964649240676,21.3817880103836,-17.4252833796674));
#119384=CARTESIAN_POINT('Ctrl Pts',(19.8894349171892,21.4265775324573,-17.5524591863489));
#119385=CARTESIAN_POINT('Ctrl Pts',(21.2223650881681,19.4387121827512,-17.6796349930303));
#119386=CARTESIAN_POINT('Ctrl Pts',(20.272374736109,17.2419350387839,-17.8068107997117));
#119387=CARTESIAN_POINT('Ctrl Pts',(17.9110210459731,16.8516527827758,-17.9339866063932));
#119388=CARTESIAN_POINT('Ctrl Pts',(16.3046994663247,18.6259251609712,-18.0611624130746));
#119389=CARTESIAN_POINT('Ctrl Pts',(16.9271103469226,20.9369673901283,-18.188338219756));
#119390=CARTESIAN_POINT('Ctrl Pts',(19.2072303360084,21.6645416644746,-18.3155140264374));
#119391=CARTESIAN_POINT('Ctrl Pts',(21.053190863776,20.1411437456081,-18.4426898331189));
#119392=CARTESIAN_POINT('Ctrl Pts',(20.7714377192819,17.764396671431,-18.5698656398003));
#119393=CARTESIAN_POINT('Ctrl Pts',(18.6204619249281,16.7148183647849,-18.6970414464817));
#119394=CARTESIAN_POINT('Ctrl Pts',(16.5736502676105,17.9553317781408,-18.8242172531632));
#119395=CARTESIAN_POINT('Ctrl Pts',(16.5088254030919,20.347842849113,-18.9513930598446));
#119396=CARTESIAN_POINT('Ctrl Pts',(18.4854601217909,21.6973711671814,-19.078568866526));
#119397=CARTESIAN_POINT('Ctrl Pts',(20.6901147517246,20.7658082595486,-19.2057446732075));
#119398=CARTESIAN_POINT('Ctrl Pts',(21.100155508854,18.4078052787827,-19.3329204798889));
#119399=CARTESIAN_POINT('Ctrl Pts',(19.3393954434521,16.786683597609,-19.4600962865703));
#119400=CARTESIAN_POINT('Ctrl Pts',(17.02322264018,17.3897217556752,-19.5872720932518));
#119401=CARTESIAN_POINT('Ctrl Pts',(16.2765818693588,19.6636696421892,-19.7144478999332));
#119402=CARTESIAN_POINT('Ctrl Pts',(17.7844697326546,21.5223212653023,-19.8416237066147));
#119403=CARTESIAN_POINT('Ctrl Pts',(20.1634926358433,21.2604790121031,-19.9687995132961));
#119404=CARTESIAN_POINT('Ctrl Pts',(21.231044858401,19.1183671093666,-20.0959753199775));
#119405=CARTESIAN_POINT('Ctrl Pts',(20.0077132370737,17.0612398664333,-20.2231511266589));
#119406=CARTESIAN_POINT('Ctrl Pts',(17.6158291045619,16.976384633048,-20.3503269333404));
#119407=CARTESIAN_POINT('Ctrl Pts',(16.2497967346393,18.9416493085074,-20.4775027400218));
#119408=CARTESIAN_POINT('Ctrl Pts',(17.1628678921721,21.1540284415978,-20.6046785467032));
#119409=CARTESIAN_POINT('Ctrl Pts',(19.5173528955041,21.5837958860619,-20.7318543533847));
#119410=CARTESIAN_POINT('Ctrl Pts',(21.1531647607153,19.8366774894172,-20.8590301600661));
#119411=CARTESIAN_POINT('Ctrl Pts',(20.5695343937816,17.5155251277943,-20.9862059667476));
#119412=CARTESIAN_POINT('Ctrl Pts',(18.301931936395,16.7498921279798,-21.113381773429));
#119413=CARTESIAN_POINT('Ctrl Pts',(16.430692762331,18.2421219844588,-21.2405575801104));
#119414=CARTESIAN_POINT('Ctrl Pts',(16.6726573424412,20.6233352795928,-21.3677333867919));
#119415=CARTESIAN_POINT('Ctrl Pts',(18.8056557941431,21.7086298106478,-21.4949091934733));
#119416=CARTESIAN_POINT('Ctrl Pts',(20.8731458549779,20.5028678015929,-21.6220850001547));
#119417=CARTESIAN_POINT('Ctrl Pts',(20.9776565334948,18.111196073242,-21.7492608068362));
#119418=CARTESIAN_POINT('Ctrl Pts',(19.0246114642159,16.7298799538284,-21.8764366135176));
#119419=CARTESIAN_POINT('Ctrl Pts',(16.8032831853607,17.6222026293144,-22.0036124201991));
#119420=CARTESIAN_POINT('Ctrl Pts',(16.3565572075883,19.9774759742341,-22.1307882268804));
#119421=CARTESIAN_POINT('Ctrl Pts',(17.5080922618947,21.070504731278,-22.2155720980014));
#119422=CARTESIAN_POINT('Ctrl Pts',(18.1877583250969,21.2523734297384,-22.2579640335619));
#119423=CARTESIAN_POINT('Ctrl Pts',(20.4651728790455,20.6688093317616,0.084476493734548));
#119424=CARTESIAN_POINT('Ctrl Pts',(20.9507812712845,20.0921819204693,0.0420659021223723));
#119425=CARTESIAN_POINT('Ctrl Pts',(21.2916314586439,18.4257343942419,-0.0427366250502812));
#119426=CARTESIAN_POINT('Ctrl Pts',(19.4543545616952,16.6318010405789,-0.169931087783413));
#119427=CARTESIAN_POINT('Ctrl Pts',(16.9568469381246,17.2110808818736,-0.297106894464847));
#119428=CARTESIAN_POINT('Ctrl Pts',(16.0896125331239,19.6218277093859,-0.424282701146282));
#119429=CARTESIAN_POINT('Ctrl Pts',(17.6485150766254,21.6573815714476,-0.551458507827716));
#119430=CARTESIAN_POINT('Ctrl Pts',(20.203243920748,21.4476431071891,-0.67863431450915));
#119431=CARTESIAN_POINT('Ctrl Pts',(21.410052717468,19.1863847097626,-0.805810121190585));
#119432=CARTESIAN_POINT('Ctrl Pts',(20.1617388348746,16.9474699013169,-0.932985927872018));
#119433=CARTESIAN_POINT('Ctrl Pts',(17.6035685870678,16.7853277296908,-1.06016173455346));
#119434=CARTESIAN_POINT('Ctrl Pts',(16.0824961952363,18.8485248156151,-1.18733754123489));
#119435=CARTESIAN_POINT('Ctrl Pts',(16.994015428193,21.2443038613797,-1.31451334791632));
#119436=CARTESIAN_POINT('Ctrl Pts',(19.5018617550643,21.7746354401676,-1.44168915459776));
#119437=CARTESIAN_POINT('Ctrl Pts',(21.3052429724622,19.9529996381475,-1.56886496127919));
#119438=CARTESIAN_POINT('Ctrl Pts',(20.7496681485408,17.4506205409442,-1.69604076796063));
#119439=CARTESIAN_POINT('Ctrl Pts',(18.3448430103915,16.5632827654992,-1.82321657464206));
#119440=CARTESIAN_POINT('Ctrl Pts',(16.2970452015994,18.1050599558195,-1.9503923813235));
#119441=CARTESIAN_POINT('Ctrl Pts',(16.4850021943108,20.6614691488127,-2.07756818800493));
#119442=CARTESIAN_POINT('Ctrl Pts',(18.736275070432,21.8871625843198,-2.20474399468636));
#119443=CARTESIAN_POINT('Ctrl Pts',(20.9854607183013,20.6576431264228,-2.3319198013678));
#119444=CARTESIAN_POINT('Ctrl Pts',(21.1690708945641,18.1009182973116,-2.45909560804923));
#119445=CARTESIAN_POINT('Ctrl Pts',(19.1186546646734,16.5626245784783,-2.58627141473067));
#119446=CARTESIAN_POINT('Ctrl Pts',(16.7153416532344,17.4540509075189,-2.7134472214121));
#119447=CARTESIAN_POINT('Ctrl Pts',(16.1640223834416,19.9573689931488,-2.84062302809354));
#119448=CARTESIAN_POINT('Ctrl Pts',(17.9704980657522,21.7759398458068,-2.96779883477497));
#119449=CARTESIAN_POINT('Ctrl Pts',(20.4774393846103,21.2413375915055,-3.0949746414564));
#119450=CARTESIAN_POINT('Ctrl Pts',(21.3848832780629,18.8440266121716,-3.22215044813784));
#119451=CARTESIAN_POINT('Ctrl Pts',(19.8603062963049,16.7833909401617,-3.34932625481927));
#119452=CARTESIAN_POINT('Ctrl Pts',(17.3024131941191,16.9499359056603,-3.4765020615007));
#119453=CARTESIAN_POINT('Ctrl Pts',(16.0579121320417,19.1908668405009,-3.60367786818214));
#119454=CARTESIAN_POINT('Ctrl Pts',(17.268555592065,21.4502686994473,-3.73085367486357));
#119455=CARTESIAN_POINT('Ctrl Pts',(19.8236533406339,21.6552805114082,-3.85802948154501));
#119456=CARTESIAN_POINT('Ctrl Pts',(21.3790617806833,19.6178166632753,-3.98520528822644));
#119457=CARTESIAN_POINT('Ctrl Pts',(20.5077902080058,17.2071237764952,-4.11238109490788));
#119458=CARTESIAN_POINT('Ctrl Pts',(18.0091762133191,16.634862950186,-4.23955690158931));
#119459=CARTESIAN_POINT('Ctrl Pts',(16.1755430552745,18.4260479739882,-4.36673270827075));
#119460=CARTESIAN_POINT('Ctrl Pts',(16.6891353482686,20.9373777620364,-4.49390851495218));
#119461=CARTESIAN_POINT('Ctrl Pts',(19.0787640406122,21.8648631045058,-4.62108432163361));
#119462=CARTESIAN_POINT('Ctrl Pts',(21.1520931241638,20.3575937659115,-4.74826012831505));
#119463=CARTESIAN_POINT('Ctrl Pts',(21.0069718500806,17.7983958127287,-4.87543593499648));
#119464=CARTESIAN_POINT('Ctrl Pts',(18.7765399800919,16.5351745252634,-5.00261174167792));
#119465=CARTESIAN_POINT('Ctrl Pts',(16.5070803186978,17.7268570304097,-5.12978754835935));
#119466=CARTESIAN_POINT('Ctrl Pts',(16.280681246675,20.2801485938535,-5.25696335504078));
#119467=CARTESIAN_POINT('Ctrl Pts',(18.305049860693,21.8525626812824,-5.38413916172222));
#119468=CARTESIAN_POINT('Ctrl Pts',(20.722953603877,21.0015069625052,-5.51131496840365));
#119469=CARTESIAN_POINT('Ctrl Pts',(21.3161158638869,18.5077722370249,-5.63849077508509));
#119470=CARTESIAN_POINT('Ctrl Pts',(19.5403470829654,16.6592053368368,-5.76566658176652));
#119471=CARTESIAN_POINT('Ctrl Pts',(17.0248049009675,17.1517516578618,-5.89284238844796));
#119472=CARTESIAN_POINT('Ctrl Pts',(16.0773431377199,19.5335305214322,-6.02001819512939));
#119473=CARTESIAN_POINT('Ctrl Pts',(17.5671991548932,21.6194076500902,-6.14719400181082));
#119474=CARTESIAN_POINT('Ctrl Pts',(20.127522527624,21.4957202424278,-6.27436980849226));
#119475=CARTESIAN_POINT('Ctrl Pts',(21.4093754730223,19.2759438180688,-6.40154561517369));
#119476=CARTESIAN_POINT('Ctrl Pts',(20.2367374744517,16.9965854714996,-6.52872142185513));
#119477=CARTESIAN_POINT('Ctrl Pts',(17.6854311134782,16.7488150127633,-6.65589722853656));
#119478=CARTESIAN_POINT('Ctrl Pts',(16.0961216243634,18.7599464593815,-6.78307303521799));
#119479=CARTESIAN_POINT('Ctrl Pts',(16.9269018196985,21.1848915339771,-6.91024884189944));
#119480=CARTESIAN_POINT('Ctrl Pts',(19.4155824342976,21.7989136396743,-7.03742464858086));
#119481=CARTESIAN_POINT('Ctrl Pts',(21.2789534692056,20.0386856050059,-7.1646004552623));
#119482=CARTESIAN_POINT('Ctrl Pts',(20.8074876537439,17.5191073997068,-7.29177626194374));
#119483=CARTESIAN_POINT('Ctrl Pts',(18.4337256111302,16.551735644479,-7.41895206862516));
#119484=CARTESIAN_POINT('Ctrl Pts',(16.335446683174,18.0240738828814,-7.54612787530661));
#119485=CARTESIAN_POINT('Ctrl Pts',(16.4376915523973,20.5853431647969,-7.67330368198803));
#119486=CARTESIAN_POINT('Ctrl Pts',(18.64665689732,21.8857378943683,-7.80047948866947));
#119487=CARTESIAN_POINT('Ctrl Pts',(20.9357541178272,20.7322266188132,-7.92765529535091));
#119488=CARTESIAN_POINT('Ctrl Pts',(21.2048785915005,18.1830843384694,-8.05483110203234));
#119489=CARTESIAN_POINT('Ctrl Pts',(19.2071253174932,16.5769908779387,-8.18200690871378));
#119490=CARTESIAN_POINT('Ctrl Pts',(16.7753089301549,17.3874373018554,-8.3091827153952));
#119491=CARTESIAN_POINT('Ctrl Pts',(16.1404700293211,19.8708893182541,-8.43635852207665));
#119492=CARTESIAN_POINT('Ctrl Pts',(17.8850339039608,21.7489338425049,-8.56353432875807));
#119493=CARTESIAN_POINT('Ctrl Pts',(20.4084714789379,21.2985815881968,-8.69071013543951));
#119494=CARTESIAN_POINT('Ctrl Pts',(21.3956854014105,18.9330027966444,-8.81788594212095));
#119495=CARTESIAN_POINT('Ctrl Pts',(19.9409681709163,16.8224691847183,-8.94506174880238));
#119496=CARTESIAN_POINT('Ctrl Pts',(17.3789325564997,16.9032643468714,-9.07223755548381));
#119497=CARTESIAN_POINT('Ctrl Pts',(16.0600872165237,19.1012637365415,-9.19941336216525));
#119498=CARTESIAN_POINT('Ctrl Pts',(17.1943908936429,21.3999393369342,-9.32658916884668));
#119499=CARTESIAN_POINT('Ctrl Pts',(19.7411903669265,21.6903989565872,-9.45376497552812));
#119500=CARTESIAN_POINT('Ctrl Pts',(21.3639551918393,19.7061639224262,-9.58094078220955));
#119501=CARTESIAN_POINT('Ctrl Pts',(20.5738993616681,17.2676467227782,-9.70811658889098));
#119502=CARTESIAN_POINT('Ctrl Pts',(18.0958500641997,16.6120355368737,-9.83529239557241));
#119503=CARTESIAN_POINT('Ctrl Pts',(16.2032637247762,18.3408129359606,-9.96246820225386));
#119504=CARTESIAN_POINT('Ctrl Pts',(16.6324708426624,20.8679329564033,-10.0896440089353));
#119505=CARTESIAN_POINT('Ctrl Pts',(18.989700526796,21.8749198302035,-10.2168198156167));
#119506=CARTESIAN_POINT('Ctrl Pts',(21.1123408481587,20.4379256013037,-10.3439956222982));
#119507=CARTESIAN_POINT('Ctrl Pts',(21.0530010578169,17.8753032847989,-10.4711714289796));
#119508=CARTESIAN_POINT('Ctrl Pts',(18.8661217303663,16.5380998018032,-10.5983472356611));
#119509=CARTESIAN_POINT('Ctrl Pts',(16.5580289157041,17.6531163517569,-10.7255230423425));
#119510=CARTESIAN_POINT('Ctrl Pts',(16.2462545148863,20.1973944558094,-10.8526988490239));
#119511=CARTESIAN_POINT('Ctrl Pts',(18.2168321897617,21.8367168692014,-10.9798746557054));
#119512=CARTESIAN_POINT('Ctrl Pts',(20.6618792314763,21.0671070254696,-11.1070504623868));
#119513=CARTESIAN_POINT('Ctrl Pts',(21.3382167359914,18.5946341888639,-11.2342262690682));
#119514=CARTESIAN_POINT('Ctrl Pts',(19.6253470211541,16.6876387279989,-11.3614020757497));
#119515=CARTESIAN_POINT('Ctrl Pts',(17.0947217376433,17.0956706167312,-11.4885778824311));
#119516=CARTESIAN_POINT('Ctrl Pts',(16.0680325147611,19.4443859224641,-11.6157536891125));
#119517=CARTESIAN_POINT('Ctrl Pts',(17.487202990982,21.5789841299002,-11.742929495794));
#119518=CARTESIAN_POINT('Ctrl Pts',(20.0502323380272,21.5411038718235,-11.8701053024754));
#119519=CARTESIAN_POINT('Ctrl Pts',(21.4057002095246,19.3654979339054,-11.9972811091568));
#119520=CARTESIAN_POINT('Ctrl Pts',(20.3100489631999,17.0481497308524,-12.1244569158383));
#119521=CARTESIAN_POINT('Ctrl Pts',(17.7684706137698,16.715082408115,-12.2516327225197));
#119522=CARTESIAN_POINT('Ctrl Pts',(16.1127055486938,18.6718645618152,-12.3788085292011));
#119523=CARTESIAN_POINT('Ctrl Pts',(16.8618154468087,21.1232700175309,-12.5059843358826));
#119524=CARTESIAN_POINT('Ctrl Pts',(19.3285384715983,21.8202864210249,-12.633160142564));
#119525=CARTESIAN_POINT('Ctrl Pts',(21.2498093499156,20.1234444838084,-12.7603359492454));
#119526=CARTESIAN_POINT('Ctrl Pts',(20.8629812984238,17.5894913653894,-12.8875117559269));
#119527=CARTESIAN_POINT('Ctrl Pts',(18.5229450451101,16.5431717770494,-13.0146875626083));
#119528=CARTESIAN_POINT('Ctrl Pts',(16.37653861336,17.9444189991727,-13.1418633692897));
#119529=CARTESIAN_POINT('Ctrl Pts',(16.3929566832965,20.5076756766722,-13.2690391759712));
#119530=CARTESIAN_POINT('Ctrl Pts',(18.5571366947732,21.8813129015941,-13.3962149826526));
#119531=CARTESIAN_POINT('Ctrl Pts',(20.8835778114207,20.8051037776138,-13.523390789334));
#119532=CARTESIAN_POINT('Ctrl Pts',(21.2379147039354,18.2664033789119,-13.6505665960155));
#119533=CARTESIAN_POINT('Ctrl Pts',(19.2950652660628,16.5943117517799,-13.7777424026969));
#119534=CARTESIAN_POINT('Ctrl Pts',(16.8374732702154,17.3228691824008,-13.9049182093783));
#119535=CARTESIAN_POINT('Ctrl Pts',(16.119826837221,19.7836694475537,-14.0320940160598));
#119536=CARTESIAN_POINT('Ctrl Pts',(17.800522027191,21.7190810384507,-14.1592698227412));
#119537=CARTESIAN_POINT('Ctrl Pts',(20.337625319036,21.3534839456345,-14.2864456294226));
#119538=CARTESIAN_POINT('Ctrl Pts',(21.4035019128779,19.0222908102495,-14.4136214361041));
#119539=CARTESIAN_POINT('Ctrl Pts',(20.0202761896291,16.8642266438473,-14.5407972427855));
#119540=CARTESIAN_POINT('Ctrl Pts',(17.4569718976996,16.8591813745337,-14.667973049467));
#119541=CARTESIAN_POINT('Ctrl Pts',(16.0652616283277,19.011783723759,-14.7951488561484));
#119542=CARTESIAN_POINT('Ctrl Pts',(17.1219531743809,21.347154641679,-14.9223246628298));
#119543=CARTESIAN_POINT('Ctrl Pts',(19.6575976280295,21.7227362605683,-15.0495004695112));
#119544=CARTESIAN_POINT('Ctrl Pts',(21.3458985828949,19.7939557563202,-15.1766762761927));
#119545=CARTESIAN_POINT('Ctrl Pts',(20.6379447006631,17.3303495279633,-15.3038520828741));
#119546=CARTESIAN_POINT('Ctrl Pts',(18.1832397277084,16.5921233813674,-15.4310278895556));
#119547=CARTESIAN_POINT('Ctrl Pts',(16.2338231205434,18.2565539865522,-15.558203696237));
#119548=CARTESIAN_POINT('Ctrl Pts',(16.5781636218018,20.7966295694748,-15.6853795029184));
#119549=CARTESIAN_POINT('Ctrl Pts',(18.9003501937609,21.8819884376745,-15.8125553095998));
#119550=CARTESIAN_POINT('Ctrl Pts',(21.0699207878016,20.5168811945468,-15.9397311162813));
#119551=CARTESIAN_POINT('Ctrl Pts',(21.0964290426296,17.9537090075503,-16.0669069229627));
#119552=CARTESIAN_POINT('Ctrl Pts',(18.9555552797279,16.5440232698465,-16.1940827296442));
#119553=CARTESIAN_POINT('Ctrl Pts',(16.6114182989473,17.5811231508143,-16.3212585363256));
#119554=CARTESIAN_POINT('Ctrl Pts',(16.2146182866043,20.1135338793437,-16.448434343007));
#119555=CARTESIAN_POINT('Ctrl Pts',(18.1291946258374,21.8179257911455,-16.5756101496885));
#119556=CARTESIAN_POINT('Ctrl Pts',(20.5986423574096,21.1306250936339,-16.7027859563699));
#119557=CARTESIAN_POINT('Ctrl Pts',(21.3573964588152,18.6821875180837,-16.8299617630513));
#119558=CARTESIAN_POINT('Ctrl Pts',(19.7093471356056,16.7189025728874,-16.9571375697328));
#119559=CARTESIAN_POINT('Ctrl Pts',(17.1664773523482,17.0419623400562,-17.0843133764142));
#119560=CARTESIAN_POINT('Ctrl Pts',(16.0617123068835,19.3549795345634,-17.2114891830956));
#119561=CARTESIAN_POINT('Ctrl Pts',(17.4086053589731,21.5359044424863,-17.3386649897771));
#119562=CARTESIAN_POINT('Ctrl Pts',(19.9714657309362,21.5838738242719,-17.4658407964585));
#119563=CARTESIAN_POINT('Ctrl Pts',(21.3990281005501,19.4548787494468,-17.5930166031399));
#119564=CARTESIAN_POINT('Ctrl Pts',(20.3815925982089,17.1021400588277,-17.7201924098214));
#119565=CARTESIAN_POINT('Ctrl Pts',(17.8525931481391,16.6841494736224,-17.8473682165028));
#119566=CARTESIAN_POINT('Ctrl Pts',(16.1322297783753,18.5843874123414,-17.9745440231842));
#119567=CARTESIAN_POINT('Ctrl Pts',(16.7988291028752,21.0595035082658,-18.1017198298657));
#119568=CARTESIAN_POINT('Ctrl Pts',(19.240827615245,21.8387323664388,-18.2288956365471));
#119569=CARTESIAN_POINT('Ctrl Pts',(21.2178432478782,20.2071798738389,-18.3560714432285));
#119570=CARTESIAN_POINT('Ctrl Pts',(20.9160868653179,17.661694176945,-18.48324724991));
#119571=CARTESIAN_POINT('Ctrl Pts',(18.6124012193438,16.53760041183,-18.6104230565914));
#119572=CARTESIAN_POINT('Ctrl Pts',(16.4202749074846,17.8661848391805,-18.7375988632728));
#119573=CARTESIAN_POINT('Ctrl Pts',(16.3508477617745,20.4285537075334,-18.8647746699543));
#119574=CARTESIAN_POINT('Ctrl Pts',(18.4678148800254,21.8738926199146,-18.9919504766357));
#119575=CARTESIAN_POINT('Ctrl Pts',(20.8289903235801,20.8761928297688,-19.1191262833172));
#119576=CARTESIAN_POINT('Ctrl Pts',(21.2681421768659,18.3507819747449,-19.2463020899985));
#119577=CARTESIAN_POINT('Ctrl Pts',(19.3823758659115,16.6145677611307,-19.37347789668));
#119578=CARTESIAN_POINT('Ctrl Pts',(16.901764947602,17.260418984728,-19.5006537033614));
#119579=CARTESIAN_POINT('Ctrl Pts',(16.1021159552911,19.6958072023018,-19.6278295100429));
#119580=CARTESIAN_POINT('Ctrl Pts',(17.71705724637,21.6864149424128,-19.7550053167243));
#119581=CARTESIAN_POINT('Ctrl Pts',(20.2649803461583,21.4059830371408,-19.8821811234057));
#119582=CARTESIAN_POINT('Ctrl Pts',(21.4083240964178,19.11179058023,-20.0093569300872));
#119583=CARTESIAN_POINT('Ctrl Pts',(20.0981412930058,16.9086163213996,-20.1365327367686));
#119584=CARTESIAN_POINT('Ctrl Pts',(17.5364438729955,16.8177367384453,-20.2637085434501));
#119585=CARTESIAN_POINT('Ctrl Pts',(16.0734291934315,18.9225265902324,-20.3908843501315));
#119586=CARTESIAN_POINT('Ctrl Pts',(17.051324400287,21.2919749428039,-20.5180601568129));
#119587=CARTESIAN_POINT('Ctrl Pts',(19.5729675169019,21.7522539917445,-20.6452359634943));
#119588=CARTESIAN_POINT('Ctrl Pts',(21.3249148532192,19.8810978482246,-20.7724117701758));
#119589=CARTESIAN_POINT('Ctrl Pts',(20.6998492888418,17.3951538447513,-20.8995875768572));
#119590=CARTESIAN_POINT('Ctrl Pts',(18.2712569980454,16.5751642584499,-21.0267633835387));
#119591=CARTESIAN_POINT('Ctrl Pts',(16.2671680460494,18.173335892872,-21.1539391902201));
#119592=CARTESIAN_POINT('Ctrl Pts',(16.5263110505858,20.7236048928311,-21.2811149969015));
#119593=CARTESIAN_POINT('Ctrl Pts',(18.8107430413917,21.8859505777098,-21.408290803583));
#119594=CARTESIAN_POINT('Ctrl Pts',(21.0250158327644,20.594584752017,-21.5354666102644));
#119595=CARTESIAN_POINT('Ctrl Pts',(21.1369463112861,18.033114815932,-21.6626424169459));
#119596=CARTESIAN_POINT('Ctrl Pts',(19.045243604148,16.5537313076661,-21.7898182236272));
#119597=CARTESIAN_POINT('Ctrl Pts',(16.6662107556949,17.5094049812102,-21.9169940303087));
#119598=CARTESIAN_POINT('Ctrl Pts',(16.1877691919268,20.0318924082093,-22.0441698369901));
#119599=CARTESIAN_POINT('Ctrl Pts',(17.4210581868123,21.2025214152156,-22.1289537081111));
#119600=CARTESIAN_POINT('Ctrl Pts',(18.1489775608771,21.3973019939627,-22.1713456436716));
#119601=CARTESIAN_POINT('Ctrl Pts',(20.579931224634,20.7654465822185,0.171094883624917));
#119602=CARTESIAN_POINT('Ctrl Pts',(21.0977302873553,20.150594907745,0.128684292012742));
#119603=CARTESIAN_POINT('Ctrl Pts',(21.4611752161576,18.3736796382696,0.0438817648400879));
#119604=CARTESIAN_POINT('Ctrl Pts',(19.5021064059726,16.4608275871995,-0.0833126978930439));
#119605=CARTESIAN_POINT('Ctrl Pts',(16.8390405955535,17.0785075195682,-0.210488504574479));
#119606=CARTESIAN_POINT('Ctrl Pts',(15.9143177751785,19.6490612161152,-0.337664311255912));
#119607=CARTESIAN_POINT('Ctrl Pts',(17.5765589736414,21.8195506449214,-0.464840117937347));
#119608=CARTESIAN_POINT('Ctrl Pts',(20.300639162813,21.5959087516894,-0.592015924618781));
#119609=CARTESIAN_POINT('Ctrl Pts',(21.5874465446713,19.1847529778785,-0.719191731300216));
#119610=CARTESIAN_POINT('Ctrl Pts',(20.2563827312793,16.7974219353056,-0.84636753798165));
#119611=CARTESIAN_POINT('Ctrl Pts',(17.5286330099687,16.6245314625761,-0.973543344663085));
#119612=CARTESIAN_POINT('Ctrl Pts',(15.9067296997928,18.8244965669171,-1.10071915134451));
#119613=CARTESIAN_POINT('Ctrl Pts',(16.8786729611136,21.3790902770145,-1.22789495802595));
#119614=CARTESIAN_POINT('Ctrl Pts',(19.5527628208785,21.9445771977858,-1.35507076470738));
#119615=CARTESIAN_POINT('Ctrl Pts',(21.4756890285423,20.0021863207324,-1.48224657138883));
#119616=CARTESIAN_POINT('Ctrl Pts',(20.8832855040238,17.3339261098018,-1.60942237807025));
#119617=CARTESIAN_POINT('Ctrl Pts',(18.3190460418495,16.3877672793826,-1.73659818475169));
#119618=CARTESIAN_POINT('Ctrl Pts',(16.1355010228962,18.0317478959284,-1.86377399143312));
#119619=CARTESIAN_POINT('Ctrl Pts',(16.3359175647298,20.7576198232253,-1.99094979811455));
#119620=CARTESIAN_POINT('Ctrl Pts',(18.7364258833992,22.0645636945266,-2.11812560479599));
#119621=CARTESIAN_POINT('Ctrl Pts',(21.1347086127881,20.7535401762524,-2.24530141147742));
#119622=CARTESIAN_POINT('Ctrl Pts',(21.3304901904839,18.0273316895207,-2.37247721815887));
#119623=CARTESIAN_POINT('Ctrl Pts',(19.1441531769682,16.387065461564,-2.49965302484029));
#119624=CARTESIAN_POINT('Ctrl Pts',(16.5815260794188,17.337583873188,-2.62682883152173));
#119625=CARTESIAN_POINT('Ctrl Pts',(15.9936602069971,20.0068453174889,-2.75400463820316));
#119626=CARTESIAN_POINT('Ctrl Pts',(17.9198860096782,21.9459680716425,-2.88118044488459));
#119627=CARTESIAN_POINT('Ctrl Pts',(20.5930108690263,21.3759273750031,-3.00835625156604));
#119628=CARTESIAN_POINT('Ctrl Pts',(21.5606086391872,18.8197001804373,-3.13553205824747));
#119629=CARTESIAN_POINT('Ctrl Pts',(19.9349684220548,16.6224662845049,-3.2627078649289));
#119630=CARTESIAN_POINT('Ctrl Pts',(17.2075142181716,16.8000514095034,-3.38988367161033));
#119631=CARTESIAN_POINT('Ctrl Pts',(15.8805159747347,19.1895322262035,-3.51705947829178));
#119632=CARTESIAN_POINT('Ctrl Pts',(17.1714122172801,21.5987083927831,-3.6442352849732));
#119633=CARTESIAN_POINT('Ctrl Pts',(19.8958857653384,21.8173103069526,-3.77141109165464));
#119634=CARTESIAN_POINT('Ctrl Pts',(21.5544012384607,19.6447842803171,-3.89858689833607));
#119635=CARTESIAN_POINT('Ctrl Pts',(20.6253736291394,17.074288100199,-4.02576270501751));
#119636=CARTESIAN_POINT('Ctrl Pts',(17.961128106969,16.464092468841,-4.15293851169893));
#119637=CARTESIAN_POINT('Ctrl Pts',(16.0059445768151,18.3740140050173,-4.28011431838038));
#119638=CARTESIAN_POINT('Ctrl Pts',(16.5535825752176,21.0518182423779,-4.4072901250618));
#119639=CARTESIAN_POINT('Ctrl Pts',(19.10161822889,22.0407859964237,-4.53446593174325));
#119640=CARTESIAN_POINT('Ctrl Pts',(21.3123869745163,20.4336007350771,-4.66164173842467));
#119641=CARTESIAN_POINT('Ctrl Pts',(21.1576457037679,17.7047551824572,-4.78881754510611));
#119642=CARTESIAN_POINT('Ctrl Pts',(18.7793599282299,16.3577957618358,-4.91599335178755));
#119643=CARTESIAN_POINT('Ctrl Pts',(16.3594592338956,17.6284741399031,-5.04316915846898));
#119644=CARTESIAN_POINT('Ctrl Pts',(16.1180523118408,20.3510217719769,-5.17034496515041));
#119645=CARTESIAN_POINT('Ctrl Pts',(18.2766150296472,22.0276701859931,-5.29752077183185));
#119646=CARTESIAN_POINT('Ctrl Pts',(20.8548000692393,21.1201985266286,-5.42469657851328));
#119647=CARTESIAN_POINT('Ctrl Pts',(21.4872826770021,18.4611557173071,-5.55187238519472));
#119648=CARTESIAN_POINT('Ctrl Pts',(19.5937993166108,16.4900484967713,-5.67904819187615));
#119649=CARTESIAN_POINT('Ctrl Pts',(16.9115034483931,17.0152453991512,-5.80622399855758));
#119650=CARTESIAN_POINT('Ctrl Pts',(15.9012350493816,19.5549108639094,-5.93339980523902));
#119651=CARTESIAN_POINT('Ctrl Pts',(17.4898526713405,21.7790594565463,-6.06057561192046));
#119652=CARTESIAN_POINT('Ctrl Pts',(20.2198982468525,21.6471728895478,-6.18775141860189));
#119653=CARTESIAN_POINT('Ctrl Pts',(21.5867244061235,19.2802489023316,-6.31492722528332));
#119654=CARTESIAN_POINT('Ctrl Pts',(20.3363529828215,16.8497933452978,-6.44210303196475));
#119655=CARTESIAN_POINT('Ctrl Pts',(17.615922151023,16.5855983409401,-6.56927883864619));
#119656=CARTESIAN_POINT('Ctrl Pts',(15.9212583499232,18.7300464079656,-6.69645464532763));
#119657=CARTESIAN_POINT('Ctrl Pts',(16.8071104343333,21.315739544336,-6.82363045200906));
#119658=CARTESIAN_POINT('Ctrl Pts',(19.4607640989881,21.9704647836472,-6.95080625869048));
#119659=CARTESIAN_POINT('Ctrl Pts',(21.4476568108886,20.0935523556623,-7.07798206537195));
#119660=CARTESIAN_POINT('Ctrl Pts',(20.9449378273356,17.4069529187342,-7.20515787205335));
#119661=CARTESIAN_POINT('Ctrl Pts',(18.4138206134801,16.3754547070776,-7.3323336787348));
#119662=CARTESIAN_POINT('Ctrl Pts',(16.1764481141826,17.9453933078879,-7.45950948541623));
#119663=CARTESIAN_POINT('Ctrl Pts',(16.2854707305501,20.6764474963007,-7.58668529209767));
#119664=CARTESIAN_POINT('Ctrl Pts',(18.640866978772,22.0630445627872,-7.7138610987791));
#119665=CARTESIAN_POINT('Ctrl Pts',(21.0817069934834,20.8330677607659,-7.84103690546054));
#119666=CARTESIAN_POINT('Ctrl Pts',(21.3686715568034,18.1149444651214,-7.96821271214196));
#119667=CARTESIAN_POINT('Ctrl Pts',(19.2384884929154,16.4023840938492,-8.09538851882341));
#119668=CARTESIAN_POINT('Ctrl Pts',(16.6454685488647,17.2665544941074,-8.22256432550483));
#119669=CARTESIAN_POINT('Ctrl Pts',(15.9685465823494,19.9146329601232,-8.34974013218628));
#119670=CARTESIAN_POINT('Ctrl Pts',(17.8287564831316,21.9171718576127,-8.47691593886771));
#119671=CARTESIAN_POINT('Ctrl Pts',(20.5194711248913,21.4369660397109,-8.60409174554914));
#119672=CARTESIAN_POINT('Ctrl Pts',(21.5721268283993,18.9145745394082,-8.73126755223057));
#119673=CARTESIAN_POINT('Ctrl Pts',(20.0209773208683,16.6641350009595,-8.858443358912));
#119674=CARTESIAN_POINT('Ctrl Pts',(17.2891060002617,16.7502860228609,-8.98561916559344));
#119675=CARTESIAN_POINT('Ctrl Pts',(15.8828352441794,19.0939893896534,-9.11279497227487));
#119676=CARTESIAN_POINT('Ctrl Pts',(17.0923311883199,21.5450427289413,-9.23997077895631));
#119677=CARTESIAN_POINT('Ctrl Pts',(19.8079563737189,21.8547567314554,-9.36714658563774));
#119678=CARTESIAN_POINT('Ctrl Pts',(21.5382932434809,19.7389880229077,-9.49432239231919));
#119679=CARTESIAN_POINT('Ctrl Pts',(20.6958651164175,17.1388230739748,-9.62149819900061));
#119680=CARTESIAN_POINT('Ctrl Pts',(18.0535475121228,16.439751840865,-9.74867400568204));
#119681=CARTESIAN_POINT('Ctrl Pts',(16.035502831811,18.2831287907025,-9.87584981236349));
#119682=CARTESIAN_POINT('Ctrl Pts',(16.4931618156892,20.9777699848882,-10.0030256190449));
#119683=CARTESIAN_POINT('Ctrl Pts',(19.0066507515693,22.0515093760514,-10.1302014257263));
#119684=CARTESIAN_POINT('Ctrl Pts',(21.2699995454986,20.5192577165824,-10.2573772324077));
#119685=CARTESIAN_POINT('Ctrl Pts',(21.2067261583164,17.7867608017806,-10.3845530390892));
#119686=CARTESIAN_POINT('Ctrl Pts',(18.874879995573,16.3609149530909,-10.5117288457706));
#119687=CARTESIAN_POINT('Ctrl Pts',(16.4137851808899,17.5498452387121,-10.6389046524521));
#119688=CARTESIAN_POINT('Ctrl Pts',(16.0813434539675,20.2627819149227,-10.7660804591335));
#119689=CARTESIAN_POINT('Ctrl Pts',(18.1825494655964,22.0107739651396,-10.8932562658149));
#119690=CARTESIAN_POINT('Ctrl Pts',(20.7896771156604,21.1901471759111,-11.0204320724963));
#119691=CARTESIAN_POINT('Ctrl Pts',(21.5108486018171,18.5537756925119,-11.1476078791778));
#119692=CARTESIAN_POINT('Ctrl Pts',(19.6844338464684,16.5203667192919,-11.2747836858592));
#119693=CARTESIAN_POINT('Ctrl Pts',(16.9860550275624,16.9554467815862,-11.4019594925407));
#119694=CARTESIAN_POINT('Ctrl Pts',(15.8913072311674,19.4598569263539,-11.5291352992221));
#119695=CARTESIAN_POINT('Ctrl Pts',(17.4045536127647,21.7359562869947,-11.6563111059035));
#119696=CARTESIAN_POINT('Ctrl Pts',(20.1374845399016,21.6955649707794,-11.783486912585));
#119697=CARTESIAN_POINT('Ctrl Pts',(21.5828055117534,19.3757395033677,-11.9106627192664));
#119698=CARTESIAN_POINT('Ctrl Pts',(20.4145242433828,16.9047757665027,-12.0378385259478));
#119699=CARTESIAN_POINT('Ctrl Pts',(17.7044662868062,16.5496296234525,-12.1650143326293));
#119700=CARTESIAN_POINT('Ctrl Pts',(15.9389416120162,18.6361256176097,-12.2921901393107));
#119701=CARTESIAN_POINT('Ctrl Pts',(16.7377095273126,21.2500331768819,-12.4193659459921));
#119702=CARTESIAN_POINT('Ctrl Pts',(19.3679500475393,21.9932543530368,-12.5465417526735));
#119703=CARTESIAN_POINT('Ctrl Pts',(21.416580746526,20.183929846461,-12.673717559355));
#119704=CARTESIAN_POINT('Ctrl Pts',(21.004110110314,17.4820025925939,-12.8008933660364));
#119705=CARTESIAN_POINT('Ctrl Pts',(18.5089543468127,16.3663231463401,-12.9280691727179));
#119706=CARTESIAN_POINT('Ctrl Pts',(16.2202640022022,17.8604581527614,-13.0552449793993));
#119707=CARTESIAN_POINT('Ctrl Pts',(16.2377704155193,20.5936314799435,-13.1824207860807));
#119708=CARTESIAN_POINT('Ctrl Pts',(18.5454125391162,22.0583262400653,-13.3095965927622));
#119709=CARTESIAN_POINT('Ctrl Pts',(21.0260719530159,20.9107758999245,-13.4367723994436));
#119710=CARTESIAN_POINT('Ctrl Pts',(21.4038976120531,18.2037866715935,-13.563948206125));
#119711=CARTESIAN_POINT('Ctrl Pts',(19.3322579245662,16.4208531573659,-13.6911240128065));
#119712=CARTESIAN_POINT('Ctrl Pts',(16.7117537233642,17.1977061952114,-13.8182998194879));
#119713=CARTESIAN_POINT('Ctrl Pts',(15.9465349662162,19.8216313398441,-13.9454756261693));
#119714=CARTESIAN_POINT('Ctrl Pts',(17.7386423679729,21.8853401302251,-14.0726514328508));
#119715=CARTESIAN_POINT('Ctrl Pts',(20.4439286182524,21.495507839393,-14.1998272395322));
#119716=CARTESIAN_POINT('Ctrl Pts',(21.5804614914246,19.0097813984656,-14.3270030462136));
#119717=CARTESIAN_POINT('Ctrl Pts',(20.1055426175397,16.708660535411,-14.4541788528951));
#119718=CARTESIAN_POINT('Ctrl Pts',(17.3723185195974,16.7032808184137,-14.5813546595765));
#119719=CARTESIAN_POINT('Ctrl Pts',(15.8883526644403,18.9985778039157,-14.708530466258));
#119720=CARTESIAN_POINT('Ctrl Pts',(17.0150916188663,21.4887589699166,-14.8357062729394));
#119721=CARTESIAN_POINT('Ctrl Pts',(19.7188223254962,21.8892376546847,-14.9628820796208));
#119722=CARTESIAN_POINT('Ctrl Pts',(21.5190396734505,19.8325995214557,-15.0900578863023));
#119723=CARTESIAN_POINT('Ctrl Pts',(20.7641559800708,17.2056824081085,-15.2172336929837));
#119724=CARTESIAN_POINT('Ctrl Pts',(18.1467301806671,16.4185197212751,-15.3444094996651));
#119725=CARTESIAN_POINT('Ctrl Pts',(16.0680879904256,18.1932843692987,-15.4715853063465));
#119726=CARTESIAN_POINT('Ctrl Pts',(16.4352546038082,20.9017399419349,-15.598761113028));
#119727=CARTESIAN_POINT('Ctrl Pts',(18.9113774419666,22.0590465570016,-15.7259369197094));
#119728=CARTESIAN_POINT('Ctrl Pts',(21.2247674864064,20.6034472257245,-15.8531127263909));
#119729=CARTESIAN_POINT('Ctrl Pts',(21.2530329565334,17.870363989867,-15.9802885330723));
#119730=CARTESIAN_POINT('Ctrl Pts',(18.9702420378592,16.3672310840514,-16.1074643397537));
#119731=CARTESIAN_POINT('Ctrl Pts',(16.4707137122836,17.4730796544138,-16.2346401464351));
#119732=CARTESIAN_POINT('Ctrl Pts',(16.0476100802981,20.1733622743496,-16.3618159531166));
#119733=CARTESIAN_POINT('Ctrl Pts',(18.0891024634763,21.9907372385088,-16.488991759798));
#119734=CARTESIAN_POINT('Ctrl Pts',(20.7222483095596,21.2578758162869,-16.6161675664795));
#119735=CARTESIAN_POINT('Ctrl Pts',(21.5312997362295,18.6471328760627,-16.7433433731609));
#119736=CARTESIAN_POINT('Ctrl Pts',(19.7740022749111,16.5537030245103,-16.8705191798423));
#119737=CARTESIAN_POINT('Ctrl Pts',(17.0625672761828,16.8981782175187,-16.9976949865238));
#119738=CARTESIAN_POINT('Ctrl Pts',(15.8845680607422,19.3645238460445,-17.1248707932052));
#119739=CARTESIAN_POINT('Ctrl Pts',(17.3207457938787,21.6900208745888,-17.2520465998866));
#119740=CARTESIAN_POINT('Ctrl Pts',(20.053496544683,21.7411701160866,-17.3792224065681));
#119741=CARTESIAN_POINT('Ctrl Pts',(21.5756911129322,19.4710453161425,-17.5063982132495));
#119742=CARTESIAN_POINT('Ctrl Pts',(20.4908104603086,16.9623450788714,-17.6335740199309));
#119743=CARTESIAN_POINT('Ctrl Pts',(17.794165250305,16.516646164469,-17.7607498266124));
#119744=CARTESIAN_POINT('Ctrl Pts',(15.959760090426,18.5428496637114,-17.8879256332938));
#119745=CARTESIAN_POINT('Ctrl Pts',(16.6705478588277,21.1820396264035,-18.0151014399752));
#119746=CARTESIAN_POINT('Ctrl Pts',(19.2744248944815,22.0129230684028,-18.1422772466567));
#119747=CARTESIAN_POINT('Ctrl Pts',(21.3824956319804,20.2732160020698,-18.2694530533381));
#119748=CARTESIAN_POINT('Ctrl Pts',(21.0607360113538,17.5589916824588,-18.3966288600195));
#119749=CARTESIAN_POINT('Ctrl Pts',(18.6043405137593,16.360382458875,-18.523804666701));
#119750=CARTESIAN_POINT('Ctrl Pts',(16.2668995473587,17.7770379002201,-18.6509804733824));
#119751=CARTESIAN_POINT('Ctrl Pts',(16.1928701204568,20.5092645659538,-18.7781562800638));
#119752=CARTESIAN_POINT('Ctrl Pts',(18.45016963826,22.0504140726478,-18.9053320867453));
#119753=CARTESIAN_POINT('Ctrl Pts',(20.9678658954356,20.9865773999889,-19.0325078934267));
#119754=CARTESIAN_POINT('Ctrl Pts',(21.4361288448778,18.2937586707072,-19.1596837001081));
#119755=CARTESIAN_POINT('Ctrl Pts',(19.4253562883709,16.4424519246523,-19.2868595067896));
#119756=CARTESIAN_POINT('Ctrl Pts',(16.780307255024,17.1311162137809,-19.414035313471));
#119757=CARTESIAN_POINT('Ctrl Pts',(15.9276500412235,19.7279447624144,-19.5412111201524));
#119758=CARTESIAN_POINT('Ctrl Pts',(17.6496447600855,21.8505086195232,-19.6683869268339));
#119759=CARTESIAN_POINT('Ctrl Pts',(20.3664680564733,21.5514870621786,-19.7955627335153));
#119760=CARTESIAN_POINT('Ctrl Pts',(21.5856033344346,19.1052140510933,-19.9227385401968));
#119761=CARTESIAN_POINT('Ctrl Pts',(20.1885693489379,16.7559927763657,-20.0499143468782));
#119762=CARTESIAN_POINT('Ctrl Pts',(17.457058641429,16.6590888438425,-20.1770901535596));
#119763=CARTESIAN_POINT('Ctrl Pts',(15.8970616522235,18.9034038719576,-20.3042659602411));
#119764=CARTESIAN_POINT('Ctrl Pts',(16.9397809084021,21.4299214440102,-20.4314417669225));
#119765=CARTESIAN_POINT('Ctrl Pts',(19.6285821382997,21.9207120974271,-20.5586175736039));
#119766=CARTESIAN_POINT('Ctrl Pts',(21.4966649457231,19.9255182070319,-20.6857933802854));
#119767=CARTESIAN_POINT('Ctrl Pts',(20.8301641839021,17.2747825617085,-20.8129691869668));
#119768=CARTESIAN_POINT('Ctrl Pts',(18.240582059696,16.40043638892,-20.9401449936482));
#119769=CARTESIAN_POINT('Ctrl Pts',(16.1036433297677,18.104549801285,-21.0673208003297));
#119770=CARTESIAN_POINT('Ctrl Pts',(16.3799647587305,20.8238745060694,-21.1944966070111));
#119771=CARTESIAN_POINT('Ctrl Pts',(18.8158302886401,22.0632713447717,-21.3216724136925));
#119772=CARTESIAN_POINT('Ctrl Pts',(21.176885810551,20.6863017024412,-21.4488482203739));
#119773=CARTESIAN_POINT('Ctrl Pts',(21.2962360890773,17.9550335586219,-21.5760240270554));
#119774=CARTESIAN_POINT('Ctrl Pts',(19.06587574408,16.377582661504,-21.7031998337368));
#119775=CARTESIAN_POINT('Ctrl Pts',(16.529138326029,17.396607333106,-21.8303756404183));
#119776=CARTESIAN_POINT('Ctrl Pts',(16.0189811762652,20.0863088421845,-21.9575514470997));
#119777=CARTESIAN_POINT('Ctrl Pts',(17.3340241117299,21.3345380991533,-22.0423353182207));
#119778=CARTESIAN_POINT('Ctrl Pts',(18.1101967966574,21.5422305581871,-22.0847272537811));
#119779=CARTESIAN_POINT('Ctrl Pts',(20.6946895702226,20.8620838326754,0.257713273515286));
#119780=CARTESIAN_POINT('Ctrl Pts',(21.2446793034262,20.2090078950207,0.21530268190311));
#119781=CARTESIAN_POINT('Ctrl Pts',(21.6307189736713,18.3216248822975,0.130500154730457));
#119782=CARTESIAN_POINT('Ctrl Pts',(19.54985825025,16.2898541338203,0.00330569199732501));
#119783=CARTESIAN_POINT('Ctrl Pts',(16.7212342529825,16.9459341572626,-0.12387011468411));
#119784=CARTESIAN_POINT('Ctrl Pts',(15.7390230172331,19.6762947228445,-0.251045921365544));
#119785=CARTESIAN_POINT('Ctrl Pts',(17.5046028706573,21.9817197183951,-0.378221728046978));
#119786=CARTESIAN_POINT('Ctrl Pts',(20.3980344048781,21.7441743961897,-0.505397534728411));
#119787=CARTESIAN_POINT('Ctrl Pts',(21.7648403718746,19.1831212459942,-0.632573341409846));
#119788=CARTESIAN_POINT('Ctrl Pts',(20.3510266276838,16.6473739692942,-0.75974914809128));
#119789=CARTESIAN_POINT('Ctrl Pts',(17.4536974328697,16.4637351954612,-0.886924954772716));
#119790=CARTESIAN_POINT('Ctrl Pts',(15.7309632043494,18.8004683182191,-1.01410076145415));
#119791=CARTESIAN_POINT('Ctrl Pts',(16.7633304940341,21.5138766926494,-1.14127656813558));
#119792=CARTESIAN_POINT('Ctrl Pts',(19.6036638866926,22.1145189554039,-1.26845237481702));
#119793=CARTESIAN_POINT('Ctrl Pts',(21.6461350846223,20.0513730033173,-1.39562818149845));
#119794=CARTESIAN_POINT('Ctrl Pts',(21.016902859507,17.2172316786593,-1.52280398817988));
#119795=CARTESIAN_POINT('Ctrl Pts',(18.2932490733073,16.2122517932659,-1.64997979486132));
#119796=CARTESIAN_POINT('Ctrl Pts',(15.9739568441929,17.9584358360373,-1.77715560154276));
#119797=CARTESIAN_POINT('Ctrl Pts',(16.1868329351487,20.853770497638,-1.90433140822419));
#119798=CARTESIAN_POINT('Ctrl Pts',(18.7365766963666,22.2419648047335,-2.03150721490562));
#119799=CARTESIAN_POINT('Ctrl Pts',(21.2839565072747,20.8494372260819,-2.15868302158706));
#119800=CARTESIAN_POINT('Ctrl Pts',(21.4919094864038,17.9537450817297,-2.28585882826849));
#119801=CARTESIAN_POINT('Ctrl Pts',(19.169651689263,16.2115063446496,-2.41303463494992));
#119802=CARTESIAN_POINT('Ctrl Pts',(16.4477105056032,17.2211168388571,-2.54021044163136));
#119803=CARTESIAN_POINT('Ctrl Pts',(15.8232980305526,20.0563216418289,-2.66738624831279));
#119804=CARTESIAN_POINT('Ctrl Pts',(17.8692739536042,22.1159962974782,-2.79456205499423));
#119805=CARTESIAN_POINT('Ctrl Pts',(20.7085823534422,21.5105171585006,-2.92173786167567));
#119806=CARTESIAN_POINT('Ctrl Pts',(21.7363340003116,18.7953737487032,-3.04891366835709));
#119807=CARTESIAN_POINT('Ctrl Pts',(20.0096305478046,16.4615416288479,-3.17608947503854));
#119808=CARTESIAN_POINT('Ctrl Pts',(17.1126152422242,16.6501669133465,-3.30326528171996));
#119809=CARTESIAN_POINT('Ctrl Pts',(15.7031198174278,19.1881976119062,-3.4304410884014));
#119810=CARTESIAN_POINT('Ctrl Pts',(17.0742688424951,21.7471480861189,-3.55761689508284));
#119811=CARTESIAN_POINT('Ctrl Pts',(19.9681181900429,21.9793401024969,-3.68479270176427));
#119812=CARTESIAN_POINT('Ctrl Pts',(21.7297406962381,19.671751897359,-3.8119685084457));
#119813=CARTESIAN_POINT('Ctrl Pts',(20.742957050273,16.9414524239027,-3.93914431512714));
#119814=CARTESIAN_POINT('Ctrl Pts',(17.9130800006189,16.2933219874959,-4.06632012180857));
#119815=CARTESIAN_POINT('Ctrl Pts',(15.8363460983557,18.3219800360464,-4.19349592849001));
#119816=CARTESIAN_POINT('Ctrl Pts',(16.4180298021666,21.1662587227194,-4.32067173517144));
#119817=CARTESIAN_POINT('Ctrl Pts',(19.1244724171678,22.2167088883417,-4.44784754185288));
#119818=CARTESIAN_POINT('Ctrl Pts',(21.4726808248689,20.5096077042429,-4.57502334853431));
#119819=CARTESIAN_POINT('Ctrl Pts',(21.3083195574551,17.6111145521858,-4.70219915521574));
#119820=CARTESIAN_POINT('Ctrl Pts',(18.7821798763678,16.1804169984081,-4.82937496189718));
#119821=CARTESIAN_POINT('Ctrl Pts',(16.2118381490933,17.5300912493964,-4.95655076857861));
#119822=CARTESIAN_POINT('Ctrl Pts',(15.9554233770066,20.4218949501003,-5.08372657526004));
#119823=CARTESIAN_POINT('Ctrl Pts',(18.2481801986013,22.2027776907038,-5.21090238194148));
#119824=CARTESIAN_POINT('Ctrl Pts',(20.9866465346018,21.238890090752,-5.33807818862291));
#119825=CARTESIAN_POINT('Ctrl Pts',(21.6584494901173,18.4145391975892,-5.46525399530435));
#119826=CARTESIAN_POINT('Ctrl Pts',(19.6472515502562,16.3208916567058,-5.59242980198579));
#119827=CARTESIAN_POINT('Ctrl Pts',(16.7982019958189,16.8787391404406,-5.71960560866721));
#119828=CARTESIAN_POINT('Ctrl Pts',(15.7251269610433,19.5762912063867,-5.84678141534867));
#119829=CARTESIAN_POINT('Ctrl Pts',(17.4125061877879,21.9387112630022,-5.97395722203007));
#119830=CARTESIAN_POINT('Ctrl Pts',(20.3122739660809,21.7986255366678,-6.10113302871153));
#119831=CARTESIAN_POINT('Ctrl Pts',(21.7640733392246,19.2845539865944,-6.22830883539295));
#119832=CARTESIAN_POINT('Ctrl Pts',(20.4359684911912,16.703001219096,-6.35548464207439));
#119833=CARTESIAN_POINT('Ctrl Pts',(17.5464131885679,16.422381669117,-6.48266044875582));
#119834=CARTESIAN_POINT('Ctrl Pts',(15.7463950754831,18.7001463565497,-6.60983625543726));
#119835=CARTESIAN_POINT('Ctrl Pts',(16.6873190489681,21.4465875546951,-6.7370120621187));
#119836=CARTESIAN_POINT('Ctrl Pts',(19.5059457636785,22.1420159276201,-6.86418786880012));
#119837=CARTESIAN_POINT('Ctrl Pts',(21.6163601525715,20.1484191063189,-6.99136367548156));
#119838=CARTESIAN_POINT('Ctrl Pts',(21.0823880009273,17.2947984377616,-7.118539482163));
#119839=CARTESIAN_POINT('Ctrl Pts',(18.3939156158299,16.1991737696759,-7.24571528884443));
#119840=CARTESIAN_POINT('Ctrl Pts',(16.0174495451912,17.8667127328943,-7.37289109552587));
#119841=CARTESIAN_POINT('Ctrl Pts',(16.1332499087027,20.7675518278046,-7.50006690220729));
#119842=CARTESIAN_POINT('Ctrl Pts',(18.6350770602241,22.2403512312061,-7.62724270888874));
#119843=CARTESIAN_POINT('Ctrl Pts',(21.2276598691396,20.9339089027185,-7.75441851557016));
#119844=CARTESIAN_POINT('Ctrl Pts',(21.5324645221063,18.0468045917732,-7.8815943222516));
#119845=CARTESIAN_POINT('Ctrl Pts',(19.2698516683375,16.2277773097598,-8.00877012893304));
#119846=CARTESIAN_POINT('Ctrl Pts',(16.5156281675744,17.1456716863595,-8.13594593561446));
#119847=CARTESIAN_POINT('Ctrl Pts',(15.7966231353776,19.9583766019922,-8.26312174229592));
#119848=CARTESIAN_POINT('Ctrl Pts',(17.7724790623024,22.0854098727205,-8.39029754897732));
#119849=CARTESIAN_POINT('Ctrl Pts',(20.6304707708447,21.5753504912249,-8.51747335565878));
#119850=CARTESIAN_POINT('Ctrl Pts',(21.7485682553881,18.8961462821721,-8.64464916234021));
#119851=CARTESIAN_POINT('Ctrl Pts',(20.1009864708203,16.5058008172007,-8.77182496902164));
#119852=CARTESIAN_POINT('Ctrl Pts',(17.199279444024,16.5973076988504,-8.89900077570308));
#119853=CARTESIAN_POINT('Ctrl Pts',(15.705583271835,19.0867150427652,-9.0261765823845));
#119854=CARTESIAN_POINT('Ctrl Pts',(16.9902714829968,21.6901461209486,-9.15335238906595));
#119855=CARTESIAN_POINT('Ctrl Pts',(19.8747223805114,22.0191145063235,-9.28052819574737));
#119856=CARTESIAN_POINT('Ctrl Pts',(21.7126312951226,19.7718121233893,-9.40770400242882));
#119857=CARTESIAN_POINT('Ctrl Pts',(20.8178308711669,17.0099994251714,-9.53487980911025));
#119858=CARTESIAN_POINT('Ctrl Pts',(18.011244960046,16.2674681448564,-9.66205561579168));
#119859=CARTESIAN_POINT('Ctrl Pts',(15.8677419388458,18.2254446454444,-9.78923142247312));
#119860=CARTESIAN_POINT('Ctrl Pts',(16.353852788716,21.0876070133732,-9.91640722915455));
#119861=CARTESIAN_POINT('Ctrl Pts',(19.0236009763425,22.2280989218993,-10.043583035836));
#119862=CARTESIAN_POINT('Ctrl Pts',(21.4276582428386,20.6005898318611,-10.1707588425174));
#119863=CARTESIAN_POINT('Ctrl Pts',(21.3604512588158,17.6982183187623,-10.2979346491988));
#119864=CARTESIAN_POINT('Ctrl Pts',(18.8836382607796,16.1837301043787,-10.4251104558803));
#119865=CARTESIAN_POINT('Ctrl Pts',(16.2695414460758,17.4465741256675,-10.5522862625617));
#119866=CARTESIAN_POINT('Ctrl Pts',(15.9164323930488,20.3281693740358,-10.6794620692432));
#119867=CARTESIAN_POINT('Ctrl Pts',(18.1482667414313,22.1848310610778,-10.8066378759246));
#119868=CARTESIAN_POINT('Ctrl Pts',(20.9174749998444,21.3131873263528,-10.933813682606));
#119869=CARTESIAN_POINT('Ctrl Pts',(21.6834804676428,18.5129171961597,-11.0609894892874));
#119870=CARTESIAN_POINT('Ctrl Pts',(19.7435206717827,16.3530947105848,-11.1881652959689));
#119871=CARTESIAN_POINT('Ctrl Pts',(16.8773883174812,16.8152229464412,-11.3153411026503));
#119872=CARTESIAN_POINT('Ctrl Pts',(15.7145819475737,19.4753279302437,-11.4425169093318));
#119873=CARTESIAN_POINT('Ctrl Pts',(17.3219042345475,21.8929284440893,-11.5696927160132));
#119874=CARTESIAN_POINT('Ctrl Pts',(20.2247367417761,21.8500260697353,-11.6968685226946));
#119875=CARTESIAN_POINT('Ctrl Pts',(21.7599108139823,19.3859810728298,-11.824044329376));
#119876=CARTESIAN_POINT('Ctrl Pts',(20.5189995235657,16.7614018021532,-11.9512201360575));
#119877=CARTESIAN_POINT('Ctrl Pts',(17.6404619598427,16.38417683879,-12.0783959427389));
#119878=CARTESIAN_POINT('Ctrl Pts',(15.7651776753385,18.6003866734043,-12.2055717494204));
#119879=CARTESIAN_POINT('Ctrl Pts',(16.6136036078165,21.3767963362328,-12.3327475561018));
#119880=CARTESIAN_POINT('Ctrl Pts',(19.4073616234801,22.1662222850487,-12.4599233627832));
#119881=CARTESIAN_POINT('Ctrl Pts',(21.5833521431366,20.2444152091134,-12.5870991694647));
#119882=CARTESIAN_POINT('Ctrl Pts',(21.1452389222041,17.3745138197983,-12.7142749761461));
#119883=CARTESIAN_POINT('Ctrl Pts',(18.4949636485153,16.1894745156307,-12.8414507828275));
#119884=CARTESIAN_POINT('Ctrl Pts',(16.0639893910444,17.7764973063501,-12.968626589509));
#119885=CARTESIAN_POINT('Ctrl Pts',(16.0825841477421,20.6795872832148,-13.0958023961904));
#119886=CARTESIAN_POINT('Ctrl Pts',(18.5336883834592,22.2353395785366,-13.2229782028718));
#119887=CARTESIAN_POINT('Ctrl Pts',(21.1685660946113,21.0164480222352,-13.3501540095533));
#119888=CARTESIAN_POINT('Ctrl Pts',(21.5698805201709,18.1411699642751,-13.4773298162347));
#119889=CARTESIAN_POINT('Ctrl Pts',(19.3694505830695,16.247394562952,-13.6045056229161));
#119890=CARTESIAN_POINT('Ctrl Pts',(16.5860341765131,17.072543208022,-13.7316814295976));
#119891=CARTESIAN_POINT('Ctrl Pts',(15.7732430952114,19.8595932321345,-13.858857236279));
#119892=CARTESIAN_POINT('Ctrl Pts',(17.6767627087548,22.0515992219996,-13.9860330429604));
#119893=CARTESIAN_POINT('Ctrl Pts',(20.5502319174689,21.6375317331515,-14.1132088496419));
#119894=CARTESIAN_POINT('Ctrl Pts',(21.7574210699713,18.9972719866817,-14.2403846563233));
#119895=CARTESIAN_POINT('Ctrl Pts',(20.1908090454502,16.5530944269748,-14.3675604630048));
#119896=CARTESIAN_POINT('Ctrl Pts',(17.2876651414952,16.5473802622938,-14.4947362696862));
#119897=CARTESIAN_POINT('Ctrl Pts',(15.7114437005529,18.9853718840723,-14.6219120763676));
#119898=CARTESIAN_POINT('Ctrl Pts',(16.9082300633519,21.6303632981543,-14.749087883049));
#119899=CARTESIAN_POINT('Ctrl Pts',(19.7800470229629,22.0557390488012,-14.8762636897305));
#119900=CARTESIAN_POINT('Ctrl Pts',(21.6921807640061,19.8712432865912,-15.0034394964119));
#119901=CARTESIAN_POINT('Ctrl Pts',(20.8903672594785,17.0810152882537,-15.1306153030934));
#119902=CARTESIAN_POINT('Ctrl Pts',(18.1102206336258,16.2449160611827,-15.2577911097748));
#119903=CARTESIAN_POINT('Ctrl Pts',(15.9023528603076,18.1300147520451,-15.3849669164562));
#119904=CARTESIAN_POINT('Ctrl Pts',(16.2923455858144,21.0068503143949,-15.5121427231376));
#119905=CARTESIAN_POINT('Ctrl Pts',(18.9224046901724,22.2361046763285,-15.6393185298191));
#119906=CARTESIAN_POINT('Ctrl Pts',(21.379614185011,20.6900132569022,-15.7664943365005));
#119907=CARTESIAN_POINT('Ctrl Pts',(21.4096368704371,17.7870189721836,-15.8936701431819));
#119908=CARTESIAN_POINT('Ctrl Pts',(18.9849287959905,16.1904388982563,-16.0208459498634));
#119909=CARTESIAN_POINT('Ctrl Pts',(16.33000912562,17.3650361580133,-16.1480217565448));
#119910=CARTESIAN_POINT('Ctrl Pts',(15.8806018739919,20.2331906693557,-16.2751975632263));
#119911=CARTESIAN_POINT('Ctrl Pts',(18.0490103011151,22.1635486858722,-16.4023733699077));
#119912=CARTESIAN_POINT('Ctrl Pts',(20.8458542617096,21.3851265389399,-16.5295491765891));
#119913=CARTESIAN_POINT('Ctrl Pts',(21.7052030136437,18.6120782340418,-16.6567249832706));
#119914=CARTESIAN_POINT('Ctrl Pts',(19.8386574142166,16.3885034761332,-16.783900789952));
#119915=CARTESIAN_POINT('Ctrl Pts',(16.9586572000173,16.754394094981,-16.9110765966334));
#119916=CARTESIAN_POINT('Ctrl Pts',(15.7074238146008,19.3740681575255,-17.0382524033149));
#119917=CARTESIAN_POINT('Ctrl Pts',(17.2328862287842,21.8441373066915,-17.1654282099963));
#119918=CARTESIAN_POINT('Ctrl Pts',(20.1355273584301,21.8984664079011,-17.2926040166777));
#119919=CARTESIAN_POINT('Ctrl Pts',(21.7523541253142,19.487211882838,-17.4197798233592));
#119920=CARTESIAN_POINT('Ctrl Pts',(20.6000283224083,16.8225500989152,-17.5469556300406));
#119921=CARTESIAN_POINT('Ctrl Pts',(17.7357373524709,16.3491428553155,-17.674131436722));
#119922=CARTESIAN_POINT('Ctrl Pts',(15.7872904024767,18.5013119150815,-17.8013072434035));
#119923=CARTESIAN_POINT('Ctrl Pts',(16.5422666147802,21.304575744541,-17.9284830500849));
#119924=CARTESIAN_POINT('Ctrl Pts',(19.3080221737182,22.1871137703668,-18.0556588567663));
#119925=CARTESIAN_POINT('Ctrl Pts',(21.5471480160826,20.3392521303006,-18.1828346634478));
#119926=CARTESIAN_POINT('Ctrl Pts',(21.2053851573897,17.4562891879729,-18.3100104701292));
#119927=CARTESIAN_POINT('Ctrl Pts',(18.5962798081749,16.1831645059201,-18.4371862768106));
#119928=CARTESIAN_POINT('Ctrl Pts',(16.1135241872327,17.6878909612598,-18.5643620834921));
#119929=CARTESIAN_POINT('Ctrl Pts',(16.0348924791393,20.5899754243741,-18.6915378901735));
#119930=CARTESIAN_POINT('Ctrl Pts',(18.4325243964945,22.226935525381,-18.8187136968549));
#119931=CARTESIAN_POINT('Ctrl Pts',(21.1067414672911,21.0969619702091,-18.9458895035364));
#119932=CARTESIAN_POINT('Ctrl Pts',(21.6041155128897,18.2367353666694,-19.0730653102178));
#119933=CARTESIAN_POINT('Ctrl Pts',(19.4683367108302,16.270336088174,-19.2002411168992));
#119934=CARTESIAN_POINT('Ctrl Pts',(16.6588495624458,17.0018134428338,-19.3274169235807));
#119935=CARTESIAN_POINT('Ctrl Pts',(15.7531841271558,19.760082322527,-19.4545927302621));
#119936=CARTESIAN_POINT('Ctrl Pts',(17.5822322738009,22.0146022966338,-19.5817685369435));
#119937=CARTESIAN_POINT('Ctrl Pts',(20.4679557667883,21.6969910872163,-19.708944343625));
#119938=CARTESIAN_POINT('Ctrl Pts',(21.7628825724515,19.0986375219567,-19.8361201503064));
#119939=CARTESIAN_POINT('Ctrl Pts',(20.2789974048699,16.6033692313319,-19.9632959569879));
#119940=CARTESIAN_POINT('Ctrl Pts',(17.3776734098626,16.5004409492398,-20.0904717636693));
#119941=CARTESIAN_POINT('Ctrl Pts',(15.7206941110155,18.8842811536826,-20.2176475703507));
#119942=CARTESIAN_POINT('Ctrl Pts',(16.8282374165171,21.5678679452165,-20.3448233770321));
#119943=CARTESIAN_POINT('Ctrl Pts',(19.6841967596975,22.0891702031096,-20.4719991837136));
#119944=CARTESIAN_POINT('Ctrl Pts',(21.668415038227,19.9699385658392,-20.5991749903951));
#119945=CARTESIAN_POINT('Ctrl Pts',(20.9604790789623,17.1544112786656,-20.7263507970764));
#119946=CARTESIAN_POINT('Ctrl Pts',(18.2099071213465,16.2257085193901,-20.8535266037579));
#119947=CARTESIAN_POINT('Ctrl Pts',(15.9401186134861,18.0357637096982,-20.9807024104393));
#119948=CARTESIAN_POINT('Ctrl Pts',(16.233618466875,20.9241441193076,-21.1078782171208));
#119949=CARTESIAN_POINT('Ctrl Pts',(18.8209175358886,22.2405921118336,-21.2350540238022));
#119950=CARTESIAN_POINT('Ctrl Pts',(21.3287557883375,20.7780186528654,-21.3622298304836));
#119951=CARTESIAN_POINT('Ctrl Pts',(21.4555258668686,17.8769523013118,-21.4894056371651));
#119952=CARTESIAN_POINT('Ctrl Pts',(19.0865078840121,16.2014340153418,-21.6165814438465));
#119953=CARTESIAN_POINT('Ctrl Pts',(16.3920658963632,17.2838096850018,-21.7437572505279));
#119954=CARTESIAN_POINT('Ctrl Pts',(15.8501931606037,20.1407252761597,-21.8709330572094));
#119955=CARTESIAN_POINT('Ctrl Pts',(17.2469900366476,21.4665547830909,-21.9557169283303));
#119956=CARTESIAN_POINT('Ctrl Pts',(18.0714160324376,21.6871591224115,-21.9981088638908));
#119957=CARTESIAN_POINT('Ctrl Pts',(20.3539256943887,20.5739122292573,4.33680868994202E-19));
#119958=CARTESIAN_POINT('Ctrl Pts',(20.4076089227952,20.5221116197655,8.86638463849601E-16));
#119959=CARTESIAN_POINT('Ctrl Pts',(20.4581355934374,20.4674384227593,2.54751254348717E-14));
#119960=CARTESIAN_POINT('Ctrl Pts',(20.5055119734051,20.410263943529,1.80931658544381E-15));
#119961=CARTESIAN_POINT('Ctrl Pts',(20.554575656102,20.3510532037209,-2.26993465278348E-14));
#119962=CARTESIAN_POINT('Ctrl Pts',(20.6002611628446,20.2891594084519,-2.64214052779902E-14));
#119963=CARTESIAN_POINT('Ctrl Pts',(20.6425471151747,20.2249453565124,-1.84539883374413E-14));
#119964=CARTESIAN_POINT('Ctrl Pts',(20.6826816163242,20.1639984273464,-1.08919426286634E-14));
#119965=CARTESIAN_POINT('Ctrl Pts',(20.7197537459369,20.1009604021273,8.86790207976305E-15));
#119966=CARTESIAN_POINT('Ctrl Pts',(20.753716758437,20.0361087206568,-9.26342336171615E-15));
#119967=CARTESIAN_POINT('Ctrl Pts',(20.7688150794711,20.0072787837823,-1.71121260304889E-14));
#119968=CARTESIAN_POINT('Ctrl Pts',(20.7832985639006,19.9780900549027,-2.84108754833378E-14));
#119969=CARTESIAN_POINT('Ctrl Pts',(20.7971611119739,19.9485653699547,-5.04457586814056E-15));
#119970=CARTESIAN_POINT('Ctrl Pts',(20.8039895160331,19.9340221216659,6.44146995798704E-15));
#119971=CARTESIAN_POINT('Ctrl Pts',(20.8106672398928,19.9193973462958,-1.4380597839645E-14));
#119972=CARTESIAN_POINT('Ctrl Pts',(20.8171934366481,19.9046937060787,-1.06165076729781E-14));
#119973=CARTESIAN_POINT('Ctrl Pts',(20.8232055554644,19.8911482928261,-7.43335609254726E-15));
#119974=CARTESIAN_POINT('Ctrl Pts',(20.8290895460591,19.8775345581707,-1.6413190692469E-15));
#119975=CARTESIAN_POINT('Ctrl Pts',(20.8348368052234,19.8638741231809,-4.3229309021342E-15));
#119976=CARTESIAN_POINT('Ctrl Pts',(20.8659056669685,19.7900277637341,-1.87793915734555E-14));
#119977=CARTESIAN_POINT('Ctrl Pts',(20.8930393190126,19.7146930410775,-3.51742239851522E-14));
#119978=CARTESIAN_POINT('Ctrl Pts',(20.9162161295942,19.6382510927703,-1.83048021185073E-14));
#119979=CARTESIAN_POINT('Ctrl Pts',(20.9398193031496,19.5604029105771,-1.1250486448073E-15));
#119980=CARTESIAN_POINT('Ctrl Pts',(20.9593192292438,19.4814055816641,-1.26531324379748E-14));
#119981=CARTESIAN_POINT('Ctrl Pts',(20.9746521650441,19.4016261052139,-4.85722573273506E-16));
#119982=CARTESIAN_POINT('Ctrl Pts',(20.9885844253231,19.3291345455208,1.05701850080071E-14));
#119983=CARTESIAN_POINT('Ctrl Pts',(20.9990759703875,19.2559962568409,-3.84562964731708E-15));
#119984=CARTESIAN_POINT('Ctrl Pts',(21.0060451898833,19.1824707413237,-1.37251321419285E-14));
#119985=CARTESIAN_POINT('Ctrl Pts',(21.0087031237876,19.1544294433498,-1.74137278270615E-14));
#119986=CARTESIAN_POINT('Ctrl Pts',(21.0108483731097,19.1263317159654,5.79109875787806E-15));
#119987=CARTESIAN_POINT('Ctrl Pts',(21.0124750503239,19.0981916687962,-1.26149091173033E-14));
#119988=CARTESIAN_POINT('Ctrl Pts',(21.0133685656744,19.0827346599387,-2.27851825805648E-14));
#119989=CARTESIAN_POINT('Ctrl Pts',(21.0141056048104,19.0672648807305,1.52001378915023E-15));
#119990=CARTESIAN_POINT('Ctrl Pts',(21.0146850898148,19.0517846622215,-5.00988139862102E-15));
#119991=CARTESIAN_POINT('Ctrl Pts',(21.0151328036157,19.0398245469222,-1.02380557977565E-14));
#119992=CARTESIAN_POINT('Ctrl Pts',(21.0154863000461,19.0278615000918,-2.2507103357516E-14));
#119993=CARTESIAN_POINT('Ctrl Pts',(21.015745158205,19.0159051388708,-1.89709359332824E-14));
#119994=CARTESIAN_POINT('Ctrl Pts',(21.017551908051,18.9324534374073,5.48211938410455E-15));
#119995=CARTESIAN_POINT('Ctrl Pts',(21.014756822678,18.8492079748144,1.85977283378329E-14));
#119996=CARTESIAN_POINT('Ctrl Pts',(21.0073036571099,18.7665493842094,1.59594559789866E-15));
#119997=CARTESIAN_POINT('Ctrl Pts',(20.9998648139147,18.6840496344554,-1.61673656061961E-14));
#119998=CARTESIAN_POINT('Ctrl Pts',(20.9877861501509,18.60213349936,-5.99635044273716E-15));
#119999=CARTESIAN_POINT('Ctrl Pts',(20.9709623839625,18.5211637972932,-8.99280649946377E-15));
#120000=CARTESIAN_POINT('Ctrl Pts',(20.9545246627898,18.4420520591064,-1.23431551296896E-14));
#120001=CARTESIAN_POINT('Ctrl Pts',(20.9335573250132,18.3638428657348,1.30025920795767E-14));
#120002=CARTESIAN_POINT('Ctrl Pts',(20.9083260331535,18.2867626991381,7.21644966006352E-16));
#120003=CARTESIAN_POINT('Ctrl Pts',(20.8979286030734,18.2549991395388,-4.46408057868302E-15));
#120004=CARTESIAN_POINT('Ctrl Pts',(20.886806477603,18.223427374722,-1.4774001875713E-14));
#120005=CARTESIAN_POINT('Ctrl Pts',(20.8749757625748,18.1920637286002,-7.46624984060418E-15));
#120006=CARTESIAN_POINT('Ctrl Pts',(20.868424493201,18.1746960805925,-3.19571242173869E-15));
#120007=CARTESIAN_POINT('Ctrl Pts',(20.8616536960862,18.1573871105346,-8.6285719324816E-15));
#120008=CARTESIAN_POINT('Ctrl Pts',(20.8546784987878,18.1401696684741,-5.19029264012261E-15));
#120009=CARTESIAN_POINT('Ctrl Pts',(20.8237193197693,18.06375062996,9.6487526525259E-15));
#120010=CARTESIAN_POINT('Ctrl Pts',(20.7887042347096,17.9890383341861,-9.83388335482747E-15));
#120011=CARTESIAN_POINT('Ctrl Pts',(20.7499612622237,17.916256394916,-1.42941214420489E-14));
#120012=CARTESIAN_POINT('Ctrl Pts',(20.7091543143746,17.8395971039635,-1.89919722093448E-14));
#120013=CARTESIAN_POINT('Ctrl Pts',(20.6642116622635,17.7650784733303,4.62724630464423E-15));
#120014=CARTESIAN_POINT('Ctrl Pts',(20.6154560962815,17.692967425201,-1.04916075827077E-14));
#120015=CARTESIAN_POINT('Ctrl Pts',(20.5667005302995,17.6208563770717,-2.56104614700597E-14));
#120016=CARTESIAN_POINT('Ctrl Pts',(20.5141314518022,17.55115202568,-2.07867077809236E-14));
#120017=CARTESIAN_POINT('Ctrl Pts',(20.4580183994378,17.484139989662,-2.21489493412719E-14));
#120018=CARTESIAN_POINT('Ctrl Pts',(20.4361046684505,17.457969897886,-2.30428670320704E-14));
#120019=CARTESIAN_POINT('Ctrl Pts',(20.4136499126721,17.4322106904206,-1.69753434272788E-15));
#120020=CARTESIAN_POINT('Ctrl Pts',(20.3906682863214,17.4068806089605,-9.07607322631065E-15));
#120021=CARTESIAN_POINT('Ctrl Pts',(20.3815365196799,17.3968156819022,-1.21213507505428E-14));
#120022=CARTESIAN_POINT('Ctrl Pts',(20.3723208008609,17.3868177123508,1.59343166306336E-14));
#120023=CARTESIAN_POINT('Ctrl Pts',(20.3630243250802,17.3768903879953,1.62925228863742E-14));
#120024=CARTESIAN_POINT('Ctrl Pts',(20.3025146980146,17.3122746444938,1.88054167317304E-14));
#120025=CARTESIAN_POINT('Ctrl Pts',(20.2387852814275,17.2508599884964,1.2995950010883E-14));
#120026=CARTESIAN_POINT('Ctrl Pts',(20.1721441631346,17.1929207844063,2.06223926824123E-14));
#120027=CARTESIAN_POINT('Ctrl Pts',(20.116951256814,17.1449348990317,2.69386962906269E-14));
#120028=CARTESIAN_POINT('Ctrl Pts',(20.0597599943144,17.0993329745171,-2.07314123176772E-15));
#120029=CARTESIAN_POINT('Ctrl Pts',(20.0007222400369,17.0562848434724,-1.36002320516582E-15));
#120030=CARTESIAN_POINT('Ctrl Pts',(19.9812253415778,17.0420684314475,-1.43164437014271E-15));
#120031=CARTESIAN_POINT('Ctrl Pts',(19.9615269094649,17.0281306668005,-7.66544549292576E-16));
#120032=CARTESIAN_POINT('Ctrl Pts',(19.9416319850871,17.0144780743264,-4.9960036108132E-15));
#120033=CARTESIAN_POINT('Ctrl Pts',(19.9257068710494,17.0035497044602,-8.18062758418038E-15));
#120034=CARTESIAN_POINT('Ctrl Pts',(19.9096544915251,16.9928033016912,-1.14146940178211E-14));
#120035=CARTESIAN_POINT('Ctrl Pts',(19.8934933769624,16.9822523936718,-9.88098491916389E-15));
#120036=CARTESIAN_POINT('Ctrl Pts',(19.8189655612139,16.9335963355889,-2.5256493517142E-15));
#120037=CARTESIAN_POINT('Ctrl Pts',(19.7420556121672,16.8890439678595,1.15006185245056E-14));
#120038=CARTESIAN_POINT('Ctrl Pts',(19.6630443965311,16.8488858958507,3.24740234702858E-15));
#120039=CARTESIAN_POINT('Ctrl Pts',(19.5852031544112,16.8093224720868,-5.05879407978434E-15));
#120040=CARTESIAN_POINT('Ctrl Pts',(19.5053217346575,16.774023445591,1.33716613157219E-14));
#120041=CARTESIAN_POINT('Ctrl Pts',(19.423636270734,16.7433040636654,-2.22044604925031E-16));
#120042=CARTESIAN_POINT('Ctrl Pts',(19.414941505442,16.7400342307853,-1.73426843035966E-15));
#120043=CARTESIAN_POINT('Ctrl Pts',(19.4062262753773,16.736816326208,-1.51681798593128E-14));
#120044=CARTESIAN_POINT('Ctrl Pts',(19.3974909960169,16.7336502196964,-9.99200722162641E-16));
#120045=CARTESIAN_POINT('Ctrl Pts',(18.071416109725,16.7348411664207,-0.001890963484983));
#120046=CARTESIAN_POINT('Ctrl Pts',(17.2469902101003,16.9554454800088,-0.0442828990454611));
#120047=CARTESIAN_POINT('Ctrl Pts',(15.8501940740727,18.2812783317349,-0.129066770166417));
#120048=CARTESIAN_POINT('Ctrl Pts',(16.3920656588252,21.1381881653492,-0.256242576847851));
#120049=CARTESIAN_POINT('Ctrl Pts',(19.0865079389648,22.2205670934987,-0.383418383529286));
#120050=CARTESIAN_POINT('Ctrl Pts',(21.4555257828913,20.5450469055032,-0.510594190210719));
#120051=CARTESIAN_POINT('Ctrl Pts',(21.3287556324384,17.643981848867,-0.637769996892156));
#120052=CARTESIAN_POINT('Ctrl Pts',(18.8209175760198,16.1814077573175,-0.764945803573588));
#120053=CARTESIAN_POINT('Ctrl Pts',(16.233618537572,17.4978560985894,-0.892121610255023));
#120054=CARTESIAN_POINT('Ctrl Pts',(15.9401187499945,20.386236157729,-1.01929741693645));
#120055=CARTESIAN_POINT('Ctrl Pts',(18.2099071291442,22.1962914055474,-1.14647322361789));
#120056=CARTESIAN_POINT('Ctrl Pts',(20.9604789958506,21.2675886098998,-1.27364903029932));
#120057=CARTESIAN_POINT('Ctrl Pts',(21.6684149124547,18.4520614803885,-1.40082483698076));
#120058=CARTESIAN_POINT('Ctrl Pts',(19.6841967236086,16.3328299069189,-1.52800064366219));
#120059=CARTESIAN_POINT('Ctrl Pts',(16.8282374931634,16.8541321563464,-1.65517645034363));
#120060=CARTESIAN_POINT('Ctrl Pts',(15.7206942359514,19.5377188303282,-1.78235225702506));
#120061=CARTESIAN_POINT('Ctrl Pts',(17.3776734650805,21.9215589406766,-1.9095280637065));
#120062=CARTESIAN_POINT('Ctrl Pts',(20.2789973416443,21.8186306606476,-2.03670387038792));
#120063=CARTESIAN_POINT('Ctrl Pts',(21.7628824476932,19.3233624738419,-2.16387967706936));
#120064=CARTESIAN_POINT('Ctrl Pts',(20.4679556955709,16.7250090148042,-2.29105548375079));
#120065=CARTESIAN_POINT('Ctrl Pts',(17.5822323211178,16.4073978188031,-2.41823129043223));
#120066=CARTESIAN_POINT('Ctrl Pts',(15.7531842497881,18.6619176999891,-2.54540709711366));
#120067=CARTESIAN_POINT('Ctrl Pts',(16.65884964778,21.4201864663384,-2.6725829037951));
#120068=CARTESIAN_POINT('Ctrl Pts',(19.468336680636,22.1516637908563,-2.79975871047653));
#120069=CARTESIAN_POINT('Ctrl Pts',(21.6041153948362,20.1852645932698,-2.92693451715797));
#120070=CARTESIAN_POINT('Ctrl Pts',(21.1067413697027,17.3250381073553,-3.0541103238394));
#120071=CARTESIAN_POINT('Ctrl Pts',(18.432524408893,16.1950645986679,-3.18128613052084));
#120072=CARTESIAN_POINT('Ctrl Pts',(16.0348925901549,17.8320246323415,-3.30846193720227));
#120073=CARTESIAN_POINT('Ctrl Pts',(16.1135242950128,20.7341089760952,-3.43563774388371));
#120074=CARTESIAN_POINT('Ctrl Pts',(18.5962798138393,22.2388353695441,-3.56281355056514));
#120075=CARTESIAN_POINT('Ctrl Pts',(21.2053850557409,20.9657107398561,-3.68998935724658));
#120076=CARTESIAN_POINT('Ctrl Pts',(21.5471479003775,18.0827479161047,-3.81716516392801));
#120077=CARTESIAN_POINT('Ctrl Pts',(19.3080221501088,16.2348863520412,-3.94434097060945));
#120078=CARTESIAN_POINT('Ctrl Pts',(16.5422667049268,17.1174243415679,-4.07151677729087));
#120079=CARTESIAN_POINT('Ctrl Pts',(15.7872905236753,19.9206880557286,-4.19869258397231));
#120080=CARTESIAN_POINT('Ctrl Pts',(17.7357373935294,22.0728570269757,-4.32586839065374));
#120081=CARTESIAN_POINT('Ctrl Pts',(20.6000282456582,21.5994498028477,-4.45304419733518));
#120082=CARTESIAN_POINT('Ctrl Pts',(21.7523540011689,18.9347881285228,-4.58022000401661));
#120083=CARTESIAN_POINT('Ctrl Pts',(20.1355273007852,16.5235337026348,-4.70739581069805));
#120084=CARTESIAN_POINT('Ctrl Pts',(17.2328862905255,16.5778628016098,-4.83457161737948));
#120085=CARTESIAN_POINT('Ctrl Pts',(15.7074239390844,19.0479318491813,-4.96174742406092));
#120086=CARTESIAN_POINT('Ctrl Pts',(16.9586572730372,21.6676058039782,-5.08892323074234));
#120087=CARTESIAN_POINT('Ctrl Pts',(19.8386573687817,22.0334964077772,-5.21609903742379));
#120088=CARTESIAN_POINT('Ctrl Pts',(21.7052028914376,19.8099217413247,-5.34327484410521));
#120089=CARTESIAN_POINT('Ctrl Pts',(20.8458541748489,17.0368735504825,-5.47045065078666));
#120090=CARTESIAN_POINT('Ctrl Pts',(18.0490103292891,16.2584514355665,-5.59762645746809));
#120091=CARTESIAN_POINT('Ctrl Pts',(15.8806019913527,18.188809372687,-5.72480226414952));
#120092=CARTESIAN_POINT('Ctrl Pts',(16.3300092244964,21.0569637660617,-5.85197807083096));
#120093=CARTESIAN_POINT('Ctrl Pts',(18.9849287856695,22.2315609775075,-5.97915387751239));
#120094=CARTESIAN_POINT('Ctrl Pts',(21.4096367603877,20.634980969248,-6.10632968419383));
#120095=CARTESIAN_POINT('Ctrl Pts',(21.3796140761966,17.73198680393,-6.23350549087526));
#120096=CARTESIAN_POINT('Ctrl Pts',(18.9224046824235,16.1858954480944,-6.36068129755669));
#120097=CARTESIAN_POINT('Ctrl Pts',(16.2923456862402,17.4151497594685,-6.48785710423813));
#120098=CARTESIAN_POINT('Ctrl Pts',(15.9023529767735,20.2919852034935,-6.61503291091956));
#120099=CARTESIAN_POINT('Ctrl Pts',(18.1102206592817,22.1770838168218,-6.742208717601));
#120100=CARTESIAN_POINT('Ctrl Pts',(20.8903671707866,21.3409846241399,-6.86938452428244));
#120101=CARTESIAN_POINT('Ctrl Pts',(21.6921806423356,18.550756740565,-6.99656033096386));
#120102=CARTESIAN_POINT('Ctrl Pts',(19.7800469799392,16.3662610682035,-7.1237361376453));
#120103=CARTESIAN_POINT('Ctrl Pts',(16.9082301384463,16.7916368013544,-7.25091194432673));
#120104=CARTESIAN_POINT('Ctrl Pts',(15.7114438248711,19.4366281066474,-7.37808775100818));
#120105=CARTESIAN_POINT('Ctrl Pts',(17.2876652009831,21.8746196281511,-7.50526355768959));
#120106=CARTESIAN_POINT('Ctrl Pts',(20.1908089855312,21.8689054637052,-7.63243936437104));
#120107=CARTESIAN_POINT('Ctrl Pts',(21.7574209456176,19.4247280045279,-7.75961517105247));
#120108=CARTESIAN_POINT('Ctrl Pts',(20.5502318427671,16.7844683666522,-7.88679097773391));
#120109=CARTESIAN_POINT('Ctrl Pts',(17.6767627522393,16.3704008948346,-8.01396678441534));
#120110=CARTESIAN_POINT('Ctrl Pts',(15.7732432169878,18.562406794542,-8.14114259109678));
#120111=CARTESIAN_POINT('Ctrl Pts',(16.5860342648591,21.3494567040227,-8.2683183977782));
#120112=CARTESIAN_POINT('Ctrl Pts',(19.3694505569332,22.1746053151545,-8.39549420445964));
#120113=CARTESIAN_POINT('Ctrl Pts',(21.5698804035306,20.2808299917227,-8.52267001114108));
#120114=CARTESIAN_POINT('Ctrl Pts',(21.1685659944773,17.4055520520233,-8.64984581782251));
#120115=CARTESIAN_POINT('Ctrl Pts',(18.5336883916982,16.1866605458549,-8.77702162450395));
#120116=CARTESIAN_POINT('Ctrl Pts',(16.0825842567954,17.7424127771882,-8.90419743118537));
#120117=CARTESIAN_POINT('Ctrl Pts',(16.0639895008622,20.6455026346484,-9.03137323786682));
#120118=CARTESIAN_POINT('Ctrl Pts',(18.4949636583467,22.2325253600934,-9.15854904454825));
#120119=CARTESIAN_POINT('Ctrl Pts',(21.1452388230294,21.0474861046668,-9.28572485122969));
#120120=CARTESIAN_POINT('Ctrl Pts',(21.5833520259422,18.1775848333912,-9.41290065791111));
#120121=CARTESIAN_POINT('Ctrl Pts',(19.4073615957849,16.2557778365002,-9.54007646459256));
#120122=CARTESIAN_POINT('Ctrl Pts',(16.6136036950289,17.0452037528466,-9.66725227127399));
#120123=CARTESIAN_POINT('Ctrl Pts',(15.7651777974467,19.8216133014809,-9.79442807795542));
#120124=CARTESIAN_POINT('Ctrl Pts',(17.6404620048199,22.0378230449422,-9.92160388463685));
#120125=CARTESIAN_POINT('Ctrl Pts',(20.5189994501482,21.6605980970946,-10.0487796913183));
#120126=CARTESIAN_POINT('Ctrl Pts',(21.7599106895262,19.0360189343673,-10.1759554979997));
#120127=CARTESIAN_POINT('Ctrl Pts',(20.2247366804621,16.5719740388084,-10.3031313046812));
#120128=CARTESIAN_POINT('Ctrl Pts',(17.3219042926274,16.5290716662188,-10.4303071113626));
#120129=CARTESIAN_POINT('Ctrl Pts',(15.7145820717629,18.9466720806279,-10.557482918044));
#120130=CARTESIAN_POINT('Ctrl Pts',(16.8773883938439,21.60677695502,-10.6846587247255));
#120131=CARTESIAN_POINT('Ctrl Pts',(19.7435206302607,22.0689051718692,-10.8118345314069));
#120132=CARTESIAN_POINT('Ctrl Pts',(21.6834803463302,19.9090827751282,-10.9390103380884));
#120133=CARTESIAN_POINT('Ctrl Pts',(20.9174749100379,17.1088127601106,-11.0661861447698));
#120134=CARTESIAN_POINT('Ctrl Pts',(18.1482667655227,16.2371690612364,-11.1933619514512));
#120135=CARTESIAN_POINT('Ctrl Pts',(15.9164325089359,18.0938306719134,-11.3205377581326));
#120136=CARTESIAN_POINT('Ctrl Pts',(16.2695415474392,20.9754258017613,-11.4477135648141));
#120137=CARTESIAN_POINT('Ctrl Pts',(18.8836382546247,22.2382697711092,-11.5748893714955));
#120138=CARTESIAN_POINT('Ctrl Pts',(21.3604511507894,20.7237816190169,-11.702065178177));
#120139=CARTESIAN_POINT('Ctrl Pts',(21.4276581320481,17.8214102252931,-11.8292409848584));
#120140=CARTESIAN_POINT('Ctrl Pts',(19.0236009644314,16.1939012021945,-11.9564167915398));
#120141=CARTESIAN_POINT('Ctrl Pts',(16.353852886612,17.3343930638118,-12.0835925982213));
#120142=CARTESIAN_POINT('Ctrl Pts',(15.8677420567354,20.1965553140193,-12.2107684049027));
#120143=CARTESIAN_POINT('Ctrl Pts',(18.0112449897728,22.1545317340756,-12.3379442115841));
#120144=CARTESIAN_POINT('Ctrl Pts',(20.8178307854584,21.4120004843013,-12.4651200182656));
#120145=CARTESIAN_POINT('Ctrl Pts',(21.712631172611,18.6501878996771,-12.592295824947));
#120146=CARTESIAN_POINT('Ctrl Pts',(19.8747223335935,16.4028856091748,-12.7194716316284));
#120147=CARTESIAN_POINT('Ctrl Pts',(16.9902715547168,16.731853981019,-12.8466474383099));
#120148=CARTESIAN_POINT('Ctrl Pts',(15.7055833963943,19.3352849521227,-12.9738232449913));
#120149=CARTESIAN_POINT('Ctrl Pts',(17.199279507147,21.824692193648,-13.1009990516727));
#120150=CARTESIAN_POINT('Ctrl Pts',(20.1009864145957,21.9161990715341,-13.2281748583542));
#120151=CARTESIAN_POINT('Ctrl Pts',(21.7485681313984,19.5258537048782,-13.3553506650356));
#120152=CARTESIAN_POINT('Ctrl Pts',(20.6304706928427,16.8466496060213,-13.482526471717));
#120153=CARTESIAN_POINT('Ctrl Pts',(17.77247910185,16.3365902455044,-13.6097022783985));
#120154=CARTESIAN_POINT('Ctrl Pts',(15.7966232561924,18.4636234287474,-13.7368780850799));
#120155=CARTESIAN_POINT('Ctrl Pts',(16.5156282588163,21.2763282286931,-13.8640538917614));
#120156=CARTESIAN_POINT('Ctrl Pts',(19.2698516462976,22.1942225675398,-13.9912296984428));
#120157=CARTESIAN_POINT('Ctrl Pts',(21.5324644070049,20.3751953603434,-14.1184055051242));
#120158=CARTESIAN_POINT('Ctrl Pts',(21.2276597665751,17.4880911681452,-14.2455813118056));
#120159=CARTESIAN_POINT('Ctrl Pts',(18.635077064293,16.1816488933915,-14.3727571184871));
#120160=CARTESIAN_POINT('Ctrl Pts',(16.1332500156721,17.6544482362164,-14.4999329251685));
#120161=CARTESIAN_POINT('Ctrl Pts',(16.0174496569233,20.5552872118146,-14.6271087318499));
#120162=CARTESIAN_POINT('Ctrl Pts',(18.3939156298174,22.2228261064472,-14.7542845385314));
#120163=CARTESIAN_POINT('Ctrl Pts',(21.0823879043376,21.1272014834248,-14.8814603452128));
#120164=CARTESIAN_POINT('Ctrl Pts',(21.6163600340196,18.2735809322375,-15.0086361518943));
#120165=CARTESIAN_POINT('Ctrl Pts',(19.5059457319285,16.279984192933,-15.1358119585757));
#120166=CARTESIAN_POINT('Ctrl Pts',(16.6873191331485,16.975412537255,-15.2629877652571));
#120167=CARTESIAN_POINT('Ctrl Pts',(15.7463951983637,19.7218536224386,-15.3901635719385));
#120168=CARTESIAN_POINT('Ctrl Pts',(17.5464132374134,21.9996182161866,-15.51733937862));
#120169=CARTESIAN_POINT('Ctrl Pts',(20.4359684211888,21.7189986777498,-15.6445151853014));
#120170=CARTESIAN_POINT('Ctrl Pts',(21.7640732145973,19.137446016431,-15.7716909919829));
#120171=CARTESIAN_POINT('Ctrl Pts',(20.3122739011664,16.6233745697617,-15.8988667986643));
#120172=CARTESIAN_POINT('Ctrl Pts',(17.4125062421414,16.4832888491888,-16.0260426053457));
#120173=CARTESIAN_POINT('Ctrl Pts',(15.7251270847987,18.8457088086375,-16.1532184120272));
#120174=CARTESIAN_POINT('Ctrl Pts',(16.7982020754384,21.543260763633,-16.2803942187086));
#120175=CARTESIAN_POINT('Ctrl Pts',(19.6472515126938,22.1011082244237,-16.40757002539));
#120176=CARTESIAN_POINT('Ctrl Pts',(21.6584493698341,20.0074607696524,-16.5347458320715));
#120177=CARTESIAN_POINT('Ctrl Pts',(20.9866464419503,17.1831099926555,-16.6619216387529));
#120178=CARTESIAN_POINT('Ctrl Pts',(18.2481802185833,16.2192224323484,-16.7890974454343));
#120179=CARTESIAN_POINT('Ctrl Pts',(15.9554234912899,18.0001050997038,-16.9162732521158));
#120180=CARTESIAN_POINT('Ctrl Pts',(16.2118382528302,20.8919086814673,-17.0434490587972));
#120181=CARTESIAN_POINT('Ctrl Pts',(18.782179874386,22.2415828769435,-17.1706248654786));
#120182=CARTESIAN_POINT('Ctrl Pts',(21.3083194515728,20.8108853820109,-17.2978006721601));
#120183=CARTESIAN_POINT('Ctrl Pts',(21.4726807122266,17.9123923491693,-17.4249764788415));
#120184=CARTESIAN_POINT('Ctrl Pts',(19.1244724011078,16.2052912352836,-17.552152285523));
#120185=CARTESIAN_POINT('Ctrl Pts',(16.418029897423,17.2557413577005,-17.6793280922044));
#120186=CARTESIAN_POINT('Ctrl Pts',(15.8363462175366,20.1000199273879,-17.8065038988858));
#120187=CARTESIAN_POINT('Ctrl Pts',(17.9130800343833,22.1286778924994,-17.9336797055672));
#120188=CARTESIAN_POINT('Ctrl Pts',(20.7429569676441,21.4805474827506,-18.0608555122487));
#120189=CARTESIAN_POINT('Ctrl Pts',(21.7297405730228,18.7502481215919,-18.1880313189301));
#120190=CARTESIAN_POINT('Ctrl Pts',(19.9681181392836,16.4426600113656,-18.3152071256115));
#120191=CARTESIAN_POINT('Ctrl Pts',(17.0742689107603,16.6748520181929,-18.442382932293));
#120192=CARTESIAN_POINT('Ctrl Pts',(15.7031199420884,19.2338023871561,-18.5695587389744));
#120193=CARTESIAN_POINT('Ctrl Pts',(17.1126153089119,21.7718329813254,-18.6967345456558));
#120194=CARTESIAN_POINT('Ctrl Pts',(20.0096304953375,21.9604582580674,-18.8239103523373));
#120195=CARTESIAN_POINT('Ctrl Pts',(21.7363338768253,19.6266262342004,-18.9510861590187));
#120196=CARTESIAN_POINT('Ctrl Pts',(20.708582272227,16.9114829360825,-19.0782619657001));
#120197=CARTESIAN_POINT('Ctrl Pts',(17.8692739891718,16.3060038219983,-19.2054377723816));
#120198=CARTESIAN_POINT('Ctrl Pts',(15.8232981502683,18.3656783929507,-19.332613579063));
#120199=CARTESIAN_POINT('Ctrl Pts',(16.4477105996423,21.2008830792771,-19.4597893857445));
#120200=CARTESIAN_POINT('Ctrl Pts',(19.1696516713374,22.2104935320204,-19.5869651924259));
#120201=CARTESIAN_POINT('Ctrl Pts',(21.4919093729839,20.4682548664865,-19.7141409991073));
#120202=CARTESIAN_POINT('Ctrl Pts',(21.2839564023691,17.5725628414412,-19.8413168057888));
#120203=CARTESIAN_POINT('Ctrl Pts',(18.7365766963097,16.1800353196856,-19.9684926124702));
#120204=CARTESIAN_POINT('Ctrl Pts',(16.186833039821,17.5682295703764,-20.0956684191516));
#120205=CARTESIAN_POINT('Ctrl Pts',(15.9739569578914,20.4635641116309,-20.222844225833));
#120206=CARTESIAN_POINT('Ctrl Pts',(18.2932490910976,22.2097480848697,-20.3500200325145));
#120207=CARTESIAN_POINT('Ctrl Pts',(21.0169027662538,21.2047682366741,-20.4771958391959));
#120208=CARTESIAN_POINT('Ctrl Pts',(21.6461349636216,18.3706270360342,-20.6043716458773));
#120209=CARTESIAN_POINT('Ctrl Pts',(19.6036638532537,16.3074811554586,-20.7315474525588));
#120210=CARTESIAN_POINT('Ctrl Pts',(16.7633305706532,16.9081234172833,-20.8587232592402));
#120211=CARTESIAN_POINT('Ctrl Pts',(15.7309633363042,19.6215316380409,-20.9858990659217));
#120212=CARTESIAN_POINT('Ctrl Pts',(17.4536974694716,21.9582647385426,-21.1130748726031));
#120213=CARTESIAN_POINT('Ctrl Pts',(20.3510265917206,21.7746258438458,-21.2402506792845));
#120214=CARTESIAN_POINT('Ctrl Pts',(21.7648401891172,19.2388788921253,-21.367426485966));
#120215=CARTESIAN_POINT('Ctrl Pts',(20.3980344469297,16.677825473566,-21.4946022926474));
#120216=CARTESIAN_POINT('Ctrl Pts',(17.5046027110691,16.4402807821758,-21.6217780993288));
#120217=CARTESIAN_POINT('Ctrl Pts',(15.7390235403886,18.7457046750729,-21.7489539060103));
#120218=CARTESIAN_POINT('Ctrl Pts',(16.7212335728181,21.4760667201902,-21.8761297126917));
#120219=CARTESIAN_POINT('Ctrl Pts',(19.5498596762323,22.1321442401452,-22.0033055193731));
#120220=CARTESIAN_POINT('Ctrl Pts',(21.6307161859342,20.100377524994,-22.1304999838292));
#120221=CARTESIAN_POINT('Ctrl Pts',(21.2446789959721,18.2129921435845,-22.2153025127247));
#120222=CARTESIAN_POINT('Ctrl Pts',(20.6946892744878,17.5599162803241,-22.2577131060598));
#120223=CARTESIAN_POINT('Ctrl Pts',(18.1101968784744,16.8797697475724,0.0847274365222686));
#120224=CARTESIAN_POINT('Ctrl Pts',(17.3340242953481,17.0874621793657,0.0423355009617904));
#120225=CARTESIAN_POINT('Ctrl Pts',(16.0189820756719,18.3356945672447,-0.0424483701591659));
#120226=CARTESIAN_POINT('Ctrl Pts',(16.5291381343926,21.0253906167311,-0.1696241768406));
#120227=CARTESIAN_POINT('Ctrl Pts',(19.065875791,22.0444183413159,-0.296799983522035));
#120228=CARTESIAN_POINT('Ctrl Pts',(21.2962359728301,20.4669656763903,-0.423975790203469));
#120229=CARTESIAN_POINT('Ctrl Pts',(21.1768856283234,17.7356987913358,-0.551151596884904));
#120230=CARTESIAN_POINT('Ctrl Pts',(18.8158303252349,16.3587285734324,-0.678327403566337));
#120231=CARTESIAN_POINT('Ctrl Pts',(16.3799648594531,17.5981257224815,-0.805503210247772));
#120232=CARTESIAN_POINT('Ctrl Pts',(16.1036434964602,20.3174500578439,-0.932679016929205));
#120233=CARTESIAN_POINT('Ctrl Pts',(18.2405820741981,22.0215634996219,-1.05985482361064));
#120234=CARTESIAN_POINT('Ctrl Pts',(20.8301640752336,21.1472173052792,-1.18703063029207));
#120235=CARTESIAN_POINT('Ctrl Pts',(21.4966647872182,18.4964818468598,-1.31420643697351));
#120236=CARTESIAN_POINT('Ctrl Pts',(19.6285820913403,16.501288045487,-1.44138224365494));
#120237=CARTESIAN_POINT('Ctrl Pts',(16.9397810066015,16.992078683811,-1.56855805033638));
#120238=CARTESIAN_POINT('Ctrl Pts',(15.8970618110187,19.518596108525,-1.69573385701782));
#120239=CARTESIAN_POINT('Ctrl Pts',(17.4570587119471,21.7629110154817,-1.82290966369925));
#120240=CARTESIAN_POINT('Ctrl Pts',(20.1885692683029,21.6660070863072,-1.95008547038068));
#120241=CARTESIAN_POINT('Ctrl Pts',(21.5856031755938,19.3167859434159,-2.07726127706212));
#120242=CARTESIAN_POINT('Ctrl Pts',(20.3664679657325,16.8705130678377,-2.20443708374355));
#120243=CARTESIAN_POINT('Ctrl Pts',(17.64964482037,16.5714915274638,-2.33161289042498));
#120244=CARTESIAN_POINT('Ctrl Pts',(15.927650197406,18.6940552662862,-2.45878869710642));
#120245=CARTESIAN_POINT('Ctrl Pts',(16.780307363717,21.2908836705225,-2.58596450378785));
#120246=CARTESIAN_POINT('Ctrl Pts',(19.4253562499103,21.979547921279,-2.71314031046929));
#120247=CARTESIAN_POINT('Ctrl Pts',(21.4361286945186,20.128241278265,-2.84031611715073));
#120248=CARTESIAN_POINT('Ctrl Pts',(20.9678657711395,17.4354226988042,-2.96749192383215));
#120249=CARTESIAN_POINT('Ctrl Pts',(18.4501696540519,16.3715860853484,-3.0946677305136));
#120250=CARTESIAN_POINT('Ctrl Pts',(16.1928702618537,17.9127355062838,-3.22184353719502));
#120251=CARTESIAN_POINT('Ctrl Pts',(16.2668996846349,20.6449620199907,-3.34901934387646));
#120252=CARTESIAN_POINT('Ctrl Pts',(18.6043405209739,22.0616173825078,-3.47619515055789));
#120253=CARTESIAN_POINT('Ctrl Pts',(21.0607358818871,20.8630082256189,-3.60337095723933));
#120254=CARTESIAN_POINT('Ctrl Pts',(21.3824954846104,18.1487840570351,-3.73054676392076));
#120255=CARTESIAN_POINT('Ctrl Pts',(19.2744248644109,16.4090770875045,-3.8577225706022));
#120256=CARTESIAN_POINT('Ctrl Pts',(16.6705479736445,17.2399604832709,-3.98489837728363));
#120257=CARTESIAN_POINT('Ctrl Pts',(15.9597602447928,19.8791502991104,-4.11207418396507));
#120258=CARTESIAN_POINT('Ctrl Pts',(17.7941653025999,21.9053536856092,-4.23924999064649));
#120259=CARTESIAN_POINT('Ctrl Pts',(20.4908103625543,21.4596547960069,-4.36642579732794));
#120260=CARTESIAN_POINT('Ctrl Pts',(21.5756909548122,18.9509546983274,-4.49360160400936));
#120261=CARTESIAN_POINT('Ctrl Pts',(20.0534964712626,16.6808300246996,-4.62077741069081));
#120262=CARTESIAN_POINT('Ctrl Pts',(17.3207458725165,16.7319792633511,-4.74795321737223));
#120263=CARTESIAN_POINT('Ctrl Pts',(15.8845682192929,19.0574761624978,-4.87512902405368));
#120264=CARTESIAN_POINT('Ctrl Pts',(17.062567369186,21.5238216537891,-5.0023048307351));
#120265=CARTESIAN_POINT('Ctrl Pts',(19.7740022170421,21.86829682763,-5.12948063741654));
#120266=CARTESIAN_POINT('Ctrl Pts',(21.5312995805795,19.7748670925622,-5.25665644409798));
#120267=CARTESIAN_POINT('Ctrl Pts',(20.7222481989278,17.1641242976074,-5.3838322507794));
#120268=CARTESIAN_POINT('Ctrl Pts',(18.0891024993605,16.4312629161638,-5.51100805746085));
#120269=CARTESIAN_POINT('Ctrl Pts',(16.0476102297768,18.2486377791988,-5.63818386414227));
#120270=CARTESIAN_POINT('Ctrl Pts',(16.4707138382194,20.948920248883,-5.76535967082371));
#120271=CARTESIAN_POINT('Ctrl Pts',(18.9702420247138,22.0547687577129,-5.89253547750515));
#120272=CARTESIAN_POINT('Ctrl Pts',(21.253032816367,20.5516359355363,-6.01971128418657));
#120273=CARTESIAN_POINT('Ctrl Pts',(21.2247673478128,17.8185528517555,-6.14688709086802));
#120274=CARTESIAN_POINT('Ctrl Pts',(18.911377432097,16.3629536014721,-6.27406289754945));
#120275=CARTESIAN_POINT('Ctrl Pts',(16.4352547317172,17.5202601521426,-6.40123870423088));
#120276=CARTESIAN_POINT('Ctrl Pts',(16.0680881387646,20.2287155740725,-6.52841451091232));
#120277=CARTESIAN_POINT('Ctrl Pts',(18.1467302133443,22.003480123343,-6.65559031759375));
#120278=CARTESIAN_POINT('Ctrl Pts',(20.7641558671069,21.2163174803099,-6.78276612427519));
#120279=CARTESIAN_POINT('Ctrl Pts',(21.5190395184827,18.5894005131322,-6.90994193095662));
#120280=CARTESIAN_POINT('Ctrl Pts',(19.718822270698,16.5327624943404,-7.03711773763806));
#120281=CARTESIAN_POINT('Ctrl Pts',(17.0150917145117,16.9332411568245,-7.16429354431949));
#120282=CARTESIAN_POINT('Ctrl Pts',(15.8883528227805,19.4234221842643,-7.29146935100092));
#120283=CARTESIAN_POINT('Ctrl Pts',(17.3723185953652,21.7187190420494,-7.41864515768236));
#120284=CARTESIAN_POINT('Ctrl Pts',(20.1055425412228,21.7133393253515,-7.54582096436379));
#120285=CARTESIAN_POINT('Ctrl Pts',(21.5804613330392,19.4122185903382,-7.67299677104523));
#120286=CARTESIAN_POINT('Ctrl Pts',(20.4439285231071,16.9264922877238,-7.80017257772666));
#120287=CARTESIAN_POINT('Ctrl Pts',(17.7386424233578,16.5366600185829,-7.9273483844081));
#120288=CARTESIAN_POINT('Ctrl Pts',(15.946535121319,18.600368694133,-8.05452419108952));
#120289=CARTESIAN_POINT('Ctrl Pts',(16.7117538358879,21.2242936927628,-8.18169999777097));
#120290=CARTESIAN_POINT('Ctrl Pts',(19.3322578912771,22.0011466873821,-8.30887580445239));
#120291=CARTESIAN_POINT('Ctrl Pts',(21.4038974634922,20.2182132723624,-8.43605161113384));
#120292=CARTESIAN_POINT('Ctrl Pts',(21.0260718254785,17.5112241946562,-8.56322741781526));
#120293=CARTESIAN_POINT('Ctrl Pts',(18.5454125496099,16.3636739183683,-8.69040322449671));
#120294=CARTESIAN_POINT('Ctrl Pts',(16.237770554417,17.82836859699,-8.81757903117813));
#120295=CARTESIAN_POINT('Ctrl Pts',(16.2202641420738,20.5615417720903,-8.94475483785957));
#120296=CARTESIAN_POINT('Ctrl Pts',(18.5089543593347,22.0556766953737,-9.071930644541));
#120297=CARTESIAN_POINT('Ctrl Pts',(21.0041099839982,20.9399973111998,-9.19910645122244));
#120298=CARTESIAN_POINT('Ctrl Pts',(21.4165805972594,18.2380702076759,-9.32628225790388));
#120299=CARTESIAN_POINT('Ctrl Pts',(19.3679500122646,16.4287458017761,-9.4534580645853));
#120300=CARTESIAN_POINT('Ctrl Pts',(16.7377096383923,17.1719669365758,-9.58063387126675));
#120301=CARTESIAN_POINT('Ctrl Pts',(15.9389417675414,19.7858743504024,-9.70780967794817));
#120302=CARTESIAN_POINT('Ctrl Pts',(17.7044663440924,21.8723702284609,-9.83498548462961));
#120303=CARTESIAN_POINT('Ctrl Pts',(20.4145241498733,21.5172241051723,-9.96216129131105));
#120304=CARTESIAN_POINT('Ctrl Pts',(21.5828053532376,19.0462605057991,-10.0893370979925));
#120305=CARTESIAN_POINT('Ctrl Pts',(20.1374844618078,16.7264351674692,-10.2165129046739));
#120306=CARTESIAN_POINT('Ctrl Pts',(17.4045536867392,16.6860438535011,-10.3436887113554));
#120307=CARTESIAN_POINT('Ctrl Pts',(15.8913073893432,18.9621430874931,-10.4708645180368));
#120308=CARTESIAN_POINT('Ctrl Pts',(16.986055124823,21.4665530929081,-10.5980403247182));
#120309=CARTESIAN_POINT('Ctrl Pts',(19.6844337935833,21.9016331309934,-10.7252161313997));
#120310=CARTESIAN_POINT('Ctrl Pts',(21.5108484473051,19.8682242709185,-10.8523919380811));
#120311=CARTESIAN_POINT('Ctrl Pts',(20.7896770012766,17.2318529342145,-10.9795677447625));
#120312=CARTESIAN_POINT('Ctrl Pts',(18.182549496281,16.4112261906481,-11.106743551444));
#120313=CARTESIAN_POINT('Ctrl Pts',(16.0813436015692,18.1592181436015,-11.2339193581254));
#120314=CARTESIAN_POINT('Ctrl Pts',(16.4137853099934,20.8721546688561,-11.3610951648069));
#120315=CARTESIAN_POINT('Ctrl Pts',(18.8748799877338,22.0610848883219,-11.4882709714883));
#120316=CARTESIAN_POINT('Ctrl Pts',(21.2067260207266,20.6352391189707,-11.6154467781697));
#120317=CARTESIAN_POINT('Ctrl Pts',(21.2699994043883,17.902742356213,-11.7426225848512));
#120318=CARTESIAN_POINT('Ctrl Pts',(19.0066507363984,16.3704907820029,-11.8697983915326));
#120319=CARTESIAN_POINT('Ctrl Pts',(16.4931619403762,17.4442301134199,-11.996974198214));
#120320=CARTESIAN_POINT('Ctrl Pts',(16.0355029819632,20.1388711576679,-12.1241500048955));
#120321=CARTESIAN_POINT('Ctrl Pts',(18.053547549985,21.9822480049345,-12.2513258115769));
#120322=CARTESIAN_POINT('Ctrl Pts',(20.6958650072534,21.2831768107233,-12.3785016182583));
#120323=CARTESIAN_POINT('Ctrl Pts',(21.5382930874419,18.6830120064713,-12.5056774249398));
#120324=CARTESIAN_POINT('Ctrl Pts',(19.807956313961,16.5672434156512,-12.6328532316212));
#120325=CARTESIAN_POINT('Ctrl Pts',(17.0923312796673,16.8769574009315,-12.7600290383026));
#120326=CARTESIAN_POINT('Ctrl Pts',(15.8828354028266,19.3280106038356,-12.8872048449841));
#120327=CARTESIAN_POINT('Ctrl Pts',(17.2891060806598,21.6717138402177,-13.0143806516655));
#120328=CARTESIAN_POINT('Ctrl Pts',(20.0209772492569,21.7578648573255,-13.1415564583469));
#120329=CARTESIAN_POINT('Ctrl Pts',(21.5721266704775,19.507425444098,-13.2687322650284));
#120330=CARTESIAN_POINT('Ctrl Pts',(20.5194710255427,16.9850340841485,-13.3959080717098));
#120331=CARTESIAN_POINT('Ctrl Pts',(17.8287565335022,16.5048282929666,-13.5230838783912));
#120332=CARTESIAN_POINT('Ctrl Pts',(15.9685467362274,18.5073670790289,-13.6502596850727));
#120333=CARTESIAN_POINT('Ctrl Pts',(16.6454686650766,21.1554453976977,-13.7774354917541));
#120334=CARTESIAN_POINT('Ctrl Pts',(19.2384884648439,22.0196157498711,-13.9046112984355));
#120335=CARTESIAN_POINT('Ctrl Pts',(21.3686714102025,20.3070554738911,-14.031787105117));
#120336=CARTESIAN_POINT('Ctrl Pts',(21.0817068628502,17.5889323294909,-14.1589629117984));
#120337=CARTESIAN_POINT('Ctrl Pts',(18.6408669839544,16.3589555959089,-14.2861387184799));
#120338=CARTESIAN_POINT('Ctrl Pts',(16.2854708667935,17.7455525852409,-14.4133145251613));
#120339=CARTESIAN_POINT('Ctrl Pts',(16.1764482564922,20.4766066216898,-14.5404903318427));
#120340=CARTESIAN_POINT('Ctrl Pts',(18.4138206312956,22.0465451351444,-14.6676661385241));
#120341=CARTESIAN_POINT('Ctrl Pts',(20.9449377043124,21.0150469808834,-14.7948419452056));
#120342=CARTESIAN_POINT('Ctrl Pts',(21.4476566598927,18.3284476934456,-14.922017751887));
#120343=CARTESIAN_POINT('Ctrl Pts',(19.4607640585489,16.4515353698976,-15.0491935585684));
#120344=CARTESIAN_POINT('Ctrl Pts',(16.8071105415512,17.1062605727777,-15.1763693652499));
#120345=CARTESIAN_POINT('Ctrl Pts',(15.9212585064325,19.6919535652726,-15.3035451719313));
#120346=CARTESIAN_POINT('Ctrl Pts',(17.615922213236,21.8364015129747,-15.4307209786127));
#120347=CARTESIAN_POINT('Ctrl Pts',(20.3363528936617,21.5722065233178,-15.5578967852942));
#120348=CARTESIAN_POINT('Ctrl Pts',(21.5867242473895,19.1417511015219,-15.6850725919756));
#120349=CARTESIAN_POINT('Ctrl Pts',(20.2198981641729,16.7748272460081,-15.8122483986571));
#120350=CARTESIAN_POINT('Ctrl Pts',(17.4898527405687,16.642940686348,-15.9394242053385));
#120351=CARTESIAN_POINT('Ctrl Pts',(15.9012352070049,18.8670891552265,-16.0666000120199));
#120352=CARTESIAN_POINT('Ctrl Pts',(16.9115035498021,21.4067544786704,-16.1937758187014));
#120353=CARTESIAN_POINT('Ctrl Pts',(19.5937992687688,21.931951351827,-16.3209516253828));
#120354=CARTESIAN_POINT('Ctrl Pts',(21.4872825238012,19.9608442409695,-16.4481274320642));
#120355=CARTESIAN_POINT('Ctrl Pts',(20.854799951232,17.3018015796049,-16.5753032387457));
#120356=CARTESIAN_POINT('Ctrl Pts',(18.2766150550976,16.3943299707347,-16.7024790454271));
#120357=CARTESIAN_POINT('Ctrl Pts',(16.1180524573998,18.0709782914572,-16.8296548521085));
#120358=CARTESIAN_POINT('Ctrl Pts',(16.3594593660219,20.7935257720403,-16.9568306587899));
#120359=CARTESIAN_POINT('Ctrl Pts',(18.7793599257057,22.0642040794035,-17.0840064654714));
#120360=CARTESIAN_POINT('Ctrl Pts',(21.1576455689089,20.717244733731,-17.2111822721528));
#120361=CARTESIAN_POINT('Ctrl Pts',(21.3123868310473,17.9883993329521,-17.3383580788343));
#120362=CARTESIAN_POINT('Ctrl Pts',(19.1016182084348,16.3812141610339,-17.4655338855157));
#120363=CARTESIAN_POINT('Ctrl Pts',(16.5535826965425,17.3701818600505,-17.5927096921971));
#120364=CARTESIAN_POINT('Ctrl Pts',(16.0059447286121,20.0479859484101,-17.7198854988786));
#120365=CARTESIAN_POINT('Ctrl Pts',(17.9611281499736,21.9579073783129,-17.84706130556));
#120366=CARTESIAN_POINT('Ctrl Pts',(20.6253735238976,21.3477117809083,-17.9742371122414));
#120367=CARTESIAN_POINT('Ctrl Pts',(21.5544010815252,18.7772157438201,-18.1014129189229));
#120368=CARTESIAN_POINT('Ctrl Pts',(19.8958857006878,16.6046898380703,-18.2285887256043));
#120369=CARTESIAN_POINT('Ctrl Pts',(17.1714123042272,16.8232917400757,-18.3557645322858));
#120370=CARTESIAN_POINT('Ctrl Pts',(15.8805161335109,19.2324677726021,-18.4829403389672));
#120371=CARTESIAN_POINT('Ctrl Pts',(17.2075143031097,21.6219484563437,-18.6101161456486));
#120372=CARTESIAN_POINT('Ctrl Pts',(19.9349683552291,21.7995335714625,-18.7372919523301));
#120373=CARTESIAN_POINT('Ctrl Pts',(21.5606084819066,19.6022997977881,-18.8644677590115));
#120374=CARTESIAN_POINT('Ctrl Pts',(20.5930107655851,17.0460727454631,-18.9916435656929));
#120375=CARTESIAN_POINT('Ctrl Pts',(17.919886054979,16.4760320805331,-19.1188193723744));
#120376=CARTESIAN_POINT('Ctrl Pts',(15.9936603594759,18.4151547268051,-19.2459951790558));
#120377=CARTESIAN_POINT('Ctrl Pts',(16.5815261991922,21.0844160225493,-19.3731709857372));
#120378=CARTESIAN_POINT('Ctrl Pts',(19.1441531541393,22.0349343813413,-19.5003467924186));
#120379=CARTESIAN_POINT('Ctrl Pts',(21.3304900460201,20.3946682445481,-19.6275225991001));
#120380=CARTESIAN_POINT('Ctrl Pts',(21.1347084791815,17.6684599097052,-19.7546984057815));
#120381=CARTESIAN_POINT('Ctrl Pts',(18.7364258833105,16.3574364640233,-19.8818742124629));
#120382=CARTESIAN_POINT('Ctrl Pts',(16.3359176980786,17.6643802632539,-20.0090500191444));
#120383=CARTESIAN_POINT('Ctrl Pts',(16.1355011676512,20.3902520376885,-20.1362258258258));
#120384=CARTESIAN_POINT('Ctrl Pts',(18.3190460646205,22.0342325649128,-20.2634016325072));
#120385=CARTESIAN_POINT('Ctrl Pts',(20.8832853850366,21.0880737832455,-20.3905774391887));
#120386=CARTESIAN_POINT('Ctrl Pts',(21.4756888748341,18.4198137277981,-20.5177532458701));
#120387=CARTESIAN_POINT('Ctrl Pts',(19.5527627775141,16.4774229462598,-20.6449290525516));
#120388=CARTESIAN_POINT('Ctrl Pts',(16.8786730601742,17.0429098579489,-20.772104859233));
#120389=CARTESIAN_POINT('Ctrl Pts',(15.9067298650559,19.5975033862937,-20.8992806659144));
#120390=CARTESIAN_POINT('Ctrl Pts',(17.5286330619216,21.7974684377538,-21.0264564725959));
#120391=CARTESIAN_POINT('Ctrl Pts',(20.2563826753269,21.6245778537434,-21.1536322792773));
#120392=CARTESIAN_POINT('Ctrl Pts',(21.5874463311991,19.2372471517761,-21.2808080859587));
#120393=CARTESIAN_POINT('Ctrl Pts',(20.300639179667,16.8260911603011,-21.4079838926401));
#120394=CARTESIAN_POINT('Ctrl Pts',(17.5765588401915,16.6024498642088,-21.5351596993216));
#120395=CARTESIAN_POINT('Ctrl Pts',(15.9143183086354,18.7729382233993,-21.662335506003));
#120396=CARTESIAN_POINT('Ctrl Pts',(16.8390399827,21.3434932755793,-21.7895113126845));
#120397=CARTESIAN_POINT('Ctrl Pts',(19.5021077373455,21.9611708420245,-21.9166871193659));
#120398=CARTESIAN_POINT('Ctrl Pts',(21.4611725520066,20.0483226159722,-22.0438815838219));
#120399=CARTESIAN_POINT('Ctrl Pts',(21.097729963592,18.2714051422367,-22.1286841127175));
#120400=CARTESIAN_POINT('Ctrl Pts',(20.5799309194189,17.6565535467265,-22.1710947060526));
#120401=CARTESIAN_POINT('Ctrl Pts',(18.1489776472236,17.0246983287242,0.17134583652952));
#120402=CARTESIAN_POINT('Ctrl Pts',(17.4210583805961,17.2194788787227,0.128953900969042));
#120403=CARTESIAN_POINT('Ctrl Pts',(16.1877700772709,18.3901108027545,0.0441700298480857));
#120404=CARTESIAN_POINT('Ctrl Pts',(16.6662106099602,20.9125930681132,-0.0830057768333481));
#120405=CARTESIAN_POINT('Ctrl Pts',(19.0452436430351,21.8682695891329,-0.210181583514783));
#120406=CARTESIAN_POINT('Ctrl Pts',(21.1369461627689,20.3888844472776,-0.337357390196217));
#120407=CARTESIAN_POINT('Ctrl Pts',(21.0250156242086,17.8274157338044,-0.464533196877652));
#120408=CARTESIAN_POINT('Ctrl Pts',(18.8107430744499,16.5360493895473,-0.591709003559086));
#120409=CARTESIAN_POINT('Ctrl Pts',(16.5263111813342,17.6983953463737,-0.71888481024052));
#120410=CARTESIAN_POINT('Ctrl Pts',(16.2671682429258,20.2486639579588,-0.846060616921954));
#120411=CARTESIAN_POINT('Ctrl Pts',(18.271257019252,21.8468355936962,-0.97323642360339));
#120412=CARTESIAN_POINT('Ctrl Pts',(20.6998491546166,21.0268460006587,-1.10041223028482));
#120413=CARTESIAN_POINT('Ctrl Pts',(21.3249146619818,18.5409022133311,-1.22758803696626));
#120414=CARTESIAN_POINT('Ctrl Pts',(19.5729674590718,16.669746184055,-1.35476384364769));
#120415=CARTESIAN_POINT('Ctrl Pts',(17.0513245200395,17.1300252112755,-1.48193965032912));
#120416=CARTESIAN_POINT('Ctrl Pts',(16.0734293860861,19.4994733867219,-1.60911545701056));
#120417=CARTESIAN_POINT('Ctrl Pts',(17.5364439588135,21.6042630902867,-1.73629126369199));
#120418=CARTESIAN_POINT('Ctrl Pts',(20.0981411949616,21.5133835119668,-1.86346707037343));
#120419=CARTESIAN_POINT('Ctrl Pts',(21.4083239034943,19.3102094129899,-1.99064287705486));
#120420=CARTESIAN_POINT('Ctrl Pts',(20.2649802358942,17.0160171208712,-2.1178186837363));
#120421=CARTESIAN_POINT('Ctrl Pts',(17.7170573196222,16.7355852361245,-2.24499449041773));
#120422=CARTESIAN_POINT('Ctrl Pts',(16.1021161450239,18.7261928325832,-2.37217029709916));
#120423=CARTESIAN_POINT('Ctrl Pts',(16.9017650796541,21.1615808747066,-2.4993461037806));
#120424=CARTESIAN_POINT('Ctrl Pts',(19.3823758191848,21.8074320517016,-2.62652191046204));
#120425=CARTESIAN_POINT('Ctrl Pts',(21.2681419942009,20.0712179632603,-2.75369771714347));
#120426=CARTESIAN_POINT('Ctrl Pts',(20.8289901725761,17.5458072902532,-2.8808735238249));
#120427=CARTESIAN_POINT('Ctrl Pts',(18.4678148992109,16.5481075720289,-3.00804933050634));
#120428=CARTESIAN_POINT('Ctrl Pts',(16.3508479335524,17.9934463802261,-3.13522513718777));
#120429=CARTESIAN_POINT('Ctrl Pts',(16.420275074257,20.5558150638861,-3.26240094386921));
#120430=CARTESIAN_POINT('Ctrl Pts',(18.6124012281085,21.8843993954715,-3.38957675055063));
#120431=CARTESIAN_POINT('Ctrl Pts',(20.9160867080332,20.7603057113818,-3.51675255723208));
#120432=CARTESIAN_POINT('Ctrl Pts',(21.2178430688434,18.2148201979656,-3.64392836391351));
#120433=CARTESIAN_POINT('Ctrl Pts',(19.2408275787131,16.5832678229678,-3.77110417059494));
#120434=CARTESIAN_POINT('Ctrl Pts',(16.7988292423621,17.3624966249737,-3.89827997727638));
#120435=CARTESIAN_POINT('Ctrl Pts',(16.1322299659104,19.8376125424924,-4.02545578395781));
#120436=CARTESIAN_POINT('Ctrl Pts',(17.8525932116705,21.7378503442427,-4.15263159063924));
#120437=CARTESIAN_POINT('Ctrl Pts',(20.3815924794505,21.3198597891662,-4.27980739732068));
#120438=CARTESIAN_POINT('Ctrl Pts',(21.3990279084555,18.9671212681321,-4.40698320400211));
#120439=CARTESIAN_POINT('Ctrl Pts',(19.97146564174,16.8381263467644,-4.53415901068355));
#120440=CARTESIAN_POINT('Ctrl Pts',(17.4086054545075,16.8860957250923,-4.66133481736498));
#120441=CARTESIAN_POINT('Ctrl Pts',(16.0617124995014,19.0670204758143,-4.78851062404641));
#120442=CARTESIAN_POINT('Ctrl Pts',(17.1664774653348,21.3800375035998,-4.91568643072785));
#120443=CARTESIAN_POINT('Ctrl Pts',(19.7093470653026,21.7030972474828,-5.04286223740928));
#120444=CARTESIAN_POINT('Ctrl Pts',(21.3573962697213,19.7398124437998,-5.17003804409073));
#120445=CARTESIAN_POINT('Ctrl Pts',(20.5986422230066,17.2913750447324,-5.29721385077215));
#120446=CARTESIAN_POINT('Ctrl Pts',(18.1291946694319,16.6040743967613,-5.42438965745359));
#120447=CARTESIAN_POINT('Ctrl Pts',(16.214618468201,18.3084661857105,-5.55156546413503));
#120448=CARTESIAN_POINT('Ctrl Pts',(16.6114184519424,20.8408767317044,-5.67874127081646));
#120449=CARTESIAN_POINT('Ctrl Pts',(18.9555552637581,21.8779765379183,-5.80591707749789));
#120450=CARTESIAN_POINT('Ctrl Pts',(21.0964288723461,20.4682909018246,-5.93309288417933));
#120451=CARTESIAN_POINT('Ctrl Pts',(21.069920619429,17.905118899581,-6.06026869086075));
#120452=CARTESIAN_POINT('Ctrl Pts',(18.9003501817706,16.5400117548499,-6.1874444975422));
#120453=CARTESIAN_POINT('Ctrl Pts',(16.5781637771942,17.6253705448169,-6.31462030422363));
#120454=CARTESIAN_POINT('Ctrl Pts',(16.2338233007557,20.1654459446513,-6.44179611090507));
#120455=CARTESIAN_POINT('Ctrl Pts',(18.1832397674068,21.8298764298645,-6.5689719175865));
#120456=CARTESIAN_POINT('Ctrl Pts',(20.637944563427,21.09165033648,-6.69614772426794));
#120457=CARTESIAN_POINT('Ctrl Pts',(21.3458983946297,18.6280442856993,-6.82332353094937));
#120458=CARTESIAN_POINT('Ctrl Pts',(19.657597561457,16.6992639204773,-6.9504993376308));
#120459=CARTESIAN_POINT('Ctrl Pts',(17.1219532905771,17.0748455122945,-7.07767514431223));
#120460=CARTESIAN_POINT('Ctrl Pts',(16.0652618206899,19.4102162618813,-7.20485095099367));
#120461=CARTESIAN_POINT('Ctrl Pts',(17.4569719897474,21.5628184559476,-7.3320267576751));
#120462=CARTESIAN_POINT('Ctrl Pts',(20.0202760969144,21.5577731869978,-7.45920256435654));
#120463=CARTESIAN_POINT('Ctrl Pts',(21.4035017204607,19.3997091761485,-7.58637837103798));
#120464=CARTESIAN_POINT('Ctrl Pts',(20.3376252034471,17.0685162087954,-7.7135541777194));
#120465=CARTESIAN_POINT('Ctrl Pts',(17.8005220944761,16.7029191423313,-7.84072998440084));
#120466=CARTESIAN_POINT('Ctrl Pts',(16.1198270256501,18.638330593724,-7.96790579108227));
#120467=CARTESIAN_POINT('Ctrl Pts',(16.8374734069165,21.099130681503,-8.09508159776372));
#120468=CARTESIAN_POINT('Ctrl Pts',(19.2950652256212,21.8276880596097,-8.22225740444514));
#120469=CARTESIAN_POINT('Ctrl Pts',(21.2379145234536,20.155596553002,-8.34943321112658));
#120470=CARTESIAN_POINT('Ctrl Pts',(20.8835776564797,17.616896337289,-8.47660901780802));
#120471=CARTESIAN_POINT('Ctrl Pts',(18.5571367075217,16.5406872908817,-8.60378482448944));
#120472=CARTESIAN_POINT('Ctrl Pts',(16.3929568520385,17.9143244167918,-8.73096063117089));
#120473=CARTESIAN_POINT('Ctrl Pts',(16.3765387832853,20.4775809095322,-8.85813643785231));
#120474=CARTESIAN_POINT('Ctrl Pts',(18.5229450603227,21.878828030654,-8.98531224453375));
#120475=CARTESIAN_POINT('Ctrl Pts',(20.8629811449671,20.8325085177327,-9.11248805121519));
#120476=CARTESIAN_POINT('Ctrl Pts',(21.2498091685766,18.2985555819606,-9.23966385789662));
#120477=CARTESIAN_POINT('Ctrl Pts',(19.3285384287442,16.6017137670521,-9.36683966457805));
#120478=CARTESIAN_POINT('Ctrl Pts',(16.8618155817557,17.2987301203051,-9.49401547125949));
#120479=CARTESIAN_POINT('Ctrl Pts',(16.1127057376362,19.7501353993238,-9.62119127794092));
#120480=CARTESIAN_POINT('Ctrl Pts',(17.7684706833649,21.7069174119797,-9.74836708462235));
#120481=CARTESIAN_POINT('Ctrl Pts',(20.3100488495983,21.3738501132499,-9.87554289130379));
#120482=CARTESIAN_POINT('Ctrl Pts',(21.405700016949,19.0565020772309,-10.0027186979853));
#120483=CARTESIAN_POINT('Ctrl Pts',(20.0502322431535,16.8808962961301,-10.1298945046666));
#120484=CARTESIAN_POINT('Ctrl Pts',(17.487203080851,16.8430160407836,-10.2570703113481));
#120485=CARTESIAN_POINT('Ctrl Pts',(16.0680327069235,18.9776140943582,-10.3842461180296));
#120486=CARTESIAN_POINT('Ctrl Pts',(17.0947218558021,21.3263292307962,-10.511421924711));
#120487=CARTESIAN_POINT('Ctrl Pts',(19.6253469569058,21.7343610901177,-10.6385977313924));
#120488=CARTESIAN_POINT('Ctrl Pts',(21.3382165482799,19.8273657667087,-10.7657735380739));
#120489=CARTESIAN_POINT('Ctrl Pts',(20.6618790925152,17.3548931083184,-10.8929493447553));
#120490=CARTESIAN_POINT('Ctrl Pts',(18.2168322270393,16.5852833200598,-11.0201251514367));
#120491=CARTESIAN_POINT('Ctrl Pts',(16.2462546942025,18.2246056152896,-11.1473009581181));
#120492=CARTESIAN_POINT('Ctrl Pts',(16.5580290725475,20.768883535951,-11.2744767647995));
#120493=CARTESIAN_POINT('Ctrl Pts',(18.8661217208428,21.8839000055346,-11.401652571481));
#120494=CARTESIAN_POINT('Ctrl Pts',(21.0530008906637,20.5466966189245,-11.5288283781625));
#120495=CARTESIAN_POINT('Ctrl Pts',(21.1123406767285,17.984074487133,-11.6560041848439));
#120496=CARTESIAN_POINT('Ctrl Pts',(18.9897005083654,16.5470803618114,-11.7831799915254));
#120497=CARTESIAN_POINT('Ctrl Pts',(16.6324709941403,17.554067163028,-11.9103557982068));
#120498=CARTESIAN_POINT('Ctrl Pts',(16.2032639071911,20.0811870013163,-12.0375316048882));
#120499=CARTESIAN_POINT('Ctrl Pts',(18.0958501101972,21.8099642757934,-12.1647074115696));
#120500=CARTESIAN_POINT('Ctrl Pts',(20.5738992290484,21.1543531371454,-12.291883218251));
#120501=CARTESIAN_POINT('Ctrl Pts',(21.3639550022726,18.7158361132654,-12.4190590249325));
#120502=CARTESIAN_POINT('Ctrl Pts',(19.7411902943285,16.7316012221275,-12.546234831614));
#120503=CARTESIAN_POINT('Ctrl Pts',(17.1943910046178,17.0220608208441,-12.6734106382954));
#120504=CARTESIAN_POINT('Ctrl Pts',(16.0600874092589,19.3207362555485,-12.8005864449768));
#120505=CARTESIAN_POINT('Ctrl Pts',(17.3789326541725,21.5187354867873,-12.9277622516583));
#120506=CARTESIAN_POINT('Ctrl Pts',(19.940968083918,21.5995306431169,-13.0549380583397));
#120507=CARTESIAN_POINT('Ctrl Pts',(21.3956852095567,19.4889971833178,-13.1821138650211));
#120508=CARTESIAN_POINT('Ctrl Pts',(20.4084713582425,17.1234185622757,-13.3092896717026));
#120509=CARTESIAN_POINT('Ctrl Pts',(17.8850339651544,16.6730663404289,-13.436465478384));
#120510=CARTESIAN_POINT('Ctrl Pts',(16.1404702162623,18.5511107293104,-13.5636412850654));
#120511=CARTESIAN_POINT('Ctrl Pts',(16.7753090713368,21.0345625667023,-13.6908170917469));
#120512=CARTESIAN_POINT('Ctrl Pts',(19.2071252833902,21.8450089322025,-13.8179928984283));
#120513=CARTESIAN_POINT('Ctrl Pts',(21.2048784133999,20.2389155874388,-13.9451687051096));
#120514=CARTESIAN_POINT('Ctrl Pts',(20.9357539591253,17.6897734908367,-14.0723445117912));
#120515=CARTESIAN_POINT('Ctrl Pts',(18.6466569036158,16.5362622984264,-14.1995203184726));
#120516=CARTESIAN_POINT('Ctrl Pts',(16.4376917179148,17.8366569342653,-14.326696125154));
#120517=CARTESIAN_POINT('Ctrl Pts',(16.3354468560612,20.3979260315651,-14.4538719318355));
#120518=CARTESIAN_POINT('Ctrl Pts',(18.4337256327737,21.8702641638416,-14.5810477385169));
#120519=CARTESIAN_POINT('Ctrl Pts',(20.8074875042872,20.9028924783419,-14.7082235451983));
#120520=CARTESIAN_POINT('Ctrl Pts',(21.2789532857658,18.3833144546537,-14.8353993518798));
#120521=CARTESIAN_POINT('Ctrl Pts',(19.4155823851695,16.6230865468621,-14.9625751585612));
#120522=CARTESIAN_POINT('Ctrl Pts',(16.9269019499539,17.2371086083006,-15.0897509652427));
#120523=CARTESIAN_POINT('Ctrl Pts',(16.0961218145012,19.6620535081066,-15.2169267719241));
#120524=CARTESIAN_POINT('Ctrl Pts',(17.6854311890587,21.6731848097627,-15.3441025786055));
#120525=CARTESIAN_POINT('Ctrl Pts',(20.2367373661345,21.425414368886,-15.4712783852869));
#120526=CARTESIAN_POINT('Ctrl Pts',(21.4093752801818,19.1460561866125,-15.5984541919684));
#120527=CARTESIAN_POINT('Ctrl Pts',(20.1275224271794,16.9262799222545,-15.7256299986498));
#120528=CARTESIAN_POINT('Ctrl Pts',(17.5671992389961,16.8025925235073,-15.8528058053313));
#120529=CARTESIAN_POINT('Ctrl Pts',(16.0773433292112,18.8884695018156,-15.9799816120127));
#120530=CARTESIAN_POINT('Ctrl Pts',(17.0248050241658,21.2702481937078,-16.1071574186941));
#120531=CARTESIAN_POINT('Ctrl Pts',(19.5403470248439,21.7627944792304,-16.2343332253756));
#120532=CARTESIAN_POINT('Ctrl Pts',(21.3161156777683,19.9142277122867,-16.361509032057));
#120533=CARTESIAN_POINT('Ctrl Pts',(20.7229534605137,17.4204931665544,-16.4886848387384));
#120534=CARTESIAN_POINT('Ctrl Pts',(18.3050498916118,16.5694375091209,-16.6158606454198));
#120535=CARTESIAN_POINT('Ctrl Pts',(16.2806814235098,18.1418514832104,-16.7430364521013));
#120536=CARTESIAN_POINT('Ctrl Pts',(16.5070804792137,20.6951428626135,-16.8702122587827));
#120537=CARTESIAN_POINT('Ctrl Pts',(18.7765399770255,21.8868252818636,-16.9973880654642));
#120538=CARTESIAN_POINT('Ctrl Pts',(21.0069716862451,20.6236040854512,-17.1245638721456));
#120539=CARTESIAN_POINT('Ctrl Pts',(21.1520929498682,18.0644063167351,-17.251739678827));
#120540=CARTESIAN_POINT('Ctrl Pts',(19.0787640157619,16.5571370867842,-17.3789154855085));
#120541=CARTESIAN_POINT('Ctrl Pts',(16.6891354956622,17.4846223624005,-17.5060912921899));
#120542=CARTESIAN_POINT('Ctrl Pts',(16.1755432396875,19.9959519694325,-17.6332670988714));
#120543=CARTESIAN_POINT('Ctrl Pts',(18.0091762655641,21.7871368641264,-17.7604429055528));
#120544=CARTESIAN_POINT('Ctrl Pts',(20.5077900801511,21.2148760790659,-17.8876187122342));
#120545=CARTESIAN_POINT('Ctrl Pts',(21.3790615900277,18.8041833660481,-18.0147945189156));
#120546=CARTESIAN_POINT('Ctrl Pts',(19.8236532620919,16.7667196647752,-18.1419703255971));
#120547=CARTESIAN_POINT('Ctrl Pts',(17.2685556976942,16.9717314619586,-18.2691461322785));
#120548=CARTESIAN_POINT('Ctrl Pts',(16.0579123249335,19.231133158048,-18.3963219389599));
#120549=CARTESIAN_POINT('Ctrl Pts',(17.3024132973075,21.4720639313621,-18.5234977456414));
#120550=CARTESIAN_POINT('Ctrl Pts',(19.8603062151207,21.6386088848577,-18.6506735523228));
#120551=CARTESIAN_POINT('Ctrl Pts',(21.3848830869879,19.5779733613755,-18.7778493590042));
#120552=CARTESIAN_POINT('Ctrl Pts',(20.4774392589433,17.1806625548439,-18.9050251656857));
#120553=CARTESIAN_POINT('Ctrl Pts',(17.9704981207863,16.6460603390679,-19.0322009723671));
#120554=CARTESIAN_POINT('Ctrl Pts',(16.1640225686834,18.4646310606594,-19.1593767790485));
#120555=CARTESIAN_POINT('Ctrl Pts',(16.7153417987421,20.9679489658214,-19.28655258573));
#120556=CARTESIAN_POINT('Ctrl Pts',(19.1186546369411,21.8593752306623,-19.4137283924114));
#120557=CARTESIAN_POINT('Ctrl Pts',(21.1690707190565,20.3210816226097,-19.5409041990928));
#120558=CARTESIAN_POINT('Ctrl Pts',(20.985460555994,17.7643569779692,-19.6680800057743));
#120559=CARTESIAN_POINT('Ctrl Pts',(18.7362750703113,16.5348376083611,-19.7952558124557));
#120560=CARTESIAN_POINT('Ctrl Pts',(16.485002356336,17.7605309561315,-19.9224316191372));
#120561=CARTESIAN_POINT('Ctrl Pts',(16.2970453774111,20.3169399637462,-20.0496074258186));
#120562=CARTESIAN_POINT('Ctrl Pts',(18.3448430381436,21.8587170449558,-20.1767832325));
#120563=CARTESIAN_POINT('Ctrl Pts',(20.7496680038194,20.9713793298171,-20.3039590391814));
#120564=CARTESIAN_POINT('Ctrl Pts',(21.3052427860467,18.4690004195621,-20.4311348458629));
#120565=CARTESIAN_POINT('Ctrl Pts',(19.5018617017747,16.6473647370611,-20.5583106525443));
#120566=CARTESIAN_POINT('Ctrl Pts',(16.9940155496951,17.1776962986144,-20.6854864592258));
#120567=CARTESIAN_POINT('Ctrl Pts',(16.0824963938076,19.5734751345466,-20.8126622659072));
#120568=CARTESIAN_POINT('Ctrl Pts',(17.6035686543715,21.6366721369649,-20.9398380725886));
#120569=CARTESIAN_POINT('Ctrl Pts',(20.1617387589333,21.4745298636412,-21.0670138792701));
#120570=CARTESIAN_POINT('Ctrl Pts',(21.4100524732811,19.2356154114268,-21.1941896859515));
#120571=CARTESIAN_POINT('Ctrl Pts',(20.2032439124044,16.9743568470362,-21.3213654926329));
#120572=CARTESIAN_POINT('Ctrl Pts',(17.6485149693138,16.7646189462416,-21.4485412993143));
#120573=CARTESIAN_POINT('Ctrl Pts',(16.0896130768821,18.8001717717257,-21.5757171059958));
#120574=CARTESIAN_POINT('Ctrl Pts',(16.9568463925819,21.2109198309685,-21.7028929126772));
#120575=CARTESIAN_POINT('Ctrl Pts',(19.4543557984586,21.7901974439036,-21.8300687193587));
#120576=CARTESIAN_POINT('Ctrl Pts',(21.2916289180791,19.9962677069502,-21.9572631838147));
#120577=CARTESIAN_POINT('Ctrl Pts',(20.950780931212,18.329818140889,-22.0420657127103));
#120578=CARTESIAN_POINT('Ctrl Pts',(20.46517256435,17.753190813129,-22.0844763060453));
#120579=CARTESIAN_POINT('Ctrl Pts',(18.1877584159729,17.169626909876,0.257964236536772));
#120580=CARTESIAN_POINT('Ctrl Pts',(17.5080924658439,17.3514955780797,0.215572300976294));
#120581=CARTESIAN_POINT('Ctrl Pts',(16.3565580788699,18.4445270382643,0.130788429855338));
#120582=CARTESIAN_POINT('Ctrl Pts',(16.8032830855277,20.7997955194952,0.00361262317390322));
#120583=CARTESIAN_POINT('Ctrl Pts',(19.0246114950703,21.6921208369499,-0.123563183507531));
#120584=CARTESIAN_POINT('Ctrl Pts',(20.9776563527076,20.3108032181647,-0.250738990188965));
#120585=CARTESIAN_POINT('Ctrl Pts',(20.8731456200936,17.9191326762732,-0.3779147968704));
#120586=CARTESIAN_POINT('Ctrl Pts',(18.8056558236651,16.7133702056622,-0.505090603551834));
#120587=CARTESIAN_POINT('Ctrl Pts',(16.6726575032154,17.7986649702659,-0.632266410233268));
#120588=CARTESIAN_POINT('Ctrl Pts',(16.4306929893915,20.1798778580737,-0.759442216914702));
#120589=CARTESIAN_POINT('Ctrl Pts',(18.301931964306,21.6721076877706,-0.886618023596137));
#120590=CARTESIAN_POINT('Ctrl Pts',(20.5695342339997,20.9064746960381,-1.01379383027757));
#120591=CARTESIAN_POINT('Ctrl Pts',(21.1531645367453,18.5853225798024,-1.140969636959));
#120592=CARTESIAN_POINT('Ctrl Pts',(19.5173528268034,16.8382043226231,-1.26814544364043));
#120593=CARTESIAN_POINT('Ctrl Pts',(17.1628680334775,17.2679717387401,-1.39532125032187));
#120594=CARTESIAN_POINT('Ctrl Pts',(16.2497969611534,19.4803506649187,-1.5224970570033));
#120595=CARTESIAN_POINT('Ctrl Pts',(17.6158292056801,21.4456151650917,-1.64967286368474));
#120596=CARTESIAN_POINT('Ctrl Pts',(20.0077131216202,21.3607599376264,-1.77684867036617));
#120597=CARTESIAN_POINT('Ctrl Pts',(21.2310446313948,19.3036328825639,-1.90402447704761));
#120598=CARTESIAN_POINT('Ctrl Pts',(20.1634925060559,17.1615211739047,-2.03120028372904));
#120599=CARTESIAN_POINT('Ctrl Pts',(17.7844698188743,16.8996789447851,-2.15837609041048));
#120600=CARTESIAN_POINT('Ctrl Pts',(16.2765820926419,18.7583303988802,-2.28555189709191));
#120601=CARTESIAN_POINT('Ctrl Pts',(17.0232227955911,21.0322780788906,-2.41272770377335));
#120602=CARTESIAN_POINT('Ctrl Pts',(19.3393953884592,21.6353161821242,-2.53990351045478));
#120603=CARTESIAN_POINT('Ctrl Pts',(21.1001552938832,20.0141946482555,-2.66707931713621));
#120604=CARTESIAN_POINT('Ctrl Pts',(20.6901145740129,17.6561918817021,-2.79425512381765));
#120605=CARTESIAN_POINT('Ctrl Pts',(18.4854601443698,16.7246290587094,-2.92143093049908));
#120606=CARTESIAN_POINT('Ctrl Pts',(16.5088256052511,18.0741572541683,-3.04860673718052));
#120607=CARTESIAN_POINT('Ctrl Pts',(16.5736504638791,20.4666681077815,-3.17578254386197));
#120608=CARTESIAN_POINT('Ctrl Pts',(18.6204619352431,21.7071814084352,-3.30295835054339));
#120609=CARTESIAN_POINT('Ctrl Pts',(20.7714375341794,20.6576031971447,-3.43013415722482));
#120610=CARTESIAN_POINT('Ctrl Pts',(21.0531906530764,18.2808563388961,-3.55730996390625));
#120611=CARTESIAN_POINT('Ctrl Pts',(19.2072302930153,16.7574585584311,-3.6844857705877));
#120612=CARTESIAN_POINT('Ctrl Pts',(16.9271105110797,17.4850327666767,-3.81166157726912));
#120613=CARTESIAN_POINT('Ctrl Pts',(16.3046996870279,19.7960747858742,-3.93883738395056));
#120614=CARTESIAN_POINT('Ctrl Pts',(17.911021120741,21.5703470028761,-4.066013190632));
#120615=CARTESIAN_POINT('Ctrl Pts',(20.2723745963467,21.1800647823256,-4.19318899731344));
#120616=CARTESIAN_POINT('Ctrl Pts',(21.2223648620988,18.9832878379367,-4.32036480399487));
#120617=CARTESIAN_POINT('Ctrl Pts',(19.8894348122174,16.9954226688293,-4.44754061067631));
#120618=CARTESIAN_POINT('Ctrl Pts',(17.4964650364985,17.0402121868336,-4.57471641735773));
#120619=CARTESIAN_POINT('Ctrl Pts',(16.23885677971,19.0765647891309,-4.70189222403917));
#120620=CARTESIAN_POINT('Ctrl Pts',(17.2703875614835,21.2362533534106,-4.8290680307206));
#120621=CARTESIAN_POINT('Ctrl Pts',(19.6446919135629,21.5378976673356,-4.95624383740204));
#120622=CARTESIAN_POINT('Ctrl Pts',(21.1834929588632,19.7047577950374,-5.08341964408348));
#120623=CARTESIAN_POINT('Ctrl Pts',(20.4750362470855,17.4186257918574,-5.21059545076491));
#120624=CARTESIAN_POINT('Ctrl Pts',(18.1692868395033,16.7768858773585,-5.33777125744635));
#120625=CARTESIAN_POINT('Ctrl Pts',(16.3816267066251,18.3682945922223,-5.46494706412778));
#120626=CARTESIAN_POINT('Ctrl Pts',(16.7521230656655,20.7328332145257,-5.59212287080921));
#120627=CARTESIAN_POINT('Ctrl Pts',(18.9408685028023,21.7011843181237,-5.71929867749065));
#120628=CARTESIAN_POINT('Ctrl Pts',(20.9398249283253,20.3849458681128,-5.84647448417208));
#120629=CARTESIAN_POINT('Ctrl Pts',(20.9150738910453,17.9916849474066,-5.97365029085351));
#120630=CARTESIAN_POINT('Ctrl Pts',(18.889322931444,16.7170699082275,-6.10082609753496));
#120631=CARTESIAN_POINT('Ctrl Pts',(16.7210728226713,17.7304809374911,-6.22800190421637));
#120632=CARTESIAN_POINT('Ctrl Pts',(16.3995584627467,20.1021763152302,-6.35517771089783));
#120633=CARTESIAN_POINT('Ctrl Pts',(18.2197493214694,21.6562727363857,-6.48235351757925));
#120634=CARTESIAN_POINT('Ctrl Pts',(20.5117332597471,20.96698319265,-6.6095293242607));
#120635=CARTESIAN_POINT('Ctrl Pts',(21.1727572707768,18.6666880582664,-6.73670513094212));
#120636=CARTESIAN_POINT('Ctrl Pts',(19.5963728522159,16.8657653466142,-6.86388093762356));
#120637=CARTESIAN_POINT('Ctrl Pts',(17.2288148666425,17.2164498677646,-6.99105674430498));
#120638=CARTESIAN_POINT('Ctrl Pts',(16.2421708185993,19.3970103394982,-7.11823255098643));
#120639=CARTESIAN_POINT('Ctrl Pts',(17.5416253841297,21.406917869846,-7.24540835766785));
#120640=CARTESIAN_POINT('Ctrl Pts',(19.935009652606,21.4022070486441,-7.3725841643493));
#120641=CARTESIAN_POINT('Ctrl Pts',(21.2265421078823,19.3871997619589,-7.49975997103072));
#120642=CARTESIAN_POINT('Ctrl Pts',(20.2313218837872,17.210540129867,-7.62693577771217));
#120643=CARTESIAN_POINT('Ctrl Pts',(17.8624017655944,16.8691782660797,-7.75411158439359));
#120644=CARTESIAN_POINT('Ctrl Pts',(16.2931189299813,18.676292493315,-7.88128739107503));
#120645=CARTESIAN_POINT('Ctrl Pts',(16.9631929779452,20.9739676702432,-8.00846319775646));
#120646=CARTESIAN_POINT('Ctrl Pts',(19.2578725599652,21.6542294318373,-8.13563900443789));
#120647=CARTESIAN_POINT('Ctrl Pts',(21.0719315834152,20.0929798336416,-8.26281481111933));
#120648=CARTESIAN_POINT('Ctrl Pts',(20.7410834874809,17.7225684799219,-8.38999061780077));
#120649=CARTESIAN_POINT('Ctrl Pts',(18.5688608654335,16.7177006633949,-8.5171664244822));
#120650=CARTESIAN_POINT('Ctrl Pts',(16.5481431496601,18.0002802365935,-8.64434223116363));
#120651=CARTESIAN_POINT('Ctrl Pts',(16.5328134244968,20.3936200469742,-8.77151803784506));
#120652=CARTESIAN_POINT('Ctrl Pts',(18.5369357613108,21.7019793659344,-8.89869384452652));
#120653=CARTESIAN_POINT('Ctrl Pts',(20.721852305936,20.7250197242656,-9.02586965120793));
#120654=CARTESIAN_POINT('Ctrl Pts',(21.0830377398936,18.3590409562453,-9.15304545788938));
#120655=CARTESIAN_POINT('Ctrl Pts',(19.2891268452239,16.774681732328,-9.2802212645708));
#120656=CARTESIAN_POINT('Ctrl Pts',(16.985921525119,17.4254933040343,-9.40739707125225));
#120657=CARTESIAN_POINT('Ctrl Pts',(16.2864697077309,19.7143964482452,-9.53457287793367));
#120658=CARTESIAN_POINT('Ctrl Pts',(17.8324750226373,21.5414645954985,-9.66174868461511));
#120659=CARTESIAN_POINT('Ctrl Pts',(20.2055735493235,21.2304761213276,-9.78892449129655));
#120660=CARTESIAN_POINT('Ctrl Pts',(21.2285946806605,19.0667436486627,-9.91610029797797));
#120661=CARTESIAN_POINT('Ctrl Pts',(19.9629800244992,17.0353574247909,-10.0432761046594));
#120662=CARTESIAN_POINT('Ctrl Pts',(17.5698524749629,16.999988228066,-10.1704519113408));
#120663=CARTESIAN_POINT('Ctrl Pts',(16.2447580245038,18.9930851012233,-10.2976277180222));
#120664=CARTESIAN_POINT('Ctrl Pts',(17.2033885867812,21.1861053686842,-10.4248035247037));
#120665=CARTESIAN_POINT('Ctrl Pts',(19.5662601202284,21.567089049242,-10.5519793313851));
#120666=CARTESIAN_POINT('Ctrl Pts',(21.1655846492548,19.786507262499,-10.6791551380666));
#120667=CARTESIAN_POINT('Ctrl Pts',(20.534081183754,17.4779332824223,-10.806330944748));
#120668=CARTESIAN_POINT('Ctrl Pts',(18.2511149577974,16.7593404494715,-10.9335067514294));
#120669=CARTESIAN_POINT('Ctrl Pts',(16.4111657868359,18.2899930869776,-11.0606825581108));
#120670=CARTESIAN_POINT('Ctrl Pts',(16.7022728351016,20.6656124030459,-11.1878583647923));
#120671=CARTESIAN_POINT('Ctrl Pts',(18.8573634539519,21.7067151227473,-11.3150341714737));
#120672=CARTESIAN_POINT('Ctrl Pts',(20.8992757606008,20.4581541188783,-11.4422099781552));
#120673=CARTESIAN_POINT('Ctrl Pts',(20.9546819490687,18.065406618053,-11.5693857848366));
#120674=CARTESIAN_POINT('Ctrl Pts',(18.9727502803322,16.7236699416198,-11.696561591518));
#120675=CARTESIAN_POINT('Ctrl Pts',(16.7717800479045,17.663904212636,-11.8237373981994));
#120676=CARTESIAN_POINT('Ctrl Pts',(16.371024832419,20.0235028449647,-11.9509132048809));
#120677=CARTESIAN_POINT('Ctrl Pts',(18.1381526704095,21.6376805466522,-12.0780890115623));
#120678=CARTESIAN_POINT('Ctrl Pts',(20.4519334508432,21.0255294635675,-12.2052648182438));
#120679=CARTESIAN_POINT('Ctrl Pts',(21.1896169171035,18.7486602200595,-12.3324406249252));
#120680=CARTESIAN_POINT('Ctrl Pts',(19.6744242746961,16.8959590286039,-12.4596164316066));
#120681=CARTESIAN_POINT('Ctrl Pts',(17.2964507295683,17.1671642407565,-12.5867922382881));
#120682=CARTESIAN_POINT('Ctrl Pts',(16.2373394156912,19.3134619072614,-12.7139680449695));
#120683=CARTESIAN_POINT('Ctrl Pts',(17.4687592276853,21.365757133357,-12.8411438516509));
#120684=CARTESIAN_POINT('Ctrl Pts',(19.8609589185792,21.4411964289083,-12.9683196583324));
#120685=CARTESIAN_POINT('Ctrl Pts',(21.2192437486358,19.4705689225376,-13.0954954650138));
#120686=CARTESIAN_POINT('Ctrl Pts',(20.2974716909424,17.2618030404029,-13.2226712716952));
#120687=CARTESIAN_POINT('Ctrl Pts',(17.9413113968065,16.8413043878911,-13.3498470783767));
#120688=CARTESIAN_POINT('Ctrl Pts',(16.3123936962972,18.5948543795921,-13.4770228850581));
#120689=CARTESIAN_POINT('Ctrl Pts',(16.9051494775971,20.9136797357071,-13.6041986917395));
#120690=CARTESIAN_POINT('Ctrl Pts',(19.1757621019364,21.6704021145338,-13.731374498421));
#120691=CARTESIAN_POINT('Ctrl Pts',(21.0410854165974,20.1707757009864,-13.8585503051024));
#120692=CARTESIAN_POINT('Ctrl Pts',(20.7898010554004,17.7906146521824,-13.9857261117838));
#120693=CARTESIAN_POINT('Ctrl Pts',(18.6524468232773,16.7135690009438,-14.1129019184653));
#120694=CARTESIAN_POINT('Ctrl Pts',(16.5899125690362,17.9277612832899,-14.2400777251467));
#120695=CARTESIAN_POINT('Ctrl Pts',(16.4944454556301,20.3192454414403,-14.3672535318281));
#120696=CARTESIAN_POINT('Ctrl Pts',(18.4536306342518,21.6939831925389,-14.4944293385096));
#120697=CARTESIAN_POINT('Ctrl Pts',(20.6700373042621,20.7907379758005,-14.621605145191));
#120698=CARTESIAN_POINT('Ctrl Pts',(21.1102499116389,18.438181215862,-14.7487809518724));
#120699=CARTESIAN_POINT('Ctrl Pts',(19.37040071179,16.7946377238266,-14.8759567585539));
#120700=CARTESIAN_POINT('Ctrl Pts',(17.0466933583566,17.3679566438234,-15.0031325652353));
#120701=CARTESIAN_POINT('Ctrl Pts',(16.27098512257,19.6321534509405,-15.1303083719167));
#120702=CARTESIAN_POINT('Ctrl Pts',(17.7549401648813,21.5099681065509,-15.2574841785982));
#120703=CARTESIAN_POINT('Ctrl Pts',(20.1371218386074,21.278622214454,-15.3846599852796));
#120704=CARTESIAN_POINT('Ctrl Pts',(21.2320263129741,19.1503612717033,-15.5118357919611));
#120705=CARTESIAN_POINT('Ctrl Pts',(20.0351466901858,17.0777325985008,-15.6390115986425));
#120706=CARTESIAN_POINT('Ctrl Pts',(17.6445457374235,16.9622443606664,-15.7661874053239));
#120707=CARTESIAN_POINT('Ctrl Pts',(16.2534514514175,18.9098498484046,-15.8933632120053));
#120708=CARTESIAN_POINT('Ctrl Pts',(17.1381064985295,21.1337419087451,-16.0205390186868));
#120709=CARTESIAN_POINT('Ctrl Pts',(19.4868947809189,21.5936376066338,-16.1477148253682));
#120710=CARTESIAN_POINT('Ctrl Pts',(21.1449488317356,19.8676111836039,-16.2748906320497));
#120711=CARTESIAN_POINT('Ctrl Pts',(20.5911069697954,17.5391847535037,-16.4020664387311));
#120712=CARTESIAN_POINT('Ctrl Pts',(18.3334847281261,16.7445450475071,-16.5292422454125));
#120713=CARTESIAN_POINT('Ctrl Pts',(16.4433103896197,18.2127246749636,-16.656418052094));
#120714=CARTESIAN_POINT('Ctrl Pts',(16.6547015924054,20.5967599531865,-16.7835938587754));
#120715=CARTESIAN_POINT('Ctrl Pts',(18.7737200283452,21.7094464843237,-16.9107696654568));
#120716=CARTESIAN_POINT('Ctrl Pts',(20.8562978035812,20.5299634371713,-17.0379454721383));
#120717=CARTESIAN_POINT('Ctrl Pts',(20.9917990686889,18.140413300518,-17.1651212788197));
#120718=CARTESIAN_POINT('Ctrl Pts',(19.0559098230889,16.7330600125345,-17.2922970855011));
#120719=CARTESIAN_POINT('Ctrl Pts',(16.8246882947818,17.5990628647505,-17.4194728921826));
#120720=CARTESIAN_POINT('Ctrl Pts',(16.3451417507631,19.9439179904547,-17.546648698864));
#120721=CARTESIAN_POINT('Ctrl Pts',(18.0572243811545,21.6163663499399,-17.6738245055454));
#120722=CARTESIAN_POINT('Ctrl Pts',(20.3902066364046,21.0820403772236,-17.8010003122269));
#120723=CARTESIAN_POINT('Ctrl Pts',(21.2037220985302,18.8311509882762,-17.9281761189083));
#120724=CARTESIAN_POINT('Ctrl Pts',(19.7514208234961,16.92874949148,-18.0553519255897));
#120725=CARTESIAN_POINT('Ctrl Pts',(17.3656990911611,17.1201711838414,-18.1825277322712));
#120726=CARTESIAN_POINT('Ctrl Pts',(16.2353085163561,19.229798543494,-18.3097035389526));
#120727=CARTESIAN_POINT('Ctrl Pts',(17.3973122915052,21.3221794063805,-18.4368793456341));
#120728=CARTESIAN_POINT('Ctrl Pts',(19.7856440750124,21.4776841982527,-18.5640551523154));
#120729=CARTESIAN_POINT('Ctrl Pts',(21.2091576920692,19.5536469249632,-18.6912309589969));
#120730=CARTESIAN_POINT('Ctrl Pts',(20.3618677523014,17.3152523642247,-18.8184067656783));
#120731=CARTESIAN_POINT('Ctrl Pts',(18.0211101865936,16.8160885976028,-18.9455825723598));
#120732=CARTESIAN_POINT('Ctrl Pts',(16.3343847778911,18.5141073945138,-19.0727583790412));
#120733=CARTESIAN_POINT('Ctrl Pts',(16.849157398292,20.8514819090936,-19.1999341857227));
#120734=CARTESIAN_POINT('Ctrl Pts',(19.093156119743,21.6838160799832,-19.327109992404));
#120735=CARTESIAN_POINT('Ctrl Pts',(21.0076513920927,20.2474950006713,-19.4542857990855));
#120736=CARTESIAN_POINT('Ctrl Pts',(20.8362126328065,17.8602540462332,-19.5814616057669));
#120737=CARTESIAN_POINT('Ctrl Pts',(18.7361242573121,16.7122387526989,-19.7086374124484));
#120738=CARTESIAN_POINT('Ctrl Pts',(16.6340870145935,17.8566816490089,-19.8358132191298));
#120739=CARTESIAN_POINT('Ctrl Pts',(16.4585895871711,20.243627889804,-19.9629890258113));
#120740=CARTESIAN_POINT('Ctrl Pts',(18.3706400116666,21.6832015249988,-20.0901648324927));
#120741=CARTESIAN_POINT('Ctrl Pts',(20.6160506226023,20.8546848763886,-20.2173406391741));
#120742=CARTESIAN_POINT('Ctrl Pts',(21.1347966972592,18.518187111326,-20.3445164458556));
#120743=CARTESIAN_POINT('Ctrl Pts',(19.4509606260352,16.8173065278623,-20.471692252537));
#120744=CARTESIAN_POINT('Ctrl Pts',(17.1093580392161,17.31248273928,-20.5988680592184));
#120745=CARTESIAN_POINT('Ctrl Pts',(16.2582629225594,19.5494468827994,-20.7260438658998));
#120746=CARTESIAN_POINT('Ctrl Pts',(17.6785042468215,21.475875836176,-20.8532196725813));
#120747=CARTESIAN_POINT('Ctrl Pts',(20.0670948425395,21.324481873539,-20.9803954792627));
#120748=CARTESIAN_POINT('Ctrl Pts',(21.2326586153631,19.2339836710777,-21.1075712859442));
#120749=CARTESIAN_POINT('Ctrl Pts',(20.1058486451417,17.1226225337713,-21.2347470926256));
#120750=CARTESIAN_POINT('Ctrl Pts',(17.7204710984363,16.9267880282744,-21.361922899307));
#120751=CARTESIAN_POINT('Ctrl Pts',(16.2649078451288,18.8274053200522,-21.4890987059885));
#120752=CARTESIAN_POINT('Ctrl Pts',(17.0746528024638,21.0783463863576,-21.6162745126699));
#120753=CARTESIAN_POINT('Ctrl Pts',(19.4066038595716,21.6192240457828,-21.7434503193513));
#120754=CARTESIAN_POINT('Ctrl Pts',(21.1220852841517,19.9442127979284,-21.8706447838074));
#120755=CARTESIAN_POINT('Ctrl Pts',(20.803831898832,18.3882311395412,-21.955447312703));
#120756=CARTESIAN_POINT('Ctrl Pts',(20.3504142092811,17.8498280795315,-21.997857906038));
#120757=CARTESIAN_POINT('Ctrl Pts',(18.0722627314315,16.7380050975816,1.38691141904346E-15));
#120758=CARTESIAN_POINT('Ctrl Pts',(17.9906109534297,16.7675693131061,-3.14694538653141E-14));
#120759=CARTESIAN_POINT('Ctrl Pts',(17.9108508876399,16.801533969706,6.86855221048143E-15));
#120760=CARTESIAN_POINT('Ctrl Pts',(17.833184560489,16.8395812357413,8.79504802320241E-16));
#120761=CARTESIAN_POINT('Ctrl Pts',(17.753672918112,16.8785324868355,-5.25183954169529E-15));
#120762=CARTESIAN_POINT('Ctrl Pts',(17.6763549684803,16.9217633043122,-1.85298947912786E-14));
#120763=CARTESIAN_POINT('Ctrl Pts',(17.601476924462,16.9689790985631,-1.06130382260261E-14));
#120764=CARTESIAN_POINT('Ctrl Pts',(17.5314114952683,17.0131602057527,-3.20501948859016E-15));
#120765=CARTESIAN_POINT('Ctrl Pts',(17.463482274071,17.0608314720442,1.11820055827351E-14));
#120766=CARTESIAN_POINT('Ctrl Pts',(17.3979218193959,17.1117790406503,1.23651089367627E-14));
#120767=CARTESIAN_POINT('Ctrl Pts',(17.3682534093495,17.1348346061396,1.26760648409614E-14));
#120768=CARTESIAN_POINT('Ctrl Pts',(17.3390705414607,17.1585614233309,2.36784452741916E-14));
#120769=CARTESIAN_POINT('Ctrl Pts',(17.310397157226,17.1829409553506,2.57155408078802E-14));
#120770=CARTESIAN_POINT('Ctrl Pts',(17.2926919353297,17.1979948122865,2.73538097927482E-14));
#120771=CARTESIAN_POINT('Ctrl Pts',(17.27518100039,17.2132975506653,1.30324840963727E-14));
#120772=CARTESIAN_POINT('Ctrl Pts',(17.257870302469,17.2288449191993,-8.4446338810551E-15));
#120773=CARTESIAN_POINT('Ctrl Pts',(17.2457082697189,17.239768083947,-2.37561771158851E-14));
#120774=CARTESIAN_POINT('Ctrl Pts',(17.2336433007629,17.2508137998582,-1.24432143521951E-14));
#120775=CARTESIAN_POINT('Ctrl Pts',(17.2216943574194,17.2619645032884,-7.15399961492835E-15));
#120776=CARTESIAN_POINT('Ctrl Pts',(17.1582625823413,17.3211587677193,2.03808243867262E-14));
#120777=CARTESIAN_POINT('Ctrl Pts',(17.0979931462804,17.3834003799274,6.45801759227035E-15));
#120778=CARTESIAN_POINT('Ctrl Pts',(17.041116608508,17.4484111431913,9.57567358739198E-15));
#120779=CARTESIAN_POINT('Ctrl Pts',(16.984962464847,17.5125961988015,1.26537319484047E-14));
#120780=CARTESIAN_POINT('Ctrl Pts',(16.9321151284108,17.5794813469685,1.14065042207504E-14));
#120781=CARTESIAN_POINT('Ctrl Pts',(16.8828390026402,17.6488249957258,1.34753319613878E-14));
#120782=CARTESIAN_POINT('Ctrl Pts',(16.8374017786391,17.7127663639311,1.53829857795583E-14));
#120783=CARTESIAN_POINT('Ctrl Pts',(16.7950011366565,17.7787988087843,-4.98584307276175E-15));
#120784=CARTESIAN_POINT('Ctrl Pts',(16.7558820673411,17.8467441370846,6.63358257213531E-15));
#120785=CARTESIAN_POINT('Ctrl Pts',(16.7395100185488,17.8751805045547,1.13870112004006E-14));
#120786=CARTESIAN_POINT('Ctrl Pts',(16.723713229623,17.903952012734,-1.077566553237E-15));
#120787=CARTESIAN_POINT('Ctrl Pts',(16.7085117731593,17.9330458325382,3.69149155687865E-15));
#120788=CARTESIAN_POINT('Ctrl Pts',(16.6986550833365,17.9519103905663,6.75998993358336E-15));
#120789=CARTESIAN_POINT('Ctrl Pts',(16.6890487140929,17.9709104592438,1.73723425931104E-14));
#120790=CARTESIAN_POINT('Ctrl Pts',(16.6796984374459,17.9900425446149,6.0507154842071E-15));
#120791=CARTESIAN_POINT('Ctrl Pts',(16.6737724856049,18.0021679416281,-6.19111889800206E-16));
#120792=CARTESIAN_POINT('Ctrl Pts',(16.6679532270762,18.0143385914813,2.13664567833998E-16));
#120793=CARTESIAN_POINT('Ctrl Pts',(16.6622433304787,18.0265499321002,2.5951463200613E-15));
#120794=CARTESIAN_POINT('Ctrl Pts',(16.6271177976284,18.1016703548131,1.76314342966372E-14));
#120795=CARTESIAN_POINT('Ctrl Pts',(16.5961057017263,18.1783725156421,-1.14329481650844E-14));
#120796=CARTESIAN_POINT('Ctrl Pts',(16.5694538401814,18.2564278430498,4.39925873507718E-15));
#120797=CARTESIAN_POINT('Ctrl Pts',(16.5428019786364,18.3344831704575,2.02314656352387E-14));
#120798=CARTESIAN_POINT('Ctrl Pts',(16.5205098793409,18.4138923942319,1.04011446651248E-14));
#120799=CARTESIAN_POINT('Ctrl Pts',(16.5028786483266,18.4944362051925,9.4091401336982E-15));
#120800=CARTESIAN_POINT('Ctrl Pts',(16.4850464602744,18.5758980374565,8.67831743648321E-15));
#120801=CARTESIAN_POINT('Ctrl Pts',(16.4719827280125,18.6585216956155,-2.53066140108434E-14));
#120802=CARTESIAN_POINT('Ctrl Pts',(16.4636117053936,18.7419152200439,-1.91235915991683E-14));
#120803=CARTESIAN_POINT('Ctrl Pts',(16.4601585345833,18.7763162839797,-1.6573003280011E-14));
#120804=CARTESIAN_POINT('Ctrl Pts',(16.4575045102803,18.8108481987005,-1.23100883047652E-14));
#120805=CARTESIAN_POINT('Ctrl Pts',(16.4556467292437,18.845482524778,-3.85802501057242E-15));
#120806=CARTESIAN_POINT('Ctrl Pts',(16.454914769638,18.859128335107,-7.53928088074055E-16));
#120807=CARTESIAN_POINT('Ctrl Pts',(16.4543064277075,18.8727920340357,-1.66414205223653E-14));
#120808=CARTESIAN_POINT('Ctrl Pts',(16.4538219965805,18.8864542247022,-1.65978342181461E-14));
#120809=CARTESIAN_POINT('Ctrl Pts',(16.4509322011605,18.9679538101119,-1.63169175235896E-14));
#120810=CARTESIAN_POINT('Ctrl Pts',(16.4524389841394,19.0495303086149,1.17186656710794E-14));
#120811=CARTESIAN_POINT('Ctrl Pts',(16.458209072107,19.1308246613079,1.11577413974828E-14));
#120812=CARTESIAN_POINT('Ctrl Pts',(16.4640075078908,19.212518404336,1.05940613637857E-14));
#120813=CARTESIAN_POINT('Ctrl Pts',(16.4741116098931,19.2939282562688,-2.01713604129673E-16));
#120814=CARTESIAN_POINT('Ctrl Pts',(16.4884373885337,19.3746780989613,-9.38138455808257E-15));
#120815=CARTESIAN_POINT('Ctrl Pts',(16.5025242207667,19.4540810770041,-1.84079434576874E-14));
#120816=CARTESIAN_POINT('Ctrl Pts',(16.5206935647272,19.5328467548947,8.94254489680765E-15));
#120817=CARTESIAN_POINT('Ctrl Pts',(16.5429083611757,19.6105921329322,6.30051566474776E-15));
#120818=CARTESIAN_POINT('Ctrl Pts',(16.5522119867773,19.6431521382056,5.19402563408715E-15));
#120819=CARTESIAN_POINT('Ctrl Pts',(16.5622256486948,19.6755328027596,3.88113245870864E-15));
#120820=CARTESIAN_POINT('Ctrl Pts',(16.5729486044555,19.7077040845634,4.66293670342566E-15));
#120821=CARTESIAN_POINT('Ctrl Pts',(16.5784892728338,19.7243273373082,5.05407298290637E-15));
#120822=CARTESIAN_POINT('Ctrl Pts',(16.5842201982241,19.7408967187103,-7.47574057736949E-15));
#120823=CARTESIAN_POINT('Ctrl Pts',(16.59013339505,19.757386717525,-3.5527136788005E-15));
#120824=CARTESIAN_POINT('Ctrl Pts',(16.6171691937068,19.8327808403536,1.42878117443501E-14));
#120825=CARTESIAN_POINT('Ctrl Pts',(16.6480432448069,19.9066161661436,5.97421475994626E-15));
#120826=CARTESIAN_POINT('Ctrl Pts',(16.6826949054327,19.9785209088995,-4.21884749357559E-15));
#120827=CARTESIAN_POINT('Ctrl Pts',(16.708683650902,20.0324494659664,-1.17360773291967E-14));
#120828=CARTESIAN_POINT('Ctrl Pts',(16.7367982565916,20.085291634914,2.01726906480219E-14));
#120829=CARTESIAN_POINT('Ctrl Pts',(16.7670276708943,20.1368764988564,7.7715611723761E-15));
#120830=CARTESIAN_POINT('Ctrl Pts',(16.776261941294,20.1526342828943,4.25330862624586E-15));
#120831=CARTESIAN_POINT('Ctrl Pts',(16.7856936339531,20.1682746431805,-1.0466123746905E-14));
#120832=CARTESIAN_POINT('Ctrl Pts',(16.7953226427023,20.1837924294014,-1.16573417585641E-15));
#120833=CARTESIAN_POINT('Ctrl Pts',(16.803547563051,20.1970474340419,6.67029465765244E-15));
#120834=CARTESIAN_POINT('Ctrl Pts',(16.8119141832479,20.2102092393014,-2.4083441391153E-14));
#120835=CARTESIAN_POINT('Ctrl Pts',(16.8204178931759,20.2232683327282,-1.87627691161651E-14));
#120836=CARTESIAN_POINT('Ctrl Pts',(16.8615694216389,20.2864644741072,6.85731831263342E-15));
#120837=CARTESIAN_POINT('Ctrl Pts',(16.9059580723631,20.3473056667748,2.60350180919675E-15));
#120838=CARTESIAN_POINT('Ctrl Pts',(16.9535504700224,20.4054521814502,-5.32907051820075E-15));
#120839=CARTESIAN_POINT('Ctrl Pts',(16.997682676699,20.459371171234,-1.13595455771569E-14));
#120840=CARTESIAN_POINT('Ctrl Pts',(17.0445702571952,20.51097318916,-3.05225759359301E-14));
#120841=CARTESIAN_POINT('Ctrl Pts',(17.0942091691994,20.55995417271,-1.27675647831893E-14));
#120842=CARTESIAN_POINT('Ctrl Pts',(17.0997977295932,20.5654686607127,-1.06144939056098E-14));
#120843=CARTESIAN_POINT('Ctrl Pts',(17.1054211843278,20.5709498884042,-1.65578075338009E-15));
#120844=CARTESIAN_POINT('Ctrl Pts',(17.1110791648801,20.5763977067475,-3.95239396766556E-14));
#120845=CARTESIAN_POINT('Ctrl Pts',(20.3504145393176,-17.5908279157877,
-0.0021418925797119));
#120846=CARTESIAN_POINT('Ctrl Pts',(20.8038322616566,-18.1292310654914,
-0.0445524841607392));
#120847=CARTESIAN_POINT('Ctrl Pts',(21.1220877448274,-19.685210814566,-0.129355011302244));
#120848=CARTESIAN_POINT('Ctrl Pts',(19.4066026967562,-21.3602255324577,
-0.256549474004229));
#120849=CARTESIAN_POINT('Ctrl Pts',(17.0746532893504,-20.819345744412,-0.383725280685663));
#120850=CARTESIAN_POINT('Ctrl Pts',(16.264907281043,-18.5684058059804,-0.510901087367098));
#120851=CARTESIAN_POINT('Ctrl Pts',(17.7204711810805,-16.6677874925037,
-0.638076894048532));
#120852=CARTESIAN_POINT('Ctrl Pts',(20.105848679288,-16.8636225373773,-0.765252700729966));
#120853=CARTESIAN_POINT('Ctrl Pts',(21.2326588952387,-18.9749835563125,
-0.8924285074114));
#120854=CARTESIAN_POINT('Ctrl Pts',(20.0670949402048,-21.0654821373604,
-1.01960431409284));
#120855=CARTESIAN_POINT('Ctrl Pts',(17.678504162672,-21.2168760062151,-1.14678012077427));
#120856=CARTESIAN_POINT('Ctrl Pts',(16.2582626864848,-19.2904469366441,
-1.2739559274557));
#120857=CARTESIAN_POINT('Ctrl Pts',(17.1093578926688,-17.0534825509078,
-1.40113173413714));
#120858=CARTESIAN_POINT('Ctrl Pts',(19.4509606903938,-16.5583063136444,
-1.52830754081857));
#120859=CARTESIAN_POINT('Ctrl Pts',(21.1347969203461,-18.2591870432273,
-1.65548334750001));
#120860=CARTESIAN_POINT('Ctrl Pts',(20.6160507961411,-20.5956850306546,
-1.78265915418144));
#120861=CARTESIAN_POINT('Ctrl Pts',(18.3706399783415,-21.4242017524251,
-1.90983496086288));
#120862=CARTESIAN_POINT('Ctrl Pts',(16.4585893765603,-19.9846279859987,
-2.03701076754431));
#120863=CARTESIAN_POINT('Ctrl Pts',(16.6340868204421,-17.5976815233674,
-2.16418657422575));
#120864=CARTESIAN_POINT('Ctrl Pts',(18.7361242574674,-16.453238521784,-2.29136238090717));
#120865=CARTESIAN_POINT('Ctrl Pts',(20.8362128272701,-17.6012539211848,
-2.41853818758862));
#120866=CARTESIAN_POINT('Ctrl Pts',(21.0076516023807,-19.9884950966021,
-2.54571399427004));
#120867=CARTESIAN_POINT('Ctrl Pts',(19.0931561529689,-21.4248163086708,
-2.67288980095148));
#120868=CARTESIAN_POINT('Ctrl Pts',(16.8491572239522,-20.5924820608467,
-2.80006560763291));
#120869=CARTESIAN_POINT('Ctrl Pts',(16.3343845559425,-18.2551073300457,
-2.92724141431435));
#120870=CARTESIAN_POINT('Ctrl Pts',(18.0211101206545,-16.557088376093,-3.05441722099578));
#120871=CARTESIAN_POINT('Ctrl Pts',(20.3618679028699,-17.0562521888763,
-3.18159302767722));
#120872=CARTESIAN_POINT('Ctrl Pts',(21.2091579210064,-19.2946469566574,
-3.30876883435865));
#120873=CARTESIAN_POINT('Ctrl Pts',(19.7856441722836,-21.2186844079067,
-3.43594464104009));
#120874=CARTESIAN_POINT('Ctrl Pts',(17.3973121678696,-21.0631796016525,
-3.56312044772152));
#120875=CARTESIAN_POINT('Ctrl Pts',(16.2353082852419,-18.9707985452326,
-3.69029625440296));
#120876=CARTESIAN_POINT('Ctrl Pts',(17.3656989646013,-16.8611709904523,
-3.81747206108439));
#120877=CARTESIAN_POINT('Ctrl Pts',(19.7514209176014,-16.6697492803852,
-3.94464786776582));
#120878=CARTESIAN_POINT('Ctrl Pts',(21.2037223269647,-18.5721509531424,
-4.07182367444726));
#120879=CARTESIAN_POINT('Ctrl Pts',(20.390206789594,-20.8230405502836,-4.19899948112869));
#120880=CARTESIAN_POINT('Ctrl Pts',(18.0572243185569,-21.357366572422,-4.32617528781012));
#120881=CARTESIAN_POINT('Ctrl Pts',(16.3451415298078,-19.6849180582454,
-4.45335109449157));
#120882=CARTESIAN_POINT('Ctrl Pts',(16.8246881181817,-17.340062715656,-4.58052690117299));
#120883=CARTESIAN_POINT('Ctrl Pts',(19.0559098528636,-16.4740597833398,
-4.70770270785444));
#120884=CARTESIAN_POINT('Ctrl Pts',(20.9917992775219,-17.8814132014949,
-4.83487851453586));
#120885=CARTESIAN_POINT('Ctrl Pts',(20.8562979998813,-20.2709635591674,
-4.9620543212173));
#120886=CARTESIAN_POINT('Ctrl Pts',(18.7737200320192,-21.4504467154151,
-5.08923012789874));
#120887=CARTESIAN_POINT('Ctrl Pts',(16.6547014000827,-20.3377600813612,
-5.21640593458017));
#120888=CARTESIAN_POINT('Ctrl Pts',(16.4433101777445,-17.9537245826292,
-5.34358174126161));
#120889=CARTESIAN_POINT('Ctrl Pts',(18.3334846910807,-16.4855448193747,
-5.47075754794303));
#120890=CARTESIAN_POINT('Ctrl Pts',(20.5911071415668,-17.2801845988705,
-5.59793335462448));
#120891=CARTESIAN_POINT('Ctrl Pts',(21.144949054734,-19.6086112443364,-5.7251091613059));
#120892=CARTESIAN_POINT('Ctrl Pts',(19.4868948505574,-21.3346378270135,
-5.85228496798734));
#120893=CARTESIAN_POINT('Ctrl Pts',(17.1381063509189,-20.8747420865874,
-5.97946077466877));
#120894=CARTESIAN_POINT('Ctrl Pts',(16.2534512219814,-18.6508498205501,
-6.10663658135021));
#120895=CARTESIAN_POINT('Ctrl Pts',(17.6445456366553,-16.7032441526699,
-6.23381238803165));
#120896=CARTESIAN_POINT('Ctrl Pts',(20.0351468105341,-16.8187324011862,
-6.36098819471307));
#120897=CARTESIAN_POINT('Ctrl Pts',(21.2320265440266,-18.8913612660945,
-6.48816400139451));
#120898=CARTESIAN_POINT('Ctrl Pts',(20.137121968388,-21.0196224056966,-6.61533980807595));
#120899=CARTESIAN_POINT('Ctrl Pts',(17.7549400743241,-21.2509683191918,
-6.74251561475738));
#120900=CARTESIAN_POINT('Ctrl Pts',(16.2709848947557,-19.3731534898947,
-6.86969142143882));
#120901=CARTESIAN_POINT('Ctrl Pts',(17.0466932022907,-17.1089564733528,
-6.99686722812024));
#120902=CARTESIAN_POINT('Ctrl Pts',(19.3704007706532,-16.5356375003274,
-7.12404303480169));
#120903=CARTESIAN_POINT('Ctrl Pts',(21.1102501314279,-18.1791811443807,
-7.25121884148312));
#120904=CARTESIAN_POINT('Ctrl Pts',(20.6700374833341,-20.5317381219169,
-7.37839464816456));
#120905=CARTESIAN_POINT('Ctrl Pts',(18.4536306083194,-21.4349834222001,
-7.50557045484598));
#120906=CARTESIAN_POINT('Ctrl Pts',(16.4944452484846,-20.0602455439464,
-7.63274626152742));
#120907=CARTESIAN_POINT('Ctrl Pts',(16.5899123707208,-17.668761164598,-7.75992206820886));
#120908=CARTESIAN_POINT('Ctrl Pts',(18.6524468157339,-16.4545687699462,
-7.88709787489029));
#120909=CARTESIAN_POINT('Ctrl Pts',(20.7898012455497,-17.531614520805,-8.01427368157173));
#120910=CARTESIAN_POINT('Ctrl Pts',(21.0410856299891,-19.9117757897599,
-8.14144948825315));
#120911=CARTESIAN_POINT('Ctrl Pts',(19.175762142797,-21.4114023420139,-8.2686252949346));
#120912=CARTESIAN_POINT('Ctrl Pts',(16.9051493084394,-20.6546798931949,
-8.39580110161602));
#120913=CARTESIAN_POINT('Ctrl Pts',(16.312393472313,-18.3358543226023,-8.52297690829747));
#120914=CARTESIAN_POINT('Ctrl Pts',(17.9413113234874,-16.5823041687085,
-8.65015271497889));
#120915=CARTESIAN_POINT('Ctrl Pts',(20.2974718355542,-17.0028028601137,
-8.77732852166034));
#120916=CARTESIAN_POINT('Ctrl Pts',(21.2192439785061,-19.211568946546,-8.90450432834176));
#120917=CARTESIAN_POINT('Ctrl Pts',(19.8609590228163,-21.1821966351882,
-9.0316801350232));
#120918=CARTESIAN_POINT('Ctrl Pts',(17.4687591106581,-21.1067573326593,
-9.15885594170464));
#120919=CARTESIAN_POINT('Ctrl Pts',(16.2373391847649,-19.0544619167386,
-9.28603174838607));
#120920=CARTESIAN_POINT('Ctrl Pts',(17.2964505966034,-16.908164051714,-9.4132075550675));
#120921=CARTESIAN_POINT('Ctrl Pts',(19.6744243616797,-16.6369588144763,
-9.54038336174894));
#120922=CARTESIAN_POINT('Ctrl Pts',(21.1896171442334,-18.4896601772957,
-9.66755916843036));
#120923=CARTESIAN_POINT('Ctrl Pts',(20.4519336097419,-20.7665296314006,
-9.79473497511181));
#120924=CARTESIAN_POINT('Ctrl Pts',(18.1381526152972,-21.3786807711059,
-9.92191078179324));
#120925=CARTESIAN_POINT('Ctrl Pts',(16.3710246138578,-19.7645029201165,
-10.0490865884747));
#120926=CARTESIAN_POINT('Ctrl Pts',(16.7717798664108,-17.4049040695389,
-10.1762623951561));
#120927=CARTESIAN_POINT('Ctrl Pts',(18.9727503024152,-16.4646697115565,
-10.3034382018376));
#120928=CARTESIAN_POINT('Ctrl Pts',(20.9546821544686,-17.8064065120923,
-10.430614008519));
#120929=CARTESIAN_POINT('Ctrl Pts',(20.8992759608759,-20.1991542342326,
-10.5577898152005));
#120930=CARTESIAN_POINT('Ctrl Pts',(18.8573634653625,-21.4477153535862,
-10.6849656218819));
#120931=CARTESIAN_POINT('Ctrl Pts',(16.702272647179,-20.4066125375889,-10.8121414285633));
#120932=CARTESIAN_POINT('Ctrl Pts',(16.4111655719875,-18.0309930017901,
-10.9393172352448));
#120933=CARTESIAN_POINT('Ctrl Pts',(18.2511149131333,-16.5003402227076,
-11.0664930419262));
#120934=CARTESIAN_POINT('Ctrl Pts',(20.5340813502507,-17.2189331221239,
-11.1936688486076));
#120935=CARTESIAN_POINT('Ctrl Pts',(21.165584874162,-19.5275073157298,-11.3208446552891));
#120936=CARTESIAN_POINT('Ctrl Pts',(19.5662601972076,-21.3080892671662,
-11.4480204619705));
#120937=CARTESIAN_POINT('Ctrl Pts',(17.2033884452088,-20.9271055513698,
-11.575196268652));
#120938=CARTESIAN_POINT('Ctrl Pts',(16.2447577942637,-18.7340850810675,
-11.7023720753333));
#120939=CARTESIAN_POINT('Ctrl Pts',(17.5698523672862,-16.7409880235606,
-11.8295478820148));
#120940=CARTESIAN_POINT('Ctrl Pts',(19.9629801381724,-16.7763572235568,
-11.9567236886962));
#120941=CARTESIAN_POINT('Ctrl Pts',(21.2285949113957,-18.8077436353198,
-12.0838994953777));
#120942=CARTESIAN_POINT('Ctrl Pts',(20.2055736854352,-20.9714763081171,
-12.2110753020591));
#120943=CARTESIAN_POINT('Ctrl Pts',(17.8324749392518,-21.2824648110527,
-12.3382511087405));
#120944=CARTESIAN_POINT('Ctrl Pts',(16.2864694813489,-19.4553964948066,
-12.465426915422));
#120945=CARTESIAN_POINT('Ctrl Pts',(16.985921363432,-17.1664931388855,-12.5926027221034));
#120946=CARTESIAN_POINT('Ctrl Pts',(19.2891268965698,-16.515681506983,-12.7197785287849));
#120947=CARTESIAN_POINT('Ctrl Pts',(21.0830379571657,-18.100040877444,-12.8469543354662));
#120948=CARTESIAN_POINT('Ctrl Pts',(20.7218524898006,-20.4660198643034,
-12.9741301421477));
#120949=CARTESIAN_POINT('Ctrl Pts',(18.5369357430837,-21.4429795963352,
-13.1013059488291));
#120950=CARTESIAN_POINT('Ctrl Pts',(16.5328132209002,-20.1346201563596,
-13.2284817555106));
#120951=CARTESIAN_POINT('Ctrl Pts',(16.5481429474813,-17.7412801246093,
-13.355657562192));
#120952=CARTESIAN_POINT('Ctrl Pts',(18.5688608501589,-16.4587004327796,
-13.4828333688734));
#120953=CARTESIAN_POINT('Ctrl Pts',(20.7410836731242,-17.4635683422508,
-13.6100091755549));
#120954=CARTESIAN_POINT('Ctrl Pts',(21.0719317996599,-19.8339799152194,
-13.7371849822363));
#120955=CARTESIAN_POINT('Ctrl Pts',(19.2578726084204,-21.3952296578215,
-13.8643607889177));
#120956=CARTESIAN_POINT('Ctrl Pts',(16.9631928141561,-20.7149678333072,
-13.9915365955992));
#120957=CARTESIAN_POINT('Ctrl Pts',(16.2931187042143,-18.4172924438578,
-14.1187124022806));
#120958=CARTESIAN_POINT('Ctrl Pts',(17.8624016849767,-16.6101780494751,
-14.245888208962));
#120959=CARTESIAN_POINT('Ctrl Pts',(20.2313220222805,-16.9515399448363,
-14.3730640156435));
#120960=CARTESIAN_POINT('Ctrl Pts',(21.2265423384276,-19.1281997782562,
-14.5002398223249));
#120961=CARTESIAN_POINT('Ctrl Pts',(19.9350097636923,-21.1432072513177,
-14.6274156290064));
#120962=CARTESIAN_POINT('Ctrl Pts',(17.5416252738421,-21.1479180729553,
-14.7545914356878));
#120963=CARTESIAN_POINT('Ctrl Pts',(16.2421705881198,-19.1380103567032,
-14.8817672423692));
#120964=CARTESIAN_POINT('Ctrl Pts',(17.2288147274218,-16.9574496832805,
-15.0089430490507));
#120965=CARTESIAN_POINT('Ctrl Pts',(19.5963729319801,-16.6067651296939,
-15.1361188557321));
#120966=CARTESIAN_POINT('Ctrl Pts',(21.1727574963474,-18.4076880079206,
-15.2632946624135));
#120967=CARTESIAN_POINT('Ctrl Pts',(20.511733424177,-20.707983355068,-15.3904704690949));
#120968=CARTESIAN_POINT('Ctrl Pts',(18.2197492739044,-21.397272962559,-15.5176462757764));
#120969=CARTESIAN_POINT('Ctrl Pts',(16.3995582468247,-19.8431763976587,
-15.6448220824578));
#120970=CARTESIAN_POINT('Ctrl Pts',(16.7210726364874,-17.471480800552,-15.7719978891392));
#120971=CARTESIAN_POINT('Ctrl Pts',(18.8893229458104,-16.4580696775538,
-15.8991736958207));
#120972=CARTESIAN_POINT('Ctrl Pts',(20.9150740927816,-17.732684834627,-16.0263495025021));
#120973=CARTESIAN_POINT('Ctrl Pts',(20.939825132351,-20.1259459766957,-16.1535253091836));
#120974=CARTESIAN_POINT('Ctrl Pts',(18.9408685219365,-21.4421845484509,
-16.280701115865));
#120975=CARTESIAN_POINT('Ctrl Pts',(16.7521228823537,-20.4738333552863,
-16.4078769225464));
#120976=CARTESIAN_POINT('Ctrl Pts',(16.3816264890446,-18.1092945142771,
-16.5350527292279));
#120977=CARTESIAN_POINT('Ctrl Pts',(18.1692867872707,-16.5178856522175,
-16.6622285359093));
#120978=CARTESIAN_POINT('Ctrl Pts',(20.475036408121,-17.1596256260733,-16.7894043425907));
#120979=CARTESIAN_POINT('Ctrl Pts',(21.1834931854267,-19.445757840707,-16.9165801492722));
#120980=CARTESIAN_POINT('Ctrl Pts',(19.6446919977966,-21.2788978825597,
-17.0437559559536));
#120981=CARTESIAN_POINT('Ctrl Pts',(17.2703874261082,-20.9772535407345,
-17.1709317626351));
#120982=CARTESIAN_POINT('Ctrl Pts',(16.2388565489241,-18.8175647766965,
-17.2981075693165));
#120983=CARTESIAN_POINT('Ctrl Pts',(17.4964649220338,-16.7812119860486,
-17.4252833759979));
#120984=CARTESIAN_POINT('Ctrl Pts',(19.8894349190882,-16.7364224639015,
-17.5524591826793));
#120985=CARTESIAN_POINT('Ctrl Pts',(21.2223650922577,-18.7242878168747,
-17.6796349893608));
#120986=CARTESIAN_POINT('Ctrl Pts',(20.2723747386373,-20.9210649644522,
-17.8068107960422));
#120987=CARTESIAN_POINT('Ctrl Pts',(17.9110210446204,-21.3113472211018,
-17.9339866027237));
#120988=CARTESIAN_POINT('Ctrl Pts',(16.3046994623321,-19.5370748399901,
-18.061162409405));
#120989=CARTESIAN_POINT('Ctrl Pts',(16.9271103439532,-17.226032607035,-18.1883382160865));
#120990=CARTESIAN_POINT('Ctrl Pts',(19.2072303367862,-16.498458331493,-18.3155140227679));
#120991=CARTESIAN_POINT('Ctrl Pts',(21.0531908675876,-18.0218562528634,
-18.4426898294494));
#120992=CARTESIAN_POINT('Ctrl Pts',(20.7714377226303,-20.3986033309466,
-18.5698656361308));
#120993=CARTESIAN_POINT('Ctrl Pts',(18.6204619247414,-21.4481816393175,
-18.6970414428122));
#120994=CARTESIAN_POINT('Ctrl Pts',(16.57365026406,-20.2076682239227,-18.8242172494937));
#120995=CARTESIAN_POINT('Ctrl Pts',(16.508825399435,-17.8151571490185,-18.9513930561751));
#120996=CARTESIAN_POINT('Ctrl Pts',(18.4854601213826,-16.4656288287323,
-19.0785688628566));
#120997=CARTESIAN_POINT('Ctrl Pts',(20.6901147549395,-17.3971917378963,
-19.205744669538));
#120998=CARTESIAN_POINT('Ctrl Pts',(21.1001555127428,-19.7551947225373,
-19.3329204762194));
#120999=CARTESIAN_POINT('Ctrl Pts',(19.3393954444469,-21.3763164063757,
-19.4600962829008));
#121000=CARTESIAN_POINT('Ctrl Pts',(17.0232226373686,-20.7732782473175,
-19.5872720895823));
#121001=CARTESIAN_POINT('Ctrl Pts',(16.2765818653196,-18.4993303570677,
-19.7144478962637));
#121002=CARTESIAN_POINT('Ctrl Pts',(17.784469731095,-16.6406787308973,-19.8416237029452));
#121003=CARTESIAN_POINT('Ctrl Pts',(20.1634926381912,-16.9025209845322,
-19.9687995096266));
#121004=CARTESIAN_POINT('Ctrl Pts',(21.2310448625075,-19.0446328907795,
-20.095975316308));
#121005=CARTESIAN_POINT('Ctrl Pts',(20.0077132391621,-21.1017601371114,
-20.2231511229895));
#121006=CARTESIAN_POINT('Ctrl Pts',(17.6158291027325,-21.1866153706034,
-20.3503269296709));
#121007=CARTESIAN_POINT('Ctrl Pts',(16.2497967305417,-19.2213506919733,
-20.4775027363524));
#121008=CARTESIAN_POINT('Ctrl Pts',(17.162867889616,-17.0089715551397,-20.6046785430338));
#121009=CARTESIAN_POINT('Ctrl Pts',(19.517352896747,-16.5792041101631,-20.7318543497152));
#121010=CARTESIAN_POINT('Ctrl Pts',(21.1531647647671,-18.3263225093304,
-20.8590301563966));
#121011=CARTESIAN_POINT('Ctrl Pts',(20.5695343966717,-20.6474748753932,
-20.9862059630781));
#121012=CARTESIAN_POINT('Ctrl Pts',(18.3019319358899,-21.4131078753525,
-21.1133817697595));
#121013=CARTESIAN_POINT('Ctrl Pts',(16.4306927582234,-19.9208780183908,
-21.2405575764409));
#121014=CARTESIAN_POINT('Ctrl Pts',(16.672657339533,-17.5396647158853,-21.3677333831224));
#121015=CARTESIAN_POINT('Ctrl Pts',(18.8056557936095,-16.4543701890598,
-21.4949091898038));
#121016=CARTESIAN_POINT('Ctrl Pts',(20.8731458592265,-17.6601321897591,
-21.6220849964852));
#121017=CARTESIAN_POINT('Ctrl Pts',(20.9776565367662,-20.0518039395808,
-21.7492608031667));
#121018=CARTESIAN_POINT('Ctrl Pts',(19.0246114636561,-21.4331200318623,
-21.8764366098481));
#121019=CARTESIAN_POINT('Ctrl Pts',(16.8032831871667,-20.5407974041735,
-22.0036124165295));
#121020=CARTESIAN_POINT('Ctrl Pts',(16.3565571918356,-18.1855239713029,
-22.130788223211));
#121021=CARTESIAN_POINT('Ctrl Pts',(17.5080922582077,-17.0924952631291,
-22.2155720943319));
#121022=CARTESIAN_POINT('Ctrl Pts',(18.187758323454,-16.9106265641217,-22.2579640298924));
#121023=CARTESIAN_POINT('Ctrl Pts',(20.4651728847368,-17.4941906656173,
0.0844764971292257));
#121024=CARTESIAN_POINT('Ctrl Pts',(20.9507812774351,-18.0708180784204,
0.0420659055481983));
#121025=CARTESIAN_POINT('Ctrl Pts',(21.2916315045783,-19.7372655677721,
-0.0427366215933074));
#121026=CARTESIAN_POINT('Ctrl Pts',(19.454354539323,-21.53119898684,-0.16993108429529));
#121027=CARTESIAN_POINT('Ctrl Pts',(16.9568469479949,-20.951919105231,-0.297106890976726));
#121028=CARTESIAN_POINT('Ctrl Pts',(16.0896125232803,-18.5411723000033,
-0.424282697658159));
#121029=CARTESIAN_POINT('Ctrl Pts',(17.648515078568,-16.5056184191814,-0.551458504339595));
#121030=CARTESIAN_POINT('Ctrl Pts',(20.2032439208991,-16.7153568936381,
-0.678634311021027));
#121031=CARTESIAN_POINT('Ctrl Pts',(21.41005272189,-18.9766152880434,-0.805810117702463));
#121032=CARTESIAN_POINT('Ctrl Pts',(20.1617388362496,-21.2155301029391,
-0.932985924383897));
#121033=CARTESIAN_POINT('Ctrl Pts',(17.6035685858491,-21.3776722727239,
-1.06016173106533));
#121034=CARTESIAN_POINT('Ctrl Pts',(16.0824961916403,-19.3144751852875,
-1.18733753774677));
#121035=CARTESIAN_POINT('Ctrl Pts',(16.9940154259929,-16.918696135723,-1.3145133444282));
#121036=CARTESIAN_POINT('Ctrl Pts',(19.5018617560294,-16.3883645566231,
-1.44168915110964));
#121037=CARTESIAN_POINT('Ctrl Pts',(21.3052429758379,-18.2100003608074,
-1.56886495779107));
#121038=CARTESIAN_POINT('Ctrl Pts',(20.7496681511615,-20.7123794613962,
-1.69604076447251));
#121039=CARTESIAN_POINT('Ctrl Pts',(18.344843009889,-21.599717237933,-1.82321657115394));
#121040=CARTESIAN_POINT('Ctrl Pts',(16.2970451984157,-20.057940045637,-1.95039237783538));
#121041=CARTESIAN_POINT('Ctrl Pts',(16.4850021913768,-17.5015308492868,
-2.07756818451681));
#121042=CARTESIAN_POINT('Ctrl Pts',(18.7362750704342,-16.275837412191,-2.20474399119824));
#121043=CARTESIAN_POINT('Ctrl Pts',(20.9854607212405,-17.5053568716867,
-2.33191979787968));
#121044=CARTESIAN_POINT('Ctrl Pts',(21.1690708977422,-20.0620817041385,
-2.45909560456111));
#121045=CARTESIAN_POINT('Ctrl Pts',(19.1186546651756,-21.6003754249779,
-2.58627141124255));
#121046=CARTESIAN_POINT('Ctrl Pts',(16.7153416505994,-20.7089490947747,
-2.71344721792398));
#121047=CARTESIAN_POINT('Ctrl Pts',(16.1640223800872,-18.2056310058767,
-2.84062302460542));
#121048=CARTESIAN_POINT('Ctrl Pts',(17.9704980647556,-16.3870601508454,
-2.96779883128685));
#121049=CARTESIAN_POINT('Ctrl Pts',(20.477439386886,-16.9216624058443,-3.09497463796828));
#121050=CARTESIAN_POINT('Ctrl Pts',(21.3848832815229,-19.3189733883075,
-3.22215044464972));
#121051=CARTESIAN_POINT('Ctrl Pts',(19.8603062977751,-21.3796090630069,
-3.34932625133115));
#121052=CARTESIAN_POINT('Ctrl Pts',(17.3024131922505,-21.213064097291,-3.47650205801259));
#121053=CARTESIAN_POINT('Ctrl Pts',(16.0579121285487,-18.9721331595253,
-3.60367786469402));
#121054=CARTESIAN_POINT('Ctrl Pts',(17.2685555901523,-16.7127312976299,
-3.73085367137545));
#121055=CARTESIAN_POINT('Ctrl Pts',(19.8236533420561,-16.5077194854014,
-3.85802947805689));
#121056=CARTESIAN_POINT('Ctrl Pts',(21.3790617841357,-18.5451833361938,
-3.98520528473832));
#121057=CARTESIAN_POINT('Ctrl Pts',(20.5077902103209,-20.9558762261203,
-4.11238109141976));
#121058=CARTESIAN_POINT('Ctrl Pts',(18.009176212373,-21.5281370531764,-4.23955689810119));
#121059=CARTESIAN_POINT('Ctrl Pts',(16.1755430519351,-19.7369520270363,
-4.36673270478263));
#121060=CARTESIAN_POINT('Ctrl Pts',(16.6891353455995,-17.2256222357103,
-4.49390851146406));
#121061=CARTESIAN_POINT('Ctrl Pts',(19.0787640410623,-16.2981368920303,
-4.6210843181455));
#121062=CARTESIAN_POINT('Ctrl Pts',(21.15209312732,-17.805406232592,-4.74826012482693));
#121063=CARTESIAN_POINT('Ctrl Pts',(21.0069718530473,-20.364604189115,-4.87543593150836));
#121064=CARTESIAN_POINT('Ctrl Pts',(18.7765399801474,-21.6278254782292,
-5.0026117381898));
#121065=CARTESIAN_POINT('Ctrl Pts',(16.5070803157911,-20.4361429715275,
-5.12978754487123));
#121066=CARTESIAN_POINT('Ctrl Pts',(16.2806812434728,-17.8828514047509,
-5.25696335155267));
#121067=CARTESIAN_POINT('Ctrl Pts',(18.3050498601331,-16.3104373152697,
-5.38413915823409));
#121068=CARTESIAN_POINT('Ctrl Pts',(20.7229536064731,-17.1614930351577,
-5.51131496491554));
#121069=CARTESIAN_POINT('Ctrl Pts',(21.3161158672572,-19.6552277638931,
-5.63849077159696));
#121070=CARTESIAN_POINT('Ctrl Pts',(19.5403470840179,-21.503794666494,-5.76566657827842));
#121071=CARTESIAN_POINT('Ctrl Pts',(17.0248048987365,-21.0112483448259,
-5.89284238495983));
#121072=CARTESIAN_POINT('Ctrl Pts',(16.0773431342523,-18.6294694781468,
-6.02001819164128));
#121073=CARTESIAN_POINT('Ctrl Pts',(17.5671991533703,-16.5435923467661,
-6.1471939983227));
#121074=CARTESIAN_POINT('Ctrl Pts',(20.127522529443,-16.6672797545901,-6.27436980500414));
#121075=CARTESIAN_POINT('Ctrl Pts',(21.4093754765144,-18.8870561818465,
-6.40154561168558));
#121076=CARTESIAN_POINT('Ctrl Pts',(20.2367374764131,-21.1664145313908,
-6.52872141836701));
#121077=CARTESIAN_POINT('Ctrl Pts',(17.6854311121095,-21.4141849904505,
-6.65589722504845));
#121078=CARTESIAN_POINT('Ctrl Pts',(16.0961216209204,-19.4030535412072,
-6.78307303172988));
#121079=CARTESIAN_POINT('Ctrl Pts',(16.9269018173399,-16.9781084634466,
-6.91024883841132));
#121080=CARTESIAN_POINT('Ctrl Pts',(19.4155824351873,-16.3640863569478,
-7.03742464509275));
#121081=CARTESIAN_POINT('Ctrl Pts',(21.2789534725274,-18.1243143939139,
-7.16460045177418));
#121082=CARTESIAN_POINT('Ctrl Pts',(20.8074876564503,-20.6438926025015,
-7.29177625845562));
#121083=CARTESIAN_POINT('Ctrl Pts',(18.4337256107381,-21.6112643589919,
-7.41895206513705));
#121084=CARTESIAN_POINT('Ctrl Pts',(16.3354466800433,-20.1389261186678,
-7.54612787181849));
#121085=CARTESIAN_POINT('Ctrl Pts',(16.4376915494001,-17.5776568334092,
-7.67330367849992));
#121086=CARTESIAN_POINT('Ctrl Pts',(18.646656897206,-16.2772621021406,-7.80047948518135));
#121087=CARTESIAN_POINT('Ctrl Pts',(20.9357541207011,-17.4307733792013,
-7.92765529186279));
#121088=CARTESIAN_POINT('Ctrl Pts',(21.2048785947256,-19.9799156628723,
-8.05483109854422));
#121089=CARTESIAN_POINT('Ctrl Pts',(19.2071253181107,-21.5860091254994,
-8.18200690522566));
#121090=CARTESIAN_POINT('Ctrl Pts',(16.7753089275983,-20.7755627005247,
-8.3091827119071));
#121091=CARTESIAN_POINT('Ctrl Pts',(16.1404700259359,-18.2921106808846,
-8.43635851858852));
#121092=CARTESIAN_POINT('Ctrl Pts',(17.8850339028528,-16.4140661541825,
-8.56353432526996));
#121093=CARTESIAN_POINT('Ctrl Pts',(20.4084714811236,-16.8644184090784,
-8.69071013195139));
#121094=CARTESIAN_POINT('Ctrl Pts',(21.3956854048846,-19.2299972037186,
-8.81788593863284));
#121095=CARTESIAN_POINT('Ctrl Pts',(19.9409681724916,-21.3405308183994,
-8.94506174531426));
#121096=CARTESIAN_POINT('Ctrl Pts',(17.3789325547309,-21.2597356561407,
-9.0722375519957));
#121097=CARTESIAN_POINT('Ctrl Pts',(16.0600872130337,-19.0617362636016,
-9.19941335867713));
#121098=CARTESIAN_POINT('Ctrl Pts',(17.1943908916334,-16.7630606602087,
-9.32658916535856));
#121099=CARTESIAN_POINT('Ctrl Pts',(19.7411903682412,-16.4726010401766,
-9.45376497204));
#121100=CARTESIAN_POINT('Ctrl Pts',(21.3639551952721,-18.4568360769276,
-9.58094077872143));
#121101=CARTESIAN_POINT('Ctrl Pts',(20.5738993640695,-20.8953532797583,
-9.70811658540287));
#121102=CARTESIAN_POINT('Ctrl Pts',(18.0958500633667,-21.5509644665186,
-9.83529239208431));
#121103=CARTESIAN_POINT('Ctrl Pts',(16.2032637214729,-19.8221870651751,
-9.96246819876573));
#121104=CARTESIAN_POINT('Ctrl Pts',(16.6324708399194,-17.2950670414339,
-10.0896440054472));
#121105=CARTESIAN_POINT('Ctrl Pts',(18.9897005271298,-16.2880801663194,
-10.2168198121286));
#121106=CARTESIAN_POINT('Ctrl Pts',(21.1123408512631,-17.7250743970949,
-10.3439956188101));
#121107=CARTESIAN_POINT('Ctrl Pts',(21.0530010608437,-20.2876967169446,
-10.4711714254915));
#121108=CARTESIAN_POINT('Ctrl Pts',(18.8661217305387,-21.6249002016856,
-10.598347232173));
#121109=CARTESIAN_POINT('Ctrl Pts',(16.5580289128638,-20.5098836502765,
-10.7255230388544));
#121110=CARTESIAN_POINT('Ctrl Pts',(16.2462545116391,-17.965605542903,-10.8526988455358));
#121111=CARTESIAN_POINT('Ctrl Pts',(18.2168321890867,-16.3262831273715,
-10.9798746522173));
#121112=CARTESIAN_POINT('Ctrl Pts',(20.6618792339927,-17.0958929721078,
-11.1070504588987));
#121113=CARTESIAN_POINT('Ctrl Pts',(21.3382167393905,-19.5683658119407,
-11.2342262655802));
#121114=CARTESIAN_POINT('Ctrl Pts',(19.6253470223175,-21.4753612752947,
-11.3614020722615));
#121115=CARTESIAN_POINT('Ctrl Pts',(17.0947217355035,-21.0673293860297,
-11.488577878943));
#121116=CARTESIAN_POINT('Ctrl Pts',(16.0680325112813,-18.7186140772312,
-11.6157536856244));
#121117=CARTESIAN_POINT('Ctrl Pts',(17.4872029893547,-16.584015867009,-11.7429294923059));
#121118=CARTESIAN_POINT('Ctrl Pts',(20.0502323397452,-16.6218961251351,
-11.8701052989873));
#121119=CARTESIAN_POINT('Ctrl Pts',(21.4057002130119,-18.797502065893,-11.9972811056688));
#121120=CARTESIAN_POINT('Ctrl Pts',(20.3100489652568,-21.1148502719707,
-12.1244569123501));
#121121=CARTESIAN_POINT('Ctrl Pts',(17.7684706125095,-21.4479175951428,
-12.2516327190316));
#121122=CARTESIAN_POINT('Ctrl Pts',(16.1127055452724,-19.4911354388884,
-12.378808525713));
#121123=CARTESIAN_POINT('Ctrl Pts',(16.8618154443651,-17.0397299799731,
-12.5059843323945));
#121124=CARTESIAN_POINT('Ctrl Pts',(19.3285384723745,-16.3427135755694,
-12.6331601390759));
#121125=CARTESIAN_POINT('Ctrl Pts',(21.2498093531994,-18.0395555150007,
-12.7603359457573));
#121126=CARTESIAN_POINT('Ctrl Pts',(20.8629813012026,-20.5735086367272,
-12.8875117524388));
#121127=CARTESIAN_POINT('Ctrl Pts',(18.5229450448345,-21.6198282264327,
-13.0146875591202));
#121128=CARTESIAN_POINT('Ctrl Pts',(16.3765386102829,-20.2185810024805,
-13.1418633658017));
#121129=CARTESIAN_POINT('Ctrl Pts',(16.3929566802409,-17.6553243216352,
-13.2690391724831));
#121130=CARTESIAN_POINT('Ctrl Pts',(18.5571366945425,-16.2816870949206,
-13.3962149791645));
#121131=CARTESIAN_POINT('Ctrl Pts',(20.8835778142264,-17.3578962203056,
-13.5233907858459));
#121132=CARTESIAN_POINT('Ctrl Pts',(21.2379147072037,-19.8965966223211,
-13.6505665925274));
#121133=CARTESIAN_POINT('Ctrl Pts',(19.2950652667951,-21.5686882516355,
-13.7777423992088));
#121134=CARTESIAN_POINT('Ctrl Pts',(16.8374732677398,-20.8401308200636,
-13.9049182058902));
#121135=CARTESIAN_POINT('Ctrl Pts',(16.1198268338089,-18.3793305516987,
-14.0320940125717));
#121136=CARTESIAN_POINT('Ctrl Pts',(17.8005220259727,-16.4439189582757,
-14.1592698192531));
#121137=CARTESIAN_POINT('Ctrl Pts',(20.3376253211293,-16.809516051569,-14.2864456259346));
#121138=CARTESIAN_POINT('Ctrl Pts',(21.4035019163622,-19.140709189997,-14.413621432616));
#121139=CARTESIAN_POINT('Ctrl Pts',(20.0202761913079,-21.2987733592159,
-14.5407972392974));
#121140=CARTESIAN_POINT('Ctrl Pts',(17.4569718960327,-21.303818628536,-14.6679730459788));
#121141=CARTESIAN_POINT('Ctrl Pts',(16.0652616248443,-19.1512162765007,
-14.7951488526603));
#121142=CARTESIAN_POINT('Ctrl Pts',(17.1219531722769,-16.8158453555327,
-14.9223246593417));
#121143=CARTESIAN_POINT('Ctrl Pts',(19.6575976292351,-16.4402637361534,
-15.0495004660232));
#121144=CARTESIAN_POINT('Ctrl Pts',(21.3458985863041,-18.369044242919,-15.1766762727046));
#121145=CARTESIAN_POINT('Ctrl Pts',(20.6379447031482,-20.8326504744915,
-15.303852079386));
#121146=CARTESIAN_POINT('Ctrl Pts',(18.1832397269893,-21.5708766220509,
-15.4310278860674));
#121147=CARTESIAN_POINT('Ctrl Pts',(16.2338231172801,-19.9064460146934,
-15.5582036927489));
#121148=CARTESIAN_POINT('Ctrl Pts',(16.578163618988,-17.3663704284554,-15.6853794994303));
#121149=CARTESIAN_POINT('Ctrl Pts',(18.9003501939781,-16.2810115588392,
-15.8125553061118));
#121150=CARTESIAN_POINT('Ctrl Pts',(21.0699207908507,-17.6461188037487,
-15.9397311127932));
#121151=CARTESIAN_POINT('Ctrl Pts',(21.0964290457131,-20.2092909940909,
-16.0669069194746));
#121152=CARTESIAN_POINT('Ctrl Pts',(18.955555280017,-21.6189767336345,-16.194082726156));
#121153=CARTESIAN_POINT('Ctrl Pts',(16.6114182961767,-20.5818768513131,
-16.3212585328375));
#121154=CARTESIAN_POINT('Ctrl Pts',(16.214618283316,-18.0494661194781,-16.4484343395189));
#121155=CARTESIAN_POINT('Ctrl Pts',(18.1291946250482,-16.3450742054518,
-16.5756101462004));
#121156=CARTESIAN_POINT('Ctrl Pts',(20.5986423598435,-17.0323749038605,
-16.7027859528818));
#121157=CARTESIAN_POINT('Ctrl Pts',(21.3573964622394,-19.4808124826067,
-16.8299617595632));
#121158=CARTESIAN_POINT('Ctrl Pts',(19.7093471368785,-21.4440974303655,
-16.9571375662447));
#121159=CARTESIAN_POINT('Ctrl Pts',(17.1664773503022,-21.1210376627748,
-17.0843133729261));
#121160=CARTESIAN_POINT('Ctrl Pts',(16.0617123033954,-18.8080204652485,
-17.2114891796075));
#121161=CARTESIAN_POINT('Ctrl Pts',(17.4086053572432,-16.6270955544791,
-17.338664986289));
#121162=CARTESIAN_POINT('Ctrl Pts',(19.9714657325515,-16.579126172631,-17.4658407929704));
#121163=CARTESIAN_POINT('Ctrl Pts',(21.3990281040287,-18.708121250235,-17.5930165996518));
#121164=CARTESIAN_POINT('Ctrl Pts',(20.3815926003592,-21.0608599439249,
-17.7201924063333));
#121165=CARTESIAN_POINT('Ctrl Pts',(17.8525931469884,-21.4788505296758,
-17.8473682130147));
#121166=CARTESIAN_POINT('Ctrl Pts',(16.1322297749793,-19.5786125884764,
-17.9745440196961));
#121167=CARTESIAN_POINT('Ctrl Pts',(16.7988291003494,-17.1034964893213,
-18.1017198263776));
#121168=CARTESIAN_POINT('Ctrl Pts',(19.2408276159067,-16.3242676301314,
-18.228895633059));
#121169=CARTESIAN_POINT('Ctrl Pts',(21.2178432511203,-17.955820124861,-18.3560714397405));
#121170=CARTESIAN_POINT('Ctrl Pts',(20.9160868681659,-20.5013058250774,
-18.4832472464219));
#121171=CARTESIAN_POINT('Ctrl Pts',(18.6124012191849,-21.6253995916595,
-18.6104230531033));
#121172=CARTESIAN_POINT('Ctrl Pts',(16.4202749044646,-20.2968151625747,
-18.7375988597848));
#121173=CARTESIAN_POINT('Ctrl Pts',(16.3508477586638,-17.7344462908773,
-18.8647746664662));
#121174=CARTESIAN_POINT('Ctrl Pts',(18.4678148796782,-16.2891073766096,
-18.9919504731476));
#121175=CARTESIAN_POINT('Ctrl Pts',(20.8289903263147,-17.286807168058,-19.119126279829));
#121176=CARTESIAN_POINT('Ctrl Pts',(21.2681421801737,-19.8122180263779,
-19.2463020865105));
#121177=CARTESIAN_POINT('Ctrl Pts',(19.3823758667575,-21.5484322422587,
-19.3734778931919));
#121178=CARTESIAN_POINT('Ctrl Pts',(16.9017649452107,-20.9025810178173,
-19.5006536998734));
#121179=CARTESIAN_POINT('Ctrl Pts',(16.1021159518554,-18.4671927970664,
-19.6278295065548));
#121180=CARTESIAN_POINT('Ctrl Pts',(17.7170572450437,-16.4765850543542,
-19.7550053132362));
#121181=CARTESIAN_POINT('Ctrl Pts',(20.2649803481551,-16.757016959998,-19.8821811199177));
#121182=CARTESIAN_POINT('Ctrl Pts',(21.4083240999114,-19.0512094198929,
-20.0093569265991));
#121183=CARTESIAN_POINT('Ctrl Pts',(20.0981412947811,-21.2543836816181,
-20.1365327332805));
#121184=CARTESIAN_POINT('Ctrl Pts',(17.5364438714413,-21.345263264656,-20.2637085399619));
#121185=CARTESIAN_POINT('Ctrl Pts',(16.0734291899427,-19.2404734101847,
-20.3908843466434));
#121186=CARTESIAN_POINT('Ctrl Pts',(17.0513243981187,-16.8710250544057,
-20.5180601533248));
#121187=CARTESIAN_POINT('Ctrl Pts',(19.5729675179493,-16.4107460050722,
-20.6452359600063));
#121188=CARTESIAN_POINT('Ctrl Pts',(21.3249148566822,-18.2819021506609,
-20.7724117666877));
#121189=CARTESIAN_POINT('Ctrl Pts',(20.6998492912724,-20.7678461580482,
-20.8995875733692));
#121190=CARTESIAN_POINT('Ctrl Pts',(18.2712569976611,-21.5878357442275,
-21.0267633800505));
#121191=CARTESIAN_POINT('Ctrl Pts',(16.2671680424845,-19.989664109829,-21.153939186732));
#121192=CARTESIAN_POINT('Ctrl Pts',(16.5263110482178,-17.4393951028376,
-21.2811149934134));
#121193=CARTESIAN_POINT('Ctrl Pts',(18.8107430407941,-16.2770494228818,
-21.4082908000949));
#121194=CARTESIAN_POINT('Ctrl Pts',(21.0250158365398,-17.568415239189,-21.5354666067763));
#121195=CARTESIAN_POINT('Ctrl Pts',(21.1369463139771,-20.1298851974028,
-21.6626424134577));
#121196=CARTESIAN_POINT('Ctrl Pts',(19.0452436034431,-21.6092686761098,
-21.7898182201392));
#121197=CARTESIAN_POINT('Ctrl Pts',(16.6662107583285,-20.6535950540795,
-21.9169940268206));
#121198=CARTESIAN_POINT('Ctrl Pts',(16.1877691759169,-18.1311075337387,
-22.044169833502));
#121199=CARTESIAN_POINT('Ctrl Pts',(17.4210581833076,-16.960478579468,-22.128953704623));
#121200=CARTESIAN_POINT('Ctrl Pts',(18.1489775593156,-16.7656980002009,
-22.1713456401835));
#121201=CARTESIAN_POINT('Ctrl Pts',(20.5799312301559,-17.397553415447,0.171094886838164));
#121202=CARTESIAN_POINT('Ctrl Pts',(21.0977302932135,-18.0124050913494,
0.128684295257136));
#121203=CARTESIAN_POINT('Ctrl Pts',(21.4611752643293,-19.7893203209783,
0.0438817681156306));
#121204=CARTESIAN_POINT('Ctrl Pts',(19.5021063818899,-21.7021724412225,
-0.083312694586353));
#121205=CARTESIAN_POINT('Ctrl Pts',(16.8390406066394,-21.0844924660501,
-0.210488501267787));
#121206=CARTESIAN_POINT('Ctrl Pts',(15.9143177655174,-18.5139387940262,
-0.337664307949222));
#121207=CARTESIAN_POINT('Ctrl Pts',(17.5765589760555,-16.343449345859,-0.464840114630656));
#121208=CARTESIAN_POINT('Ctrl Pts',(20.3006391625102,-16.567091249899,-0.592015921312091));
#121209=CARTESIAN_POINT('Ctrl Pts',(21.5874465485414,-18.9782470197745,
-0.719191727993525));
#121210=CARTESIAN_POINT('Ctrl Pts',(20.2563827322944,-21.3655780685178,
-0.84636753467496));
#121211=CARTESIAN_POINT('Ctrl Pts',(17.5286330090264,-21.5384685392327,
-0.973543341356393));
#121212=CARTESIAN_POINT('Ctrl Pts',(15.906729696796,-19.3385034339308,-1.10071914803782));
#121213=CARTESIAN_POINT('Ctrl Pts',(16.8786729593171,-16.7839097205383,
-1.22789495471926));
#121214=CARTESIAN_POINT('Ctrl Pts',(19.5527628216649,-16.2184227996018,
-1.35507076140069));
#121215=CARTESIAN_POINT('Ctrl Pts',(21.4756890313297,-18.1608136783876,
-1.48224656808212));
#121216=CARTESIAN_POINT('Ctrl Pts',(20.8832855061817,-20.8290738921377,
-1.60942237476356));
#121217=CARTESIAN_POINT('Ctrl Pts',(18.3190460414365,-21.7752327234411,
-1.73659818144499));
#121218=CARTESIAN_POINT('Ctrl Pts',(16.1355010202711,-20.1312521052755,
-1.86377398812643));
#121219=CARTESIAN_POINT('Ctrl Pts',(16.3359175623115,-17.4053801752063,
-1.99094979480786));
#121220=CARTESIAN_POINT('Ctrl Pts',(18.7364258834009,-16.0984363025981,
-2.1181256014893));
#121221=CARTESIAN_POINT('Ctrl Pts',(21.134708615211,-17.4094598221888,-2.24530140817073));
#121222=CARTESIAN_POINT('Ctrl Pts',(21.3304901931037,-20.135668311675,-2.37247721485217));
#121223=CARTESIAN_POINT('Ctrl Pts',(19.1441531773822,-21.7759345412849,
-2.4996530215336));
#121224=CARTESIAN_POINT('Ctrl Pts',(16.5815260772467,-20.8254161287028,
-2.62682882821504));
#121225=CARTESIAN_POINT('Ctrl Pts',(15.9936602042319,-18.1561546817078,
-2.75400463489647));
#121226=CARTESIAN_POINT('Ctrl Pts',(17.9198860088567,-16.2170319255978,
-2.8811804415779));
#121227=CARTESIAN_POINT('Ctrl Pts',(20.5930108709022,-16.7870726228123,
-3.00835624825934));
#121228=CARTESIAN_POINT('Ctrl Pts',(21.5606086420394,-19.3432998199575,
-3.13553205494077));
#121229=CARTESIAN_POINT('Ctrl Pts',(19.9349684232667,-21.5405337181072,
-3.26270786162221));
#121230=CARTESIAN_POINT('Ctrl Pts',(17.2075142166313,-21.3629485929295,
-3.38988366830364));
#121231=CARTESIAN_POINT('Ctrl Pts',(15.8805159718553,-18.9734677738181,
-3.51705947498508));
#121232=CARTESIAN_POINT('Ctrl Pts',(17.1714122157033,-16.5642916048074,
-3.64423528166651));
#121233=CARTESIAN_POINT('Ctrl Pts',(19.8958857665108,-16.3456896904175,
-3.77141108834795));
#121234=CARTESIAN_POINT('Ctrl Pts',(21.5544012413067,-18.5182157192451,
-3.89858689502938));
#121235=CARTESIAN_POINT('Ctrl Pts',(20.6253736310478,-21.0887119019572,
-4.02576270171081));
#121236=CARTESIAN_POINT('Ctrl Pts',(17.9611281061891,-21.6989075339308,
-4.15293850839225));
#121237=CARTESIAN_POINT('Ctrl Pts',(16.0059445740623,-19.7889859958273,
-4.28011431507368));
#121238=CARTESIAN_POINT('Ctrl Pts',(16.5535825730174,-17.1111817557645,
-4.40729012175512));
#121239=CARTESIAN_POINT('Ctrl Pts',(19.101618229261,-16.1222140007207,-4.53446592843655));
#121240=CARTESIAN_POINT('Ctrl Pts',(21.3123869771181,-17.7293992636892,
-4.66164173511799));
#121241=CARTESIAN_POINT('Ctrl Pts',(21.1576457062134,-20.4582448190627,
-4.78881754179942));
#121242=CARTESIAN_POINT('Ctrl Pts',(18.7793599282756,-21.8052042410432,
-4.91599334848085));
#121243=CARTESIAN_POINT('Ctrl Pts',(16.3594592314994,-20.5345258616938,
-5.04316915516229));
#121244=CARTESIAN_POINT('Ctrl Pts',(16.1180523092011,-17.8119782268727,
-5.17034496184372));
#121245=CARTESIAN_POINT('Ctrl Pts',(18.2766150291857,-16.1353298111647,
-5.29752076852516));
#121246=CARTESIAN_POINT('Ctrl Pts',(20.8548000713794,-17.0428014714449,
-5.42469657520659));
#121247=CARTESIAN_POINT('Ctrl Pts',(21.4872826797803,-19.7018442834496,
-5.55187238188803));
#121248=CARTESIAN_POINT('Ctrl Pts',(19.5937993174784,-21.6729515059744,
-5.67904818856947));
#121249=CARTESIAN_POINT('Ctrl Pts',(16.9115034465541,-21.1477546030643,
-5.80622399525089));
#121250=CARTESIAN_POINT('Ctrl Pts',(15.901235046523,-18.6080891357435,-5.93339980193234));
#121251=CARTESIAN_POINT('Ctrl Pts',(17.4898526700851,-16.3839405408623,
-6.06057560861376));
#121252=CARTESIAN_POINT('Ctrl Pts',(20.2198982483519,-16.515827107994,-6.1877514152952));
#121253=CARTESIAN_POINT('Ctrl Pts',(21.5867244090021,-18.8827510975986,
-6.31492722197664));
#121254=CARTESIAN_POINT('Ctrl Pts',(20.3363529844383,-21.3132066570849,
-6.44210302865807));
#121255=CARTESIAN_POINT('Ctrl Pts',(17.6159221498948,-21.577401661709,-6.5692788353395));
#121256=CARTESIAN_POINT('Ctrl Pts',(15.921258347085,-19.4329535925197,-6.69645464202094));
#121257=CARTESIAN_POINT('Ctrl Pts',(16.8071104323889,-16.8472604535401,
-6.82363044870237));
#121258=CARTESIAN_POINT('Ctrl Pts',(19.4607640997214,-16.1925352135684,
-6.95080625538382));
#121259=CARTESIAN_POINT('Ctrl Pts',(21.4476568136269,-18.0694476434471,
-7.07798206206524));
#121260=CARTESIAN_POINT('Ctrl Pts',(20.9449378295665,-20.7560470830862,
-7.20515786874667));
#121261=CARTESIAN_POINT('Ctrl Pts',(18.4138206131569,-21.7875452957837,
-7.33233367542811));
#121262=CARTESIAN_POINT('Ctrl Pts',(16.1764481116018,-20.2176066933892,
-7.45950948210954));
#121263=CARTESIAN_POINT('Ctrl Pts',(16.2854707280793,-17.4865525022204,
-7.58668528879099));
#121264=CARTESIAN_POINT('Ctrl Pts',(18.6408669786781,-16.0999554343348,
-7.7138610954724));
#121265=CARTESIAN_POINT('Ctrl Pts',(21.0817069958525,-17.3299322375973,
-7.84103690215386));
#121266=CARTESIAN_POINT('Ctrl Pts',(21.3686715594619,-20.0480555359847,
-7.96821270883527));
#121267=CARTESIAN_POINT('Ctrl Pts',(19.2384884934243,-21.7606159089848,
-8.09538851551672));
#121268=CARTESIAN_POINT('Ctrl Pts',(16.6454685467572,-20.8964455078546,
-8.22256432219814));
#121269=CARTESIAN_POINT('Ctrl Pts',(15.9685465795588,-18.2483670391668,
-8.3497401288796));
#121270=CARTESIAN_POINT('Ctrl Pts',(17.8287564822182,-16.2458281396566,
-8.47691593556101));
#121271=CARTESIAN_POINT('Ctrl Pts',(20.5194711266931,-16.726033958043,-8.60409174224245));
#121272=CARTESIAN_POINT('Ctrl Pts',(21.5721268312631,-19.248425460891,-8.7312675489239));
#121273=CARTESIAN_POINT('Ctrl Pts',(20.0209773221669,-21.4988650016106,
-8.85844335560532));
#121274=CARTESIAN_POINT('Ctrl Pts',(17.2891059988037,-21.412713979622,-8.98561916228675));
#121275=CARTESIAN_POINT('Ctrl Pts',(15.8828352413023,-19.0690106104646,
-9.11279496896819));
#121276=CARTESIAN_POINT('Ctrl Pts',(17.0923311866634,-16.6179572687033,
-9.23997077564962));
#121277=CARTESIAN_POINT('Ctrl Pts',(19.8079563748028,-16.308243265877,-9.36714658233106));
#121278=CARTESIAN_POINT('Ctrl Pts',(21.5382932463106,-18.4240119765596,
-9.49432238901249));
#121279=CARTESIAN_POINT('Ctrl Pts',(20.6958651183971,-21.0241769281162,
-9.62149819569393));
#121280=CARTESIAN_POINT('Ctrl Pts',(18.0535475114361,-21.7232481619313,
-9.74867400237536));
#121281=CARTESIAN_POINT('Ctrl Pts',(16.0355028290879,-19.8798712102337,
-9.87584980905679));
#121282=CARTESIAN_POINT('Ctrl Pts',(16.4931618134281,-17.1852300133289,
-10.0030256157383));
#121283=CARTESIAN_POINT('Ctrl Pts',(19.0066507518444,-16.1114906210823,
-10.1302014224197));
#121284=CARTESIAN_POINT('Ctrl Pts',(21.2699995480578,-17.6437422820975,
-10.2573772291012));
#121285=CARTESIAN_POINT('Ctrl Pts',(21.2067261608115,-20.3762391996566,
-10.3845530357826));
#121286=CARTESIAN_POINT('Ctrl Pts',(18.874879995715,-21.802085049785,-10.511728842464));
#121287=CARTESIAN_POINT('Ctrl Pts',(16.4137851785486,-20.613154762964,-10.6389046491454));
#121288=CARTESIAN_POINT('Ctrl Pts',(16.0813434512909,-17.9002180840159,
-10.7660804558269));
#121289=CARTESIAN_POINT('Ctrl Pts',(18.1825494650401,-16.1522260320353,
-10.8932562625082));
#121290=CARTESIAN_POINT('Ctrl Pts',(20.7896771177347,-16.9728528220917,
-11.0204320691897));
#121291=CARTESIAN_POINT('Ctrl Pts',(21.5108486046191,-19.6092243081515,
-11.1476078758711));
#121292=CARTESIAN_POINT('Ctrl Pts',(19.6844338474273,-21.6426332834231,
-11.2747836825526));
#121293=CARTESIAN_POINT('Ctrl Pts',(16.9860550257985,-21.2075532206898,
-11.4019594892341));
#121294=CARTESIAN_POINT('Ctrl Pts',(15.8913072282989,-18.7031430733949,
-11.5291352959155));
#121295=CARTESIAN_POINT('Ctrl Pts',(17.4045536114233,-16.4270437104573,
-11.6563111025968));
#121296=CARTESIAN_POINT('Ctrl Pts',(20.1374845413179,-16.4674350267135,
-11.7834869092783));
#121297=CARTESIAN_POINT('Ctrl Pts',(21.5828055146281,-18.7872604964662,
-11.9106627159598));
#121298=CARTESIAN_POINT('Ctrl Pts',(20.4145242450785,-21.2582242358244,
-12.0378385226412));
#121299=CARTESIAN_POINT('Ctrl Pts',(17.7044662857673,-21.613370379233,-12.1650143293227));
#121300=CARTESIAN_POINT('Ctrl Pts',(15.9389416091958,-19.5268743829703,
-12.2921901360041));
#121301=CARTESIAN_POINT('Ctrl Pts',(16.7377095252982,-16.9129668210605,
-12.4193659426856));
#121302=CARTESIAN_POINT('Ctrl Pts',(19.3679500481791,-16.1697456441557,
-12.5465417493669));
#121303=CARTESIAN_POINT('Ctrl Pts',(21.416580749233,-17.9790701525573,-12.6737175560484));
#121304=CARTESIAN_POINT('Ctrl Pts',(21.0041101126047,-20.6809974091509,
-12.8008933627298));
#121305=CARTESIAN_POINT('Ctrl Pts',(18.5089543465855,-21.7966768565304,
-12.9280691694113));
#121306=CARTESIAN_POINT('Ctrl Pts',(16.2202639996657,-20.3025418486013,
-13.0552449760926));
#121307=CARTESIAN_POINT('Ctrl Pts',(16.2377704130005,-17.5693685186612,
-13.1824207827741));
#121308=CARTESIAN_POINT('Ctrl Pts',(18.545412538926,-16.1046737570615,-13.3095965894556));
#121309=CARTESIAN_POINT('Ctrl Pts',(21.0260719553289,-17.2522240983603,
-13.436772396137));
#121310=CARTESIAN_POINT('Ctrl Pts',(21.4038976147472,-19.9592133294229,
-13.5639482028184));
#121311=CARTESIAN_POINT('Ctrl Pts',(19.3322579251698,-21.7421468454496,
-13.6911240094999));
#121312=CARTESIAN_POINT('Ctrl Pts',(16.7117537213236,-20.96529380682,-13.8182998161813));
#121313=CARTESIAN_POINT('Ctrl Pts',(15.9465349634034,-18.3413686595396,
-13.9454756228628));
#121314=CARTESIAN_POINT('Ctrl Pts',(17.7386423669686,-16.2776598670762,
-14.0726514295442));
#121315=CARTESIAN_POINT('Ctrl Pts',(20.443928619978,-16.6674921583018,-14.1998272362256));
#121316=CARTESIAN_POINT('Ctrl Pts',(21.5804614942969,-19.1532186017375,
-14.3270030429069));
#121317=CARTESIAN_POINT('Ctrl Pts',(20.1055426189236,-21.454339467114,-14.4541788495885));
#121318=CARTESIAN_POINT('Ctrl Pts',(17.3723185182233,-21.4597191841168,
-14.5813546562699));
#121319=CARTESIAN_POINT('Ctrl Pts',(15.8883526615688,-19.1644221962985,
-14.7085304629514));
#121320=CARTESIAN_POINT('Ctrl Pts',(17.0150916171319,-16.6742410277849,
-14.8357062696328));
#121321=CARTESIAN_POINT('Ctrl Pts',(19.7188223264901,-16.2737623426128,
-14.9628820763142));
#121322=CARTESIAN_POINT('Ctrl Pts',(21.5190396762608,-18.3304004779172,
-15.0900578829957));
#121323=CARTESIAN_POINT('Ctrl Pts',(20.7641559821193,-20.9573175939151,
-15.2172336896771));
#121324=CARTESIAN_POINT('Ctrl Pts',(18.1467301800744,-21.7444802815428,
-15.3444094963585));
#121325=CARTESIAN_POINT('Ctrl Pts',(16.0680879877353,-19.9697156317281,
-15.4715853030399));
#121326=CARTESIAN_POINT('Ctrl Pts',(16.4352546014886,-17.2612600563589,
-15.5987611097214));
#121327=CARTESIAN_POINT('Ctrl Pts',(18.9113774421457,-16.1039534401246,
-15.7259369164028));
#121328=CARTESIAN_POINT('Ctrl Pts',(21.2247674889198,-17.5595527728704,
-15.8531127230842));
#121329=CARTESIAN_POINT('Ctrl Pts',(21.2530329590753,-20.2926360114859,
-15.9802885297657));
#121330=CARTESIAN_POINT('Ctrl Pts',(18.9702420380974,-21.7957689188181,
-16.1074643364471));
#121331=CARTESIAN_POINT('Ctrl Pts',(16.4707137099997,-20.6899203473398,
-16.2346401431286));
#121332=CARTESIAN_POINT('Ctrl Pts',(16.0476100775874,-17.9896377246791,
-16.3618159498099));
#121333=CARTESIAN_POINT('Ctrl Pts',(18.0891024628257,-16.1722627586861,
-16.4889917564913));
#121334=CARTESIAN_POINT('Ctrl Pts',(20.722248311566,-16.9051241816477,-16.6161675631729));
#121335=CARTESIAN_POINT('Ctrl Pts',(21.5312997390521,-19.5158671245064,
-16.7433433698543));
#121336=CARTESIAN_POINT('Ctrl Pts',(19.7740022759604,-21.6092969781711,
-16.8705191765357));
#121337=CARTESIAN_POINT('Ctrl Pts',(17.062567274496,-21.2648217848151,-16.9976949832172));
#121338=CARTESIAN_POINT('Ctrl Pts',(15.8845680578669,-18.7984761538005,
-17.1248707898986));
#121339=CARTESIAN_POINT('Ctrl Pts',(17.3207457924526,-16.4729791229096,
-17.2520465965799));
#121340=CARTESIAN_POINT('Ctrl Pts',(20.0534965460147,-16.4218298813604,
-17.3792224032615));
#121341=CARTESIAN_POINT('Ctrl Pts',(21.5756911157996,-18.6919546835953,
-17.5063982099429));
#121342=CARTESIAN_POINT('Ctrl Pts',(20.4908104620813,-21.2006549233977,
-17.6335740166242));
#121343=CARTESIAN_POINT('Ctrl Pts',(17.7941652493564,-21.6463538382498,
-17.7607498233058));
#121344=CARTESIAN_POINT('Ctrl Pts',(15.9597600876265,-19.6201503369626,
-17.8879256299872));
#121345=CARTESIAN_POINT('Ctrl Pts',(16.6705478567457,-16.9809603716076,
-18.0151014366687));
#121346=CARTESIAN_POINT('Ctrl Pts',(19.274424895027,-16.1500769287699,-18.1422772433501));
#121347=CARTESIAN_POINT('Ctrl Pts',(21.382495634653,-17.8897839968585,-18.2694530500315));
#121348=CARTESIAN_POINT('Ctrl Pts',(21.0607360137014,-20.6040083192082,
-18.3966288567128));
#121349=CARTESIAN_POINT('Ctrl Pts',(18.6043405136283,-21.8026175440015,
-18.5238046633944));
#121350=CARTESIAN_POINT('Ctrl Pts',(16.2668995448691,-20.3859621012267,
-18.6509804700757));
#121351=CARTESIAN_POINT('Ctrl Pts',(16.1928701178928,-17.6537354327361,
-18.7781562767572));
#121352=CARTESIAN_POINT('Ctrl Pts',(18.4501696379737,-16.1125859244869,
-18.9053320834387));
#121353=CARTESIAN_POINT('Ctrl Pts',(20.9678658976898,-17.1764225982197,
-19.0325078901201));
#121354=CARTESIAN_POINT('Ctrl Pts',(21.4361288476046,-19.8692413302184,
-19.1596836968014));
#121355=CARTESIAN_POINT('Ctrl Pts',(19.4253562890682,-21.7205480781417,
-19.286859503483));
#121356=CARTESIAN_POINT('Ctrl Pts',(16.7803072530527,-21.0318837883171,
-19.4140353101644));
#121357=CARTESIAN_POINT('Ctrl Pts',(15.9276500383911,-18.4350552370649,
-19.5412111168458));
#121358=CARTESIAN_POINT('Ctrl Pts',(17.6496447589923,-16.3124913778111,
-19.6683869235273));
#121359=CARTESIAN_POINT('Ctrl Pts',(20.366468058119,-16.6115129354638,-19.7955627302086));
#121360=CARTESIAN_POINT('Ctrl Pts',(21.5856033373152,-19.0577859490064,
-19.9227385368901));
#121361=CARTESIAN_POINT('Ctrl Pts',(20.1885693504001,-21.4070072261248,
-20.0499143435716));
#121362=CARTESIAN_POINT('Ctrl Pts',(17.45705864015,-21.5039111587085,-20.1770901502529));
#121363=CARTESIAN_POINT('Ctrl Pts',(15.8970616493438,-19.2595961283962,
-20.3042659569345));
#121364=CARTESIAN_POINT('Ctrl Pts',(16.9397809066213,-16.7330785536716,
-20.4314417636159));
#121365=CARTESIAN_POINT('Ctrl Pts',(19.6285821391516,-16.2422878999811,
-20.5586175702973));
#121366=CARTESIAN_POINT('Ctrl Pts',(21.4966649485975,-18.2374817919912,
-20.6857933769788));
#121367=CARTESIAN_POINT('Ctrl Pts',(20.8301641858729,-20.8882174407032,
-20.8129691836602));
#121368=CARTESIAN_POINT('Ctrl Pts',(18.2405820594323,-21.7625636131024,
-20.9401449903416));
#121369=CARTESIAN_POINT('Ctrl Pts',(16.1036433267455,-20.0584502012673,
-21.0673207970231));
#121370=CARTESIAN_POINT('Ctrl Pts',(16.3799647569026,-17.3391254897899,
-21.1944966037045));
#121371=CARTESIAN_POINT('Ctrl Pts',(18.8158302879787,-16.0997286567039,
-21.3216724103859));
#121372=CARTESIAN_POINT('Ctrl Pts',(21.1768858138531,-17.4766982886188,
-21.4488482170674));
#121373=CARTESIAN_POINT('Ctrl Pts',(21.2962360911878,-20.207966455225,-21.5760240237488));
#121374=CARTESIAN_POINT('Ctrl Pts',(19.0658757432302,-21.7854173203574,
-21.7031998304301));
#121375=CARTESIAN_POINT('Ctrl Pts',(16.5291383294904,-20.7663927039858,
-21.8303756371117));
#121376=CARTESIAN_POINT('Ctrl Pts',(16.0189811599981,-18.0766910961744,
-21.9575514437931));
#121377=CARTESIAN_POINT('Ctrl Pts',(17.3340241084075,-16.8284618958069,
-22.0423353149141));
#121378=CARTESIAN_POINT('Ctrl Pts',(18.110196795177,-16.6207694362802,-22.0847272504745));
#121379=CARTESIAN_POINT('Ctrl Pts',(20.694689575575,-17.3009161652768,0.2577132765471));
#121380=CARTESIAN_POINT('Ctrl Pts',(21.2446793089921,-17.9539921042784,
0.215302684966073));
#121381=CARTESIAN_POINT('Ctrl Pts',(21.6307190240803,-19.8413750741844,
0.130500157824568));
#121382=CARTESIAN_POINT('Ctrl Pts',(19.5498582244566,-21.8731458956047,
0.00330569512258449));
#121383=CARTESIAN_POINT('Ctrl Pts',(16.721234265284,-21.2170658268692,-0.123870111558849));
#121384=CARTESIAN_POINT('Ctrl Pts',(15.7390230077546,-18.486705288049,-0.251045918240284));
#121385=CARTESIAN_POINT('Ctrl Pts',(17.504602873543,-16.1812802725366,-0.378221724921718));
#121386=CARTESIAN_POINT('Ctrl Pts',(20.3980344041213,-16.4188256061598,
-0.505397531603153));
#121387=CARTESIAN_POINT('Ctrl Pts',(21.7648403751927,-18.9798787515055,
-0.632573338284587));
#121388=CARTESIAN_POINT('Ctrl Pts',(20.3510266283393,-21.5156260340964,
-0.759749144966022));
#121389=CARTESIAN_POINT('Ctrl Pts',(17.4536974322035,-21.6992648057414,
-0.886924951647455));
#121390=CARTESIAN_POINT('Ctrl Pts',(15.7309632019515,-19.3625316825741,
-1.01410075832889));
#121391=CARTESIAN_POINT('Ctrl Pts',(16.7633304926413,-16.6491233053535,
-1.14127656501032));
#121392=CARTESIAN_POINT('Ctrl Pts',(19.6036638873005,-16.0484810425805,
-1.26845237169176));
#121393=CARTESIAN_POINT('Ctrl Pts',(21.6461350868215,-18.1116269959678,
-1.39562817837319));
#121394=CARTESIAN_POINT('Ctrl Pts',(21.016902861202,-20.9457683228794,-1.52280398505463));
#121395=CARTESIAN_POINT('Ctrl Pts',(18.2932490729839,-21.9507482089492,
-1.64997979173606));
#121396=CARTESIAN_POINT('Ctrl Pts',(15.9739568421265,-20.2045641649137,
-1.7771555984175));
#121397=CARTESIAN_POINT('Ctrl Pts',(16.1868329332462,-17.3092295011259,
-1.90433140509893));
#121398=CARTESIAN_POINT('Ctrl Pts',(18.7365766963677,-15.9210351930051,
-2.03150721178036));
#121399=CARTESIAN_POINT('Ctrl Pts',(21.2839565091815,-17.3135627726908,
-2.1586830184618));
#121400=CARTESIAN_POINT('Ctrl Pts',(21.4919094884653,-20.2092549192115,
-2.28585882514323));
#121401=CARTESIAN_POINT('Ctrl Pts',(19.1696516895889,-21.951493657592,-2.41303463182467));
#121402=CARTESIAN_POINT('Ctrl Pts',(16.447710503894,-20.9418831626308,-2.5402104385061));
#121403=CARTESIAN_POINT('Ctrl Pts',(15.8232980283766,-18.1066783575389,
-2.66738624518754));
#121404=CARTESIAN_POINT('Ctrl Pts',(17.8692739529578,-16.0470037003502,
-2.79456205186897));
#121405=CARTESIAN_POINT('Ctrl Pts',(20.7085823549184,-16.6524828397803,
-2.9217378585504));
#121406=CARTESIAN_POINT('Ctrl Pts',(21.7363340025561,-19.3676262516076,
-3.04891366523184));
#121407=CARTESIAN_POINT('Ctrl Pts',(20.0096305487582,-21.7014583732073,
-3.17608947191327));
#121408=CARTESIAN_POINT('Ctrl Pts',(17.1126152410121,-21.5128330885679,
-3.30326527859471));
#121409=CARTESIAN_POINT('Ctrl Pts',(15.703119815162,-18.9748023881108,-3.43044108527614));
#121410=CARTESIAN_POINT('Ctrl Pts',(17.0742688412544,-16.4158519119851,
-3.55761689195758));
#121411=CARTESIAN_POINT('Ctrl Pts',(19.9681181909656,-16.1836598954335,
-3.68479269863901));
#121412=CARTESIAN_POINT('Ctrl Pts',(21.7297406984776,-18.4912481022967,
-3.81196850532045));
#121413=CARTESIAN_POINT('Ctrl Pts',(20.7429570517748,-21.221547577794,-3.93914431200188));
#121414=CARTESIAN_POINT('Ctrl Pts',(17.9130800000052,-21.8696780146852,
-4.06632011868332));
#121415=CARTESIAN_POINT('Ctrl Pts',(15.8363460961894,-19.8410199646181,
-4.19349592536474));
#121416=CARTESIAN_POINT('Ctrl Pts',(16.4180298004353,-16.9967412758189,
-4.32067173204619));
#121417=CARTESIAN_POINT('Ctrl Pts',(19.1244724174598,-15.9462911094113,
-4.44784753872761));
#121418=CARTESIAN_POINT('Ctrl Pts',(21.4726808269163,-17.6533922947864,
-4.57502334540905));
#121419=CARTESIAN_POINT('Ctrl Pts',(21.3083195593796,-20.5518854490104,
-4.70219915209049));
#121420=CARTESIAN_POINT('Ctrl Pts',(18.7821798764038,-21.9825830038574,
-4.82937495877192));
#121421=CARTESIAN_POINT('Ctrl Pts',(16.2118381472079,-20.6329087518601,
-4.95655076545335));
#121422=CARTESIAN_POINT('Ctrl Pts',(15.9554233749293,-17.7411050489944,
-5.08372657213479));
#121423=CARTESIAN_POINT('Ctrl Pts',(18.2481801982382,-15.9602223070596,
-5.21090237881622));
#121424=CARTESIAN_POINT('Ctrl Pts',(20.9866465362858,-16.9241099077319,
-5.33807818549766));
#121425=CARTESIAN_POINT('Ctrl Pts',(21.6584494923035,-19.7484608030061,
-5.46525399217908));
#121426=CARTESIAN_POINT('Ctrl Pts',(19.6472515509388,-21.8421083454547,
-5.59242979886053));
#121427=CARTESIAN_POINT('Ctrl Pts',(16.7982019943716,-21.2842608613028,
-5.71960560554195));
#121428=CARTESIAN_POINT('Ctrl Pts',(15.7251269587939,-18.5867087933401,
-5.8467814122234));
#121429=CARTESIAN_POINT('Ctrl Pts',(17.4125061868001,-16.2242887349586,
-5.97395721890483));
#121430=CARTESIAN_POINT('Ctrl Pts',(20.3122739672608,-16.3643744613978,
-6.10113302558626));
#121431=CARTESIAN_POINT('Ctrl Pts',(21.7640733414898,-18.8784460133507,
-6.2283088322677));
#121432=CARTESIAN_POINT('Ctrl Pts',(20.4359684924635,-21.459998782779,-6.35548463894913));
#121433=CARTESIAN_POINT('Ctrl Pts',(17.54641318768,-21.7406183329676,-6.48266044563057));
#121434=CARTESIAN_POINT('Ctrl Pts',(15.7463950732497,-19.4628536438322,
-6.609836252312));
#121435=CARTESIAN_POINT('Ctrl Pts',(16.687319047438,-16.7164124436336,-6.73701205899344));
#121436=CARTESIAN_POINT('Ctrl Pts',(19.5059457642557,-16.0209840701888,
-6.86418786567487));
#121437=CARTESIAN_POINT('Ctrl Pts',(21.6163601547263,-18.0145808929804,
-6.99136367235631));
#121438=CARTESIAN_POINT('Ctrl Pts',(21.0823880026828,-20.8682015636709,
-7.11853947903774));
#121439=CARTESIAN_POINT('Ctrl Pts',(18.3939156155756,-21.9638262325755,
-7.24571528571917));
#121440=CARTESIAN_POINT('Ctrl Pts',(16.0174495431603,-20.2962872681105,
-7.37289109240061));
#121441=CARTESIAN_POINT('Ctrl Pts',(16.1332499067586,-17.3954481710316,
-7.50006689908204));
#121442=CARTESIAN_POINT('Ctrl Pts',(18.6350770601501,-15.9226487665292,
-7.62724270576348));
#121443=CARTESIAN_POINT('Ctrl Pts',(21.2276598710039,-17.2290910959936,
-7.75441851244491));
#121444=CARTESIAN_POINT('Ctrl Pts',(21.5324645241983,-20.1161954090971,
-7.88159431912634));
#121445=CARTESIAN_POINT('Ctrl Pts',(19.2698516687381,-21.9352226924704,
-8.00877012580778));
#121446=CARTESIAN_POINT('Ctrl Pts',(16.515628165916,-21.0173283151844,-8.13594593248921));
#121447=CARTESIAN_POINT('Ctrl Pts',(15.7966231331817,-18.204623397449,-8.26312173917066));
#121448=CARTESIAN_POINT('Ctrl Pts',(17.7724790615836,-16.0775901251306,
-8.39029754585207));
#121449=CARTESIAN_POINT('Ctrl Pts',(20.6304707722626,-16.5876495070077,
-8.51747335253352));
#121450=CARTESIAN_POINT('Ctrl Pts',(21.7485682576417,-19.2668537180634,
-8.64464915921495));
#121451=CARTESIAN_POINT('Ctrl Pts',(20.1009864718422,-21.6571991848217,
-8.77182496589638));
#121452=CARTESIAN_POINT('Ctrl Pts',(17.1992794428765,-21.5656923031035,
-8.89900077257782));
#121453=CARTESIAN_POINT('Ctrl Pts',(15.7055832695711,-19.0762849573276,
-9.02617657925925));
#121454=CARTESIAN_POINT('Ctrl Pts',(16.9902714816934,-16.4728538771981,
-9.15335238594069));
#121455=CARTESIAN_POINT('Ctrl Pts',(19.8747223813643,-16.1438854915773,
-9.28052819262213));
#121456=CARTESIAN_POINT('Ctrl Pts',(21.7126312973492,-18.3911878761916,
-9.40770399930354));
#121457=CARTESIAN_POINT('Ctrl Pts',(20.8178308727247,-21.1530005764741,
-9.53487980598501));
#121458=CARTESIAN_POINT('Ctrl Pts',(18.0112449595055,-21.8955318573441,
-9.66205561266641));
#121459=CARTESIAN_POINT('Ctrl Pts',(15.8677419367031,-19.9375553552922,
-9.78923141934787));
#121460=CARTESIAN_POINT('Ctrl Pts',(16.3538527869367,-17.0753929852239,
-9.91640722602929));
#121461=CARTESIAN_POINT('Ctrl Pts',(19.0236009765592,-15.9349010758452,
-10.0435830327107));
#121462=CARTESIAN_POINT('Ctrl Pts',(21.4276582448523,-17.5624101671002,
-10.1707588393921));
#121463=CARTESIAN_POINT('Ctrl Pts',(21.3604512607793,-20.4647816823687,
-10.2979346460736));
#121464=CARTESIAN_POINT('Ctrl Pts',(18.8836382608913,-21.9792698978844,
-10.4251104527551));
#121465=CARTESIAN_POINT('Ctrl Pts',(16.2695414442334,-20.7164258756515,
-10.5522862594364));
#121466=CARTESIAN_POINT('Ctrl Pts',(15.9164323909425,-17.8348306251289,
-10.6794620661178));
#121467=CARTESIAN_POINT('Ctrl Pts',(18.1482667409934,-15.9781689366991,
-10.8066378727993));
#121468=CARTESIAN_POINT('Ctrl Pts',(20.9174750014767,-16.8498126720757,
-10.9338136794807));
#121469=CARTESIAN_POINT('Ctrl Pts',(21.6834804698477,-19.6500828043623,
-11.0609894861622));
#121470=CARTESIAN_POINT('Ctrl Pts',(19.7435206725372,-21.8099052915517,
-11.1881652928436));
#121471=CARTESIAN_POINT('Ctrl Pts',(16.8773883160933,-21.3477770553498,
-11.315341099525));
#121472=CARTESIAN_POINT('Ctrl Pts',(15.7145819453165,-18.6876720695586,
-11.4425169062064));
#121473=CARTESIAN_POINT('Ctrl Pts',(17.321904233492,-16.2700715539058,-11.5696927128879));
#121474=CARTESIAN_POINT('Ctrl Pts',(20.2247367428907,-16.3129739282918,
-11.6968685195694));
#121475=CARTESIAN_POINT('Ctrl Pts',(21.7599108162444,-18.7770189270394,
-11.8240443262508));
#121476=CARTESIAN_POINT('Ctrl Pts',(20.5189995249,-21.401598199678,-11.9512201329322));
#121477=CARTESIAN_POINT('Ctrl Pts',(17.6404619590251,-21.7788231633232,
-12.0783959396136));
#121478=CARTESIAN_POINT('Ctrl Pts',(15.7651776731192,-19.5626133270521,
-12.2055717462951));
#121479=CARTESIAN_POINT('Ctrl Pts',(16.6136036062314,-16.7862036621481,
-12.3327475529765));
#121480=CARTESIAN_POINT('Ctrl Pts',(19.4073616239837,-15.9967777127422,
-12.4599233596579));
#121481=CARTESIAN_POINT('Ctrl Pts',(21.5833521452667,-17.9185847901141,
-12.5870991663394));
#121482=CARTESIAN_POINT('Ctrl Pts',(21.1452389240066,-20.7884861815747,
-12.7142749730208));
#121483=CARTESIAN_POINT('Ctrl Pts',(18.4949636483364,-21.973525486628,-12.8414507797022));
#121484=CARTESIAN_POINT('Ctrl Pts',(16.0639893890483,-20.3865026947222,
-12.9686265863837));
#121485=CARTESIAN_POINT('Ctrl Pts',(16.0825841457601,-17.4834127156872,
-13.0958023930651));
#121486=CARTESIAN_POINT('Ctrl Pts',(18.5336883833095,-15.9276604192025,
-13.2229781997465));
#121487=CARTESIAN_POINT('Ctrl Pts',(21.1685660964313,-17.1465519764151,
-13.350154006428));
#121488=CARTESIAN_POINT('Ctrl Pts',(21.5698805222909,-20.0218300365248,
-13.4773298131094));
#121489=CARTESIAN_POINT('Ctrl Pts',(19.3694505835445,-21.9156054392635,
-13.6045056197909));
#121490=CARTESIAN_POINT('Ctrl Pts',(16.5860341749072,-21.0904567935765,
-13.7316814264723));
#121491=CARTESIAN_POINT('Ctrl Pts',(15.773243092998,-18.3034067673804,-13.8588572331537));
#121492=CARTESIAN_POINT('Ctrl Pts',(17.6767627079645,-16.1114007758768,
-13.9860330398351));
#121493=CARTESIAN_POINT('Ctrl Pts',(20.5502319188267,-16.5254682650346,
-14.1132088465166));
#121494=CARTESIAN_POINT('Ctrl Pts',(21.7574210722316,-19.1657280134782,
-14.240384653198));
#121495=CARTESIAN_POINT('Ctrl Pts',(20.1908090465392,-21.6099055750122,
-14.3675604598796));
#121496=CARTESIAN_POINT('Ctrl Pts',(17.2876651404139,-21.6156197396974,
-14.4947362665609));
#121497=CARTESIAN_POINT('Ctrl Pts',(15.7114436982933,-19.1776281160963,
-14.6219120732423));
#121498=CARTESIAN_POINT('Ctrl Pts',(16.9082300619871,-16.5326367000369,
-14.7490878799237));
#121499=CARTESIAN_POINT('Ctrl Pts',(19.7800470237451,-16.1072609490722,
-14.8762636866052));
#121500=CARTESIAN_POINT('Ctrl Pts',(21.6921807662175,-18.2917567129154,
-15.0034394932866));
#121501=CARTESIAN_POINT('Ctrl Pts',(20.8903672610905,-21.0819847133387,
-15.130615299968));
#121502=CARTESIAN_POINT('Ctrl Pts',(18.1102206331594,-21.9180839410347,
-15.2577911066495));
#121503=CARTESIAN_POINT('Ctrl Pts',(15.9023528581907,-20.0329852487628,
-15.3849669133309));
#121504=CARTESIAN_POINT('Ctrl Pts',(16.2923455839892,-17.1561496842624,
-15.5121427200123));
#121505=CARTESIAN_POINT('Ctrl Pts',(18.9224046903134,-15.9268953214099,
-15.6393185266939));
#121506=CARTESIAN_POINT('Ctrl Pts',(21.3796141869889,-17.4729867419922,
-15.7664943333752));
#121507=CARTESIAN_POINT('Ctrl Pts',(21.4096368724374,-20.375981028881,-15.8936701400568));
#121508=CARTESIAN_POINT('Ctrl Pts',(18.9849287961779,-21.9725611040017,
-16.0208459467382));
#121509=CARTESIAN_POINT('Ctrl Pts',(16.3300091238228,-20.7979638433666,
-16.1480217534195));
#121510=CARTESIAN_POINT('Ctrl Pts',(15.8806018718589,-17.9298093298801,
-16.2751975601011));
#121511=CARTESIAN_POINT('Ctrl Pts',(18.0490103006032,-15.9994513119205,
-16.4023733667824));
#121512=CARTESIAN_POINT('Ctrl Pts',(20.8458542632885,-16.7778734594348,
-16.5295491734638));
#121513=CARTESIAN_POINT('Ctrl Pts',(21.7052030158649,-19.5509217664061,
-16.6567249801453));
#121514=CARTESIAN_POINT('Ctrl Pts',(19.8386574150423,-21.7744965259768,
-16.7839007868268));
#121515=CARTESIAN_POINT('Ctrl Pts',(16.9586571986901,-21.4086059068554,
-16.9110765935081));
#121516=CARTESIAN_POINT('Ctrl Pts',(15.7074238123383,-18.7889318423525,
-17.0382524001897));
#121517=CARTESIAN_POINT('Ctrl Pts',(17.2328862276622,-16.31886269134,-17.165428206871));
#121518=CARTESIAN_POINT('Ctrl Pts',(20.135527359478,-16.2645335900898,-17.2926040135526));
#121519=CARTESIAN_POINT('Ctrl Pts',(21.7523541275707,-18.6757881169556,
-17.4197798202338));
#121520=CARTESIAN_POINT('Ctrl Pts',(20.6000283238032,-21.3404499028704,
-17.5469556269153));
#121521=CARTESIAN_POINT('Ctrl Pts',(17.7357373517245,-21.8138571468239,
-17.6741314335968));
#121522=CARTESIAN_POINT('Ctrl Pts',(15.7872904002738,-19.6616880854488,
-17.8013072402782));
#121523=CARTESIAN_POINT('Ctrl Pts',(16.5422666131419,-16.8584242538938,
-17.9284830469596));
#121524=CARTESIAN_POINT('Ctrl Pts',(19.3080221741474,-15.9758862274083,
-18.055658853641));
#121525=CARTESIAN_POINT('Ctrl Pts',(21.5471480181857,-17.8237478688561,
-18.1828346603226));
#121526=CARTESIAN_POINT('Ctrl Pts',(21.2053851592371,-20.7067108133391,
-18.3100104670039));
#121527=CARTESIAN_POINT('Ctrl Pts',(18.5962798080717,-21.9798354963434,
-18.4371862736854));
#121528=CARTESIAN_POINT('Ctrl Pts',(16.1135241852737,-20.4751090398787,
-18.5643620803668));
#121529=CARTESIAN_POINT('Ctrl Pts',(16.0348924771216,-17.5730245745949,
-18.6915378870482));
#121530=CARTESIAN_POINT('Ctrl Pts',(18.4325243962693,-15.9360644723642,
-18.8187136937296));
#121531=CARTESIAN_POINT('Ctrl Pts',(21.1067414690649,-17.0660380283814,
-18.9458895004112));
#121532=CARTESIAN_POINT('Ctrl Pts',(21.6041155150354,-19.9262646340588,
-19.0730653070925));
#121533=CARTESIAN_POINT('Ctrl Pts',(19.4683367113789,-21.8926639140248,
-19.2002411137739));
#121534=CARTESIAN_POINT('Ctrl Pts',(16.6588495608948,-21.1611865588169,
-19.3274169204554));
#121535=CARTESIAN_POINT('Ctrl Pts',(15.7531841249269,-18.4029176770636,
-19.4545927271368));
#121536=CARTESIAN_POINT('Ctrl Pts',(17.582232272941,-16.148397701268,-19.5817685338183));
#121537=CARTESIAN_POINT('Ctrl Pts',(20.4679557680829,-16.4660089109295,
-19.7089443404997));
#121538=CARTESIAN_POINT('Ctrl Pts',(21.762882574719,-19.0643624781199,-19.8361201471812));
#121539=CARTESIAN_POINT('Ctrl Pts',(20.278997406019,-21.5596307706316,-19.9632959538626));
#121540=CARTESIAN_POINT('Ctrl Pts',(17.3776734088588,-21.662559052761,-20.0904717605441));
#121541=CARTESIAN_POINT('Ctrl Pts',(15.7206941087448,-19.2787188466078,
-20.2176475672255));
#121542=CARTESIAN_POINT('Ctrl Pts',(16.828237415124,-16.5951320529376,-20.3448233739069));
#121543=CARTESIAN_POINT('Ctrl Pts',(19.6841967603538,-16.0738297948901,
-20.4719991805884));
#121544=CARTESIAN_POINT('Ctrl Pts',(21.6684150405127,-18.1930614333217,
-20.5991749872697));
#121545=CARTESIAN_POINT('Ctrl Pts',(20.9604790804735,-21.0085887233582,
-20.7263507939513));
#121546=CARTESIAN_POINT('Ctrl Pts',(18.2099071212035,-21.9372914819773,
-20.8535266006326));
#121547=CARTESIAN_POINT('Ctrl Pts',(15.9401186110067,-20.1272362927054,
-20.980702407314));
#121548=CARTESIAN_POINT('Ctrl Pts',(16.2336184655874,-17.2388558767421,
-21.1078782139955));
#121549=CARTESIAN_POINT('Ctrl Pts',(18.8209175351634,-15.9224078905259,
-21.2350540206769));
#121550=CARTESIAN_POINT('Ctrl Pts',(21.3287557911663,-17.3849813380486,
-21.3622298273583));
#121551=CARTESIAN_POINT('Ctrl Pts',(21.4555258683986,-20.286047713047,-21.4894056340398));
#121552=CARTESIAN_POINT('Ctrl Pts',(19.0865078830173,-21.9615659646048,
-21.6165814407212));
#121553=CARTESIAN_POINT('Ctrl Pts',(16.3920659006521,-20.879190353892,-21.7437572474027));
#121554=CARTESIAN_POINT('Ctrl Pts',(15.8501931440795,-18.0222746586101,
-21.8709330540841));
#121555=CARTESIAN_POINT('Ctrl Pts',(17.2469900335074,-16.6964452121458,
-21.9557169252051));
#121556=CARTESIAN_POINT('Ctrl Pts',(18.0714160310384,-16.4758408723594,
-21.9981088607656));
#121557=CARTESIAN_POINT('Ctrl Pts',(20.3539256943887,-17.5890877707427,
0.));
#121558=CARTESIAN_POINT('Ctrl Pts',(20.4076089239479,-17.6408883813468,
-1.14883615034368E-14));
#121559=CARTESIAN_POINT('Ctrl Pts',(20.458135595812,-17.6955615793788,-3.45732861075315E-15));
#121560=CARTESIAN_POINT('Ctrl Pts',(20.505511977026,-17.7527360595703,-3.1641356201817E-15));
#121561=CARTESIAN_POINT('Ctrl Pts',(20.554575660781,-17.811946800093,-2.86050060627935E-15));
#121562=CARTESIAN_POINT('Ctrl Pts',(20.6002611686399,-17.8738405959818,
-1.28830115027514E-14));
#121563=CARTESIAN_POINT('Ctrl Pts',(20.6425471220964,-17.938054648476,-1.24275589818978E-14));
#121564=CARTESIAN_POINT('Ctrl Pts',(20.6826816235517,-17.9990015770096,
-1.19952792680244E-14));
#121565=CARTESIAN_POINT('Ctrl Pts',(20.7197537535955,-18.0620396014581,
-1.56156834274937E-14));
#121566=CARTESIAN_POINT('Ctrl Pts',(20.7537167666138,-18.1268912820608,
-3.64291929955129E-15));
#121567=CARTESIAN_POINT('Ctrl Pts',(20.7688150878339,-18.1557212184648,
1.86923291261623E-15));
#121568=CARTESIAN_POINT('Ctrl Pts',(20.7832985724702,-18.1849099468526,
1.07609079391212E-16));
#121569=CARTESIAN_POINT('Ctrl Pts',(20.7971611207678,-18.2144346312911,
4.69763117294519E-15));
#121570=CARTESIAN_POINT('Ctrl Pts',(20.8057380545325,-18.2327019265545,
7.27018219478905E-15));
#121571=CARTESIAN_POINT('Ctrl Pts',(20.8140776656103,-18.2510987616938,
-4.62727264044915E-15));
#121572=CARTESIAN_POINT('Ctrl Pts',(20.8221770088969,-18.269617013417,-1.43565714871841E-14));
#121573=CARTESIAN_POINT('Ctrl Pts',(20.8264660877165,-18.2794235172817,
-1.95088076791796E-14));
#121574=CARTESIAN_POINT('Ctrl Pts',(20.8306870781385,-18.2892625308288,
-2.33904285261234E-14));
#121575=CARTESIAN_POINT('Ctrl Pts',(20.8348368140281,-18.2991258749815,
-2.39808173319034E-14));
#121576=CARTESIAN_POINT('Ctrl Pts',(20.8659056770803,-18.372972234574,-2.9180491333638E-14));
#121577=CARTESIAN_POINT('Ctrl Pts',(20.8930393303568,-18.4483069573626,
-1.39833664931511E-14));
#121578=CARTESIAN_POINT('Ctrl Pts',(20.9162161420459,-18.5247489058203,
-2.07472927726826E-14));
#121579=CARTESIAN_POINT('Ctrl Pts',(20.9398193164084,-18.6025970871087,
-2.76356488370442E-14));
#121580=CARTESIAN_POINT('Ctrl Pts',(20.9593192432917,-18.681594415105,7.90483084619676E-15));
#121581=CARTESIAN_POINT('Ctrl Pts',(20.9746521798118,-18.7613738906752,
-2.84494650060196E-15));
#121582=CARTESIAN_POINT('Ctrl Pts',(20.9885844406084,-18.8338654488586,
-1.26127232931092E-14));
#121583=CARTESIAN_POINT('Ctrl Pts',(20.9990759862006,-18.9070037360463,
-7.2353415164223E-15));
#121584=CARTESIAN_POINT('Ctrl Pts',(21.0060452061984,-18.9805292501327,
-6.82787160144471E-15));
#121585=CARTESIAN_POINT('Ctrl Pts',(21.0087031403799,-19.0085705484655,
-6.66025088122286E-15));
#121586=CARTESIAN_POINT('Ctrl Pts',(21.0108483899423,-19.0366682762212,
-1.4471649499982E-15));
#121587=CARTESIAN_POINT('Ctrl Pts',(21.0124750673575,-19.0648083237754,
-9.10382880192628E-15));
#121588=CARTESIAN_POINT('Ctrl Pts',(21.0133685834701,-19.0802653441188,
-1.32692796682525E-14));
#121589=CARTESIAN_POINT('Ctrl Pts',(21.014105623128,-19.0957351348357,-1.68888790667805E-14));
#121590=CARTESIAN_POINT('Ctrl Pts',(21.0146851084115,-19.1112153648711,
3.7470027081099E-15));
#121591=CARTESIAN_POINT('Ctrl Pts',(21.0151328224698,-19.1231754901941,
2.01287399453959E-14));
#121592=CARTESIAN_POINT('Ctrl Pts',(21.0154863189935,-19.1351385470168,
-5.6262880174693E-15));
#121593=CARTESIAN_POINT('Ctrl Pts',(21.0157451770828,-19.1470949182306,
-6.38378239159465E-15));
#121594=CARTESIAN_POINT('Ctrl Pts',(21.0175519249061,-19.2305466184455,
-1.17840328135284E-14));
#121595=CARTESIAN_POINT('Ctrl Pts',(21.0147568373932,-19.3137920798114,
1.49690073973068E-14));
#121596=CARTESIAN_POINT('Ctrl Pts',(21.0073036695044,-19.3964506692726,
1.12271303365219E-14));
#121597=CARTESIAN_POINT('Ctrl Pts',(20.9998648261745,-19.4789503936919,
7.57364944833593E-15));
#121598=CARTESIAN_POINT('Ctrl Pts',(20.9877861648147,-19.5608665038776,
8.08948018227706E-15));
#121599=CARTESIAN_POINT('Ctrl Pts',(20.9709624036051,-19.6418361818354,
1.15740750317173E-14));
#121600=CARTESIAN_POINT('Ctrl Pts',(20.9545246825771,-19.7209479191819,
1.49539710127781E-14));
#121601=CARTESIAN_POINT('Ctrl Pts',(20.9335573448041,-19.799157111958,8.98046188800277E-15));
#121602=CARTESIAN_POINT('Ctrl Pts',(20.9083260528412,-19.8762372781696,
1.75970349403087E-14));
#121603=CARTESIAN_POINT('Ctrl Pts',(20.8979286223519,-19.9080008387303,
2.11190768885281E-14));
#121604=CARTESIAN_POINT('Ctrl Pts',(20.886806496403,-19.9395726045308,6.78433755510298E-15));
#121605=CARTESIAN_POINT('Ctrl Pts',(20.8749757808311,-19.9709362516545,
-5.4678483962789E-15));
#121606=CARTESIAN_POINT('Ctrl Pts',(20.8684245113494,-19.9883038997047,
-1.2315661009052E-14));
#121607=CARTESIAN_POINT('Ctrl Pts',(20.8616537141196,-20.0056128698145,
8.27179597674389E-15));
#121608=CARTESIAN_POINT('Ctrl Pts',(20.8546785166995,-20.0228303119358,
5.07927033766009E-15));
#121609=CARTESIAN_POINT('Ctrl Pts',(20.8236218670382,-20.0994899440325,
-8.89802862727266E-15));
#121610=CARTESIAN_POINT('Ctrl Pts',(20.7884837604207,-20.1744320701159,
-3.12356070928148E-15));
#121611=CARTESIAN_POINT('Ctrl Pts',(20.7495952387339,-20.2474309568179,
-1.0325074129014E-14));
#121612=CARTESIAN_POINT('Ctrl Pts',(20.7099066604842,-20.321931655259,-1.76747448410191E-14));
#121613=CARTESIAN_POINT('Ctrl Pts',(20.6663114480309,-20.3944090798955,
1.85848361403515E-14));
#121614=CARTESIAN_POINT('Ctrl Pts',(20.6191066061262,-20.4646182429904,
4.49640324973188E-15));
#121615=CARTESIAN_POINT('Ctrl Pts',(20.5711286079629,-20.5359773443472,
-9.82278054742002E-15));
#121616=CARTESIAN_POINT('Ctrl Pts',(20.5194213554741,-20.6049941328796,
-2.55515037437809E-15));
#121617=CARTESIAN_POINT('Ctrl Pts',(20.4642461984827,-20.6713939738053,
2.77555756156289E-15));
#121618=CARTESIAN_POINT('Ctrl Pts',(20.4403643182492,-20.7001343188262,
5.08288816881304E-15));
#121619=CARTESIAN_POINT('Ctrl Pts',(20.4158321356568,-20.7283840869166,
6.72524383598771E-15));
#121620=CARTESIAN_POINT('Ctrl Pts',(20.3906682941055,-20.7561193805442,
3.1641356201817E-15));
#121621=CARTESIAN_POINT('Ctrl Pts',(20.3815365270621,-20.7661843080224,
1.76576788124933E-15));
#121622=CARTESIAN_POINT('Ctrl Pts',(20.3723208078371,-20.7761822779911,
-4.33283550333587E-16));
#121623=CARTESIAN_POINT('Ctrl Pts',(20.3630243316464,-20.7861096027615,
1.94289029309402E-16));
#121624=CARTESIAN_POINT('Ctrl Pts',(20.3025147033051,-20.8507253474758,
4.82486799989442E-15));
#121625=CARTESIAN_POINT('Ctrl Pts',(20.2387852854453,-20.9121400047012,
1.82120019294766E-14));
#121626=CARTESIAN_POINT('Ctrl Pts',(20.1721441659295,-20.9700792099884,
2.01505478969466E-14));
#121627=CARTESIAN_POINT('Ctrl Pts',(20.1169512585411,-21.0180650964023,
2.17560729665775E-14));
#121628=CARTESIAN_POINT('Ctrl Pts',(20.0597599950038,-21.0636670219304,
1.76866719771448E-14));
#121629=CARTESIAN_POINT('Ctrl Pts',(20.0007222397457,-21.1067151539364,
1.05748743095546E-14));
#121630=CARTESIAN_POINT('Ctrl Pts',(19.9812253420094,-21.1209315655156,
8.41816628900994E-15));
#121631=CARTESIAN_POINT('Ctrl Pts',(19.9615269106471,-21.1348693297411,
-1.5795805565849E-14));
#121632=CARTESIAN_POINT('Ctrl Pts',(19.941631987048,-21.1485219218181,-5.80091530366644E-15));
#121633=CARTESIAN_POINT('Ctrl Pts',(19.9257068710437,-21.1594502931437,
2.07770478644972E-15));
#121634=CARTESIAN_POINT('Ctrl Pts',(19.9096544895287,-21.170196697329,1.40562940309176E-14));
#121635=CARTESIAN_POINT('Ctrl Pts',(19.8934933729568,-21.1807476067171,
1.42941214420489E-14));
#121636=CARTESIAN_POINT('Ctrl Pts',(19.8189655561075,-21.2294036657816,
1.49872222632139E-14));
#121637=CARTESIAN_POINT('Ctrl Pts',(19.7420556060774,-21.2739560343907,
1.33704818268334E-14));
#121638=CARTESIAN_POINT('Ctrl Pts',(19.6630443896218,-21.3141141071315,
1.13797860024079E-14));
#121639=CARTESIAN_POINT('Ctrl Pts',(19.585203146919,-21.3536775315023,9.81319007009315E-15));
#121640=CARTESIAN_POINT('Ctrl Pts',(19.5053217267533,-21.3889765584864,
2.19043743988934E-14));
#121641=CARTESIAN_POINT('Ctrl Pts',(19.4236362626317,-21.4196959407397,
5.55111512312578E-17));
#121642=CARTESIAN_POINT('Ctrl Pts',(19.4149414973774,-21.4229657736325,
-2.15692061228505E-15));
#121643=CARTESIAN_POINT('Ctrl Pts',(19.4062262673531,-21.4261836782215,
3.67808051293056E-14));
#121644=CARTESIAN_POINT('Ctrl Pts',(19.3974909880357,-21.4293497847436,
2.33146835171283E-15));
#121645=CARTESIAN_POINT('Ctrl Pts',(18.0714161019496,-21.428158862637,-0.00189098085166848));
#121646=CARTESIAN_POINT('Ctrl Pts',(17.2469901926503,-21.2075545464601,
-0.0442829164121466));
#121647=CARTESIAN_POINT('Ctrl Pts',(15.8501939821074,-19.8817220316731,
-0.129066787533102));
#121648=CARTESIAN_POINT('Ctrl Pts',(16.3920656827787,-17.0248116182672,
-0.256242594214537));
#121649=CARTESIAN_POINT('Ctrl Pts',(19.0865079334355,-15.9424330181619,
-0.38341840089597));
#121650=CARTESIAN_POINT('Ctrl Pts',(21.4555257912919,-17.6179530146914,
-0.510594207577405));
#121651=CARTESIAN_POINT('Ctrl Pts',(21.3287556480917,-20.5190182015967,
-0.63777001425884));
#121652=CARTESIAN_POINT('Ctrl Pts',(18.8209175719769,-21.9815922294721,
-0.764945820940274));
#121653=CARTESIAN_POINT('Ctrl Pts',(16.2336185304982,-20.6651439233068,
-0.892121627621709));
#121654=CARTESIAN_POINT('Ctrl Pts',(15.9401187363004,-17.7767638289518,
-1.01929743430314));
#121655=CARTESIAN_POINT('Ctrl Pts',(18.2099071283678,-15.9667085869429,
-1.14647324098458));
#121656=CARTESIAN_POINT('Ctrl Pts',(20.9604790041794,-16.8954113789202,
-1.27364904766601));
#121657=CARTESIAN_POINT('Ctrl Pts',(21.6684149250656,-19.7109385242504,
-1.40082485434745));
#121658=CARTESIAN_POINT('Ctrl Pts',(19.6841967272255,-21.8301701041092,
-1.52800066102888));
#121659=CARTESIAN_POINT('Ctrl Pts',(16.8282374854801,-21.3088678538367,
-1.65517646771032));
#121660=CARTESIAN_POINT('Ctrl Pts',(15.720694223426,-18.6252811680681,-1.78235227439175));
#121661=CARTESIAN_POINT('Ctrl Pts',(17.3776734595451,-16.2414410482877,
-1.90952808107318));
#121662=CARTESIAN_POINT('Ctrl Pts',(20.2789973479827,-16.3443693285228,
-2.03670388775462));
#121663=CARTESIAN_POINT('Ctrl Pts',(21.7628824602007,-18.839637525737,-2.16387969443605));
#121664=CARTESIAN_POINT('Ctrl Pts',(20.4679557027106,-21.4379909954235,
-2.29105550111749));
#121665=CARTESIAN_POINT('Ctrl Pts',(17.5822323163742,-21.7556021927696,
-2.41823130779892));
#121666=CARTESIAN_POINT('Ctrl Pts',(15.7531842374939,-19.5010823022681,
-2.54540711448036));
#121667=CARTESIAN_POINT('Ctrl Pts',(16.6588496392251,-16.7428135245559,
-2.67258292116179));
#121668=CARTESIAN_POINT('Ctrl Pts',(19.468336683663,-16.0113361970163,-2.79975872784322));
#121669=CARTESIAN_POINT('Ctrl Pts',(21.6041154066714,-17.977735402714,-2.92693453452466));
#121670=CARTESIAN_POINT('Ctrl Pts',(21.1067413794861,-20.8379619004206,
-3.05411034120609));
#121671=CARTESIAN_POINT('Ctrl Pts',(18.43252440765,-21.9679354137682,-3.18128614788753));
#121672=CARTESIAN_POINT('Ctrl Pts',(16.0348925790254,-20.3309753733442,
-3.30846195456896));
#121673=CARTESIAN_POINT('Ctrl Pts',(16.1135242842076,-17.4288910176245,
-3.43563776125039));
#121674=CARTESIAN_POINT('Ctrl Pts',(18.5962798132715,-15.924164617971,-3.56281356793183));
#121675=CARTESIAN_POINT('Ctrl Pts',(21.2053850659314,-17.1972892529086,
-3.68998937461327));
#121676=CARTESIAN_POINT('Ctrl Pts',(21.5471479119772,-20.0802520885476,
-3.8171651812947));
#121677=CARTESIAN_POINT('Ctrl Pts',(19.3080221524756,-21.9281136602303,
-3.94434098797614));
#121678=CARTESIAN_POINT('Ctrl Pts',(16.5422666958893,-21.0455756670647,
-4.07151679465757));
#121679=CARTESIAN_POINT('Ctrl Pts',(15.7872905115249,-18.242311941345,-4.198692601339));
#121680=CARTESIAN_POINT('Ctrl Pts',(17.7357373894132,-16.0901429612237,
-4.32586840802044));
#121681=CARTESIAN_POINT('Ctrl Pts',(20.6000282533525,-16.5635501873038,
-4.45304421470187));
#121682=CARTESIAN_POINT('Ctrl Pts',(21.7523540136147,-19.2282118726162,
-4.5802200213833));
#121683=CARTESIAN_POINT('Ctrl Pts',(20.1355273065643,-21.6394663084466,
-4.70739582806474));
#121684=CARTESIAN_POINT('Ctrl Pts',(17.2328862843358,-21.5851372092476,
-4.83457163474617));
#121685=CARTESIAN_POINT('Ctrl Pts',(15.7074239266047,-19.115068151491,-4.96174744142761));
#121686=CARTESIAN_POINT('Ctrl Pts',(16.9586572657169,-16.4953941858922,
-5.08892324810904));
#121687=CARTESIAN_POINT('Ctrl Pts',(19.8386573733367,-16.1295035805846,
-5.21609905479048));
#121688=CARTESIAN_POINT('Ctrl Pts',(21.705202903689,-18.3530782562058,-5.34327486147191));
#121689=CARTESIAN_POINT('Ctrl Pts',(20.8458541835569,-21.1261264584823,
-5.47045066815334));
#121690=CARTESIAN_POINT('Ctrl Pts',(18.0490103264645,-21.9045485766079,
-5.59762647483478));
#121691=CARTESIAN_POINT('Ctrl Pts',(15.8806019795871,-19.9741906315278,
-5.72480228151621));
#121692=CARTESIAN_POINT('Ctrl Pts',(16.3300092145838,-17.1060362263267,
-5.85197808819766));
#121693=CARTESIAN_POINT('Ctrl Pts',(18.9849287867042,-15.9314390100375,
-5.97915389487907));
#121694=CARTESIAN_POINT('Ctrl Pts',(21.4096367714204,-17.5280190248805,
-6.10632970156052));
#121695=CARTESIAN_POINT('Ctrl Pts',(21.3796140871054,-20.4310132021685,
-6.23350550824194));
#121696=CARTESIAN_POINT('Ctrl Pts',(18.9224046832003,-21.9771045643792,
-6.36068131492339));
#121697=CARTESIAN_POINT('Ctrl Pts',(16.2923456761723,-20.7478502479364,
-6.48785712160482));
#121698=CARTESIAN_POINT('Ctrl Pts',(15.9023529650977,-17.8710147920491,
-6.61503292828625));
#121699=CARTESIAN_POINT('Ctrl Pts',(18.1102206567097,-15.9859161709479,
-6.74220873496769));
#121700=CARTESIAN_POINT('Ctrl Pts',(20.8903671796782,-16.8220153670774,
-6.86938454164913));
#121701=CARTESIAN_POINT('Ctrl Pts',(21.6921806545333,-19.6122432621575,
-6.99656034833056));
#121702=CARTESIAN_POINT('Ctrl Pts',(19.7800469842523,-21.7967389435265,
-7.12373615501199));
#121703=CARTESIAN_POINT('Ctrl Pts',(16.9082301309179,-21.3713632086215,
-7.25091196169343));
#121704=CARTESIAN_POINT('Ctrl Pts',(15.711443812408,-18.7263718924222,-7.37808776837486));
#121705=CARTESIAN_POINT('Ctrl Pts',(17.2876651950193,-16.2883803608658,
-7.5052635750563));
#121706=CARTESIAN_POINT('Ctrl Pts',(20.1908089915383,-16.2940945253353,
-7.63243938173773));
#121707=CARTESIAN_POINT('Ctrl Pts',(21.7574209580843,-18.7382719945909,
-7.75961518841917));
#121708=CARTESIAN_POINT('Ctrl Pts',(20.5502318502561,-21.3785316433533,
-7.8867909951006));
#121709=CARTESIAN_POINT('Ctrl Pts',(17.6767627478799,-21.7925991168782,
-8.01396680178203));
#121710=CARTESIAN_POINT('Ctrl Pts',(15.7732432047795,-19.6005932081323,
-8.14114260846348));
#121711=CARTESIAN_POINT('Ctrl Pts',(16.5860342560023,-16.8135432871596,
-8.26831841514489));
#121712=CARTESIAN_POINT('Ctrl Pts',(19.3694505595535,-15.9883946726254,
-8.39549422182634));
#121713=CARTESIAN_POINT('Ctrl Pts',(21.5698804152241,-17.8821700038661,
-8.52267002850777));
#121714=CARTESIAN_POINT('Ctrl Pts',(21.1685660045158,-20.7574479554213,
-8.6498458351892));
#121715=CARTESIAN_POINT('Ctrl Pts',(18.5336883908723,-21.9763394666155,
-8.77702164187065));
#121716=CARTESIAN_POINT('Ctrl Pts',(16.0825842458626,-20.4205872288672,
-8.90419744855206));
#121717=CARTESIAN_POINT('Ctrl Pts',(16.0639894898528,-17.5174973594366,
-9.03137325523352));
#121718=CARTESIAN_POINT('Ctrl Pts',(18.4949636573611,-15.9304746274477,
-9.15854906191495));
#121719=CARTESIAN_POINT('Ctrl Pts',(21.1452388329719,-17.1155138877607,
-9.28572486859637));
#121720=CARTESIAN_POINT('Ctrl Pts',(21.5833520376912,-19.98541517087,-9.4129006752778));
#121721=CARTESIAN_POINT('Ctrl Pts',(19.4073615985613,-21.9072221756853,
-9.54007648195925));
#121722=CARTESIAN_POINT('Ctrl Pts',(16.6136036862856,-21.1177962560837,
-9.66725228864067));
#121723=CARTESIAN_POINT('Ctrl Pts',(15.7651777852051,-18.3413866960012,
-9.79442809532212));
#121724=CARTESIAN_POINT('Ctrl Pts',(17.6404620003109,-16.1251769434017,
-9.92160390200354));
#121725=CARTESIAN_POINT('Ctrl Pts',(20.5189994575086,-16.5024018928049,
-10.048779708685));
#121726=CARTESIAN_POINT('Ctrl Pts',(21.7599107020031,-19.1269810663543,
-10.1759555153665));
#121727=CARTESIAN_POINT('Ctrl Pts',(20.2247366866089,-21.5910259720733,
-10.3031313220479));
#121728=CARTESIAN_POINT('Ctrl Pts',(17.3219042868047,-21.6339283448398,
-10.4303071287293));
#121729=CARTESIAN_POINT('Ctrl Pts',(15.7145820593127,-19.2163279204619,
-10.5574829354107));
#121730=CARTESIAN_POINT('Ctrl Pts',(16.8773883861884,-16.5562230351012,
-10.6846587420922));
#121731=CARTESIAN_POINT('Ctrl Pts',(19.7435206344235,-16.0940948163466,
-10.8118345487736));
#121732=CARTESIAN_POINT('Ctrl Pts',(21.683480358492,-18.2539172219934,-10.9390103554551));
#121733=CARTESIAN_POINT('Ctrl Pts',(20.9174749190411,-21.0541872485576,
-11.0661861621365));
#121734=CARTESIAN_POINT('Ctrl Pts',(18.1482667631075,-21.9258309510259,
-11.1933619688179));
#121735=CARTESIAN_POINT('Ctrl Pts',(15.9164324973179,-20.069169332693,-11.3205377754993));
#121736=CARTESIAN_POINT('Ctrl Pts',(16.2695415372774,-17.1875741909633,
-11.4477135821808));
#121737=CARTESIAN_POINT('Ctrl Pts',(18.8836382552418,-15.9247302164082,
-11.5748893888622));
#121738=CARTESIAN_POINT('Ctrl Pts',(21.3604511616193,-17.4392183747454,
-11.7020651955437));
#121739=CARTESIAN_POINT('Ctrl Pts',(21.427658143155,-20.3415897804367,-11.8292410022251));
#121740=CARTESIAN_POINT('Ctrl Pts',(19.0236009656254,-21.9690988102461,
-11.9564168089065));
#121741=CARTESIAN_POINT('Ctrl Pts',(16.3538528767977,-20.8286069439261,
-12.083592615588));
#121742=CARTESIAN_POINT('Ctrl Pts',(15.8677420449167,-17.9664446819167,
-12.2107684222694));
#121743=CARTESIAN_POINT('Ctrl Pts',(18.0112449867927,-16.008468253787,-12.3379442289508));
#121744=CARTESIAN_POINT('Ctrl Pts',(20.817830794051,-16.7509995066233,-12.4651200356323));
#121745=CARTESIAN_POINT('Ctrl Pts',(21.712631184893,-19.5128121026353,-12.5922958423137));
#121746=CARTESIAN_POINT('Ctrl Pts',(19.874722338297,-21.7601144024042,-12.7194716489951));
#121747=CARTESIAN_POINT('Ctrl Pts',(16.9902715475267,-21.4311460292034,
-12.8466474556766));
#121748=CARTESIAN_POINT('Ctrl Pts',(15.7055833839069,-18.8277150473647,
-12.973823262358));
#121749=CARTESIAN_POINT('Ctrl Pts',(17.1992795008189,-16.3383077955748,
-13.1009990690394));
#121750=CARTESIAN_POINT('Ctrl Pts',(20.1009864202325,-16.2468009173113,
-13.2281748757209));
#121751=CARTESIAN_POINT('Ctrl Pts',(21.7485681438287,-18.6371462938237,
-13.3553506824023));
#121752=CARTESIAN_POINT('Ctrl Pts',(20.6304707006625,-21.3163504037278,
-13.4825264890837));
#121753=CARTESIAN_POINT('Ctrl Pts',(17.7724790978853,-21.8264097663479,
-13.6097022957652));
#121754=CARTESIAN_POINT('Ctrl Pts',(15.7966232440805,-19.6993765743343,
-13.7368781024466));
#121755=CARTESIAN_POINT('Ctrl Pts',(16.5156282496692,-16.8866717627907,
-13.864053909128));
#121756=CARTESIAN_POINT('Ctrl Pts',(19.2698516485073,-15.9687774201593,
-13.9912297158095));
#121757=CARTESIAN_POINT('Ctrl Pts',(21.532464418544,-17.7878046348562,-14.1184055224909));
#121758=CARTESIAN_POINT('Ctrl Pts',(21.2276597768573,-20.674908838959,-14.2455813291723));
#121759=CARTESIAN_POINT('Ctrl Pts',(18.6350770638849,-21.9813511190996,
-14.3727571358538));
#121760=CARTESIAN_POINT('Ctrl Pts',(16.1332500049482,-20.5085517702016,
-14.4999329425352));
#121761=CARTESIAN_POINT('Ctrl Pts',(16.0174496457219,-17.6077127826422,
-14.6271087492167));
#121762=CARTESIAN_POINT('Ctrl Pts',(18.3939156284153,-15.940173881134,-14.7542845558981));
#121763=CARTESIAN_POINT('Ctrl Pts',(21.082387914021,-17.0357985086741,-14.8814603625795));
#121764=CARTESIAN_POINT('Ctrl Pts',(21.6163600459046,-19.889419071628,-15.008636169261));
#121765=CARTESIAN_POINT('Ctrl Pts',(19.5059457351114,-21.8830158191527,
-15.1358119759424));
#121766=CARTESIAN_POINT('Ctrl Pts',(16.6873191247092,-21.1875874719632,
-15.2629877826238));
#121767=CARTESIAN_POINT('Ctrl Pts',(15.7463951860447,-18.4411463754548,
-15.3901635893052));
#121768=CARTESIAN_POINT('Ctrl Pts',(17.5464132325167,-16.1633817723147,
-15.5173393959867));
#121769=CARTESIAN_POINT('Ctrl Pts',(20.4359684282068,-16.4440013119089,
-15.6445152026681));
#121770=CARTESIAN_POINT('Ctrl Pts',(21.7640732270913,-19.0255539838723,
-15.7716910093496));
#121771=CARTESIAN_POINT('Ctrl Pts',(20.3122739076741,-21.539625440908,-15.898866816031));
#121772=CARTESIAN_POINT('Ctrl Pts',(17.4125062366922,-21.6797111620585,
-16.0260426227124));
#121773=CARTESIAN_POINT('Ctrl Pts',(15.725127072392,-19.3172911928685,-16.1532184293939));
#121774=CARTESIAN_POINT('Ctrl Pts',(16.7982020674565,-16.6197392267502,
-16.2803942360753));
#121775=CARTESIAN_POINT('Ctrl Pts',(19.6472515164596,-16.0618917636594,
-16.4075700427567));
#121776=CARTESIAN_POINT('Ctrl Pts',(21.6584493818927,-18.1555392270637,
-16.5347458494382));
#121777=CARTESIAN_POINT('Ctrl Pts',(20.9866464512386,-20.9798900157063,
-16.6619216561196));
#121778=CARTESIAN_POINT('Ctrl Pts',(18.24818021658,-21.9437775799877,-16.789097462801));
#121779=CARTESIAN_POINT('Ctrl Pts',(15.9554234798327,-20.162894905289,-16.9162732694825));
#121780=CARTESIAN_POINT('Ctrl Pts',(16.2118382424305,-17.2710913116015,
-17.0434490761639));
#121781=CARTESIAN_POINT('Ctrl Pts',(18.7821798745847,-15.9214171105603,
-17.1706248828453));
#121782=CARTESIAN_POINT('Ctrl Pts',(21.3083194621878,-17.3521146113923,
-17.2978006895268));
#121783=CARTESIAN_POINT('Ctrl Pts',(21.4726807235191,-20.2506076561855,
-17.4249764962082));
#121784=CARTESIAN_POINT('Ctrl Pts',(19.1244724027178,-21.9577087771101,
-17.5521523028896));
#121785=CARTESIAN_POINT('Ctrl Pts',(16.4180298878732,-20.9072586503617,
-17.6793281095711));
#121786=CARTESIAN_POINT('Ctrl Pts',(15.8363462055885,-18.0629800689462,
-17.8065039162525));
#121787=CARTESIAN_POINT('Ctrl Pts',(17.9130800309984,-16.0343220954698,
-17.9336797229339));
#121788=CARTESIAN_POINT('Ctrl Pts',(20.7429569759279,-16.6824525078913,
-18.0608555296154));
#121789=CARTESIAN_POINT('Ctrl Pts',(21.7297405853753,-19.412751880308,-18.1880313362968));
#121790=CARTESIAN_POINT('Ctrl Pts',(19.9681181443722,-21.7203400000494,
-18.3152071429782));
#121791=CARTESIAN_POINT('Ctrl Pts',(17.0742689039165,-21.4881479922645,
-18.4423829496597));
#121792=CARTESIAN_POINT('Ctrl Pts',(15.7031199295909,-18.9291976127498,
-18.5695587563411));
#121793=CARTESIAN_POINT('Ctrl Pts',(17.1126153022265,-16.3911670081152,
-18.6967345630226));
#121794=CARTESIAN_POINT('Ctrl Pts',(20.0096305005975,-16.2025417305957,
-18.823910369704));
#121795=CARTESIAN_POINT('Ctrl Pts',(21.7363338892051,-18.5363737640858,
-18.9510861763854));
#121796=CARTESIAN_POINT('Ctrl Pts',(20.7085822803688,-21.2515170733997,
-19.0782619830668));
#121797=CARTESIAN_POINT('Ctrl Pts',(17.8692739856059,-21.8569961899794,
-19.2054377897483));
#121798=CARTESIAN_POINT('Ctrl Pts',(15.8232981382665,-19.7973216105359,
-19.3326135964297));
#121799=CARTESIAN_POINT('Ctrl Pts',(16.4477105902148,-16.9621169125157,
-19.4597894031112));
#121800=CARTESIAN_POINT('Ctrl Pts',(19.1696516731346,-15.9525064556156,
-19.5869652097926));
#121801=CARTESIAN_POINT('Ctrl Pts',(21.4919093843545,-17.6947451283222,
-19.714141016474));
#121802=CARTESIAN_POINT('Ctrl Pts',(21.2839564128859,-20.5904371653283,
-19.8413168231554));
#121803=CARTESIAN_POINT('Ctrl Pts',(18.7365766963153,-21.9829646927876,
-19.9684926298369));
#121804=CARTESIAN_POINT('Ctrl Pts',(16.1868330293274,-20.5947704364421,
-20.0956684365183));
#121805=CARTESIAN_POINT('Ctrl Pts',(15.9739569464928,-17.6994358831224,
-20.2228442431997));
#121806=CARTESIAN_POINT('Ctrl Pts',(18.2932490893143,-15.9532519029135,
-20.3500200498812));
#121807=CARTESIAN_POINT('Ctrl Pts',(21.0169027756026,-16.9582317548374,
-20.4771958565626));
#121808=CARTESIAN_POINT('Ctrl Pts',(21.6461349757523,-19.7923729679124,
-20.6043716632441));
#121809=CARTESIAN_POINT('Ctrl Pts',(19.6036638566053,-21.855518855653,-20.7315474699255));
#121810=CARTESIAN_POINT('Ctrl Pts',(16.7633305629729,-21.2548765937423,
-20.8587232766069));
#121811=CARTESIAN_POINT('Ctrl Pts',(15.7309633230734,-18.5414683575651,
-20.9858990832884));
#121812=CARTESIAN_POINT('Ctrl Pts',(17.4536974658068,-16.2047352548569,
-21.1130748899698));
#121813=CARTESIAN_POINT('Ctrl Pts',(20.3510265953171,-16.3883741373928,
-21.2402506966512));
#121814=CARTESIAN_POINT('Ctrl Pts',(21.7648402074573,-18.9241211217718,
-21.3674265033327));
#121815=CARTESIAN_POINT('Ctrl Pts',(20.3980344426769,-21.4851745132897,
-21.4946023100141));
#121816=CARTESIAN_POINT('Ctrl Pts',(17.5046027271422,-21.7227192681557,
-21.6217781166956));
#121817=CARTESIAN_POINT('Ctrl Pts',(15.7390234877918,-19.4172952643212,
-21.748953923377));
#121818=CARTESIAN_POINT('Ctrl Pts',(16.7212336413073,-16.6869333681719,
-21.8761297300584));
#121819=CARTESIAN_POINT('Ctrl Pts',(19.5498595326579,-16.0308555962028,
-22.0033055367398));
#121820=CARTESIAN_POINT('Ctrl Pts',(21.6307164666946,-18.0626227175078,
-22.1305000010223));
#121821=CARTESIAN_POINT('Ctrl Pts',(21.244679026905,-19.9500078602896,-22.2153025297443));
#121822=CARTESIAN_POINT('Ctrl Pts',(20.6946893042483,-20.6030837310341,
-22.2577131229058));
#121823=CARTESIAN_POINT('Ctrl Pts',(18.1101968702393,-21.2832302832024,
0.0847274181292425));
#121824=CARTESIAN_POINT('Ctrl Pts',(17.3340242768668,-21.0755378486675,
0.0423354825687643));
#121825=CARTESIAN_POINT('Ctrl Pts',(16.0189819851084,-19.8273057761765,
-0.0424483885521918));
#121826=CARTESIAN_POINT('Ctrl Pts',(16.5291381537116,-17.1376091768898,
-0.169624195233626));
#121827=CARTESIAN_POINT('Ctrl Pts',(19.0658757862808,-16.118581759655,-0.29680000191506));
#121828=CARTESIAN_POINT('Ctrl Pts',(21.2962359844956,-17.6960342466338,
-0.423975808596494));
#121829=CARTESIAN_POINT('Ctrl Pts',(21.1768856466422,-20.4273012583374,
-0.551151615277929));
#121830=CARTESIAN_POINT('Ctrl Pts',(18.8158303215486,-21.8042714183123,
-0.678327421959364));
#121831=CARTESIAN_POINT('Ctrl Pts',(16.379964849342,-20.5648743004978,-0.805503228640797));
#121832=CARTESIAN_POINT('Ctrl Pts',(16.103643479711,-17.8455499279943,-0.932679035322232));
#121833=CARTESIAN_POINT('Ctrl Pts',(18.2405820727437,-16.1414364891873,
-1.05985484200366));
#121834=CARTESIAN_POINT('Ctrl Pts',(20.8301640861484,-17.0157826813563,
-1.1870306486851));
#121835=CARTESIAN_POINT('Ctrl Pts',(21.4966648031415,-19.6665181585552,
-1.31420645536653));
#121836=CARTESIAN_POINT('Ctrl Pts',(19.6285820960571,-21.6617119688685,
-1.44138226204797));
#121837=CARTESIAN_POINT('Ctrl Pts',(16.9397809967372,-21.1709213290295,
-1.5685580687294));
#121838=CARTESIAN_POINT('Ctrl Pts',(15.897061795067,-18.6444038895142,-1.69573387541083));
#121839=CARTESIAN_POINT('Ctrl Pts',(17.4570587048633,-16.400088970387,-1.82290968209227));
#121840=CARTESIAN_POINT('Ctrl Pts',(20.188569276403,-16.4969928998977,-1.9500854887737));
#121841=CARTESIAN_POINT('Ctrl Pts',(21.58560319155,-18.8462140560325,-2.07726129545514));
#121842=CARTESIAN_POINT('Ctrl Pts',(20.3664679748478,-21.2924869452229,
-2.20443710213657));
#121843=CARTESIAN_POINT('Ctrl Pts',(17.6496448143142,-21.5915084873017,
-2.33161290881801));
#121844=CARTESIAN_POINT('Ctrl Pts',(15.9276501817169,-19.4689447365969,
-2.45878871549944));
#121845=CARTESIAN_POINT('Ctrl Pts',(16.7803073527985,-16.8721163178553,
-2.58596452218088));
#121846=CARTESIAN_POINT('Ctrl Pts',(19.4253562537739,-16.1834520632443,
-2.71314032886231));
#121847=CARTESIAN_POINT('Ctrl Pts',(21.4361287096228,-18.034758716609,-2.84031613554374));
#121848=CARTESIAN_POINT('Ctrl Pts',(20.9678657836256,-20.72757731112,-2.96749194222518));
#121849=CARTESIAN_POINT('Ctrl Pts',(18.4501696524655,-21.7914139305229,
-3.09466774890661));
#121850=CARTESIAN_POINT('Ctrl Pts',(16.1928702476498,-20.2502645009728,
-3.22184355558806));
#121851=CARTESIAN_POINT('Ctrl Pts',(16.2668996708449,-17.5180379719942,
-3.34901936226947));
#121852=CARTESIAN_POINT('Ctrl Pts',(18.6043405202493,-16.1013826015585,
-3.47619516895092));
#121853=CARTESIAN_POINT('Ctrl Pts',(21.0607358948925,-17.2999917651471,
-3.60337097563235));
#121854=CARTESIAN_POINT('Ctrl Pts',(21.3824954994144,-20.0142159489022,
-3.73054678231378));
#121855=CARTESIAN_POINT('Ctrl Pts',(19.2744248674316,-21.7539229281569,
-3.85772258899522));
#121856=CARTESIAN_POINT('Ctrl Pts',(16.6705479621107,-20.9230395277464,
-3.98489839567665));
#121857=CARTESIAN_POINT('Ctrl Pts',(15.9597602292861,-18.2838496971548,
-4.11207420235809));
#121858=CARTESIAN_POINT('Ctrl Pts',(17.7941652973467,-16.2576462993305,
-4.23925000903952));
#121859=CARTESIAN_POINT('Ctrl Pts',(20.4908103723742,-16.7033451914242,
-4.36642581572096));
#121860=CARTESIAN_POINT('Ctrl Pts',(21.5756909706959,-19.2120453031261,
-4.49360162240239));
#121861=CARTESIAN_POINT('Ctrl Pts',(20.053496478638,-21.4821699894429,-4.62077742908383));
#121862=CARTESIAN_POINT('Ctrl Pts',(17.320745864617,-21.4310207505056,-4.74795323576526));
#121863=CARTESIAN_POINT('Ctrl Pts',(15.8845682033658,-19.1055238383603,
-4.8751290424467));
#121864=CARTESIAN_POINT('Ctrl Pts',(17.0625673598435,-16.6391783332833,
-5.00230484912813));
#121865=CARTESIAN_POINT('Ctrl Pts',(19.7740022228553,-16.294703157517,-5.12948065580956));
#121866=CARTESIAN_POINT('Ctrl Pts',(21.5312995962151,-18.388132904286,-5.256656462491));
#121867=CARTESIAN_POINT('Ctrl Pts',(20.7222482100412,-20.9988757138337,
-5.38383226917243));
#121868=CARTESIAN_POINT('Ctrl Pts',(18.0891024957557,-21.7317370993736,
-5.51100807585386));
#121869=CARTESIAN_POINT('Ctrl Pts',(16.0476102147611,-19.9143622261804,
-5.6381838825353));
#121870=CARTESIAN_POINT('Ctrl Pts',(16.4707138255686,-17.2140797414027,
-5.76535968921673));
#121871=CARTESIAN_POINT('Ctrl Pts',(18.9702420260344,-16.1082312263917,
-5.89253549589816));
#121872=CARTESIAN_POINT('Ctrl Pts',(21.2530328304472,-17.6113640569702,
-6.01971130257962));
#121873=CARTESIAN_POINT('Ctrl Pts',(21.2247673617351,-20.3444471560277,
-6.14688710926103));
#121874=CARTESIAN_POINT('Ctrl Pts',(18.9113774330884,-21.8000464144471,
-6.27406291594248));
#121875=CARTESIAN_POINT('Ctrl Pts',(16.4352547188683,-20.6427398573077,
-6.4012387226239));
#121876=CARTESIAN_POINT('Ctrl Pts',(16.0680881238634,-17.934284420239,-6.52841452930535));
#121877=CARTESIAN_POINT('Ctrl Pts',(18.1467302100618,-16.1595198610482,
-6.65559033598677));
#121878=CARTESIAN_POINT('Ctrl Pts',(20.7641558784545,-16.9466825084813,
-6.78276614266821));
#121879=CARTESIAN_POINT('Ctrl Pts',(21.5190395340498,-19.5735994903424,
-6.90994194934964));
#121880=CARTESIAN_POINT('Ctrl Pts',(19.7188222762027,-21.6302375206298,
-7.03711775603107));
#121881=CARTESIAN_POINT('Ctrl Pts',(17.0150917049037,-21.2297588559072,
-7.16429356271251));
#121882=CARTESIAN_POINT('Ctrl Pts',(15.8883528068746,-18.7395778145483,
-7.29146936939396));
#121883=CARTESIAN_POINT('Ctrl Pts',(17.3723185877541,-16.4442809439337,
-7.41864517607538));
#121884=CARTESIAN_POINT('Ctrl Pts',(20.1055425488892,-16.4496606606615,
-7.54582098275682));
#121885=CARTESIAN_POINT('Ctrl Pts',(21.5804613489495,-18.7507814085371,
-7.67299678943824));
#121886=CARTESIAN_POINT('Ctrl Pts',(20.4439285326649,-21.2365077250456,
-7.80017259611969));
#121887=CARTESIAN_POINT('Ctrl Pts',(17.7386424177941,-21.6263399963654,
-7.92734840280111));
#121888=CARTESIAN_POINT('Ctrl Pts',(15.9465351057383,-19.5626313092801,
-8.05452420948257));
#121889=CARTESIAN_POINT('Ctrl Pts',(16.7117538245844,-16.9387062959837,
-8.18170001616398));
#121890=CARTESIAN_POINT('Ctrl Pts',(19.3322578946213,-16.1618532970222,
-8.30887582284543));
#121891=CARTESIAN_POINT('Ctrl Pts',(21.4038974784157,-17.9447867220078,
-8.43605162952684));
#121892=CARTESIAN_POINT('Ctrl Pts',(21.0260718382901,-20.6517758148449,
-8.5632274362083));
#121893=CARTESIAN_POINT('Ctrl Pts',(18.5454125485558,-21.799326097547,-8.69040324288972));
#121894=CARTESIAN_POINT('Ctrl Pts',(16.2377705404641,-20.3346314107382,
-8.81757904957117));
#121895=CARTESIAN_POINT('Ctrl Pts',(16.2202641280231,-17.6014582203607,
-8.94475485625259));
#121896=CARTESIAN_POINT('Ctrl Pts',(18.5089543580768,-16.1073232887258,
-9.07193066293403));
#121897=CARTESIAN_POINT('Ctrl Pts',(21.0041099966872,-17.223002679136,-9.19910646961547));
#121898=CARTESIAN_POINT('Ctrl Pts',(21.4165806122538,-19.9249297977624,
-9.32628227629688));
#121899=CARTESIAN_POINT('Ctrl Pts',(19.3679500158079,-21.7342542137755,
-9.45345808297835));
#121900=CARTESIAN_POINT('Ctrl Pts',(16.7377096272338,-20.9910330748214,
-9.58063388965975));
#121901=CARTESIAN_POINT('Ctrl Pts',(15.9389417519183,-18.3771256463843,
-9.70780969634122));
#121902=CARTESIAN_POINT('Ctrl Pts',(17.7044663383378,-16.2906297566631,
-9.83498550302262));
#121903=CARTESIAN_POINT('Ctrl Pts',(20.4145241592668,-16.6457758819371,
-9.96216130970408));
#121904=CARTESIAN_POINT('Ctrl Pts',(21.5828053691612,-19.1167394951217,
-10.0893371163855));
#121905=CARTESIAN_POINT('Ctrl Pts',(20.1374844696525,-21.4365648464185,
-10.2165129230669));
#121906=CARTESIAN_POINT('Ctrl Pts',(17.4045536793081,-21.4769561606121,
-10.3436887297484));
#121907=CARTESIAN_POINT('Ctrl Pts',(15.8913073734538,-19.2008569138979,
-10.4708645364298));
#121908=CARTESIAN_POINT('Ctrl Pts',(16.9860551150528,-16.6964468944843,
-10.5980403431112));
#121909=CARTESIAN_POINT('Ctrl Pts',(19.6844337988958,-16.2613668539671,
-10.7252161497927));
#121910=CARTESIAN_POINT('Ctrl Pts',(21.5108484628264,-18.294775725408,-10.8523919564741));
#121911=CARTESIAN_POINT('Ctrl Pts',(20.7896770127668,-20.9311470768482,
-10.9795677631555));
#121912=CARTESIAN_POINT('Ctrl Pts',(18.1825494931985,-21.7517738250013,
-11.106743569837));
#121913=CARTESIAN_POINT('Ctrl Pts',(16.081343586742,-20.0037818622775,-11.2339193765184));
#121914=CARTESIAN_POINT('Ctrl Pts',(16.4137852970245,-17.2908453218587,
-11.3610951831999));
#121915=CARTESIAN_POINT('Ctrl Pts',(18.8748799885214,-16.1019150957474,
-11.4882709898813));
#121916=CARTESIAN_POINT('Ctrl Pts',(21.206726034548,-17.5277608730685,-11.6154467965627));
#121917=CARTESIAN_POINT('Ctrl Pts',(21.2699994185634,-20.2602576510996,
-11.7426226032442));
#121918=CARTESIAN_POINT('Ctrl Pts',(19.0066507379223,-21.7925092338742,
-11.8697984099256));
#121919=CARTESIAN_POINT('Ctrl Pts',(16.4931619278508,-20.7187698964554,
-11.996974216607));
#121920=CARTESIAN_POINT('Ctrl Pts',(16.0355029668799,-18.0241288371456,
-12.1241500232885));
#121921=CARTESIAN_POINT('Ctrl Pts',(18.0535475461816,-16.1807519795754,
-12.2513258299699));
#121922=CARTESIAN_POINT('Ctrl Pts',(20.6958650182194,-16.8798231776942,
-12.3785016366513));
#121923=CARTESIAN_POINT('Ctrl Pts',(21.5382931031166,-19.4799879964801,
-12.5056774433328));
#121924=CARTESIAN_POINT('Ctrl Pts',(19.8079563199639,-21.5957565991263,
-12.6328532500142));
#121925=CARTESIAN_POINT('Ctrl Pts',(17.092331270491,-21.2860426121147,-12.7600290566956));
#121926=CARTESIAN_POINT('Ctrl Pts',(15.8828353868898,-18.8349893955103,
-12.8872048633771));
#121927=CARTESIAN_POINT('Ctrl Pts',(17.2891060725835,-16.491286146028,-13.0143806700585));
#121928=CARTESIAN_POINT('Ctrl Pts',(20.0209772564507,-16.4051351284387,
-13.1415564767399));
#121929=CARTESIAN_POINT('Ctrl Pts',(21.5721266863414,-18.6555745542452,
-13.2687322834214));
#121930=CARTESIAN_POINT('Ctrl Pts',(20.5194710355226,-21.1779659282937,
-13.3959080901028));
#121931=CARTESIAN_POINT('Ctrl Pts',(17.8287565284422,-21.6581717221597,
-13.5230838967842));
#121932=CARTESIAN_POINT('Ctrl Pts',(15.9685467207697,-19.6556329249039,
-13.6502597034657));
#121933=CARTESIAN_POINT('Ctrl Pts',(16.6454686534027,-17.0075545914336,
-13.7774355101471));
#121934=CARTESIAN_POINT('Ctrl Pts',(19.2384884676639,-16.14338423443,-13.9046113168286));
#121935=CARTESIAN_POINT('Ctrl Pts',(21.3686714249291,-17.8559445199825,
-14.03178712351));
#121936=CARTESIAN_POINT('Ctrl Pts',(21.0817068759728,-20.5740676795759,
-14.1589629301914));
#121937=CARTESIAN_POINT('Ctrl Pts',(18.6408669834337,-21.8040444200327,
-14.2861387368729));
#121938=CARTESIAN_POINT('Ctrl Pts',(16.2854708531072,-20.4174474229502,
-14.4133145435543));
#121939=CARTESIAN_POINT('Ctrl Pts',(16.1764482421967,-17.6863933712359,
-14.5404903502357));
#121940=CARTESIAN_POINT('Ctrl Pts',(18.413820629506,-16.1164548490061,-14.6676661569172));
#121941=CARTESIAN_POINT('Ctrl Pts',(20.9449377166707,-17.1479530090328,
-14.7948419635986));
#121942=CARTESIAN_POINT('Ctrl Pts',(21.4476566750608,-19.8345523114875,
-14.92201777028));
#121943=CARTESIAN_POINT('Ctrl Pts',(19.4607640626112,-21.7114646455266,
-15.0491935769614));
#121944=CARTESIAN_POINT('Ctrl Pts',(16.8071105307807,-21.0567394389867,
-15.1763693836429));
#121945=CARTESIAN_POINT('Ctrl Pts',(15.9212584907105,-18.471046432039,-15.3035451903243));
#121946=CARTESIAN_POINT('Ctrl Pts',(17.6159222069866,-16.3265984723504,
-15.4307209970058));
#121947=CARTESIAN_POINT('Ctrl Pts',(20.3363529026182,-16.5907934634841,
-15.5578968036872));
#121948=CARTESIAN_POINT('Ctrl Pts',(21.5867242633349,-19.0212488988654,
-15.6850726103686));
#121949=CARTESIAN_POINT('Ctrl Pts',(20.2198981724784,-21.388172767609,-15.8122484170501));
#121950=CARTESIAN_POINT('Ctrl Pts',(17.4898527336144,-21.5200593280063,
-15.9394242237315));
#121951=CARTESIAN_POINT('Ctrl Pts',(15.9012351911711,-19.2959108466956,
-16.0666000304129));
#121952=CARTESIAN_POINT('Ctrl Pts',(16.9115035396152,-16.7562455090563,
-16.1937758370943));
#121953=CARTESIAN_POINT('Ctrl Pts',(19.5937992735749,-16.2310486329641,
-16.3209516437758));
#121954=CARTESIAN_POINT('Ctrl Pts',(21.4872825391909,-18.2021557548393,
-16.4481274504572));
#121955=CARTESIAN_POINT('Ctrl Pts',(20.8547999630863,-20.8611984310668,
-16.5753032571387));
#121956=CARTESIAN_POINT('Ctrl Pts',(18.2766150525408,-21.7686700450093,
-16.7024790638201));
#121957=CARTESIAN_POINT('Ctrl Pts',(16.1180524427778,-20.092021714915,-16.8296548705015));
#121958=CARTESIAN_POINT('Ctrl Pts',(16.3594593527494,-17.3694742191139,
-16.956830677183));
#121959=CARTESIAN_POINT('Ctrl Pts',(18.7793599259594,-16.0987959046484,
-17.0840064838644));
#121960=CARTESIAN_POINT('Ctrl Pts',(21.1576455824562,-17.4457552578498,
-17.2111822905458));
#121961=CARTESIAN_POINT('Ctrl Pts',(21.3123868454594,-20.1746006738818,
-17.3383580972273));
#121962=CARTESIAN_POINT('Ctrl Pts',(19.1016182104896,-21.7817858547834,
-17.4655339039087));
#121963=CARTESIAN_POINT('Ctrl Pts',(16.5535826843549,-20.7928181502387,
-17.5927097105901));
#121964=CARTESIAN_POINT('Ctrl Pts',(16.0059447133635,-18.1150140469113,
-17.7198855172716));
#121965=CARTESIAN_POINT('Ctrl Pts',(17.9611281456538,-16.2050926063331,
-17.847061323953));
#121966=CARTESIAN_POINT('Ctrl Pts',(20.6253735344697,-16.8152882071486,
-17.9742371306345));
#121967=CARTESIAN_POINT('Ctrl Pts',(21.55440109729,-19.3857842586047,-18.1014129373159));
#121968=CARTESIAN_POINT('Ctrl Pts',(19.8958857071821,-21.5583101764979,
-18.2285887439973));
#121969=CARTESIAN_POINT('Ctrl Pts',(17.171412295493,-21.3397082732704,-18.3557645506787));
#121970=CARTESIAN_POINT('Ctrl Pts',(15.8805161175613,-18.9305322272779,
-18.4829403573602));
#121971=CARTESIAN_POINT('Ctrl Pts',(17.2075142945774,-16.54105153018,-18.6101161640416));
#121972=CARTESIAN_POINT('Ctrl Pts',(19.9349683619421,-16.3634664140689,
-18.7372919707231));
#121973=CARTESIAN_POINT('Ctrl Pts',(21.5606084977061,-18.5607002000248,
-18.8644677774045));
#121974=CARTESIAN_POINT('Ctrl Pts',(20.5930107759761,-21.1169272666383,
-18.9916435840859));
#121975=CARTESIAN_POINT('Ctrl Pts',(17.9198860504282,-21.6869679347534,
-19.1188193907673));
#121976=CARTESIAN_POINT('Ctrl Pts',(15.9936603441588,-19.7478452776443,
-19.2459951974488));
#121977=CARTESIAN_POINT('Ctrl Pts',(16.5815261871606,-17.078583966977,-19.3731710041302));
#121978=CARTESIAN_POINT('Ctrl Pts',(19.1441531564327,-16.1280656028778,
-19.5003468108116));
#121979=CARTESIAN_POINT('Ctrl Pts',(21.3304900605322,-17.768331748829,-19.6275226174931));
#121980=CARTESIAN_POINT('Ctrl Pts',(21.1347084926027,-20.4945400989296,
-19.7546984241745));
#121981=CARTESIAN_POINT('Ctrl Pts',(18.7364258833193,-21.8055635519036,
-19.881874230856));
#121982=CARTESIAN_POINT('Ctrl Pts',(16.335917684683,-20.4986197454331,-20.0090500375374));
#121983=CARTESIAN_POINT('Ctrl Pts',(16.13550115311,-17.7727479556429,-20.1362258442188));
#121984=CARTESIAN_POINT('Ctrl Pts',(18.3190460623333,-16.1287674194462,
-20.2634016509003));
#121985=CARTESIAN_POINT('Ctrl Pts',(20.8832853969895,-17.0749262060105,
-20.3905774575817));
#121986=CARTESIAN_POINT('Ctrl Pts',(21.4756888902747,-19.7431862770776,
-20.5177532642631));
#121987=CARTESIAN_POINT('Ctrl Pts',(19.5527627818701,-21.6855770682093,
-20.6449290709446));
#121988=CARTESIAN_POINT('Ctrl Pts',(16.8786730502231,-21.1200901556103,
-20.772104877626));
#121989=CARTESIAN_POINT('Ctrl Pts',(15.9067298484541,-18.5654966090028,
-20.8992806843074));
#121990=CARTESIAN_POINT('Ctrl Pts',(17.5286330567039,-16.3655315522399,
-21.0264564909889));
#121991=CARTESIAN_POINT('Ctrl Pts',(20.256382680945,-16.5384221250544,-21.1536322976703));
#121992=CARTESIAN_POINT('Ctrl Pts',(21.5874463526494,-18.9257528612692,
-21.2808081043517));
#121993=CARTESIAN_POINT('Ctrl Pts',(20.3006391779602,-21.3369088308205,
-21.4079839110332));
#121994=CARTESIAN_POINT('Ctrl Pts',(17.5765588536269,-21.5605501870015,
-21.5351597177146));
#121995=CARTESIAN_POINT('Ctrl Pts',(15.9143182549829,-19.3900617201843,
-21.6623355243961));
#121996=CARTESIAN_POINT('Ctrl Pts',(16.8390400444023,-16.8195068044844,
-21.7895113310775));
#121997=CARTESIAN_POINT('Ctrl Pts',(19.5021076033005,-16.2018289998698,
-21.9166871377589));
#121998=CARTESIAN_POINT('Ctrl Pts',(21.4611728203329,-18.1146776111084,
-22.0438816020413));
#121999=CARTESIAN_POINT('Ctrl Pts',(21.0977299961801,-19.8915948627883,
-22.1286841307634));
#122000=CARTESIAN_POINT('Ctrl Pts',(20.5799309501441,-20.506446466246,-22.171094723925));
#122001=CARTESIAN_POINT('Ctrl Pts',(18.1489776385292,-21.138301703768,0.171345817110153));
#122002=CARTESIAN_POINT('Ctrl Pts',(17.4210583610835,-20.9435211508747,
0.128953881549675));
#122003=CARTESIAN_POINT('Ctrl Pts',(16.1877699881095,-19.77288952068,0.0441700104287191));
#122004=CARTESIAN_POINT('Ctrl Pts',(16.6662106246443,-17.2504067355124,
-0.083005796252715));
#122005=CARTESIAN_POINT('Ctrl Pts',(19.0452436391262,-16.2947305011482,
-0.210181602934149));
#122006=CARTESIAN_POINT('Ctrl Pts',(21.1369461776993,-17.7741154785761,
-0.337357409615584));
#122007=CARTESIAN_POINT('Ctrl Pts',(21.0250156451928,-20.3355843150782,
-0.464533216297019));
#122008=CARTESIAN_POINT('Ctrl Pts',(18.8107430711202,-21.6269506071526,
-0.591709022978452));
#122009=CARTESIAN_POINT('Ctrl Pts',(16.5263111681857,-20.4646046776889,
-0.718884829659889));
#122010=CARTESIAN_POINT('Ctrl Pts',(16.2671682231216,-17.9143360270367,
-0.84606063634132));
#122011=CARTESIAN_POINT('Ctrl Pts',(18.2712570171198,-16.3161643914318,
-0.973236443022757));
#122012=CARTESIAN_POINT('Ctrl Pts',(20.6998491681173,-17.1361539837924,
-1.10041224970419));
#122013=CARTESIAN_POINT('Ctrl Pts',(21.3249146812175,-19.6220977928601,
-1.22758805638563));
#122014=CARTESIAN_POINT('Ctrl Pts',(19.5729674648886,-21.4932538336279,
-1.35476386306706));
#122015=CARTESIAN_POINT('Ctrl Pts',(17.0513245079943,-21.0329748042223,
-1.4819396697485));
#122016=CARTESIAN_POINT('Ctrl Pts',(16.0734293667079,-18.6635266109603,
-1.60911547642993));
#122017=CARTESIAN_POINT('Ctrl Pts',(17.5364439501815,-16.5587368924863,
-1.73629128311137));
#122018=CARTESIAN_POINT('Ctrl Pts',(20.0981412048233,-16.6496164712725,
-1.8634670897928));
#122019=CARTESIAN_POINT('Ctrl Pts',(21.4083239228994,-18.852790586328,-1.99064289647423));
#122020=CARTESIAN_POINT('Ctrl Pts',(20.264980246985,-21.1469828950223,-2.11781870315567));
#122021=CARTESIAN_POINT('Ctrl Pts',(17.717057312254,-21.4274147818336,-2.2449945098371));
#122022=CARTESIAN_POINT('Ctrl Pts',(16.1021161259398,-19.4368071709258,
-2.37217031651854));
#122023=CARTESIAN_POINT('Ctrl Pts',(16.9017650663717,-17.0014191111546,
-2.49934612319997));
#122024=CARTESIAN_POINT('Ctrl Pts',(19.3823758238848,-16.3555679294722,
-2.62652192988141));
#122025=CARTESIAN_POINT('Ctrl Pts',(21.2681420125742,-18.0917820305039,
-2.75369773656284));
#122026=CARTESIAN_POINT('Ctrl Pts',(20.8289901877649,-20.6171927218193,
-2.88087354324428));
#122027=CARTESIAN_POINT('Ctrl Pts',(18.467814897281,-21.6148924472776,-3.0080493499257));
#122028=CARTESIAN_POINT('Ctrl Pts',(16.3508479162742,-20.1695536286012,
-3.13522515660715));
#122029=CARTESIAN_POINT('Ctrl Pts',(16.4202750574822,-17.6071849263638,
-3.26240096328857));
#122030=CARTESIAN_POINT('Ctrl Pts',(18.612401227227,-16.278600585146,-3.38957676997001));
#122031=CARTESIAN_POINT('Ctrl Pts',(20.9160867238537,-17.4026942773856,
-3.51675257665145));
#122032=CARTESIAN_POINT('Ctrl Pts',(21.2178430868515,-19.9481798092568,
-3.64392838333288));
#122033=CARTESIAN_POINT('Ctrl Pts',(19.2408275823876,-21.5797321960836,
-3.77110419001432));
#122034=CARTESIAN_POINT('Ctrl Pts',(16.7988292283319,-20.8005033884281,
-3.89827999669575));
#122035=CARTESIAN_POINT('Ctrl Pts',(16.1322299470473,-18.3253874529646,
-4.02545580337718));
#122036=CARTESIAN_POINT('Ctrl Pts',(17.8525932052803,-16.4251496374373,
-4.15263161005862));
#122037=CARTESIAN_POINT('Ctrl Pts',(20.3815924913958,-16.8431401955444,
-4.27980741674006));
#122038=CARTESIAN_POINT('Ctrl Pts',(21.3990279277772,-19.1958787336361,
-4.40698322342148));
#122039=CARTESIAN_POINT('Ctrl Pts',(19.9714656507117,-21.3248736704392,
-4.53415903010293));
#122040=CARTESIAN_POINT('Ctrl Pts',(17.4086054448983,-21.2769042917635,
-4.66133483678435));
#122041=CARTESIAN_POINT('Ctrl Pts',(16.0617124801271,-19.0959795252294,
-4.78851064346579));
#122042=CARTESIAN_POINT('Ctrl Pts',(17.1664774539701,-16.7829624806744,
-4.91568645014722));
#122043=CARTESIAN_POINT('Ctrl Pts',(19.709347072374,-16.4599027344493,-5.04286225682866));
#122044=CARTESIAN_POINT('Ctrl Pts',(21.3573962887413,-18.4231875523662,
-5.1700380635101));
#122045=CARTESIAN_POINT('Ctrl Pts',(20.5986422365255,-20.8716249691852,
-5.29721387019152));
#122046=CARTESIAN_POINT('Ctrl Pts',(18.1291946650469,-21.5589256221392,
-5.42438967687296));
#122047=CARTESIAN_POINT('Ctrl Pts',(16.2146184499352,-19.8545338208328,
-5.55156548355439));
#122048=CARTESIAN_POINT('Ctrl Pts',(16.6114184365535,-17.3221232564787,
-5.67874129023583));
#122049=CARTESIAN_POINT('Ctrl Pts',(18.9555552653643,-16.2850234427458,
-5.80591709691726));
#122050=CARTESIAN_POINT('Ctrl Pts',(21.096428889474,-17.69470908906,-5.9330929035987));
#122051=CARTESIAN_POINT('Ctrl Pts',(21.0699206363647,-20.2578811098868,
-6.06026871028013));
#122052=CARTESIAN_POINT('Ctrl Pts',(18.9003501829765,-21.6229882645151,
-6.18744451696157));
#122053=CARTESIAN_POINT('Ctrl Pts',(16.5781637615641,-20.537629466679,-6.31462032364299));
#122054=CARTESIAN_POINT('Ctrl Pts',(16.2338232826291,-17.9975540484287,
-6.44179613032444));
#122055=CARTESIAN_POINT('Ctrl Pts',(18.1832397634138,-16.3331235511484,
-6.56897193700587));
#122056=CARTESIAN_POINT('Ctrl Pts',(20.6379445772308,-17.0713496498852,
-6.69614774368731));
#122057=CARTESIAN_POINT('Ctrl Pts',(21.3458984135663,-19.5349557185273,
-6.82332355036874));
#122058=CARTESIAN_POINT('Ctrl Pts',(19.6575975681531,-21.4637360977331,
-6.95049935705017));
#122059=CARTESIAN_POINT('Ctrl Pts',(17.1219532788895,-21.0881545031928,
-7.07767516373161));
#122060=CARTESIAN_POINT('Ctrl Pts',(16.0652618013412,-18.7527837366743,
-7.20485097041304));
#122061=CARTESIAN_POINT('Ctrl Pts',(17.4569719804889,-16.6001815270014,
-7.33202677709449));
#122062=CARTESIAN_POINT('Ctrl Pts',(20.0202761062402,-16.6052267959878,
-7.4592025837759));
#122063=CARTESIAN_POINT('Ctrl Pts',(21.4035017398149,-18.7632908224833,
-7.58637839045736));
#122064=CARTESIAN_POINT('Ctrl Pts',(20.3376252150736,-21.094483806738,-7.71355419713877));
#122065=CARTESIAN_POINT('Ctrl Pts',(17.8005220877082,-21.4600808758526,
-7.84073000382022));
#122066=CARTESIAN_POINT('Ctrl Pts',(16.1198270066971,-19.5246694104279,
-7.96790581050164));
#122067=CARTESIAN_POINT('Ctrl Pts',(16.8374733931665,-17.0638693048078,
-8.09508161718309));
#122068=CARTESIAN_POINT('Ctrl Pts',(19.295065229689,-16.335311921419,-8.22225742386451));
#122069=CARTESIAN_POINT('Ctrl Pts',(21.2379145416073,-18.0074034401497,
-8.34943323054596));
#122070=CARTESIAN_POINT('Ctrl Pts',(20.8835776720644,-20.5461036742685,
-8.47660903722738));
#122071=CARTESIAN_POINT('Ctrl Pts',(18.5571367062394,-21.6223127284784,
-8.60378484390882));
#122072=CARTESIAN_POINT('Ctrl Pts',(16.3929568350657,-20.2486755926092,
-8.73096065059025));
#122073=CARTESIAN_POINT('Ctrl Pts',(16.3765387661935,-17.6854190812848,
-8.85813645727169));
#122074=CARTESIAN_POINT('Ctrl Pts',(18.5229450587927,-16.2841719500039,
-8.98531226395313));
#122075=CARTESIAN_POINT('Ctrl Pts',(20.8629811604026,-17.3304914705113,
-9.11248807063455));
#122076=CARTESIAN_POINT('Ctrl Pts',(21.2498091868164,-19.8644444246549,
-9.23966387731599));
#122077=CARTESIAN_POINT('Ctrl Pts',(19.3285384330547,-21.5612862518657,
-9.36683968399743));
#122078=CARTESIAN_POINT('Ctrl Pts',(16.861815568182,-20.864269893559,-9.49401549067886));
#122079=CARTESIAN_POINT('Ctrl Pts',(16.1127057186315,-18.4128645967674,
-9.6211912973603));
#122080=CARTESIAN_POINT('Ctrl Pts',(17.7684706763648,-16.4560825699245,
-9.74836710404172));
#122081=CARTESIAN_POINT('Ctrl Pts',(20.310048861025,-16.7891498710692,-9.87554291072316));
#122082=CARTESIAN_POINT('Ctrl Pts',(21.4057000363191,-19.1064979238893,
-10.0027187174046));
#122083=CARTESIAN_POINT('Ctrl Pts',(20.0502322526962,-21.2821037207635,
-10.129894524086));
#122084=CARTESIAN_POINT('Ctrl Pts',(17.4872030718116,-21.3199839763846,
-10.2570703307675));
#122085=CARTESIAN_POINT('Ctrl Pts',(16.068032687595,-19.1853859073339,-10.3842461374489));
#122086=CARTESIAN_POINT('Ctrl Pts',(17.0947218439171,-16.8366707538674,
-10.5114219441303));
#122087=CARTESIAN_POINT('Ctrl Pts',(19.6253469633683,-16.4286388915877,
-10.6385977508117));
#122088=CARTESIAN_POINT('Ctrl Pts',(21.3382165671608,-18.3356342288226,
-10.7657735574932));
#122089=CARTESIAN_POINT('Ctrl Pts',(20.6618791064926,-20.8081069051386,
-10.8929493641746));
#122090=CARTESIAN_POINT('Ctrl Pts',(18.2168322232895,-21.577716698977,-11.0201251708561));
#122091=CARTESIAN_POINT('Ctrl Pts',(16.2462546761661,-19.9383943918618,
-11.1473009775375));
#122092=CARTESIAN_POINT('Ctrl Pts',(16.5580290567716,-17.3941164527542,
-11.2744767842189));
#122093=CARTESIAN_POINT('Ctrl Pts',(18.8661217218008,-16.2790999750865,
-11.4016525909004));
#122094=CARTESIAN_POINT('Ctrl Pts',(21.0530009074768,-17.6163033713916,
-11.5288283975818));
#122095=CARTESIAN_POINT('Ctrl Pts',(21.1123406939717,-20.1789255217625,
-11.6560042042632));
#122096=CARTESIAN_POINT('Ctrl Pts',(18.989700510219,-21.6159196575024,-11.7831800109447));
#122097=CARTESIAN_POINT('Ctrl Pts',(16.6324709789039,-20.6089328489849,
-11.9103558176261));
#122098=CARTESIAN_POINT('Ctrl Pts',(16.203263888843,-18.0818129923747,-12.0375316243075));
#122099=CARTESIAN_POINT('Ctrl Pts',(18.0958501055707,-16.3530357053638,
-12.164707430989));
#122100=CARTESIAN_POINT('Ctrl Pts',(20.5738992423879,-17.0086468487652,
-12.2918832376704));
#122101=CARTESIAN_POINT('Ctrl Pts',(21.3639550213402,-19.4471638903247,
-12.4190590443519));
#122102=CARTESIAN_POINT('Ctrl Pts',(19.7411903016307,-21.4313987958485,
-12.5462348510332));
#122103=CARTESIAN_POINT('Ctrl Pts',(17.1943909934554,-21.140939195026,-12.6734106577147));
#122104=CARTESIAN_POINT('Ctrl Pts',(16.0600873898727,-18.8422637436558,
-12.8005864643961));
#122105=CARTESIAN_POINT('Ctrl Pts',(17.3789326443482,-16.6442644964813,
-12.9277622710776));
#122106=CARTESIAN_POINT('Ctrl Pts',(19.9409680926688,-16.563469339566,-13.054938077759));
#122107=CARTESIAN_POINT('Ctrl Pts',(21.3956852288542,-18.6740028146668,
-13.1821138844404));
#122108=CARTESIAN_POINT('Ctrl Pts',(20.4084713703825,-21.0395814528595,
-13.3092896911219));
#122109=CARTESIAN_POINT('Ctrl Pts',(17.8850339589992,-21.4899336779714,
-13.4364654978033));
#122110=CARTESIAN_POINT('Ctrl Pts',(16.1404701974589,-19.6118892754737,
-13.5636413044848));
#122111=CARTESIAN_POINT('Ctrl Pts',(16.7753090571362,-17.1284374200765,
-13.6908171111662));
#122112=CARTESIAN_POINT('Ctrl Pts',(19.2071252868205,-16.3179910487006,
-13.8179929178476));
#122113=CARTESIAN_POINT('Ctrl Pts',(21.2048784313142,-17.9240844051089,
-13.945168724529));
#122114=CARTESIAN_POINT('Ctrl Pts',(20.9357539750881,-20.4732265201925,
-14.0723445312105));
#122115=CARTESIAN_POINT('Ctrl Pts',(18.6466569029825,-21.6267377209658,
-14.1995203378919));
#122116=CARTESIAN_POINT('Ctrl Pts',(16.4376917012663,-20.3263430756987,
-14.3266961445733));
#122117=CARTESIAN_POINT('Ctrl Pts',(16.3354468386715,-17.7650739598295,
-14.4538719512548));
#122118=CARTESIAN_POINT('Ctrl Pts',(18.4337256305968,-16.2927358168784,
-14.5810477579362));
#122119=CARTESIAN_POINT('Ctrl Pts',(20.8074875193202,-17.2601075093917,
-14.7082235646177));
#122120=CARTESIAN_POINT('Ctrl Pts',(21.2789533042171,-19.7796855513471,
-14.8353993712991));
#122121=CARTESIAN_POINT('Ctrl Pts',(19.4155823901109,-21.5399134719006,
-14.9625751779805));
#122122=CARTESIAN_POINT('Ctrl Pts',(16.9269019368522,-20.9258914060103,
-15.089750984662));
#122123=CARTESIAN_POINT('Ctrl Pts',(16.0961217953763,-18.5009464886232,
-15.2169267913434));
#122124=CARTESIAN_POINT('Ctrl Pts',(17.6854311814566,-16.489815172386,-15.3441025980248));
#122125=CARTESIAN_POINT('Ctrl Pts',(20.2367373770296,-16.7375856150594,
-15.4712784047062));
#122126=CARTESIAN_POINT('Ctrl Pts',(21.4093752995786,-19.0169438138584,
-15.5984542113877));
#122127=CARTESIAN_POINT('Ctrl Pts',(20.1275224372825,-21.2367200943101,
-15.7256300180691));
#122128=CARTESIAN_POINT('Ctrl Pts',(17.5671992305365,-21.3604074939539,
-15.8528058247506));
#122129=CARTESIAN_POINT('Ctrl Pts',(16.0773433099501,-19.2745305005226,
-15.979981631432));
#122130=CARTESIAN_POINT('Ctrl Pts',(17.0248050117741,-16.8927517913624,
-16.1071574381134));
#122131=CARTESIAN_POINT('Ctrl Pts',(19.5403470306901,-16.4002055022689,
-16.2343332447949));
#122132=CARTESIAN_POINT('Ctrl Pts',(21.3161156964891,-18.2487722826149,
-16.3615090514763));
#122133=CARTESIAN_POINT('Ctrl Pts',(20.7229534749337,-20.7425068464271,
-16.4886848581577));
#122134=CARTESIAN_POINT('Ctrl Pts',(18.3050498885018,-21.5935625100306,
-16.6158606648392));
#122135=CARTESIAN_POINT('Ctrl Pts',(16.2806814057228,-20.021148524541,-16.7430364715206));
#122136=CARTESIAN_POINT('Ctrl Pts',(16.5070804630683,-17.4678571266262,
-16.870212278202));
#122137=CARTESIAN_POINT('Ctrl Pts',(18.776539977334,-16.2761746987364,-16.9973880848835));
#122138=CARTESIAN_POINT('Ctrl Pts',(21.0069717027245,-17.5393959043074,
-17.1245638915649));
#122139=CARTESIAN_POINT('Ctrl Pts',(21.1520929673995,-20.0985936915781,
-17.2517396982463));
#122140=CARTESIAN_POINT('Ctrl Pts',(19.0787640182614,-21.6058629324566,
-17.3789155049278));
#122141=CARTESIAN_POINT('Ctrl Pts',(16.6891354808367,-20.6783776501158,
-17.5060913116092));
#122142=CARTESIAN_POINT('Ctrl Pts',(16.1755432211384,-18.1670480248764,
-17.6332671182907));
#122143=CARTESIAN_POINT('Ctrl Pts',(18.0091762603091,-16.3758631171963,
-17.760442924972));
#122144=CARTESIAN_POINT('Ctrl Pts',(20.5077900930114,-16.9481239064058,
-17.8876187316535));
#122145=CARTESIAN_POINT('Ctrl Pts',(21.3790616092047,-19.3588166369015,
-18.0147945383349));
#122146=CARTESIAN_POINT('Ctrl Pts',(19.8236532699919,-21.3962803529462,
-18.1419703450164));
#122147=CARTESIAN_POINT('Ctrl Pts',(17.2685556870694,-21.1912685542763,
-18.2691461516978));
#122148=CARTESIAN_POINT('Ctrl Pts',(16.0579123055315,-18.931866841806,-18.3963219583793));
#122149=CARTESIAN_POINT('Ctrl Pts',(17.3024132869284,-16.6909360522447,
-18.5234977650607));
#122150=CARTESIAN_POINT('Ctrl Pts',(19.8603062232868,-16.5243910975421,
-18.6506735717421));
#122151=CARTESIAN_POINT('Ctrl Pts',(21.3848831062071,-18.5850266359637,
-18.7778493784235));
#122152=CARTESIAN_POINT('Ctrl Pts',(20.4774392715833,-20.9823374598767,
-18.905025185105));
#122153=CARTESIAN_POINT('Ctrl Pts',(17.9704981152505,-21.5169396795275,
-19.0322009917864));
#122154=CARTESIAN_POINT('Ctrl Pts',(16.164022550051,-19.6983689447528,-19.1593767984678));
#122155=CARTESIAN_POINT('Ctrl Pts',(16.7153417841063,-17.1950510214384,
-19.2865526051493));
#122156=CARTESIAN_POINT('Ctrl Pts',(19.1186546397307,-16.3036247501402,
-19.4137284118307));
#122157=CARTESIAN_POINT('Ctrl Pts',(21.1690707367099,-17.8419183693358,
-19.5409042185122));
#122158=CARTESIAN_POINT('Ctrl Pts',(20.9854605723195,-20.3986430325311,
-19.6680800251936));
#122159=CARTESIAN_POINT('Ctrl Pts',(18.7362750703233,-21.6281624110196,
-19.795255831875));
#122160=CARTESIAN_POINT('Ctrl Pts',(16.4850023400387,-20.4024690544242,
-19.9224316385565));
#122161=CARTESIAN_POINT('Ctrl Pts',(16.2970453597273,-17.8460600281632,
-20.0496074452379));
#122162=CARTESIAN_POINT('Ctrl Pts',(18.3448430353522,-16.3042829359788,
-20.1767832519193));
#122163=CARTESIAN_POINT('Ctrl Pts',(20.7496680183763,-17.1916206571837,
-20.3039590586007));
#122164=CARTESIAN_POINT('Ctrl Pts',(21.305242804797,-19.6939995862426,-20.4311348652822));
#122165=CARTESIAN_POINT('Ctrl Pts',(19.5018617071349,-21.5156352807657,
-20.5583106719636));
#122166=CARTESIAN_POINT('Ctrl Pts',(16.9940155374735,-20.9853037174782,
-20.6854864786451));
#122167=CARTESIAN_POINT('Ctrl Pts',(16.082496373835,-18.5895248604405,-20.8126622853265));
#122168=CARTESIAN_POINT('Ctrl Pts',(17.6035686476012,-16.5263278496229,
-20.9398380920079));
#122169=CARTESIAN_POINT('Ctrl Pts',(20.1617387665729,-16.6884701127161,
-21.0670138986894));
#122170=CARTESIAN_POINT('Ctrl Pts',(21.4100524978415,-18.9273846007665,
-21.1941897053708));
#122171=CARTESIAN_POINT('Ctrl Pts',(20.2032439132434,-21.1886431483515,
-21.3213655120522));
#122172=CARTESIAN_POINT('Ctrl Pts',(17.6485149801115,-21.3983811058473,
-21.4485413187337));
#122173=CARTESIAN_POINT('Ctrl Pts',(16.0896130221739,-19.3628281760474,
-21.5757171254151));
#122174=CARTESIAN_POINT('Ctrl Pts',(16.9568464474972,-16.9520802407969,
-21.7028929320966));
#122175=CARTESIAN_POINT('Ctrl Pts',(19.4543556739431,-16.3728024035369,
-21.8300687387779));
#122176=CARTESIAN_POINT('Ctrl Pts',(21.291629173971,-18.1667325047092,-21.9572632030605));
#122177=CARTESIAN_POINT('Ctrl Pts',(20.9507809654552,-19.8331818652868,
-22.0420657317825));
#122178=CARTESIAN_POINT('Ctrl Pts',(20.4651725960397,-20.4098092014579,
-22.084476324944));
#122179=CARTESIAN_POINT('Ctrl Pts',(18.187758406819,-20.9933731243335,0.257964216091064));
#122180=CARTESIAN_POINT('Ctrl Pts',(17.5080924453001,-20.811504453082,0.215572280530586));
#122181=CARTESIAN_POINT('Ctrl Pts',(16.3565579911106,-19.7184732651834,
0.13078840940963));
#122182=CARTESIAN_POINT('Ctrl Pts',(16.8032830955771,-17.3632042941351,
0.00361260272819585));
#122183=CARTESIAN_POINT('Ctrl Pts',(19.0246114919716,-16.4708792426415,
-0.123563203953239));
#122184=CARTESIAN_POINT('Ctrl Pts',(20.9776563709031,-17.8521967105185,
-0.250739010634673));
#122185=CARTESIAN_POINT('Ctrl Pts',(20.8731456437434,-20.2438673718189,
-0.377914817316107));
#122186=CARTESIAN_POINT('Ctrl Pts',(18.805655820692,-21.4496297959928,-0.505090623997542));
#122187=CARTESIAN_POINT('Ctrl Pts',(16.6726574870295,-20.3643350548799,
-0.632266430678976));
#122188=CARTESIAN_POINT('Ctrl Pts',(16.4306929665323,-17.9831221260791,
-0.75944223736041));
#122189=CARTESIAN_POINT('Ctrl Pts',(18.3019319614957,-16.490892293676,-0.886618044041845));
#122190=CARTESIAN_POINT('Ctrl Pts',(20.5695342500862,-17.2565252862285,
-1.01379385072328));
#122191=CARTESIAN_POINT('Ctrl Pts',(21.1531645592934,-19.5776774271649,
-1.14096965740471));
#122192=CARTESIAN_POINT('Ctrl Pts',(19.5173528337202,-21.3247956983873,
-1.26814546408615));
#122193=CARTESIAN_POINT('Ctrl Pts',(17.1628680192514,-20.8950282794151,
-1.39532127076758));
#122194=CARTESIAN_POINT('Ctrl Pts',(16.249796938349,-18.6826493324063,-1.52249707744901));
#122195=CARTESIAN_POINT('Ctrl Pts',(17.6158291954999,-16.7173848145856,
-1.64967288413045));
#122196=CARTESIAN_POINT('Ctrl Pts',(20.0077131332437,-16.8022400426472,
-1.77684869081188));
#122197=CARTESIAN_POINT('Ctrl Pts',(21.2310446542488,-18.8593671166236,
-1.90402449749332));
#122198=CARTESIAN_POINT('Ctrl Pts',(20.1634925191223,-21.0014788448218,
-2.03120030417475));
#122199=CARTESIAN_POINT('Ctrl Pts',(17.784469810194,-21.2633210763656,-2.15837611085619));
#122200=CARTESIAN_POINT('Ctrl Pts',(16.2765820701628,-19.4046696052546,
-2.28555191753762));
#122201=CARTESIAN_POINT('Ctrl Pts',(17.0232227799449,-17.1307219044541,
-2.41272772421906));
#122202=CARTESIAN_POINT('Ctrl Pts',(19.3393953939956,-16.5276837957002,
-2.53990353090049));
#122203=CARTESIAN_POINT('Ctrl Pts',(21.1001553155256,-18.148805344399,-2.66707933758192));
#122204=CARTESIAN_POINT('Ctrl Pts',(20.6901145919042,-20.5068081325184,
-2.79425514426337));
#122205=CARTESIAN_POINT('Ctrl Pts',(18.4854601420967,-21.4383709640324,
-2.92143095094479));
#122206=CARTESIAN_POINT('Ctrl Pts',(16.5088255848986,-20.0888427562296,
-3.04860675762623));
#122207=CARTESIAN_POINT('Ctrl Pts',(16.5736504441196,-17.6963318807336,
-3.17578256430766));
#122208=CARTESIAN_POINT('Ctrl Pts',(18.6204619342047,-16.4558185687336,
-3.3029583709891));
#122209=CARTESIAN_POINT('Ctrl Pts',(20.7714375528147,-17.5053967896241,
-3.43013417767053));
#122210=CARTESIAN_POINT('Ctrl Pts',(21.0531906742887,-19.8821436696115,
-3.55730998435197));
#122211=CARTESIAN_POINT('Ctrl Pts',(19.2072302973436,-21.4055414640101,
-3.6844857910334));
#122212=CARTESIAN_POINT('Ctrl Pts',(16.9271104945531,-20.6779672491097,
-3.81166159771483));
#122213=CARTESIAN_POINT('Ctrl Pts',(16.3046996648085,-18.3669252087745,
-3.93883740439627));
#122214=CARTESIAN_POINT('Ctrl Pts',(17.9110211132137,-16.5926529755442,
-4.0660132110777));
#122215=CARTESIAN_POINT('Ctrl Pts',(20.2723746104174,-16.9829351996645,
-4.19318901775914));
#122216=CARTESIAN_POINT('Ctrl Pts',(21.2223648848585,-19.179712164146,-4.32036482444056));
#122217=CARTESIAN_POINT('Ctrl Pts',(19.8894348227856,-21.1675773514354,
-4.44754063112201));
#122218=CARTESIAN_POINT('Ctrl Pts',(17.4964650251793,-21.1227878330214,
-4.57471643780344));
#122219=CARTESIAN_POINT('Ctrl Pts',(16.2388567568882,-19.0864352120986,
-4.70189224448488));
#122220=CARTESIAN_POINT('Ctrl Pts',(17.2703875480967,-16.9267466280655,
-4.8290680511663));
#122221=CARTESIAN_POINT('Ctrl Pts',(19.6446919218926,-16.6251023113816,
-4.95624385784775));
#122222=CARTESIAN_POINT('Ctrl Pts',(21.1834929812674,-18.4582422004466,
-5.08341966452918));
#122223=CARTESIAN_POINT('Ctrl Pts',(20.4750362630098,-20.7443742245365,
-5.21059547121061));
#122224=CARTESIAN_POINT('Ctrl Pts',(18.1692868343382,-21.386114144905,-5.33777127789205));
#122225=CARTESIAN_POINT('Ctrl Pts',(16.3816266851093,-19.7947054154853,
-5.46494708457348));
#122226=CARTESIAN_POINT('Ctrl Pts',(16.7521230475383,-17.4301667715549,
-5.59212289125491));
#122227=CARTESIAN_POINT('Ctrl Pts',(18.9408685046945,-16.4618156591,-5.71929869793635));
#122228=CARTESIAN_POINT('Ctrl Pts',(20.9398249485008,-17.7780541211498,
-5.84647450461778));
#122229=CARTESIAN_POINT('Ctrl Pts',(20.9150739109944,-20.1713150637459,
-5.97365031129922));
#122230=CARTESIAN_POINT('Ctrl Pts',(18.8893229328647,-21.4459301145832,
-6.10082611798065));
#122231=CARTESIAN_POINT('Ctrl Pts',(16.7210728042601,-20.4325190760503,
-6.22800192466209));
#122232=CARTESIAN_POINT('Ctrl Pts',(16.3995584413949,-18.0608236766186,
-6.35517773134351));
#122233=CARTESIAN_POINT('Ctrl Pts',(18.2197493167659,-16.5067272412486,
-6.48235353802496));
#122234=CARTESIAN_POINT('Ctrl Pts',(20.5117332760072,-17.1960167912891,
-6.60952934470639));
#122235=CARTESIAN_POINT('Ctrl Pts',(21.1727572930827,-19.4963119467122,
-6.73670515138783));
#122236=CARTESIAN_POINT('Ctrl Pts',(19.5963728601034,-21.2972346748364,
-6.86388095806926));
#122237=CARTESIAN_POINT('Ctrl Pts',(17.2288148528754,-20.9465501504785,
-6.99105676475069));
#122238=CARTESIAN_POINT('Ctrl Pts',(16.2421707958078,-18.7659896588004,
-7.11823257143212));
#122239=CARTESIAN_POINT('Ctrl Pts',(17.5416253732237,-16.7560821100692,
-7.24540837811357));
#122240=CARTESIAN_POINT('Ctrl Pts',(19.935009663591,-16.7607929313141,-7.37258418479499));
#122241=CARTESIAN_POINT('Ctrl Pts',(21.2265421306802,-18.7758002364295,
-7.49975999147643));
#122242=CARTESIAN_POINT('Ctrl Pts',(20.2313218974823,-20.9524598884302,
-7.62693579815786));
#122243=CARTESIAN_POINT('Ctrl Pts',(17.8624017576224,-21.2938217553397,
-7.7541116048393));
#122244=CARTESIAN_POINT('Ctrl Pts',(16.2931189076558,-19.4867075115756,
-7.88128741152073));
#122245=CARTESIAN_POINT('Ctrl Pts',(16.9631929617487,-17.189032313632,-8.00846321820217));
#122246=CARTESIAN_POINT('Ctrl Pts',(19.2578725647568,-16.5087705458158,
-8.1356390248836));
#122247=CARTESIAN_POINT('Ctrl Pts',(21.0719316047989,-18.0700201582916,
-8.26281483156504));
#122248=CARTESIAN_POINT('Ctrl Pts',(20.7410835058385,-20.440431533692,-8.38999063824647));
#122249=CARTESIAN_POINT('Ctrl Pts',(18.5688608639229,-21.4452993594099,
-8.5171664449279));
#122250=CARTESIAN_POINT('Ctrl Pts',(16.5481431296672,-20.1627197744802,
-8.64434225160934));
#122251=CARTESIAN_POINT('Ctrl Pts',(16.5328134043638,-17.7693799422089,
-8.77151805829078));
#122252=CARTESIAN_POINT('Ctrl Pts',(18.5369357595085,-16.461020611282,-8.89869386497221));
#122253=CARTESIAN_POINT('Ctrl Pts',(20.7218523241179,-17.4379802618865,
-9.02586967165363));
#122254=CARTESIAN_POINT('Ctrl Pts',(21.0830377613791,-19.8039590515472,
-9.15304547833508));
#122255=CARTESIAN_POINT('Ctrl Pts',(19.2891268503013,-21.3883182899558,
-9.28022128501651));
#122256=CARTESIAN_POINT('Ctrl Pts',(16.9859215091302,-20.7375067122967,
-9.40739709169795));
#122257=CARTESIAN_POINT('Ctrl Pts',(16.2864696853447,-18.4486035471504,
-9.53457289837939));
#122258=CARTESIAN_POINT('Ctrl Pts',(17.8324750143917,-16.621535383186,-9.6617487050608));
#122259=CARTESIAN_POINT('Ctrl Pts',(20.2055735627832,-16.9325238602014,
-9.78892451174226));
#122260=CARTESIAN_POINT('Ctrl Pts',(21.2285947034771,-19.0962563526568,
-9.91610031842368));
#122261=CARTESIAN_POINT('Ctrl Pts',(19.9629800357399,-21.1276425951086,
-10.0432761251051));
#122262=CARTESIAN_POINT('Ctrl Pts',(17.569852464315,-21.1630117921569,-10.1704519317865));
#122263=CARTESIAN_POINT('Ctrl Pts',(16.2447580017361,-19.1699149007699,
-10.297627738468));
#122264=CARTESIAN_POINT('Ctrl Pts',(17.2033885727816,-16.9768946132505,
-10.4248035451494));
#122265=CARTESIAN_POINT('Ctrl Pts',(19.5662601278407,-16.5959109292081,
-10.5519793518308));
#122266=CARTESIAN_POINT('Ctrl Pts',(21.1655846714952,-18.3764927322373,
-10.6791551585123));
#122267=CARTESIAN_POINT('Ctrl Pts',(20.5340812002182,-20.6850667334291,
-10.8063309651937));
#122268=CARTESIAN_POINT('Ctrl Pts',(18.2511149533807,-21.4036595729525,
-10.9335067718751));
#122269=CARTESIAN_POINT('Ctrl Pts',(16.4111657655901,-19.8730069214463,
-11.0606825785565));
#122270=CARTESIAN_POINT('Ctrl Pts',(16.7022728165186,-17.4973875836496,
-11.187858385238));
#122271=CARTESIAN_POINT('Ctrl Pts',(18.8573634550803,-16.4562848544257,
-11.3150341919194));
#122272=CARTESIAN_POINT('Ctrl Pts',(20.8992757804055,-17.7048458697147,
-11.4422099986009));
#122273=CARTESIAN_POINT('Ctrl Pts',(20.9546819693801,-20.0975933924253,
-11.5693858052823));
#122274=CARTESIAN_POINT('Ctrl Pts',(18.9727502825159,-21.4393300811306,
-11.6965616119637));
#122275=CARTESIAN_POINT('Ctrl Pts',(16.7717800299571,-20.4990958015143,
-11.8237374186452));
#122276=CARTESIAN_POINT('Ctrl Pts',(16.3710248108061,-18.1394971476037,
-11.9509132253266));
#122277=CARTESIAN_POINT('Ctrl Pts',(18.1381526649597,-16.5253194311522,
-12.078089032008));
#122278=CARTESIAN_POINT('Ctrl Pts',(20.4519334665563,-17.137470519836,-12.2052648386895));
#122279=CARTESIAN_POINT('Ctrl Pts',(21.1896169395636,-19.4143397841694,
-12.3324406453709));
#122280=CARTESIAN_POINT('Ctrl Pts',(19.6744242832976,-21.2670409925706,
-12.4596164520523));
#122281=CARTESIAN_POINT('Ctrl Pts',(17.2964507164198,-20.9958357779372,
-12.5867922587338));
#122282=CARTESIAN_POINT('Ctrl Pts',(16.2373393928556,-18.8495380918013,
-12.7139680654152));
#122283=CARTESIAN_POINT('Ctrl Pts',(17.4687592161129,-16.7972428469345,
-12.8411438720966));
#122284=CARTESIAN_POINT('Ctrl Pts',(19.8609589288869,-16.7218035506933,
-12.9683196787781));
#122285=CARTESIAN_POINT('Ctrl Pts',(21.219243771367,-18.6924310750883,-13.0954954854595));
#122286=CARTESIAN_POINT('Ctrl Pts',(20.2974717052425,-20.9011969774254,
-13.222671292141));
#122287=CARTESIAN_POINT('Ctrl Pts',(17.9413113895561,-21.3216956337831,
-13.3498470988224));
#122288=CARTESIAN_POINT('Ctrl Pts',(16.3123936741481,-19.5681456260435,
-13.4770229055038));
#122289=CARTESIAN_POINT('Ctrl Pts',(16.9051494608697,-17.2493202487194,
-13.6041987121852));
#122290=CARTESIAN_POINT('Ctrl Pts',(19.1757621059772,-16.4925978629714,
-13.7313745188667));
#122291=CARTESIAN_POINT('Ctrl Pts',(21.0410854376991,-17.9922242902351,
-13.8585503255481));
#122292=CARTESIAN_POINT('Ctrl Pts',(20.7898010742036,-20.3723853608092,
-13.9857261322295));
#122293=CARTESIAN_POINT('Ctrl Pts',(18.6524468225313,-21.449431021899,-14.112901938911));
#122294=CARTESIAN_POINT('Ctrl Pts',(16.5899125494253,-20.2352387284471,
-14.2400777455924));
#122295=CARTESIAN_POINT('Ctrl Pts',(16.4944454351463,-17.8437545484231,
-14.3672535522739));
#122296=CARTESIAN_POINT('Ctrl Pts',(18.4536306316875,-16.4690167847506,
-14.4944293589553));
#122297=CARTESIAN_POINT('Ctrl Pts',(20.67003732197,-17.3722620097506,-14.6216051656367));
#122298=CARTESIAN_POINT('Ctrl Pts',(21.1102499333731,-19.7248187912068,
-14.7487809723181));
#122299=CARTESIAN_POINT('Ctrl Pts',(19.3704007176106,-21.3683622982746,
-14.8759567789996));
#122300=CARTESIAN_POINT('Ctrl Pts',(17.0466933429237,-20.7950433730338,
-15.003132585681));
#122301=CARTESIAN_POINT('Ctrl Pts',(16.2709851000421,-18.5308465452073,
-15.1303083923625));
#122302=CARTESIAN_POINT('Ctrl Pts',(17.7549401559266,-16.6530318724217,
-15.2574841990439));
#122303=CARTESIAN_POINT('Ctrl Pts',(20.137121851441,-16.8843777666347,-15.3846600057253));
#122304=CARTESIAN_POINT('Ctrl Pts',(21.2320263358222,-19.0126387288515,
-15.5118358124068));
#122305=CARTESIAN_POINT('Ctrl Pts',(20.0351467020866,-21.085267421011,-15.6390116190882));
#122306=CARTESIAN_POINT('Ctrl Pts',(17.6445457274587,-21.2007556599016,
-15.7661874257696));
#122307=CARTESIAN_POINT('Ctrl Pts',(16.2534514287292,-19.2531501543497,
-15.893363232451));
#122308=CARTESIAN_POINT('Ctrl Pts',(17.1381064839328,-17.0292580736685,
-16.0205390391325));
#122309=CARTESIAN_POINT('Ctrl Pts',(19.4868947878054,-16.5693623715735,
-16.1477148458139));
#122310=CARTESIAN_POINT('Ctrl Pts',(21.1449488537871,-18.2953888103906,
-16.2748906524954));
#122311=CARTESIAN_POINT('Ctrl Pts',(20.5911069867814,-20.6238152617876,
-16.4020664591768));
#122312=CARTESIAN_POINT('Ctrl Pts',(18.3334847244627,-21.4184549750521,
-16.5292422658582));
#122313=CARTESIAN_POINT('Ctrl Pts',(16.4433103686679,-19.950275334167,-16.6564180725397));
#122314=CARTESIAN_POINT('Ctrl Pts',(16.6547015733873,-17.5662400341386,
-16.7835938792211));
#122315=CARTESIAN_POINT('Ctrl Pts',(18.7737200287087,-16.4535534928245,
-16.9107696859025));
#122316=CARTESIAN_POINT('Ctrl Pts',(20.8562978229928,-17.633036550765,-17.037945492584));
#122317=CARTESIAN_POINT('Ctrl Pts',(20.9917990893397,-20.0225867092743,
-17.1651212992654));
#122318=CARTESIAN_POINT('Ctrl Pts',(19.0559098260331,-21.4299400101298,
-17.2922971059468));
#122319=CARTESIAN_POINT('Ctrl Pts',(16.8246882773183,-20.563937149993,-17.4194729126283));
#122320=CARTESIAN_POINT('Ctrl Pts',(16.3451417289135,-18.2190820028416,
-17.5466487193097));
#122321=CARTESIAN_POINT('Ctrl Pts',(18.0572243749645,-16.5466336280595,
-17.6738245259911));
#122322=CARTESIAN_POINT('Ctrl Pts',(20.3902066515531,-17.0809596056631,
-17.8010003326726));
#122323=CARTESIAN_POINT('Ctrl Pts',(21.2037221211194,-19.3318490151982,
-17.928176139354));
#122324=CARTESIAN_POINT('Ctrl Pts',(19.7514208328018,-21.2342505293946,
-18.0553519460354));
#122325=CARTESIAN_POINT('Ctrl Pts',(17.3656990786459,-21.0428288352822,
-18.1825277527169));
#122326=CARTESIAN_POINT('Ctrl Pts',(16.2353084935018,-18.9332014563341,
-18.3097035593983));
#122327=CARTESIAN_POINT('Ctrl Pts',(17.3973122792794,-16.8408205743096,
-18.4368793660797));
#122328=CARTESIAN_POINT('Ctrl Pts',(19.7856440846313,-16.6853157810153,
-18.5640551727612));
#122329=CARTESIAN_POINT('Ctrl Pts',(21.2091577147082,-18.6093530719028,
-18.6912309794426));
#122330=CARTESIAN_POINT('Ctrl Pts',(20.3618677671906,-20.8477476531151,
-18.8184067861241));
#122331=CARTESIAN_POINT('Ctrl Pts',(18.0211101800729,-21.3469114243016,
-18.9455825928055));
#122332=CARTESIAN_POINT('Ctrl Pts',(16.3343847559432,-19.6488926118612,
-19.072758399487));
#122333=CARTESIAN_POINT('Ctrl Pts',(16.849157381052,-17.3115180758999,-19.1999342061683));
#122334=CARTESIAN_POINT('Ctrl Pts',(19.0931561230287,-16.4791838974025,
-19.3271100128498));
#122335=CARTESIAN_POINT('Ctrl Pts',(21.0076514128875,-17.9155049898426,
-19.4542858195312));
#122336=CARTESIAN_POINT('Ctrl Pts',(20.8362126520363,-20.3027459661324,
-19.5814616262127));
#122337=CARTESIAN_POINT('Ctrl Pts',(18.7361242573274,-21.4507612701356,
-19.7086374328941));
#122338=CARTESIAN_POINT('Ctrl Pts',(16.6340869953943,-20.3063183634152,
-19.8358132395755));
#122339=CARTESIAN_POINT('Ctrl Pts',(16.4585895663445,-17.9193721006837,
-19.9629890462569));
#122340=CARTESIAN_POINT('Ctrl Pts',(18.3706400083713,-16.4797984525115,
-20.0901648529384));
#122341=CARTESIAN_POINT('Ctrl Pts',(20.6160506397633,-17.3083151083569,
-20.2173406596198));
#122342=CARTESIAN_POINT('Ctrl Pts',(21.1347967193193,-19.6448128954076,
-20.3445164663014));
#122343=CARTESIAN_POINT('Ctrl Pts',(19.4509606323997,-21.3456934933219,
-20.4716922729828));
#122344=CARTESIAN_POINT('Ctrl Pts',(17.1093580247237,-20.8505172793461,
-20.5988680796641));
#122345=CARTESIAN_POINT('Ctrl Pts',(16.2582628992159,-18.6135531118782,
-20.7260438863456));
#122346=CARTESIAN_POINT('Ctrl Pts',(17.6785042384983,-16.6871241470058,
-20.853219693027));
#122347=CARTESIAN_POINT('Ctrl Pts',(20.0670948522008,-16.8385181003778,
-20.9803954997085));
#122348=CARTESIAN_POINT('Ctrl Pts',(21.2326586430337,-18.9290163402638,
-21.1075713063899));
#122349=CARTESIAN_POINT('Ctrl Pts',(20.1058486485267,-21.0403774658824,
-21.2347471130714));
#122350=CARTESIAN_POINT('Ctrl Pts',(17.7204711065961,-21.2362120246932,
-21.3619229197528));
#122351=CARTESIAN_POINT('Ctrl Pts',(16.264907789365,-19.3355946319105,-21.4890987264342));
#122352=CARTESIAN_POINT('Ctrl Pts',(17.0746528505921,-17.0846536771093,
-21.6162745331156));
#122353=CARTESIAN_POINT('Ctrl Pts',(19.4066037445858,-16.543775807204,-21.743450339797));
#122354=CARTESIAN_POINT('Ctrl Pts',(21.1220855276092,-18.2187873983098,
-21.8706448040796));
#122355=CARTESIAN_POINT('Ctrl Pts',(20.8038319347303,-19.7747688677855,
-21.9554473328015));
#122356=CARTESIAN_POINT('Ctrl Pts',(20.3504142419353,-20.3131719366696,
-21.9978579259631));
#122357=CARTESIAN_POINT('Ctrl Pts',(18.0722627314315,-21.4249949024184,
8.33751470641353E-16));
#122358=CARTESIAN_POINT('Ctrl Pts',(17.9903580532758,-21.3953391176122,
-1.14232169905555E-14));
#122359=CARTESIAN_POINT('Ctrl Pts',(17.9103568112513,-21.3612556170403,
-1.32314169705265E-14));
#122360=CARTESIAN_POINT('Ctrl Pts',(17.8324629519401,-21.3230651201994,
1.30451205393456E-15));
#122361=CARTESIAN_POINT('Ctrl Pts',(17.7532833251897,-21.2842442258181,
1.60803807142514E-14));
#122362=CARTESIAN_POINT('Ctrl Pts',(17.6762805476582,-21.2411789324033,
2.98180794711572E-15));
#122363=CARTESIAN_POINT('Ctrl Pts',(17.6016979156742,-21.1941602566503,
-2.64718802434061E-15));
#122364=CARTESIAN_POINT('Ctrl Pts',(17.5268866858286,-21.1469974673358,
-8.29343702652826E-15));
#122365=CARTESIAN_POINT('Ctrl Pts',(17.4545098273189,-21.0958562232523,
8.2392653840351E-15));
#122366=CARTESIAN_POINT('Ctrl Pts',(17.384851733613,-21.0409959626311,1.8547663405144E-14));
#122367=CARTESIAN_POINT('Ctrl Pts',(17.3596729290768,-21.0211660232012,
2.22737650689451E-14));
#122368=CARTESIAN_POINT('Ctrl Pts',(17.3348497590583,-21.0008499098516,
1.90970525389729E-14));
#122369=CARTESIAN_POINT('Ctrl Pts',(17.3103971449292,-20.9800590889455,
1.05887520973624E-14));
#122370=CARTESIAN_POINT('Ctrl Pts',(17.2929747331899,-20.9652456935222,
4.71885765034174E-15));
#122371=CARTESIAN_POINT('Ctrl Pts',(17.2757404518089,-20.9501913039064,
6.92286535120819E-16));
#122372=CARTESIAN_POINT('Ctrl Pts',(17.2586999683651,-20.9348999714627,
1.49116829994966E-14));
#122373=CARTESIAN_POINT('Ctrl Pts',(17.2462568322336,-20.9237340833671,
2.52948324270246E-14));
#122374=CARTESIAN_POINT('Ctrl Pts',(17.2339149535825,-20.9124397717598,
2.54593689853369E-14));
#122375=CARTESIAN_POINT('Ctrl Pts',(17.2216943473019,-20.9010355554554,
1.92762472650543E-14));
#122376=CARTESIAN_POINT('Ctrl Pts',(17.1582585289398,-20.8418375273512,
-1.28966629608596E-14));
#122377=CARTESIAN_POINT('Ctrl Pts',(17.0979854521548,-20.7795917637398,
1.93414622705707E-14));
#122378=CARTESIAN_POINT('Ctrl Pts',(17.0411057216723,-20.7145765131159,
1.92346139016308E-14));
#122379=CARTESIAN_POINT('Ctrl Pts',(16.9845623465869,-20.6499457268742,
1.91283973750937E-14));
#122380=CARTESIAN_POINT('Ctrl Pts',(16.9313717910731,-20.5825772843607,
1.81649823445482E-14));
#122381=CARTESIAN_POINT('Ctrl Pts',(16.8818041708791,-20.5127177725785,
2.22044604925031E-16));
#122382=CARTESIAN_POINT('Ctrl Pts',(16.8334274591801,-20.4445367009903,
-1.72897972519719E-14));
#122383=CARTESIAN_POINT('Ctrl Pts',(16.7885013791326,-20.3739820606867,
-1.50387299598194E-15));
#122384=CARTESIAN_POINT('Ctrl Pts',(16.747324449976,-20.3012692713431,-7.63278329429795E-16));
#122385=CARTESIAN_POINT('Ctrl Pts',(16.7339895188709,-20.2777216184167,
-5.23440656792113E-16));
#122386=CARTESIAN_POINT('Ctrl Pts',(16.7210481787122,-20.2539475653132,
1.14141009925036E-15));
#122387=CARTESIAN_POINT('Ctrl Pts',(16.708511751901,-20.2299543047592,-1.69309011255336E-15));
#122388=CARTESIAN_POINT('Ctrl Pts',(16.6986550608892,-20.2110897463642,
-3.79685699442959E-15));
#122389=CARTESIAN_POINT('Ctrl Pts',(16.689048690518,-20.1920896772321,1.29326085042157E-14));
#122390=CARTESIAN_POINT('Ctrl Pts',(16.6796984128078,-20.1729575913137,
-3.7470027081099E-15));
#122391=CARTESIAN_POINT('Ctrl Pts',(16.673772461475,-20.1608321963725,-1.42576522322744E-14));
#122392=CARTESIAN_POINT('Ctrl Pts',(16.6679532034413,-20.1486615485784,
2.13653143515295E-14));
#122393=CARTESIAN_POINT('Ctrl Pts',(16.6622433073212,-20.1364502099952,
2.1538326677728E-14));
#122394=CARTESIAN_POINT('Ctrl Pts',(16.6271177740505,-20.0613297926252,
2.2817734385698E-14));
#122395=CARTESIAN_POINT('Ctrl Pts',(16.596105677901,-19.9846276360536,-1.38567986312105E-14));
#122396=CARTESIAN_POINT('Ctrl Pts',(16.5694538163414,-19.9065723114556,
-7.46624984060418E-15));
#122397=CARTESIAN_POINT('Ctrl Pts',(16.5428019547817,-19.8285169868576,
-3.91519935858294E-16));
#122398=CARTESIAN_POINT('Ctrl Pts',(16.5205098557042,-19.7491077644459,
1.50329598798952E-14));
#122399=CARTESIAN_POINT('Ctrl Pts',(16.502878625203,-19.66856395302,1.87905246917808E-14));
#122400=CARTESIAN_POINT('Ctrl Pts',(16.4850541528343,-19.5871373650609,
2.27955343740806E-14));
#122401=CARTESIAN_POINT('Ctrl Pts',(16.4719940148662,-19.5045499555443,
7.18569780110884E-15));
#122402=CARTESIAN_POINT('Ctrl Pts',(16.4636225525689,-19.4211931726568,
1.68198788230711E-14));
#122403=CARTESIAN_POINT('Ctrl Pts',(16.4601640820937,-19.3867563010228,
2.08538337015049E-14));
#122404=CARTESIAN_POINT('Ctrl Pts',(16.4575064389052,-19.3521882740751,
-1.67355792731723E-14));
#122405=CARTESIAN_POINT('Ctrl Pts',(16.4556467099008,-19.3175176204782,
-1.34892097491957E-14));
#122406=CARTESIAN_POINT('Ctrl Pts',(16.4549147504963,-19.3038718092329,
-1.22694028264887E-14));
#122407=CARTESIAN_POINT('Ctrl Pts',(16.4543064087743,-19.2902081093511,
1.29130876272536E-14));
#122408=CARTESIAN_POINT('Ctrl Pts',(16.4538219778623,-19.2765459176976,
1.27398092075737E-14));
#122409=CARTESIAN_POINT('Ctrl Pts',(16.4509249680159,-19.194842824923,1.16962727565706E-14));
#122410=CARTESIAN_POINT('Ctrl Pts',(16.4524464982906,-19.1130624309727,
8.72830971514544E-15));
#122411=CARTESIAN_POINT('Ctrl Pts',(16.458252360817,-19.0315664983848,-5.74540415243519E-15));
#122412=CARTESIAN_POINT('Ctrl Pts',(16.4640582233434,-18.9500705657969,
-2.02191180200158E-14));
#122413=CARTESIAN_POINT('Ctrl Pts',(16.474148825966,-18.868858075135,1.49310499479369E-14));
#122414=CARTESIAN_POINT('Ctrl Pts',(16.4884408456005,-18.7883024616738,
1.04360964314765E-14));
#122415=CARTESIAN_POINT('Ctrl Pts',(16.5025319927713,-18.7088790468066,
6.1238295247487E-15));
#122416=CARTESIAN_POINT('Ctrl Pts',(16.5207077570521,-18.6300932899197,
-1.34620945332921E-14));
#122417=CARTESIAN_POINT('Ctrl Pts',(16.5429310587135,-18.5523284952265,
1.63757896132211E-15));
#122418=CARTESIAN_POINT('Ctrl Pts',(16.5522282722733,-18.5197952598546,
7.80572654577075E-15));
#122419=CARTESIAN_POINT('Ctrl Pts',(16.5622343667201,-18.4874410976137,
4.24674998370723E-15));
#122420=CARTESIAN_POINT('Ctrl Pts',(16.572948601838,-18.4552959778321,1.74860126378462E-14));
#122421=CARTESIAN_POINT('Ctrl Pts',(16.578489270918,-18.4386727220153,2.43262322813947E-14));
#122422=CARTESIAN_POINT('Ctrl Pts',(16.5842201970324,-18.4221033375436,
-1.47712113728087E-14));
#122423=CARTESIAN_POINT('Ctrl Pts',(16.5901333946024,-18.4056133356731,
-1.04638520070921E-14));
#122424=CARTESIAN_POINT('Ctrl Pts',(16.6168665563098,-18.3310631652543,
9.11922743263435E-15));
#122425=CARTESIAN_POINT('Ctrl Pts',(16.6473525954954,-18.2580371498547,
2.59274245153824E-14));
#122426=CARTESIAN_POINT('Ctrl Pts',(16.6815326594994,-18.186894548015,5.71764857681956E-15));
#122427=CARTESIAN_POINT('Ctrl Pts',(16.7078448582386,-18.1321281708012,
-9.84006485838118E-15));
#122428=CARTESIAN_POINT('Ctrl Pts',(16.7363470804512,-18.0784782971011,
-1.13436528624218E-14));
#122429=CARTESIAN_POINT('Ctrl Pts',(16.7670276804213,-18.0261235050124,
-7.43849426498855E-15));
#122430=CARTESIAN_POINT('Ctrl Pts',(16.7762619506765,-18.01036571997,-6.04644969543337E-15));
#122431=CARTESIAN_POINT('Ctrl Pts',(16.7856936431618,-17.9947253587034,
4.29525693792424E-15));
#122432=CARTESIAN_POINT('Ctrl Pts',(16.795322651707,-17.9792075715296,2.3037127760972E-15));
#122433=CARTESIAN_POINT('Ctrl Pts',(16.8035475707392,-17.9659525679159,
4.3176325519934E-16));
#122434=CARTESIAN_POINT('Ctrl Pts',(16.8119141895608,-17.9527907636739,
4.11143789873392E-15));
#122435=CARTESIAN_POINT('Ctrl Pts',(16.8204178980527,-17.9397316712593,
3.41393580072236E-15));
#122436=CARTESIAN_POINT('Ctrl Pts',(16.8615694249279,-17.8765355265444,
-7.90562951105595E-16));
#122437=CARTESIAN_POINT('Ctrl Pts',(16.9059580734959,-17.8156943310143,
-1.38901968370523E-14));
#122438=CARTESIAN_POINT('Ctrl Pts',(16.9535504683774,-17.7575478141846,
-2.41473507855972E-15));
#122439=CARTESIAN_POINT('Ctrl Pts',(16.9976826813803,-17.7036288115269,
8.6369744883514E-15));
#122440=CARTESIAN_POINT('Ctrl Pts',(17.044570268779,-17.6520267822693,-9.3252529599055E-15));
#122441=CARTESIAN_POINT('Ctrl Pts',(17.0942091882108,-17.6030457893103,
-4.27435864480685E-15));
#122442=CARTESIAN_POINT('Ctrl Pts',(17.0997977486715,-17.5975313010074,
-3.76768770885319E-15));
#122443=CARTESIAN_POINT('Ctrl Pts',(17.10542120347,-17.592050073031,-7.85819778827449E-15));
#122444=CARTESIAN_POINT('Ctrl Pts',(17.1110791840834,-17.5866022544178,
-1.97064586870965E-14));
#122445=CARTESIAN_POINT('Ctrl Pts',(-17.1175855514924,-17.590827960842,
-0.00214194799035405));
#122446=CARTESIAN_POINT('Ctrl Pts',(-16.6641678381752,-18.1292310858663,
-0.0445525400540117));
#122447=CARTESIAN_POINT('Ctrl Pts',(-16.345912932243,-19.6852113602882,
-0.129355067678147));
#122448=CARTESIAN_POINT('Ctrl Pts',(-18.0613969831487,-21.3602251232166,
-0.256549530862762));
#122449=CARTESIAN_POINT('Ctrl Pts',(-20.393346844718,-20.8193459211516,
-0.383725337544195));
#122450=CARTESIAN_POINT('Ctrl Pts',(-21.203092563641,-18.5684056721843,
-0.510901144225632));
#122451=CARTESIAN_POINT('Ctrl Pts',(-19.7475288416972,-16.6677876400165,
-0.638076950907064));
#122452=CARTESIAN_POINT('Ctrl Pts',(-17.3621513300928,-16.8636225363617,
-0.765252757588499));
#122453=CARTESIAN_POINT('Ctrl Pts',(-16.2353411818156,-18.9749835879209,
-0.892428564269934));
#122454=CARTESIAN_POINT('Ctrl Pts',(-17.4009050866724,-21.0654820647258,
-1.01960437095136));
#122455=CARTESIAN_POINT('Ctrl Pts',(-19.7894958141682,-21.2168759594155,
-1.1467801776328));
#122456=CARTESIAN_POINT('Ctrl Pts',(-21.2097372485274,-19.2904469218172,
-1.27395598431423));
#122457=CARTESIAN_POINT('Ctrl Pts',(-20.3586420669921,-17.0534826027649,
-1.40113179099567));
#122458=CARTESIAN_POINT('Ctrl Pts',(-18.0170393273216,-16.558306372611,
-1.5283075976771));
#122459=CARTESIAN_POINT('Ctrl Pts',(-16.3332031410643,-18.2591870619742,
-1.65548340435853));
#122460=CARTESIAN_POINT('Ctrl Pts',(-16.8519492516291,-20.5956849881885,
-1.78265921103997));
#122461=CARTESIAN_POINT('Ctrl Pts',(-19.097360012485,-21.424201689821,-1.9098350177214));
#122462=CARTESIAN_POINT('Ctrl Pts',(-21.0094105654639,-19.9846279595186,
-2.03701082440284));
#122463=CARTESIAN_POINT('Ctrl Pts',(-20.8339131261131,-17.5976815579533,
-2.16418663108427));
#122464=CARTESIAN_POINT('Ctrl Pts',(-18.7318757425753,-16.4532385853486,
-2.29136243776571));
#122465=CARTESIAN_POINT('Ctrl Pts',(-16.6317872262606,-17.6012539556073,
-2.41853824444714));
#122466=CARTESIAN_POINT('Ctrl Pts',(-16.460348455506,-19.9884950701948,
-2.54571405112858));
#122467=CARTESIAN_POINT('Ctrl Pts',(-18.3748438561772,-21.4248162457191,
-2.67288985781001));
#122468=CARTESIAN_POINT('Ctrl Pts',(-20.6188427280565,-20.592482019073,
-2.80006566449145));
#122469=CARTESIAN_POINT('Ctrl Pts',(-21.1336153829609,-18.2551073477921,
-2.92724147117288));
#122470=CARTESIAN_POINT('Ctrl Pts',(-19.4468898611942,-16.5570884370688,
-3.05441727785431));
#122471=CARTESIAN_POINT('Ctrl Pts',(-17.1061321385776,-17.056252237145,
-3.18159308453575));
#122472=CARTESIAN_POINT('Ctrl Pts',(-16.2588421420139,-19.2946469479328,
-3.30876889121718));
#122473=CARTESIAN_POINT('Ctrl Pts',(-17.6823558544925,-21.2186843501945,
-3.43594469789862));
#122474=CARTESIAN_POINT('Ctrl Pts',(-20.0706877980967,-21.0631795478994,
-3.56312050458005));
#122475=CARTESIAN_POINT('Ctrl Pts',(-21.2326916511383,-18.970798544754,
-3.69029631126149));
#122476=CARTESIAN_POINT('Ctrl Pts',(-20.1023010005601,-16.8611710436873,
-3.81747211794292));
#122477=CARTESIAN_POINT('Ctrl Pts',(-17.7165791083032,-16.6697493384941,
-3.94464792462435));
#122478=CARTESIAN_POINT('Ctrl Pts',(-16.2642777359172,-18.5721509628136,
-4.07182373130579));
#122479=CARTESIAN_POINT('Ctrl Pts',(-17.077793252575,-20.8230405026448,
-4.19899953798722));
#122480=CARTESIAN_POINT('Ctrl Pts',(-19.4107756642115,-21.3573665111786,
-4.32617534466866));
#122481=CARTESIAN_POINT('Ctrl Pts',(-21.1228584093689,-19.6849180395844,
-4.45335115135009));
#122482=CARTESIAN_POINT('Ctrl Pts',(-20.6433118332049,-17.3400627566978,
-4.58052695803153));
#122483=CARTESIAN_POINT('Ctrl Pts',(-18.4120901553326,-16.474059846431,
-4.70770276471296));
#122484=CARTESIAN_POINT('Ctrl Pts',(-16.4762007799643,-17.8814132287533,
-4.8348785713944));
#122485=CARTESIAN_POINT('Ctrl Pts',(-16.6117020541549,-20.2709635255851,
-4.96205437807583));
#122486=CARTESIAN_POINT('Ctrl Pts',(-18.694279968992,-21.4504466518017,
-5.08923018475726));
#122487=CARTESIAN_POINT('Ctrl Pts',(-20.8132985469758,-20.3377600460781,
-5.2164059914387));
#122488=CARTESIAN_POINT('Ctrl Pts',(-21.0246897639318,-17.9537246080465,
-5.34358179812013));
#122489=CARTESIAN_POINT('Ctrl Pts',(-19.1345152987216,-16.4855448821736,
-5.47075760480157));
#122490=CARTESIAN_POINT('Ctrl Pts',(-16.8768929057173,-17.2801846414369,
-5.597933411483));
#122491=CARTESIAN_POINT('Ctrl Pts',(-16.3230510066515,-19.6086112276183,
-5.72510921816443));
#122492=CARTESIAN_POINT('Ctrl Pts',(-17.9811051686122,-21.3346377663488,
-5.85228502484587));
#122493=CARTESIAN_POINT('Ctrl Pts',(-20.3298936084476,-20.8747420376322,
-5.97946083152731));
#122494=CARTESIAN_POINT('Ctrl Pts',(-21.2145487148608,-18.6508498282177,
-6.10663663820873));
#122495=CARTESIAN_POINT('Ctrl Pts',(-19.8234543356058,-16.7032442099259,
-6.23381244489018));
#122496=CARTESIAN_POINT('Ctrl Pts',(-17.4328532225945,-16.8187324555017,
-6.36098825157161));
#122497=CARTESIAN_POINT('Ctrl Pts',(-16.2359735195759,-18.8913612676384,
-6.48816405825305));
#122498=CARTESIAN_POINT('Ctrl Pts',(-17.3308780673371,-21.0196223530527,
-6.61533986493447));
#122499=CARTESIAN_POINT('Ctrl Pts',(-19.7130599007477,-21.2509682606574,
-6.74251567161592));
#122500=CARTESIAN_POINT('Ctrl Pts',(-21.1970150425329,-19.3731534791717,
-6.86969147829734));
#122501=CARTESIAN_POINT('Ctrl Pts',(-20.4213067547485,-17.1089565202789,
-6.99686728497878));
#122502=CARTESIAN_POINT('Ctrl Pts',(-18.0975992455503,-16.5356375618508,
-7.12404309166021));
#122503=CARTESIAN_POINT('Ctrl Pts',(-16.3577499290741,-18.1791811640576,
-7.25121889834165));
#122504=CARTESIAN_POINT('Ctrl Pts',(-16.7979625659597,-20.5317380816948,
-7.37839470502308));
#122505=CARTESIAN_POINT('Ctrl Pts',(-19.014369384542,-21.4349833589804,
-7.50557051170451));
#122506=CARTESIAN_POINT('Ctrl Pts',(-20.9735546944935,-20.0602455157292,
-7.63274631838594));
#122507=CARTESIAN_POINT('Ctrl Pts',(-20.8780875746881,-17.6687611972708,
-7.75992212506739));
#122508=CARTESIAN_POINT('Ctrl Pts',(-18.8155531821895,-16.4545688335337,
-7.88709793174882));
#122509=CARTESIAN_POINT('Ctrl Pts',(-16.6781988067934,-17.5316145569697,
-8.01427373843027));
#122510=CARTESIAN_POINT('Ctrl Pts',(-16.4269144287518,-19.9117757653229,
-8.14144954511167));
#122511=CARTESIAN_POINT('Ctrl Pts',(-18.2922378684508,-21.4114022793946,
-8.26862535179315));
#122512=CARTESIAN_POINT('Ctrl Pts',(-20.5628506449959,-20.6546798498427,
-8.39580115847454));
#122513=CARTESIAN_POINT('Ctrl Pts',(-21.15560646603,-18.3358543382901,-8.52297696515602));
#122514=CARTESIAN_POINT('Ctrl Pts',(-19.5266886563297,-16.5823042290437,
-8.65015277183742));
#122515=CARTESIAN_POINT('Ctrl Pts',(-17.1705282042537,-17.0028029097426,
-8.77732857851889));
#122516=CARTESIAN_POINT('Ctrl Pts',(-16.2487560847711,-19.2115689399372,
-8.90450438520028));
#122517=CARTESIAN_POINT('Ctrl Pts',(-17.6070410058773,-21.1821965784047,
-9.03168019188174));
#122518=CARTESIAN_POINT('Ctrl Pts',(-19.9992408571273,-21.1067572777967,
-9.15885599856315));
#122519=CARTESIAN_POINT('Ctrl Pts',(-21.2306607516671,-19.0544619141298,
-9.28603180524462));
#122520=CARTESIAN_POINT('Ctrl Pts',(-20.1715493667948,-16.9081641037524,
-9.41320761192604));
#122521=CARTESIAN_POINT('Ctrl Pts',(-17.7935756622645,-16.6369588734199,
-9.54038341860746));
#122522=CARTESIAN_POINT('Ctrl Pts',(-16.2783829182894,-18.4896601890674,
-9.66755922528891));
#122523=CARTESIAN_POINT('Ctrl Pts',(-17.0160664339986,-20.7665295852005,
-9.79473503197033));
#122524=CARTESIAN_POINT('Ctrl Pts',(-19.3298473695317,-21.3786807093197,
-9.92191083865178));
#122525=CARTESIAN_POINT('Ctrl Pts',(-21.0969753259781,-19.7645028994292,
-10.0490866453332));
#122526=CARTESIAN_POINT('Ctrl Pts',(-20.6962200836287,-17.4049041089298,
-10.1762624520146));
#122527=CARTESIAN_POINT('Ctrl Pts',(-18.4952497036636,-16.4646697748868,
-10.3034382586961));
#122528=CARTESIAN_POINT('Ctrl Pts',(-16.5133179020725,-17.8064065412604,
-10.4306140653775));
#122529=CARTESIAN_POINT('Ctrl Pts',(-16.5687240942544,-20.1991542024786,
-10.5577898720589));
#122530=CARTESIAN_POINT('Ctrl Pts',(-18.6106365377785,-21.4477152900423,
-10.6849656787404));
#122531=CARTESIAN_POINT('Ctrl Pts',(-20.7657273010908,-20.4066125005527,
-10.8121414854218));
#122532=CARTESIAN_POINT('Ctrl Pts',(-21.0568343688704,-18.0309930252399,
-10.9393172921033));
#122533=CARTESIAN_POINT('Ctrl Pts',(-19.2168850745718,-16.5003402851297,
-11.0664930987847));
#122534=CARTESIAN_POINT('Ctrl Pts',(-16.9339186955814,-17.2189331662498,
-11.1936689054661));
#122535=CARTESIAN_POINT('Ctrl Pts',(-16.302415187749,-19.5275073010768,
-11.3208447121476));
#122536=CARTESIAN_POINT('Ctrl Pts',(-17.9017398239826,-21.3080892071774,
-11.448020518829));
#122537=CARTESIAN_POINT('Ctrl Pts',(-20.26461151582,-20.9271055010812,-11.5751963255104));
#122538=CARTESIAN_POINT('Ctrl Pts',(-21.2232421423571,-18.7340850866159,
-11.7023721321919));
#122539=CARTESIAN_POINT('Ctrl Pts',(-19.8981476030732,-16.7409880798555,
-11.8295479388733));
#122540=CARTESIAN_POINT('Ctrl Pts',(-17.5050198931187,-16.7763572789512,
-11.9567237455547));
#122541=CARTESIAN_POINT('Ctrl Pts',(-16.2394051521196,-18.8077436389928,
-12.0838995522362));
#122542=CARTESIAN_POINT('Ctrl Pts',(-17.2624263520327,-20.9714762566988,
-12.2110753589176));
#122543=CARTESIAN_POINT('Ctrl Pts',(-19.6355250377943,-21.2824647517163,
-12.3382511655991));
#122544=CARTESIAN_POINT('Ctrl Pts',(-21.181530456334,-19.4553964819894,
-12.4654269722804));
#122545=CARTESIAN_POINT('Ctrl Pts',(-20.4820785920598,-17.1664931843466,
-12.5926027789619));
#122546=CARTESIAN_POINT('Ctrl Pts',(-18.1788731175643,-16.5156815690145,
-12.7197785856433));
#122547=CARTESIAN_POINT('Ctrl Pts',(-16.3849621026435,-18.1000408991359,
-12.8469543923248));
#122548=CARTESIAN_POINT('Ctrl Pts',(-16.7461475608124,-20.4660198257546,
-12.9741301990062));
#122549=CARTESIAN_POINT('Ctrl Pts',(-18.9310642518988,-21.4429795329118,
-13.1013060056876));
#122550=CARTESIAN_POINT('Ctrl Pts',(-20.9351867230549,-20.1346201262487,
-13.2284818123691));
#122551=CARTESIAN_POINT('Ctrl Pts',(-20.9198569968642,-17.7412801554356,
-13.3556576190505));
#122552=CARTESIAN_POINT('Ctrl Pts',(-18.8991391456364,-16.4587004962619,
-13.4828334257319));
#122553=CARTESIAN_POINT('Ctrl Pts',(-16.7269163779785,-17.463568380148,
-13.6100092324134));
#122554=CARTESIAN_POINT('Ctrl Pts',(-16.3960682598664,-19.8339798927631,
-13.7371850390948));
#122555=CARTESIAN_POINT('Ctrl Pts',(-18.210127404918,-21.395229595614,-13.8643608457763));
#122556=CARTESIAN_POINT('Ctrl Pts',(-20.5048071407569,-20.71496778842,-13.9915366524577));
#122557=CARTESIAN_POINT('Ctrl Pts',(-21.174881233638,-18.417292457472,-14.1187124591391));
#122558=CARTESIAN_POINT('Ctrl Pts',(-19.6055982928313,-16.6101781091006,
-14.2458882658205));
#122559=CARTESIAN_POINT('Ctrl Pts',(-17.236678015843,-16.9515399957704,
-14.373064072502));
#122560=CARTESIAN_POINT('Ctrl Pts',(-16.2414577250354,-19.12819977377,-14.5002398791834));
#122561=CARTESIAN_POINT('Ctrl Pts',(-17.5329902668867,-21.1432071955271,
-14.6274156858649));
#122562=CARTESIAN_POINT('Ctrl Pts',(-19.9263746957985,-21.1479180170447,
-14.7545914925463));
#122563=CARTESIAN_POINT('Ctrl Pts',(-21.2258293484353,-19.1380103519671,
-14.8817672992277));
#122564=CARTESIAN_POINT('Ctrl Pts',(-20.2391852342543,-16.9574497340641,
-15.0089431059091));
#122565=CARTESIAN_POINT('Ctrl Pts',(-17.8716270899769,-16.6067651894063,
-15.1361189125906));
#122566=CARTESIAN_POINT('Ctrl Pts',(-16.2952425657462,-18.4076880217795,
-15.263294719272));
#122567=CARTESIAN_POINT('Ctrl Pts',(-16.9562666210861,-20.7079833103585,
-15.3904705259535));
#122568=CARTESIAN_POINT('Ctrl Pts',(-19.2482507130021,-21.3972729002994,
-15.5176463326349));
#122569=CARTESIAN_POINT('Ctrl Pts',(-21.0684416937376,-19.8431763749684,
-15.6448221393163));
#122570=CARTESIAN_POINT('Ctrl Pts',(-20.746927312261,-17.4714808382477,
-15.7719979459977));
#122571=CARTESIAN_POINT('Ctrl Pts',(-18.5786770581442,-16.4580697410522,
-15.8991737526792));
#122572=CARTESIAN_POINT('Ctrl Pts',(-16.552925962751,-17.7326848656722,
-16.0263495593606));
#122573=CARTESIAN_POINT('Ctrl Pts',(-16.5281749238118,-20.1259459468057,
-16.1535253660421));
#122574=CARTESIAN_POINT('Ctrl Pts',(-18.5271314833305,-21.4421844850479,
-16.2807011727235));
#122575=CARTESIAN_POINT('Ctrl Pts',(-20.7158770671853,-20.4738333165386,
-16.4078769794049));
#122576=CARTESIAN_POINT('Ctrl Pts',(-21.0863734510612,-18.1092945357334,
-16.5350527860864));
#122577=CARTESIAN_POINT('Ctrl Pts',(-19.298713198351,-16.5178857141929,
-16.6622285927678));
#122578=CARTESIAN_POINT('Ctrl Pts',(-16.9929636362077,-17.1596256717093,
-16.7894043994492));
#122579=CARTESIAN_POINT('Ctrl Pts',(-16.2845068769401,-19.4457578281354,
-16.9165802061307));
#122580=CARTESIAN_POINT('Ctrl Pts',(-17.8233080253906,-21.2788978233141,
-17.0437560128121));
#122581=CARTESIAN_POINT('Ctrl Pts',(-20.1976125366265,-20.9772534891692,
-17.1709318194935));
#122582=CARTESIAN_POINT('Ctrl Pts',(-21.2291433875466,-18.8175647801194,
-17.298107626175));
#122583=CARTESIAN_POINT('Ctrl Pts',(-19.9715350464571,-16.7812120413194,
-17.4252834328564));
#122584=CARTESIAN_POINT('Ctrl Pts',(-17.5785651103304,-16.7364225203127,
-17.5524592395378));
#122585=CARTESIAN_POINT('Ctrl Pts',(-16.2456349710989,-18.7242878226724,
-17.6796350462193));
#122586=CARTESIAN_POINT('Ctrl Pts',(-17.1956253005315,-20.9210649143176,
-17.8068108529007));
#122587=CARTESIAN_POINT('Ctrl Pts',(-19.5569789344254,-21.31134716103,-17.9339866595822));
#122588=CARTESIAN_POINT('Ctrl Pts',(-21.163300475815,-19.5370748250935,
-18.0611624662636));
#122589=CARTESIAN_POINT('Ctrl Pts',(-20.5408896100412,-17.2260326509801,
-18.188338272945));
#122590=CARTESIAN_POINT('Ctrl Pts',(-18.2607696752627,-16.4984583939631,
-18.3155140796264));
#122591=CARTESIAN_POINT('Ctrl Pts',(-16.4148091914615,-18.0218562765459,
-18.4426898863079));
#122592=CARTESIAN_POINT('Ctrl Pts',(-16.6965623292452,-20.3986032941145,
-18.5698656929893));
#122593=CARTESIAN_POINT('Ctrl Pts',(-18.8475380723677,-21.4481815757617,
-18.6970414996708));
#122594=CARTESIAN_POINT('Ctrl Pts',(-20.894349680935,-20.2076681919521,
-18.8242173063522));
#122595=CARTESIAN_POINT('Ctrl Pts',(-20.9591745439093,-17.8151571779635,
-18.9513931130336));
#122596=CARTESIAN_POINT('Ctrl Pts',(-18.9825398722896,-16.4656288920389,
-19.078568919715));
#122597=CARTESIAN_POINT('Ctrl Pts',(-16.7778852948647,-17.3971917774822,
-19.2057447263965));
#122598=CARTESIAN_POINT('Ctrl Pts',(-16.3678445475033,-19.7551947020895,
-19.3329205330779));
#122599=CARTESIAN_POINT('Ctrl Pts',(-18.1286045709649,-21.3763163446451,
-19.4600963397593));
#122600=CARTESIAN_POINT('Ctrl Pts',(-20.4447773190769,-20.773278200954,
-19.5872721464408));
#122601=CARTESIAN_POINT('Ctrl Pts',(-21.1914180721045,-18.4993303685776,
-19.7144479531222));
#122602=CARTESIAN_POINT('Ctrl Pts',(-19.6835302447416,-16.6406787897749,
-19.8416237598037));
#122603=CARTESIAN_POINT('Ctrl Pts',(-17.304507398182,-16.9025210366613,
-19.9687995664851));
#122604=CARTESIAN_POINT('Ctrl Pts',(-16.2369552011117,-19.0446328885181,
-20.0959753731665));
#122605=CARTESIAN_POINT('Ctrl Pts',(-17.4602867931939,-21.1017600821981,
-20.223151179848));
#122606=CARTESIAN_POINT('Ctrl Pts',(-19.8521708689288,-21.1866153140319,
-20.3503269865294));
#122607=CARTESIAN_POINT('Ctrl Pts',(-21.2182032059767,-19.221350684525,
-20.4775027932109));
#122608=CARTESIAN_POINT('Ctrl Pts',(-20.3051320707828,-17.0089716056813,
-20.6046785998922));
#122609=CARTESIAN_POINT('Ctrl Pts',(-17.9506471225061,-16.5792041686457,
-20.7318544065737));
#122610=CARTESIAN_POINT('Ctrl Pts',(-16.3148352980017,-18.3263225287329,
-20.8590302132551));
#122611=CARTESIAN_POINT('Ctrl Pts',(-16.8984656481068,-20.647474826016,
-20.9862060199366));
#122612=CARTESIAN_POINT('Ctrl Pts',(-19.1660680562885,-21.4131078237249,
-21.113381826618));
#122613=CARTESIAN_POINT('Ctrl Pts',(-21.0373071781416,-19.9208779742462,
-21.2405576332995));
#122614=CARTESIAN_POINT('Ctrl Pts',(-20.7953426154092,-17.5396647859301,
-21.3677334399809));
#122615=CARTESIAN_POINT('Ctrl Pts',(-18.6623441981192,-16.4543701936005,
-21.4949092466623));
#122616=CARTESIAN_POINT('Ctrl Pts',(-16.5948542065943,-17.6601323237235,
-21.6220850533437));
#122617=CARTESIAN_POINT('Ctrl Pts',(-16.4903435139124,-20.0518037409453,
-21.7492608600252));
#122618=CARTESIAN_POINT('Ctrl Pts',(-18.4433885276789,-21.4331202535291,
-21.8764366667066));
#122619=CARTESIAN_POINT('Ctrl Pts',(-20.6647168408145,-20.5407968853708,
-22.0036124733881));
#122620=CARTESIAN_POINT('Ctrl Pts',(-21.1114425640841,-18.1855248151863,
-22.1307882800695));
#122621=CARTESIAN_POINT('Ctrl Pts',(-19.9599076846608,-17.0924953497883,
-22.2155721511904));
#122622=CARTESIAN_POINT('Ctrl Pts',(-19.2802416510892,-16.9106266592565,
-22.2579640867509));
#122623=CARTESIAN_POINT('Ctrl Pts',(-17.0028272034401,-17.4941907062238,
0.0844764445356071));
#122624=CARTESIAN_POINT('Ctrl Pts',(-16.5172188178569,-18.0708180956198,
0.0420658524719494));
#122625=CARTESIAN_POINT('Ctrl Pts',(-16.1763692071458,-19.7372661563571,
-0.0427366751521866));
#122626=CARTESIAN_POINT('Ctrl Pts',(-18.0136451140781,-21.531198562073,
-0.1699311383368));
#122627=CARTESIAN_POINT('Ctrl Pts',(-20.5111532049132,-20.9519193050085,
-0.297106945018234));
#122628=CARTESIAN_POINT('Ctrl Pts',(-21.3783873242474,-18.5411721545534,
-0.424282751699668));
#122629=CARTESIAN_POINT('Ctrl Pts',(-19.8194849515203,-16.5056185643353,
-0.551458558381103));
#122630=CARTESIAN_POINT('Ctrl Pts',(-17.2647560814413,-16.7153568808188,
-0.678634365062537));
#122631=CARTESIAN_POINT('Ctrl Pts',(-16.0579473465983,-18.9766153220251,
-0.805810171743972));
#122632=CARTESIAN_POINT('Ctrl Pts',(-17.306261185047,-21.2155300370204,
-0.932985978425408));
#122633=CARTESIAN_POINT('Ctrl Pts',(-19.8644313952761,-21.3776722353249,
-1.06016178510684));
#122634=CARTESIAN_POINT('Ctrl Pts',(-21.3855037526656,-19.3144751713091,
-1.18733759178828));
#122635=CARTESIAN_POINT('Ctrl Pts',(-20.4739845399306,-16.9186961805966,
-1.31451339846971));
#122636=CARTESIAN_POINT('Ctrl Pts',(-17.9661382589161,-16.3883646063293,
-1.44168920515115));
#122637=CARTESIAN_POINT('Ctrl Pts',(-16.1627570764457,-18.2100003769934,
-1.56886501183258));
#122638=CARTESIAN_POINT('Ctrl Pts',(-16.7183318894278,-20.7123794251487,
-1.69604081851402));
#122639=CARTESIAN_POINT('Ctrl Pts',(-19.1231569823275,-21.5997171847722,
-1.82321662519545));
#122640=CARTESIAN_POINT('Ctrl Pts',(-21.1709547522747,-20.0579400230779,
-1.95039243187689));
#122641=CARTESIAN_POINT('Ctrl Pts',(-20.9829977631806,-17.5015308787203,
-2.07756823855832));
#122642=CARTESIAN_POINT('Ctrl Pts',(-18.7317249295996,-16.2758374662316,
-2.20474404523976));
#122643=CARTESIAN_POINT('Ctrl Pts',(-16.4825393242813,-17.5053569009653,
-2.33191985192118));
#122644=CARTESIAN_POINT('Ctrl Pts',(-16.2989291514817,-20.062081681679,
-2.45909565860262));
#122645=CARTESIAN_POINT('Ctrl Pts',(-18.3493453426023,-21.6003753714481,
-2.58627146528406));
#122646=CARTESIAN_POINT('Ctrl Pts',(-20.7526583085904,-20.708949059251,
-2.71344727196549));
#122647=CARTESIAN_POINT('Ctrl Pts',(-21.3039775679586,-18.2056310209682,
-2.84062307864693));
#122648=CARTESIAN_POINT('Ctrl Pts',(-19.4975019198092,-16.3870602026966,
-2.96779888532836));
#122649=CARTESIAN_POINT('Ctrl Pts',(-16.9905606483594,-16.9216624468904,
-3.09497469200979));
#122650=CARTESIAN_POINT('Ctrl Pts',(-16.0831167720671,-19.3189733808883,
-3.22215049869123));
#122651=CARTESIAN_POINT('Ctrl Pts',(-17.6076937249943,-21.3796090139306,
-3.34932630537266));
#122652=CARTESIAN_POINT('Ctrl Pts',(-20.1655867788085,-21.2130640515812,
-3.4765021120541));
#122653=CARTESIAN_POINT('Ctrl Pts',(-21.4100878173515,-18.9721331591184,
-3.60367791873553));
#122654=CARTESIAN_POINT('Ctrl Pts',(-20.1994443802222,-16.7127313428988,
-3.73085372541697));
#122655=CARTESIAN_POINT('Ctrl Pts',(-17.6443466799723,-16.507719534815,
-3.8580295320984));
#122656=CARTESIAN_POINT('Ctrl Pts',(-16.0889382693367,-18.545183344418,
-3.98520533877984));
#122657=CARTESIAN_POINT('Ctrl Pts',(-16.9602098255379,-20.95587618561,-4.11238114546127));
#122658=CARTESIAN_POINT('Ctrl Pts',(-19.458823772974,-21.5281370010973,
-4.2395569521427));
#122659=CARTESIAN_POINT('Ctrl Pts',(-21.2924568963431,-19.7369520111678,
-4.36673275882414));
#122660=CARTESIAN_POINT('Ctrl Pts',(-20.7788646130614,-17.2256222706107,
-4.49390856550557));
#122661=CARTESIAN_POINT('Ctrl Pts',(-18.3892359659074,-16.2981369456807,
-4.62108437218701));
#122662=CARTESIAN_POINT('Ctrl Pts',(-16.3159069215641,-17.8054062557716,
-4.74826017886844));
#122663=CARTESIAN_POINT('Ctrl Pts',(-16.4610281929029,-20.3646041605579,
-4.87543598554988));
#122664=CARTESIAN_POINT('Ctrl Pts',(-18.6914600207125,-21.6278254241348,
-5.00261179223131));
#122665=CARTESIAN_POINT('Ctrl Pts',(-20.9609196391894,-20.436142941524,
-5.12978759891275));
#122666=CARTESIAN_POINT('Ctrl Pts',(-21.187318706931,-17.8828514263649,
-5.25696340559418));
#122667=CARTESIAN_POINT('Ctrl Pts',(-19.1629501311951,-16.3104373686715,
-5.38413921227561));
#122668=CARTESIAN_POINT('Ctrl Pts',(-16.7450464337354,-17.1614930713546,
-5.51131501895704));
#122669=CARTESIAN_POINT('Ctrl Pts',(-16.1518841849428,-19.6552277496765,
-5.63849082563848));
#122670=CARTESIAN_POINT('Ctrl Pts',(-17.9276529322832,-21.503794614907,
-5.76566663231992));
#122671=CARTESIAN_POINT('Ctrl Pts',(-20.4431950667104,-21.0112483031962,
-5.89284243900135));
#122672=CARTESIAN_POINT('Ctrl Pts',(-21.3906568120407,-18.629469484667,
-6.02001824568278));
#122673=CARTESIAN_POINT('Ctrl Pts',(-19.9008008230416,-16.5435923954545,
-6.14719405236422));
#122674=CARTESIAN_POINT('Ctrl Pts',(-17.3404774987283,-16.667279800778,
-6.27436985904566));
#122675=CARTESIAN_POINT('Ctrl Pts',(-16.0586245775708,-18.8870561831594,
-6.40154566572708));
#122676=CARTESIAN_POINT('Ctrl Pts',(-17.2312625539661,-21.1664144866242,
-6.52872147240852));
#122677=CARTESIAN_POINT('Ctrl Pts',(-19.7825688666926,-21.414184940675,
-6.65589727908996));
#122678=CARTESIAN_POINT('Ctrl Pts',(-21.3718783257522,-19.4030535320888,
-6.78307308577139));
#122679=CARTESIAN_POINT('Ctrl Pts',(-20.5410981461279,-16.9781085033506,
-6.91024889245283));
#122680=CARTESIAN_POINT('Ctrl Pts',(-18.0524175785914,-16.3640864092651,
-7.03742469913425));
#122681=CARTESIAN_POINT('Ctrl Pts',(-16.1890465789213,-18.1243144106463,
-7.1646005058157));
#122682=CARTESIAN_POINT('Ctrl Pts',(-16.6605123854672,-20.6438925682982,
-7.29177631249713));
#122683=CARTESIAN_POINT('Ctrl Pts',(-19.0342743831914,-21.6112643052322,
-7.41895211917856));
#122684=CARTESIAN_POINT('Ctrl Pts',(-21.1325532714676,-20.1389260946729,
-7.54612792586));
#122685=CARTESIAN_POINT('Ctrl Pts',(-21.0303084041777,-17.5776568611929,
-7.67330373254143));
#122686=CARTESIAN_POINT('Ctrl Pts',(-18.8213431010281,-16.277262156213,
-7.80047953922286));
#122687=CARTESIAN_POINT('Ctrl Pts',(-16.5322459238095,-17.4307734099542,
-7.92765534590431));
#122688=CARTESIAN_POINT('Ctrl Pts',(-16.2631214552256,-19.979915642092,
-8.05483115258573));
#122689=CARTESIAN_POINT('Ctrl Pts',(-18.260874691454,-21.5860090722502,
-8.18200695926717));
#122690=CARTESIAN_POINT('Ctrl Pts',(-20.6926910328048,-20.7755626636597,
-8.30918276594861));
#122691=CARTESIAN_POINT('Ctrl Pts',(-21.3275299216332,-18.2921106942249,
-8.43635857263003));
#122692=CARTESIAN_POINT('Ctrl Pts',(-19.5829660799844,-16.4140662054893,
-8.56353437931147));
#122693=CARTESIAN_POINT('Ctrl Pts',(-17.0595285527274,-16.8644184512809,
-8.69071018599291));
#122694=CARTESIAN_POINT('Ctrl Pts',(-16.0723146489239,-19.2299971980986,
-8.81788599267433));
#122695=CARTESIAN_POINT('Ctrl Pts',(-17.5270318519084,-21.3405307701129,
-8.94506179935578));
#122696=CARTESIAN_POINT('Ctrl Pts',(-20.089067417875,-21.2597356094876,
-9.07223760603719));
#122697=CARTESIAN_POINT('Ctrl Pts',(-21.4079127329105,-19.0617362613832,
-9.19941341271864));
#122698=CARTESIAN_POINT('Ctrl Pts',(-20.2736090772418,-16.7630607044602,
-9.32658921940007));
#122699=CARTESIAN_POINT('Ctrl Pts',(-17.7268096521201,-16.4726010903001,
-9.45376502608151));
#122700=CARTESIAN_POINT('Ctrl Pts',(-16.1040448578949,-18.4568360869378,
-9.58094083276294));
#122701=CARTESIAN_POINT('Ctrl Pts',(-16.8941006731258,-20.8953532404716,
-9.70811663944438));
#122702=CARTESIAN_POINT('Ctrl Pts',(-19.3721499237325,-21.5509644139779,
-9.83529244612582));
#122703=CARTESIAN_POINT('Ctrl Pts',(-21.2647362273657,-19.8221870475835,
-9.96246825280725));
#122704=CARTESIAN_POINT('Ctrl Pts',(-20.835529117596,-17.2950670749305,
-10.0896440594887));
#122705=CARTESIAN_POINT('Ctrl Pts',(-18.4782994780394,-16.2880802201732,
-10.2168198661701));
#122706=CARTESIAN_POINT('Ctrl Pts',(-16.3556591968173,-17.7250744218984,
-10.3439956728516));
#122707=CARTESIAN_POINT('Ctrl Pts',(-16.414998986037,-20.2876966899422,
-10.471171479533));
#122708=CARTESIAN_POINT('Ctrl Pts',(-18.6018782721322,-21.6249001476502,
-10.5983472862144));
#122709=CARTESIAN_POINT('Ctrl Pts',(-20.9099710431467,-20.5098836187822,
-10.7255230928959));
#122710=CARTESIAN_POINT('Ctrl Pts',(-21.2217454380686,-17.965605562844,
-10.8526988995773));
#122711=CARTESIAN_POINT('Ctrl Pts',(-19.2511678004582,-16.3262831804529,
-10.9798747062588));
#122712=CARTESIAN_POINT('Ctrl Pts',(-16.8061208049812,-17.0958930096308,
-11.1070505129402));
#122713=CARTESIAN_POINT('Ctrl Pts',(-16.1297833132563,-19.5683657994802,
-11.2342263196216));
#122714=CARTESIAN_POINT('Ctrl Pts',(-17.8426529957019,-21.4753612242825,
-11.361402126303));
#122715=CARTESIAN_POINT('Ctrl Pts',(-20.3732782313567,-21.0673293432663,
-11.4885779329845));
#122716=CARTESIAN_POINT('Ctrl Pts',(-21.3999674348234,-18.7186140819493,
-11.6157537396659));
#122717=CARTESIAN_POINT('Ctrl Pts',(-19.98079698544,-16.5840159148801,-11.7429295463474));
#122718=CARTESIAN_POINT('Ctrl Pts',(-17.4177676868637,-16.6218961722405,
-11.8701053530288));
#122719=CARTESIAN_POINT('Ctrl Pts',(-16.0622998409991,-18.7975020690164,
-11.9972811597103));
#122720=CARTESIAN_POINT('Ctrl Pts',(-17.1579510666044,-21.1148502282466,
-12.1244569663916));
#122721=CARTESIAN_POINT('Ctrl Pts',(-19.6995293679712,-21.4479175446854,
-12.2516327730731));
#122722=CARTESIAN_POINT('Ctrl Pts',(-21.3552944017355,-19.4911354279892,
-12.3788085797545));
#122723=CARTESIAN_POINT('Ctrl Pts',(-20.6061845177868,-17.0397300186315,
-12.505984386436));
#122724=CARTESIAN_POINT('Ctrl Pts',(-18.1394615396447,-16.3427136283187,
-12.6331601931174));
#122725=CARTESIAN_POINT('Ctrl Pts',(-16.2181906976602,-18.0395555334466,
-12.7603359997988));
#122726=CARTESIAN_POINT('Ctrl Pts',(-16.6050187418368,-20.5735086039467,
-12.8875118064803));
#122727=CARTESIAN_POINT('Ctrl Pts',(-18.9450549508987,-21.6198281725,-13.0146876131617));
#122728=CARTESIAN_POINT('Ctrl Pts',(-21.0914613420586,-20.2185809768753,
-13.1418634198431));
#122729=CARTESIAN_POINT('Ctrl Pts',(-21.0750432724325,-17.6553243478488,
-13.2690392265246));
#122730=CARTESIAN_POINT('Ctrl Pts',(-18.9108633018819,-16.2816871489036,
-13.396215033206));
#122731=CARTESIAN_POINT('Ctrl Pts',(-16.5844222292293,-17.3578962525319,
-13.5233908398874));
#122732=CARTESIAN_POINT('Ctrl Pts',(-16.2300853434153,-19.8965966032252,
-13.6505666465689));
#122733=CARTESIAN_POINT('Ctrl Pts',(-18.1729347445473,-21.5686881987366,
-13.7777424532503));
#122734=CARTESIAN_POINT('Ctrl Pts',(-20.6305266939199,-20.8401307818932,
-13.9049182599318));
#122735=CARTESIAN_POINT('Ctrl Pts',(-21.348173113343,-18.3793305632757,
-14.0320940666132));
#122736=CARTESIAN_POINT('Ctrl Pts',(-19.6674779551561,-16.443919008979,
-14.1592698732946));
#122737=CARTESIAN_POINT('Ctrl Pts',(-17.1303747112896,-16.8095160948814,
-14.2864456799761));
#122738=CARTESIAN_POINT('Ctrl Pts',(-16.0644981376042,-19.140709186182,
-14.4136214866575));
#122739=CARTESIAN_POINT('Ctrl Pts',(-17.4477238346954,-21.2987733117736,
-14.5407972933389));
#122740=CARTESIAN_POINT('Ctrl Pts',(-20.0110280781508,-21.3038185809918,
-14.6679731000203));
#122741=CARTESIAN_POINT('Ctrl Pts',(-21.4027383212044,-19.1512162724734,
-14.7951489067018));
#122742=CARTESIAN_POINT('Ctrl Pts',(-20.3460467951339,-16.8158453987172,
-14.9223247133832));
#122743=CARTESIAN_POINT('Ctrl Pts',(-17.8104023894363,-16.4402637869306,
-15.0495005200647));
#122744=CARTESIAN_POINT('Ctrl Pts',(-16.1221014664979,-18.3690442547039,
-15.1766763267461));
#122745=CARTESIAN_POINT('Ctrl Pts',(-16.8300553353419,-20.8326504364724,
-15.3038521334275));
#122746=CARTESIAN_POINT('Ctrl Pts',(-19.2847602618764,-21.5708765691077,
-15.4310279401089));
#122747=CARTESIAN_POINT('Ctrl Pts',(-21.2341768321763,-19.9064459953984,
-15.5582037467904));
#122748=CARTESIAN_POINT('Ctrl Pts',(-20.8898363374295,-17.3663704605105,
-15.6853795534718));
#122749=CARTESIAN_POINT('Ctrl Pts',(-18.5676498093848,-16.2810116128359,
-15.8125553601533));
#122750=CARTESIAN_POINT('Ctrl Pts',(-16.3980792563722,-17.6461188301484,
-15.9397311668347));
#122751=CARTESIAN_POINT('Ctrl Pts',(-16.3715710020456,-20.2092909686735,
-16.0669069735161));
#122752=CARTESIAN_POINT('Ctrl Pts',(-18.5124447244619,-21.618976679719,
-16.1940827801976));
#122753=CARTESIAN_POINT('Ctrl Pts',(-20.8565816609132,-20.5818768183634,
-16.321258586879));
#122754=CARTESIAN_POINT('Ctrl Pts',(-21.2533816657522,-18.0494661377238,
-16.4484343935604));
#122755=CARTESIAN_POINT('Ctrl Pts',(-19.338805362725,-16.3450742581534,
-16.5756102002418));
#122756=CARTESIAN_POINT('Ctrl Pts',(-16.869357677852,-17.0323749426676,
-16.7027860069233));
#122757=CARTESIAN_POINT('Ctrl Pts',(-16.1106035907951,-19.4808124719162,
-16.8299618136047));
#122758=CARTESIAN_POINT('Ctrl Pts',(-17.7586528828391,-21.4440973799852,
-16.9571376202862));
#122759=CARTESIAN_POINT('Ctrl Pts',(-20.3015226180088,-21.1210376189256,
-17.0843134269676));
#122760=CARTESIAN_POINT('Ctrl Pts',(-21.4062876425816,-18.8080204681591,
-17.211489233649));
#122761=CARTESIAN_POINT('Ctrl Pts',(-20.0593946159625,-16.6270956014793,
-17.3386650403305));
#122762=CARTESIAN_POINT('Ctrl Pts',(-17.4965342924651,-16.5791262206009,
-17.4658408470119));
#122763=CARTESIAN_POINT('Ctrl Pts',(-16.0689719498474,-18.7081212551652,
-17.5930166536933));
#122764=CARTESIAN_POINT('Ctrl Pts',(-17.0864074329483,-21.0608599012923,
-17.7201924603748));
#122765=CARTESIAN_POINT('Ctrl Pts',(-19.6154068351929,-21.4788504785931,
-17.8473682670562));
#122766=CARTESIAN_POINT('Ctrl Pts',(-21.3357701724232,-19.5786125758088,
-17.9745440737377));
#122767=CARTESIAN_POINT('Ctrl Pts',(-20.6691708605291,-17.1034965266906,
-18.1017198804191));
#122768=CARTESIAN_POINT('Ctrl Pts',(-18.2271723943392,-16.3242676832537,
-18.2288956871005));
#122769=CARTESIAN_POINT('Ctrl Pts',(-16.2501567990929,-17.9558201449997,
-18.3560714937819));
#122770=CARTESIAN_POINT('Ctrl Pts',(-16.5519131759471,-20.5013057937568,
-18.4832473004634));
#122771=CARTESIAN_POINT('Ctrl Pts',(-18.8555987783568,-21.6253995376139,
-18.6104231071448));
#122772=CARTESIAN_POINT('Ctrl Pts',(-21.0477250487613,-20.2968151353882,
-18.7375989138263));
#122773=CARTESIAN_POINT('Ctrl Pts',(-21.1171521931581,-17.7344463154909,
-18.8647747205077));
#122774=CARTESIAN_POINT('Ctrl Pts',(-19.000185114941,-16.2891074304433,
-18.9919505271891));
#122775=CARTESIAN_POINT('Ctrl Pts',(-16.6390097160369,-17.2868072017201,
-19.1191263338706));
#122776=CARTESIAN_POINT('Ctrl Pts',(-16.1998578710576,-19.8122180089903,
-19.246302140552));
#122777=CARTESIAN_POINT('Ctrl Pts',(-18.0856241463476,-21.5484321897643,
-19.3734779472334));
#122778=CARTESIAN_POINT('Ctrl Pts',(-20.566235017753,-20.9025809783934,
-19.5006537539149));
#122779=CARTESIAN_POINT('Ctrl Pts',(-21.3658839949308,-18.4671928068505,
-19.6278295605963));
#122780=CARTESIAN_POINT('Ctrl Pts',(-19.7509427344116,-16.4765851044279,
-19.7550053672777));
#122781=CARTESIAN_POINT('Ctrl Pts',(-17.2030196827703,-16.757017004315,
-19.8821811739592));
#122782=CARTESIAN_POINT('Ctrl Pts',(-16.0596759541972,-19.0512094179914,
-20.0093569806406));
#122783=CARTESIAN_POINT('Ctrl Pts',(-17.3698587327169,-21.2543836348827,
-20.136532787322));
#122784=CARTESIAN_POINT('Ctrl Pts',(-19.9315561044895,-21.3452632166212,
-20.2637085940035));
#122785=CARTESIAN_POINT('Ctrl Pts',(-21.394570756024,-19.2404734037209,
-20.3908844006849));
#122786=CARTESIAN_POINT('Ctrl Pts',(-20.4166755682946,-16.8710250976204,
-20.5180602073664));
#122787=CARTESIAN_POINT('Ctrl Pts',(-17.8950324982703,-16.4107460543773,
-20.6452360140478));
#122788=CARTESIAN_POINT('Ctrl Pts',(-16.1430851969531,-18.281902167926,
-20.7724118207292));
#122789=CARTESIAN_POINT('Ctrl Pts',(-16.7681507463741,-20.7678461146898,
-20.8995876274106));
#122790=CARTESIAN_POINT('Ctrl Pts',(-19.1967429963892,-21.58783570276,-21.0267634340921));
#122791=CARTESIAN_POINT('Ctrl Pts',(-21.2008319023016,-19.989664067993,
-21.1539392407735));
#122792=CARTESIAN_POINT('Ctrl Pts',(-20.9416889151052,-17.4393951699213,
-21.2811150474549));
#122793=CARTESIAN_POINT('Ctrl Pts',(-18.6572569499448,-16.2770494137143,
-21.4082908541364));
#122794=CARTESIAN_POINT('Ctrl Pts',(-16.4429842219372,-17.568415375407,
-21.5354666608178));
#122795=CARTESIAN_POINT('Ctrl Pts',(-16.3310537276957,-20.1298849908433,
-21.6626424674993));
#122796=CARTESIAN_POINT('Ctrl Pts',(-18.4227563856442,-21.6092689274519,
-21.7898182741806));
#122797=CARTESIAN_POINT('Ctrl Pts',(-20.8017892824853,-20.6535945073695,
-21.9169940808621));
#122798=CARTESIAN_POINT('Ctrl Pts',(-21.2802305760296,-18.1311084332283,
-22.0441698875435));
#122799=CARTESIAN_POINT('Ctrl Pts',(-20.0469417623915,-16.9604786618337,
-22.1289537586645));
#122800=CARTESIAN_POINT('Ctrl Pts',(-19.319022416489,-16.7656980906223,
-22.171345694225));
#122801=CARTESIAN_POINT('Ctrl Pts',(-16.8880688553878,-17.3975534516058,
0.171094837061569));
#122802=CARTESIAN_POINT('Ctrl Pts',(-16.3702697975385,-18.0124051053735,
0.128684244997911));
#122803=CARTESIAN_POINT('Ctrl Pts',(-16.0068254820486,-19.7893209524259,
0.0438817173737748));
#122804=CARTESIAN_POINT('Ctrl Pts',(-17.9658932450075,-21.7021720009294,
-0.0833127458108387));
#122805=CARTESIAN_POINT('Ctrl Pts',(-20.6289595651085,-21.0844926888652,
-0.210488552492274));
#122806=CARTESIAN_POINT('Ctrl Pts',(-21.5536820848537,-18.5139386369225,
-0.337664359173708));
#122807=CARTESIAN_POINT('Ctrl Pts',(-19.8914410613435,-16.3434494886539,
-0.464840165855142));
#122808=CARTESIAN_POINT('Ctrl Pts',(-17.1673608327897,-16.567091225276,
-0.592015972536576));
#122809=CARTESIAN_POINT('Ctrl Pts',(-15.8805535113812,-18.9782470561293,
-0.719191779218011));
#122810=CARTESIAN_POINT('Ctrl Pts',(-17.2116172834215,-21.365578009315,
-0.846367585899445));
#122811=CARTESIAN_POINT('Ctrl Pts',(-19.939366976384,-21.5384685112341,
-0.973543392580879));
#122812=CARTESIAN_POINT('Ctrl Pts',(-21.5612702568039,-19.3385034208011,
-1.10071919926231));
#122813=CARTESIAN_POINT('Ctrl Pts',(-20.5893270128691,-16.7839097584284,
-1.22789500594375));
#122814=CARTESIAN_POINT('Ctrl Pts',(-17.9152371905106,-16.2184228400477,
-1.35507081262518));
#122815=CARTESIAN_POINT('Ctrl Pts',(-15.9923110118271,-18.1608136920126,
-1.48224661930662));
#122816=CARTESIAN_POINT('Ctrl Pts',(-16.5847145272265,-20.8290738621089,
-1.60942242598805));
#122817=CARTESIAN_POINT('Ctrl Pts',(-19.1489539521699,-21.7752326797234,
-1.73659823266948));
#122818=CARTESIAN_POINT('Ctrl Pts',(-21.3324989390857,-20.1312520866371,
-1.86377403935092));
#122819=CARTESIAN_POINT('Ctrl Pts',(-21.1320824002478,-17.4053801994873,
-1.99094984603235));
#122820=CARTESIAN_POINT('Ctrl Pts',(-18.731574116624,-16.0984363471145,
-2.11812565271379));
#122821=CARTESIAN_POINT('Ctrl Pts',(-16.3332914223019,-17.4094598463232,
-2.24530145939522));
#122822=CARTESIAN_POINT('Ctrl Pts',(-16.1375098474575,-20.1356682931634,
-2.37247726607666));
#122823=CARTESIAN_POINT('Ctrl Pts',(-18.3238468290274,-21.7759344971771,
-2.49965307275809));
#122824=CARTESIAN_POINT('Ctrl Pts',(-20.8864738891242,-20.8254160994288,
-2.62682887943953));
#122825=CARTESIAN_POINT('Ctrl Pts',(-21.4743397529562,-18.1561546941444,
-2.75400468612096));
#122826=CARTESIAN_POINT('Ctrl Pts',(-19.5481139784241,-16.2170319683244,
-2.88118049280239));
#122827=CARTESIAN_POINT('Ctrl Pts',(-16.8749891581411,-16.7870726566358,
-3.00835629948383));
#122828=CARTESIAN_POINT('Ctrl Pts',(-15.9073914021204,-19.3432998138438,
-3.13553210616526));
#122829=CARTESIAN_POINT('Ctrl Pts',(-17.533031595496,-21.5405336776668,
-3.2627079128467));
#122830=CARTESIAN_POINT('Ctrl Pts',(-20.2604857595204,-21.3629485552631,
-3.38988371952813));
#122831=CARTESIAN_POINT('Ctrl Pts',(-21.5874839835647,-18.9734677734828,
-3.51705952620957));
#122832=CARTESIAN_POINT('Ctrl Pts',(-20.2965877598843,-16.5642916421105,
-3.644235332891));
#122833=CARTESIAN_POINT('Ctrl Pts',(-17.5721142516412,-16.3456897311358,
-3.77141113957244));
#122834=CARTESIAN_POINT('Ctrl Pts',(-15.9135988027563,-18.5182157260222,
-3.89858694625387));
#122835=CARTESIAN_POINT('Ctrl Pts',(-16.8426263985008,-21.0887118685754,
-4.0257627529353));
#122836=CARTESIAN_POINT('Ctrl Pts',(-19.5068718817363,-21.6989074910159,
-4.15293855961674));
#122837=CARTESIAN_POINT('Ctrl Pts',(-21.4620553833173,-19.7889859827511,
-4.28011436629817));
#122838=CARTESIAN_POINT('Ctrl Pts',(-20.9144173929179,-17.1111817845236,
-4.40729017297961));
#122839=CARTESIAN_POINT('Ctrl Pts',(-18.3663817764822,-16.1222140449305,
-4.53446597966104));
#122840=CARTESIAN_POINT('Ctrl Pts',(-16.1556130631639,-17.7293992827899,
-4.66164178634248));
#122841=CARTESIAN_POINT('Ctrl Pts',(-16.310354331651,-20.4582447955307,
-4.78881759302391));
#122842=CARTESIAN_POINT('Ctrl Pts',(-18.6886400724331,-21.8052041964678,
-4.91599339970535));
#122843=CARTESIAN_POINT('Ctrl Pts',(-21.1085407314031,-20.5345258369701,
-5.04316920638678));
#122844=CARTESIAN_POINT('Ctrl Pts',(-21.34994764993,-17.8119782446832,-5.17034501306821));
#122845=CARTESIAN_POINT('Ctrl Pts',(-19.1913849636685,-16.1353298551694,
-5.29752081974965));
#122846=CARTESIAN_POINT('Ctrl Pts',(-16.6131999617537,-17.0428015012722,
-5.42469662643108));
#122847=CARTESIAN_POINT('Ctrl Pts',(-15.9807173632341,-19.7018442717348,
-5.55187243311253));
#122848=CARTESIAN_POINT('Ctrl Pts',(-17.8742006959542,-21.672951463465,
-5.67904823979394));
#122849=CARTESIAN_POINT('Ctrl Pts',(-20.556496524973,-21.1477545687602,
-5.80622404647539));
#122850=CARTESIAN_POINT('Ctrl Pts',(-21.5667649092206,-18.6080891411163,
-5.93339985315682));
#122851=CARTESIAN_POINT('Ctrl Pts',(-19.9781473104775,-16.3839405809831,
-6.06057565983826));
#122852=CARTESIAN_POINT('Ctrl Pts',(-17.2481017748621,-16.5158271460542,
-6.18775146651969));
#122853=CARTESIAN_POINT('Ctrl Pts',(-15.8812756355658,-18.8827510986805,
-6.31492727320112));
#122854=CARTESIAN_POINT('Ctrl Pts',(-17.1316470405952,-21.3132066201958,
-6.44210307988256));
#122855=CARTESIAN_POINT('Ctrl Pts',(-19.8520778326375,-21.5774016206925,
-6.569278886564));
#122856=CARTESIAN_POINT('Ctrl Pts',(-21.5467416089716,-19.4329535850057,
-6.69645469324542));
#122857=CARTESIAN_POINT('Ctrl Pts',(-20.6608895375072,-16.8472604864224,
-6.82363049992686));
#122858=CARTESIAN_POINT('Ctrl Pts',(-18.0072359116326,-16.1925352566794,
-6.95080630660829));
#122859=CARTESIAN_POINT('Ctrl Pts',(-16.0203432287685,-18.0694476572352,
-7.07798211328973));
#122860=CARTESIAN_POINT('Ctrl Pts',(-16.5230622049748,-20.7560470549016,
-7.20515791997116));
#122861=CARTESIAN_POINT('Ctrl Pts',(-19.0541793818409,-21.7875452514841,
-7.3323337266526));
#122862=CARTESIAN_POINT('Ctrl Pts',(-21.2915518484416,-20.2176066736166,
-7.45950953333402));
#122863=CARTESIAN_POINT('Ctrl Pts',(-21.1825292336674,-17.4865525251151,
-7.58668534001548));
#122864=CARTESIAN_POINT('Ctrl Pts',(-18.8271330198668,-16.0999554788923,
-7.71386114669689));
#122865=CARTESIAN_POINT('Ctrl Pts',(-16.3862930408257,-17.3299322629389,
-7.84103695337835));
#122866=CARTESIAN_POINT('Ctrl Pts',(-16.0993284816994,-20.0480555188611,
-7.96821276005976));
#122867=CARTESIAN_POINT('Ctrl Pts',(-18.2295115144572,-21.760615865106,
-8.09538856674121));
#122868=CARTESIAN_POINT('Ctrl Pts',(-20.8225314206137,-20.8964454774766,
-8.22256437342263));
#122869=CARTESIAN_POINT('Ctrl Pts',(-21.4994533772365,-18.2483670501596,
-8.34974018010408));
#122870=CARTESIAN_POINT('Ctrl Pts',(-19.6392435036391,-16.245828181935,
-8.4769159867855));
#122871=CARTESIAN_POINT('Ctrl Pts',(-16.9485289012012,-16.7260339928192,
-8.60409179346695));
#122872=CARTESIAN_POINT('Ctrl Pts',(-15.8958732130767,-19.2484254562599,
-8.73126760014836));
#122873=CARTESIAN_POINT('Ctrl Pts',(-17.4470226979395,-21.4988649618209,
-8.85844340682981));
#122874=CARTESIAN_POINT('Ctrl Pts',(-20.1788939786226,-21.4127139411785,
-8.98561921351124));
#122875=CARTESIAN_POINT('Ctrl Pts',(-21.5851647141539,-19.0690106086366,
-9.11279502019268));
#122876=CARTESIAN_POINT('Ctrl Pts',(-20.3756687876888,-16.617957305168,
-9.23997082687412));
#122877=CARTESIAN_POINT('Ctrl Pts',(-17.6600436419756,-16.3082433071803,
-9.36714663355554));
#122878=CARTESIAN_POINT('Ctrl Pts',(-15.9297067975006,-18.4240119848083,
-9.49432244023699));
#122879=CARTESIAN_POINT('Ctrl Pts',(-16.772134912253,-21.0241768957426,
-9.62149824691841));
#122880=CARTESIAN_POINT('Ctrl Pts',(-19.4144524779331,-21.7232481186362,
-9.74867405359986));
#122881=CARTESIAN_POINT('Ctrl Pts',(-21.4324971287534,-19.8798711957376,
-9.87584986028127));
#122882=CARTESIAN_POINT('Ctrl Pts',(-20.9748381515633,-17.1852300409311,
-10.0030256669627));
#122883=CARTESIAN_POINT('Ctrl Pts',(-18.461349252415,-16.1114906654595,
-10.1302014736441));
#122884=CARTESIAN_POINT('Ctrl Pts',(-16.1980004915621,-17.6437423025364,
-10.2573772803256));
#122885=CARTESIAN_POINT('Ctrl Pts',(-16.2612738778198,-20.3762391774058,
-10.384553087007));
#122886=CARTESIAN_POINT('Ctrl Pts',(-18.5931200064859,-21.8020850052583,
-10.5117288936884));
#122887=CARTESIAN_POINT('Ctrl Pts',(-21.0542147852026,-20.6131547370118,
-10.6389047003698));
#122888=CARTESIAN_POINT('Ctrl Pts',(-21.3866565072667,-17.900218100448,
-10.7660805070513));
#122889=CARTESIAN_POINT('Ctrl Pts',(-19.2854505263445,-16.152226075776,
-10.8932563137327));
#122890=CARTESIAN_POINT('Ctrl Pts',(-16.6783229143809,-16.9728528530119,
-11.0204321204142));
#122891=CARTESIAN_POINT('Ctrl Pts',(-15.9571514387634,-19.6092242978837,
-11.1476079270956));
#122892=CARTESIAN_POINT('Ctrl Pts',(-17.7835661674212,-21.6426332413875,
-11.274783733777));
#122893=CARTESIAN_POINT('Ctrl Pts',(-20.4819449468934,-21.2075531854514,
-11.4019595404585));
#122894=CARTESIAN_POINT('Ctrl Pts',(-21.5766927272896,-18.7031430772827,
-11.5291353471399));
#122895=CARTESIAN_POINT('Ctrl Pts',(-20.0634463678067,-16.4270437499047,
-11.6563111538213));
#122896=CARTESIAN_POINT('Ctrl Pts',(-17.3305154806086,-16.4674350655298,
-11.7834869605028));
#122897=CARTESIAN_POINT('Ctrl Pts',(-15.8851945298786,-18.78726049904,-11.9106627671842));
#122898=CARTESIAN_POINT('Ctrl Pts',(-17.0534757811762,-21.2582241997943,
-12.0378385738656));
#122899=CARTESIAN_POINT('Ctrl Pts',(-19.7635336981482,-21.6133703376545,
-12.1650143805471));
#122900=CARTESIAN_POINT('Ctrl Pts',(-21.5290583471371,-19.526874373989,
-12.2921901872285));
#122901=CARTESIAN_POINT('Ctrl Pts',(-20.7302904435137,-16.9129668529163,
-12.4193659939099));
#122902=CARTESIAN_POINT('Ctrl Pts',(-18.1000499617251,-16.1697456876228,
-12.5465418005913));
#122903=CARTESIAN_POINT('Ctrl Pts',(-16.0514192926768,-17.9790701677574,
-12.6737176072728));
#122904=CARTESIAN_POINT('Ctrl Pts',(-16.4638899228612,-20.6809973821388,
-12.8008934139542));
#122905=CARTESIAN_POINT('Ctrl Pts',(-18.9590456498985,-21.7966768120881,
-12.9280692206357));
#122906=CARTESIAN_POINT('Ctrl Pts',(-21.2477359610623,-20.3025418275019,
-13.0552450273171));
#122907=CARTESIAN_POINT('Ctrl Pts',(-21.2302295480009,-17.569368540262,
-13.1824208339985));
#122908=CARTESIAN_POINT('Ctrl Pts',(-18.9225874581277,-16.1046738015453,
-13.30959664068));
#122909=CARTESIAN_POINT('Ctrl Pts',(-16.44192808048,-17.2522241249159,-13.4367724473614));
#122910=CARTESIAN_POINT('Ctrl Pts',(-16.0641024269644,-19.9592133136872,
-13.5639482540428));
#122911=CARTESIAN_POINT('Ctrl Pts',(-18.1357420841767,-21.7421468018591,
-13.6911240607243));
#122912=CARTESIAN_POINT('Ctrl Pts',(-20.7562462470829,-20.9652937753664,
-13.8182998674057));
#122913=CARTESIAN_POINT('Ctrl Pts',(-21.521464993048,-18.3413686690794,
-13.9454756740872));
#122914=CARTESIAN_POINT('Ctrl Pts',(-19.7293576174809,-16.2776599088574,
-14.0726514807686));
#122915=CARTESIAN_POINT('Ctrl Pts',(-17.0240714067361,-16.6674921939926,
-14.19982728745));
#122916=CARTESIAN_POINT('Ctrl Pts',(-15.8875385501732,-19.1532185985939,
-14.3270030941314));
#122917=CARTESIAN_POINT('Ctrl Pts',(-17.3624574025039,-21.4543394280201,
-14.4541789008129));
#122918=CARTESIAN_POINT('Ctrl Pts',(-20.0956814605031,-21.4597191449386,
-14.5813547074943));
#122919=CARTESIAN_POINT('Ctrl Pts',(-21.5796472939737,-19.1644221929799,
-14.7085305141757));
#122920=CARTESIAN_POINT('Ctrl Pts',(-20.4529083560135,-16.6742410633702,
-14.8357063208572));
#122921=CARTESIAN_POINT('Ctrl Pts',(-17.7491776888957,-16.2737623844548,
-14.9628821275386));
#122922=CARTESIAN_POINT('Ctrl Pts',(-15.9489603672498,-18.3304004876284,
-15.0900579342201));
#122923=CARTESIAN_POINT('Ctrl Pts',(-16.7038440495977,-20.9573175625861,
-15.2172337409015));
#122924=CARTESIAN_POINT('Ctrl Pts',(-19.3212698107507,-21.7444802379159,
-15.3444095475829));
#122925=CARTESIAN_POINT('Ctrl Pts',(-21.3999119706151,-19.9697156158284,
-15.4715853542643));
#122926=CARTESIAN_POINT('Ctrl Pts',(-21.032745362598,-17.2612600827733,
-15.5987611609458));
#122927=CARTESIAN_POINT('Ctrl Pts',(-18.5566225606254,-16.1039534846195,
-15.7259369676272));
#122928=CARTESIAN_POINT('Ctrl Pts',(-16.2432325499933,-17.5595527946246,
-15.8531127743086));
#122929=CARTESIAN_POINT('Ctrl Pts',(-16.2149670802795,-20.2926359905412,
-15.9802885809901));
#122930=CARTESIAN_POINT('Ctrl Pts',(-18.4977579655933,-21.7957688743899,
-16.1074643876715));
#122931=CARTESIAN_POINT('Ctrl Pts',(-20.997286254641,-20.6899203201883,
-16.234640194353));
#122932=CARTESIAN_POINT('Ctrl Pts',(-21.4203898804431,-17.9896377397141,
-16.3618160010344));
#122933=CARTESIAN_POINT('Ctrl Pts',(-19.378897527099,-16.1722628021139,
-16.4889918077158));
#122934=CARTESIAN_POINT('Ctrl Pts',(-16.7457517194962,-16.9051242136259,
-16.6161676143973));
#122935=CARTESIAN_POINT('Ctrl Pts',(-15.9367003046499,-19.5158671156972,
-16.7433434210787));
#122936=CARTESIAN_POINT('Ctrl Pts',(-17.6939977402874,-21.6092969366562,
-16.8705192277601));
#122937=CARTESIAN_POINT('Ctrl Pts',(-20.4054326993911,-21.2648217486819,
-16.9976950344416));
#122938=CARTESIAN_POINT('Ctrl Pts',(-21.5834318976165,-18.798476156199,
-17.124870841123));
#122939=CARTESIAN_POINT('Ctrl Pts',(-20.147254185468,-16.4729791616393,
-17.2520466478045));
#122940=CARTESIAN_POINT('Ctrl Pts',(-17.4145034745997,-16.4218299208892,
-17.3792224544858));
#122941=CARTESIAN_POINT('Ctrl Pts',(-15.8923089285959,-18.691954687658,
-17.5063982611673));
#122942=CARTESIAN_POINT('Ctrl Pts',(-16.9771895653652,-21.200654888267,
-17.6335740678487));
#122943=CARTESIAN_POINT('Ctrl Pts',(-19.6738347359604,-21.646353796156,
-17.7607498745302));
#122944=CARTESIAN_POINT('Ctrl Pts',(-21.5082398690315,-19.6201503265241,
-17.8879256812116));
#122945=CARTESIAN_POINT('Ctrl Pts',(-20.7974521110171,-16.980960402401,
-18.015101487893));
#122946=CARTESIAN_POINT('Ctrl Pts',(-18.1935751134159,-16.1500769725442,
-18.1422772945745));
#122947=CARTESIAN_POINT('Ctrl Pts',(-16.0855044067243,-17.8897840134535,
-18.2694531012559));
#122948=CARTESIAN_POINT('Ctrl Pts',(-16.407264022649,-20.6040082933991,
-18.3966289079374));
#122949=CARTESIAN_POINT('Ctrl Pts',(-18.8636594843459,-21.8026174994663,
-18.5238047146188));
#122950=CARTESIAN_POINT('Ctrl Pts',(-21.2011004165875,-20.3859620788242,
-18.6509805213002));
#122951=CARTESIAN_POINT('Ctrl Pts',(-21.275129842407,-17.6537354530185,
-18.7781563279817));
#122952=CARTESIAN_POINT('Ctrl Pts',(-19.0178303575923,-16.1125859688478,
-18.9053321346631));
#122953=CARTESIAN_POINT('Ctrl Pts',(-16.500134137209,-17.1764226259579,
-19.0325079413445));
#122954=CARTESIAN_POINT('Ctrl Pts',(-16.031871194612,-19.8692413158911,
-19.1596837480259));
#122955=CARTESIAN_POINT('Ctrl Pts',(-18.0426437217303,-21.7205480348836,
-19.2868595547074));
#122956=CARTESIAN_POINT('Ctrl Pts',(-20.6876927164292,-21.0318837558328,
-19.4140353613888));
#122957=CARTESIAN_POINT('Ctrl Pts',(-21.5403499177572,-18.4350552451234,
-19.5412111680702));
#122958=CARTESIAN_POINT('Ctrl Pts',(-19.8183552240814,-16.3124914190809,
-19.6683869747517));
#122959=CARTESIAN_POINT('Ctrl Pts',(-17.1015319673585,-16.6115129719686,
-19.7955627814331));
#122960=CARTESIAN_POINT('Ctrl Pts',(-15.8823967072827,-19.0577859474646,
-19.9227385881146));
#122961=CARTESIAN_POINT('Ctrl Pts',(-17.2794306722399,-21.4070071875673,
-20.049914394796));
#122962=CARTESIAN_POINT('Ctrl Pts',(-20.0109413400502,-21.5039111192106,
-20.1770902014774));
#122963=CARTESIAN_POINT('Ctrl Pts',(-21.5709383060712,-19.2595961229167,
-20.3042660081589));
#122964=CARTESIAN_POINT('Ctrl Pts',(-20.5282190658065,-16.7330785895595,
-20.4314418148403));
#122965=CARTESIAN_POINT('Ctrl Pts',(-17.8394178740343,-16.242287940109,
-20.5586176215217));
#122966=CARTESIAN_POINT('Ctrl Pts',(-15.9713350959043,-18.2374818071192,
-20.6857934282032));
#122967=CARTESIAN_POINT('Ctrl Pts',(-16.6378358446413,-20.8882174033637,
-20.8129692348846));
#122968=CARTESIAN_POINT('Ctrl Pts',(-19.2274179364899,-21.762563581795,
-20.9401450415661));
#122969=CARTESIAN_POINT('Ctrl Pts',(-21.3643566264617,-20.0584501617399,
-21.0673208482474));
#122970=CARTESIAN_POINT('Ctrl Pts',(-21.0880352148013,-17.3391255539126,
-21.1944966549289));
#122971=CARTESIAN_POINT('Ctrl Pts',(-18.6521697017704,-16.099728633828,
-21.3216724616103));
#122972=CARTESIAN_POINT('Ctrl Pts',(-16.2911142372801,-17.4766984270906,
-21.4488482682919));
#122973=CARTESIAN_POINT('Ctrl Pts',(-16.171763941479,-20.2079662407414,
-21.5760240749732));
#122974=CARTESIAN_POINT('Ctrl Pts',(-18.4021242436095,-21.7854176013747,
-21.7031998816546));
#122975=CARTESIAN_POINT('Ctrl Pts',(-20.9388617241559,-20.7663921293681,
-21.8303756883361));
#122976=CARTESIAN_POINT('Ctrl Pts',(-21.4490185879752,-18.0766920512704,
-21.9575514950175));
#122977=CARTESIAN_POINT('Ctrl Pts',(-20.1339758401221,-16.8284619738791,
-22.0423353661385));
#122978=CARTESIAN_POINT('Ctrl Pts',(-19.3578031818887,-16.6207695219882,
-22.0847273016989));
#122979=CARTESIAN_POINT('Ctrl Pts',(-16.7733105073354,-17.3009161969877,
0.257713229587529));
#122980=CARTESIAN_POINT('Ctrl Pts',(-16.2233207772202,-17.9539921151271,
0.215302637523872));
#122981=CARTESIAN_POINT('Ctrl Pts',(-15.8372817569514,-19.8413757484949,
0.130500109899736));
#122982=CARTESIAN_POINT('Ctrl Pts',(-17.9181413759371,-21.8731454397858,
0.00330564671512246));
#122983=CARTESIAN_POINT('Ctrl Pts',(-20.7467659253037,-21.217066072722,
-0.123870159966312));
#122984=CARTESIAN_POINT('Ctrl Pts',(-21.7289768454601,-18.4867051192915,
-0.251045966647746));
#122985=CARTESIAN_POINT('Ctrl Pts',(-19.9633971711666,-16.1812804129726,
-0.378221773329182));
#122986=CARTESIAN_POINT('Ctrl Pts',(-17.0699655841381,-16.4188255697332,
-0.505397580010615));
#122987=CARTESIAN_POINT('Ctrl Pts',(-15.703159676164,-18.9798787902334,
-0.632573386692051));
#122988=CARTESIAN_POINT('Ctrl Pts',(-17.1169733817962,-21.5156259816095,
-0.759749193373484));
#122989=CARTESIAN_POINT('Ctrl Pts',(-20.0143025574919,-21.6992647871434,
-0.886925000054919));
#122990=CARTESIAN_POINT('Ctrl Pts',(-21.737036760942,-19.362531670293,-1.01410080673635));
#122991=CARTESIAN_POINT('Ctrl Pts',(-20.7046694858076,-16.6491233362602,
-1.14127661341778));
#122992=CARTESIAN_POINT('Ctrl Pts',(-17.8643361221052,-16.0484810737661,
-1.26845242009922));
#122993=CARTESIAN_POINT('Ctrl Pts',(-15.8218649472086,-18.1116270070318,
-1.39562822678065));
#122994=CARTESIAN_POINT('Ctrl Pts',(-16.4510971650251,-20.9457682990692,
-1.52280403346208));
#122995=CARTESIAN_POINT('Ctrl Pts',(-19.1747509220124,-21.9507481746746,
-1.64997984014352));
#122996=CARTESIAN_POINT('Ctrl Pts',(-21.4940431258966,-20.2045641501962,
-1.77715564682495));
#122997=CARTESIAN_POINT('Ctrl Pts',(-21.2811670373152,-17.3092295202543,
-1.90433145350639));
#122998=CARTESIAN_POINT('Ctrl Pts',(-18.7314233036483,-15.9210352279973,
-2.03150726018783));
#122999=CARTESIAN_POINT('Ctrl Pts',(-16.1840435203226,-17.3135627916812,
-2.15868306686926));
#123000=CARTESIAN_POINT('Ctrl Pts',(-15.9760905434333,-20.2092549046476,
-2.28585887355069));
#123001=CARTESIAN_POINT('Ctrl Pts',(-18.2983483154525,-21.9514936229061,
-2.41303468023213));
#123002=CARTESIAN_POINT('Ctrl Pts',(-21.020289469658,-20.9418831396066,
-2.54021048691356));
#123003=CARTESIAN_POINT('Ctrl Pts',(-21.644701937954,-18.1066783673205,
-2.66738629359499));
#123004=CARTESIAN_POINT('Ctrl Pts',(-19.598726037039,-16.0470037339522,
-2.79456210027643));
#123005=CARTESIAN_POINT('Ctrl Pts',(-16.7594176679228,-16.6524828663812,
-2.92173790695786));
#123006=CARTESIAN_POINT('Ctrl Pts',(-15.7316660321737,-19.3676262467993,
-3.0489137136393));
#123007=CARTESIAN_POINT('Ctrl Pts',(-17.4583694659978,-21.701458341403,
-3.17608952032073));
#123008=CARTESIAN_POINT('Ctrl Pts',(-20.3553847402323,-21.512833058945,
-3.30326532700217));
#123009=CARTESIAN_POINT('Ctrl Pts',(-21.7648801497778,-18.9748023878472,
-3.4304411336836));
#123010=CARTESIAN_POINT('Ctrl Pts',(-20.3937311395464,-16.4158519413221,
-3.55761694036504));
#123011=CARTESIAN_POINT('Ctrl Pts',(-17.4998818233102,-16.1836599274567,
-3.68479274704647));
#123012=CARTESIAN_POINT('Ctrl Pts',(-15.7382593361759,-18.4912481076264,
-3.8119685537279));
#123013=CARTESIAN_POINT('Ctrl Pts',(-16.7250429714639,-21.2215475515407,
-3.93914436040934));
#123014=CARTESIAN_POINT('Ctrl Pts',(-19.5549199904986,-21.8696779809346,
-4.06632016709077));
#123015=CARTESIAN_POINT('Ctrl Pts',(-21.6316538702915,-19.8410199543343,
-4.19349597377222));
#123016=CARTESIAN_POINT('Ctrl Pts',(-21.0499701727744,-16.9967412984365,
-4.32067178045365));
#123017=CARTESIAN_POINT('Ctrl Pts',(-18.3435275870569,-15.9462911441802,
-4.44784758713508));
#123018=CARTESIAN_POINT('Ctrl Pts',(-15.9953192047637,-17.6533923098082,
-4.57502339381652));
#123019=CARTESIAN_POINT('Ctrl Pts',(-16.159680470399,-20.5518854305035,
-4.70219920049796));
#123020=CARTESIAN_POINT('Ctrl Pts',(-18.6858201241535,-21.9825829688008,
-4.82937500717938));
#123021=CARTESIAN_POINT('Ctrl Pts',(-21.2561618236167,-20.6329087324161,
-4.95655081386081));
#123022=CARTESIAN_POINT('Ctrl Pts',(-21.5125765929291,-17.7411050630016,
-5.08372662054226));
#123023=CARTESIAN_POINT('Ctrl Pts',(-19.219819796142,-15.9602223416674,
-5.21090242722368));
#123024=CARTESIAN_POINT('Ctrl Pts',(-16.4813534897718,-16.9241099311898,
-5.33807823390512));
#123025=CARTESIAN_POINT('Ctrl Pts',(-15.8095505415254,-19.748460793793,
-5.46525404058655));
#123026=CARTESIAN_POINT('Ctrl Pts',(-17.8207484596252,-21.8421083120231,
-5.59242984726799));
#123027=CARTESIAN_POINT('Ctrl Pts',(-20.6697979832357,-21.2842608343242,
-5.71960565394942));
#123028=CARTESIAN_POINT('Ctrl Pts',(-21.7428730064005,-18.5867087975656,
-5.84678146063087));
#123029=CARTESIAN_POINT('Ctrl Pts',(-20.0554937979133,-16.2242887665116,
-5.9739572673123));
#123030=CARTESIAN_POINT('Ctrl Pts',(-17.1557260509959,-16.3643744913304,
-6.10113307399374));
#123031=CARTESIAN_POINT('Ctrl Pts',(-15.7039266935608,-18.8784460142016,
-6.22830888067515));
#123032=CARTESIAN_POINT('Ctrl Pts',(-17.0320315272241,-21.4599987537674,
-6.35548468735659));
#123033=CARTESIAN_POINT('Ctrl Pts',(-19.9215867985823,-21.7406183007101,
-6.48266049403803));
#123034=CARTESIAN_POINT('Ctrl Pts',(-21.7216048921908,-19.4628536379228,
-6.60983630071946));
#123035=CARTESIAN_POINT('Ctrl Pts',(-20.7806809288866,-16.7164124694941,
-6.73701210740091));
#123036=CARTESIAN_POINT('Ctrl Pts',(-17.9620542446739,-16.0209841040936,
-6.86418791408233));
#123037=CARTESIAN_POINT('Ctrl Pts',(-15.8516398786156,-18.0145809038241,
-6.99136372076378));
#123038=CARTESIAN_POINT('Ctrl Pts',(-16.3856120244824,-20.868201541505,
-7.1185395274452));
#123039=CARTESIAN_POINT('Ctrl Pts',(-19.0740843804904,-21.9638261977359,
-7.24571533412664));
#123040=CARTESIAN_POINT('Ctrl Pts',(-21.4505504254156,-20.2962872525602,
-7.37289114080807));
#123041=CARTESIAN_POINT('Ctrl Pts',(-21.3347500631569,-17.3954481890373,
-7.50006694748951));
#123042=CARTESIAN_POINT('Ctrl Pts',(-18.8329229387055,-15.9226488015715,
-7.62724275417095));
#123043=CARTESIAN_POINT('Ctrl Pts',(-16.2403401578418,-17.2290911159235,
-7.75441856085238));
#123044=CARTESIAN_POINT('Ctrl Pts',(-15.9355355081732,-20.1161953956302,
-7.8815943675338));
#123045=CARTESIAN_POINT('Ctrl Pts',(-18.1981483374604,-21.9352226579616,
-8.00877017421523));
#123046=CARTESIAN_POINT('Ctrl Pts',(-20.9523718084227,-21.0173282912935,
-8.13594598089667));
#123047=CARTESIAN_POINT('Ctrl Pts',(-21.6713768328398,-18.2046234060944,
-8.26312178757811));
#123048=CARTESIAN_POINT('Ctrl Pts',(-19.6955209272938,-16.0775901583807,
-8.39029759425955));
#123049=CARTESIAN_POINT('Ctrl Pts',(-16.837529249675,-16.5876495343575,
-8.51747340094098));
#123050=CARTESIAN_POINT('Ctrl Pts',(-15.7194317772296,-19.2668537144213,
-8.64464920762241));
#123051=CARTESIAN_POINT('Ctrl Pts',(-17.3670135439705,-21.657199153529,
-8.77182501430385));
#123052=CARTESIAN_POINT('Ctrl Pts',(-20.2687205393704,-21.5656922728693,
-8.89900082098528));
#123053=CARTESIAN_POINT('Ctrl Pts',(-21.7624166953973,-19.07628495589,-9.02617662766673));
#123054=CARTESIAN_POINT('Ctrl Pts',(-20.4777284981358,-16.4728539058758,
-9.15335243434816));
#123055=CARTESIAN_POINT('Ctrl Pts',(-17.5932776318311,-16.1438855240604,
-9.28052824102959));
#123056=CARTESIAN_POINT('Ctrl Pts',(-15.7553687371063,-18.3911878826788,
-9.40770404771103));
#123057=CARTESIAN_POINT('Ctrl Pts',(-16.6501691513803,-21.1530005510137,
-9.53487985439245));
#123058=CARTESIAN_POINT('Ctrl Pts',(-19.4567550321338,-21.8955318232944,
-9.6620556610739));
#123059=CARTESIAN_POINT('Ctrl Pts',(-21.6002580301411,-19.9375553438918,
-9.78923146775533));
#123060=CARTESIAN_POINT('Ctrl Pts',(-21.1141471855306,-17.0753930069318,
-9.91640727443676));
#123061=CARTESIAN_POINT('Ctrl Pts',(-18.4443990267908,-15.9349011107458,
-10.0435830811182));
#123062=CARTESIAN_POINT('Ctrl Pts',(-16.0403417863069,-17.5624101831744,
-10.1707588877996));
#123063=CARTESIAN_POINT('Ctrl Pts',(-16.1075487696024,-20.4647816648694,
-10.297934694481));
#123064=CARTESIAN_POINT('Ctrl Pts',(-18.5843617408396,-21.9792698628662,
-10.4251105011625));
#123065=CARTESIAN_POINT('Ctrl Pts',(-21.1984585272586,-20.7164258552413,
-10.5522863078439));
#123066=CARTESIAN_POINT('Ctrl Pts',(-21.5515675764649,-17.8348306380519,
-10.6794621145253));
#123067=CARTESIAN_POINT('Ctrl Pts',(-19.319733252231,-15.9781689710992,
-10.8066379212068));
#123068=CARTESIAN_POINT('Ctrl Pts',(-16.5505250237807,-16.849812696393,
-10.9338137278882));
#123069=CARTESIAN_POINT('Ctrl Pts',(-15.7845195642707,-19.6500827962871,
-11.0609895345697));
#123070=CARTESIAN_POINT('Ctrl Pts',(-17.7244793391404,-21.8099052584926,
-11.1881653412511));
#123071=CARTESIAN_POINT('Ctrl Pts',(-20.5906116624301,-21.3477770276364,
-11.3153411479325));
#123072=CARTESIAN_POINT('Ctrl Pts',(-21.753418019756,-18.6876720726163,
-11.442516954614));
#123073=CARTESIAN_POINT('Ctrl Pts',(-20.1460957501734,-16.2700715849292,
-11.5696927612954));
#123074=CARTESIAN_POINT('Ctrl Pts',(-17.2432632743535,-16.3129739588191,
-11.6968685679768));
#123075=CARTESIAN_POINT('Ctrl Pts',(-15.7080892187581,-18.7770189290635,
-11.8240443746583));
#123076=CARTESIAN_POINT('Ctrl Pts',(-16.9490004957481,-21.4015981713421,
-11.9512201813397));
#123077=CARTESIAN_POINT('Ctrl Pts',(-19.8275380283252,-21.7788231306235,
-12.0783959880211));
#123078=CARTESIAN_POINT('Ctrl Pts',(-21.7028222925386,-19.5626133199888,
-12.2055717947026));
#123079=CARTESIAN_POINT('Ctrl Pts',(-20.8543963692405,-16.7862036872011,
-12.332747601384));
#123080=CARTESIAN_POINT('Ctrl Pts',(-18.0606383838055,-15.996777746927,
-12.4599234080654));
#123081=CARTESIAN_POINT('Ctrl Pts',(-15.8846478876935,-17.9185848020682,
-12.5870992147468));
#123082=CARTESIAN_POINT('Ctrl Pts',(-16.3227611038855,-20.7884861603309,
-12.7142750214283));
#123083=CARTESIAN_POINT('Ctrl Pts',(-18.9730363488984,-21.9735254516762,
-12.8414508281097));
#123084=CARTESIAN_POINT('Ctrl Pts',(-21.404010580066,-20.3865026781285,
-12.9686266347912));
#123085=CARTESIAN_POINT('Ctrl Pts',(-21.3854158235693,-17.4834127326752,
-13.0958024414726));
#123086=CARTESIAN_POINT('Ctrl Pts',(-18.9343116143732,-15.9276604541869,
-13.222978248154));
#123087=CARTESIAN_POINT('Ctrl Pts',(-16.2994339317307,-17.1465519972999,
-13.3501540548355));
#123088=CARTESIAN_POINT('Ctrl Pts',(-15.8981195105134,-20.0218300241493,
-13.4773298615169));
#123089=CARTESIAN_POINT('Ctrl Pts',(-18.0985494238061,-21.9156054049817,
-13.6045056681983));
#123090=CARTESIAN_POINT('Ctrl Pts',(-20.8819658002459,-21.0904567688396,
-13.7316814748798));
#123091=CARTESIAN_POINT('Ctrl Pts',(-21.694756872753,-18.3034067748831,
-13.8588572815612));
#123092=CARTESIAN_POINT('Ctrl Pts',(-19.7912372798057,-16.1114008087357,
-13.9860330882426));
#123093=CARTESIAN_POINT('Ctrl Pts',(-16.9177681021827,-16.5254682931038,
-14.1132088949241));
#123094=CARTESIAN_POINT('Ctrl Pts',(-15.7105789627421,-19.1657280110059,
-14.2403847016055));
#123095=CARTESIAN_POINT('Ctrl Pts',(-17.2771909703125,-21.6099055442666,
-14.367560508287));
#123096=CARTESIAN_POINT('Ctrl Pts',(-20.1803348428554,-21.6156197088857,
-14.4947363149684));
#123097=CARTESIAN_POINT('Ctrl Pts',(-21.7565562667429,-19.1776281134862,
-14.6219121216498));
#123098=CARTESIAN_POINT('Ctrl Pts',(-20.5597699168931,-16.5326367280232,
-14.7490879283312));
#123099=CARTESIAN_POINT('Ctrl Pts',(-17.6879529883551,-16.107260981979,
-14.8762637350127));
#123100=CARTESIAN_POINT('Ctrl Pts',(-15.7758192680016,-18.2917567205529,
-15.0034395416941));
#123101=CARTESIAN_POINT('Ctrl Pts',(-16.5776327638535,-21.0819846886999,
-15.1306153483755));
#123102=CARTESIAN_POINT('Ctrl Pts',(-19.3577793596249,-21.9180839067241,
-15.257791155057));
#123103=CARTESIAN_POINT('Ctrl Pts',(-21.5656471090539,-20.0329852362584,
-15.3849669617384));
#123104=CARTESIAN_POINT('Ctrl Pts',(-21.1756543877665,-17.1561497050361,
-15.5121427684199));
#123105=CARTESIAN_POINT('Ctrl Pts',(-18.545595311866,-15.9268953564031,
-15.6393185751013));
#123106=CARTESIAN_POINT('Ctrl Pts',(-16.0883858436145,-17.4729867591009,
-15.7664943817827));
#123107=CARTESIAN_POINT('Ctrl Pts',(-16.0583631585132,-20.3759810124089,
-15.8936701884641));
#123108=CARTESIAN_POINT('Ctrl Pts',(-18.4830712067246,-21.9725610690611,
-16.0208459951456));
#123109=CARTESIAN_POINT('Ctrl Pts',(-21.1379908483687,-20.7979638220132,
-16.148021801827));
#123110=CARTESIAN_POINT('Ctrl Pts',(-21.5873980951341,-17.9298093417044,
-16.2751976085084));
#123111=CARTESIAN_POINT('Ctrl Pts',(-19.418989691473,-15.9994513460744,
-16.4023734151899));
#123112=CARTESIAN_POINT('Ctrl Pts',(-16.6221457611405,-16.7778734845843,
-16.5295492218713));
#123113=CARTESIAN_POINT('Ctrl Pts',(-15.7627970185048,-19.550921759478,
-16.6567250285528));
#123114=CARTESIAN_POINT('Ctrl Pts',(-17.6293425977359,-21.7744964933273,
-16.7839008352342));
#123115=CARTESIAN_POINT('Ctrl Pts',(-20.5093427807734,-21.4086058784384,
-16.9110766419156));
#123116=CARTESIAN_POINT('Ctrl Pts',(-21.7605761526514,-18.7889318442388,
-17.0382524485971));
#123117=CARTESIAN_POINT('Ctrl Pts',(-20.2351137549734,-16.3188627217991,
-17.1654282552785));
#123118=CARTESIAN_POINT('Ctrl Pts',(-17.3324726567343,-16.2645336211774,
-17.2926040619599));
#123119=CARTESIAN_POINT('Ctrl Pts',(-15.7156459073444,-18.6757881201507,
-17.4197798686414));
#123120=CARTESIAN_POINT('Ctrl Pts',(-16.8679716977821,-21.3404498752418,
-17.5469556753228));
#123121=CARTESIAN_POINT('Ctrl Pts',(-19.7322626367279,-21.813857113719,
-17.6741314820042));
#123122=CARTESIAN_POINT('Ctrl Pts',(-21.6807095656397,-19.6616880772395,
-17.8013072886857));
#123123=CARTESIAN_POINT('Ctrl Pts',(-20.925733361505,-16.8584242781114,
-17.9284830953671));
#123124=CARTESIAN_POINT('Ctrl Pts',(-18.1599778324925,-15.9758862618349,
-18.0556589020486));
#123125=CARTESIAN_POINT('Ctrl Pts',(-15.9208520143557,-17.8237478819072,
-18.18283470873));
#123126=CARTESIAN_POINT('Ctrl Pts',(-16.2626148693509,-20.7067107930414,
-18.3100105154114));
#123127=CARTESIAN_POINT('Ctrl Pts',(-18.871720190335,-21.9798354613185,
-18.4371863220928));
#123128=CARTESIAN_POINT('Ctrl Pts',(-21.3544757844137,-20.4751090222602,
-18.5643621287743));
#123129=CARTESIAN_POINT('Ctrl Pts',(-21.4331074916559,-17.573024590546,
-18.6915379354557));
#123130=CARTESIAN_POINT('Ctrl Pts',(-19.0354756002437,-15.9360645072522,
-18.8187137421372));
#123131=CARTESIAN_POINT('Ctrl Pts',(-16.3612585583812,-17.0660380501958,
-18.9458895488186));
#123132=CARTESIAN_POINT('Ctrl Pts',(-15.8638845181663,-19.926264622792,
-19.0730653555));
#123133=CARTESIAN_POINT('Ctrl Pts',(-17.9996632971129,-21.8926638800028,
-19.2002411621814));
#123134=CARTESIAN_POINT('Ctrl Pts',(-20.8091504151054,-21.1611865332722,
-19.3274169688629));
#123135=CARTESIAN_POINT('Ctrl Pts',(-21.7148158405836,-18.4029176833963,
-19.4545927755443));
#123136=CARTESIAN_POINT('Ctrl Pts',(-19.8857677137514,-16.1483977337339,
-19.5817685822257));
#123137=CARTESIAN_POINT('Ctrl Pts',(-17.0000442519466,-16.4660089396223,
-19.7089443889072));
#123138=CARTESIAN_POINT('Ctrl Pts',(-15.7051174603682,-19.0643624769379,
-19.8361201955886));
#123139=CARTESIAN_POINT('Ctrl Pts',(-17.1890026117629,-21.5596307402518,
-19.9632960022701));
#123140=CARTESIAN_POINT('Ctrl Pts',(-20.0903265756109,-21.6625590217998,
-20.0904718089515));
#123141=CARTESIAN_POINT('Ctrl Pts',(-21.7473058561185,-19.2787188421125,
-20.2176476156329));
#123142=CARTESIAN_POINT('Ctrl Pts',(-20.6397625633182,-16.5951320814986,
-20.3448234223144));
#123143=CARTESIAN_POINT('Ctrl Pts',(-17.7838032497984,-16.0738298258407,
-20.4719992289958));
#123144=CARTESIAN_POINT('Ctrl Pts',(-15.7995849948555,-18.1930614463123,
-20.5991750356772));
#123145=CARTESIAN_POINT('Ctrl Pts',(-16.5075209429087,-21.0085886920376,
-20.7263508423587));
#123146=CARTESIAN_POINT('Ctrl Pts',(-19.2580928765906,-21.9372914608301,
-20.8535266490401));
#123147=CARTESIAN_POINT('Ctrl Pts',(-21.5278813506218,-20.1272362554868,
-20.9807024557215));
#123148=CARTESIAN_POINT('Ctrl Pts',(-21.2343815144973,-17.2388559379038,
-21.107878262403));
#123149=CARTESIAN_POINT('Ctrl Pts',(-18.647082453596,-15.9224078539418,
-21.2350540690844));
#123150=CARTESIAN_POINT('Ctrl Pts',(-16.1392442526231,-17.3849814787741,
-21.3622298757658));
#123151=CARTESIAN_POINT('Ctrl Pts',(-16.0124741552623,-20.2860474906393,
-21.4894056824473));
#123152=CARTESIAN_POINT('Ctrl Pts',(-18.3814921015747,-21.9615662752975,
-21.6165814891287));
#123153=CARTESIAN_POINT('Ctrl Pts',(-21.0759341658266,-20.8791897513666,
-21.7437572958101));
#123154=CARTESIAN_POINT('Ctrl Pts',(-21.6178065999207,-18.0222756693125,
-21.8709331024916));
#123155=CARTESIAN_POINT('Ctrl Pts',(-20.2210099178527,-16.6964452859245,
-21.9557169736125));
#123156=CARTESIAN_POINT('Ctrl Pts',(-19.3965839472885,-16.475840953354,
-21.998108909173));
#123157=CARTESIAN_POINT('Ctrl Pts',(-17.1140743056112,-17.5890877707427,
-8.67361737988404E-19));
#123158=CARTESIAN_POINT('Ctrl Pts',(-17.0606037558837,-17.6406831599911,
-2.5078829569074E-15));
#123159=CARTESIAN_POINT('Ctrl Pts',(-17.0102648206888,-17.6951284552545,
-2.007042086044E-14));
#123160=CARTESIAN_POINT('Ctrl Pts',(-16.9630512610728,-17.7520566525928,
-1.37546224410201E-14));
#123161=CARTESIAN_POINT('Ctrl Pts',(-16.9139640310005,-17.811244045856,
-7.38887994500031E-15));
#123162=CARTESIAN_POINT('Ctrl Pts',(-16.8682546395764,-17.873115719352,
2.33283173511089E-14));
#123163=CARTESIAN_POINT('Ctrl Pts',(-16.8259443403958,-17.937308752054,
1.43114686768087E-14));
#123164=CARTESIAN_POINT('Ctrl Pts',(-16.7856210013394,-17.9984871760508,
5.71806580905755E-15));
#123165=CARTESIAN_POINT('Ctrl Pts',(-16.7483849217229,-18.061774974692,
-4.47536531428885E-15));
#123166=CARTESIAN_POINT('Ctrl Pts',(-16.7142833600929,-18.1268912399334,
5.98826543907194E-15));
#123167=CARTESIAN_POINT('Ctrl Pts',(-16.6917479443229,-18.1699221757752,
1.29207969252189E-14));
#123168=CARTESIAN_POINT('Ctrl Pts',(-16.670581955631,-18.2137522504246,
3.54242763103226E-14));
#123169=CARTESIAN_POINT('Ctrl Pts',(-16.6508067523184,-18.2583061596181,
7.78543896018391E-15));
#123170=CARTESIAN_POINT('Ctrl Pts',(-16.6447946121616,-18.271851625744,
-8.45379769840918E-16));
#123171=CARTESIAN_POINT('Ctrl Pts',(-16.6389106011744,-18.2854654139231,
-1.30923055976207E-14));
#123172=CARTESIAN_POINT('Ctrl Pts',(-16.6331633226596,-18.2991259028343,
-9.75608482889356E-15));
#123173=CARTESIAN_POINT('Ctrl Pts',(-16.6020274374077,-18.3731316107767,
9.37891228514535E-15));
#123174=CARTESIAN_POINT('Ctrl Pts',(-16.5748437493431,-18.4486320984917,
1.93805730149152E-15));
#123175=CARTESIAN_POINT('Ctrl Pts',(-16.5516340690814,-18.5252437971799,
-1.49880108324396E-15));
#123176=CARTESIAN_POINT('Ctrl Pts',(-16.5281113691171,-18.6028887272984,
-4.98201100652448E-15));
#123177=CARTESIAN_POINT('Ctrl Pts',(-16.5086701130901,-18.681675875735,
-7.86786714558005E-15));
#123178=CARTESIAN_POINT('Ctrl Pts',(-16.4933735667358,-18.7612412026049,
-6.84174938925253E-15));
#123179=CARTESIAN_POINT('Ctrl Pts',(-16.4780905784648,-18.8407360068025,
-5.81654113168692E-15));
#123180=CARTESIAN_POINT('Ctrl Pts',(-16.4669445521158,-18.9210085587578,
6.00582690367431E-15));
#123181=CARTESIAN_POINT('Ctrl Pts',(-16.4600452985135,-19.0017172100912,
9.58955137519979E-15));
#123182=CARTESIAN_POINT('Ctrl Pts',(-16.4582499089088,-19.0227199854594,
1.05221423529152E-14));
#123183=CARTESIAN_POINT('Ctrl Pts',(-16.4567423723373,-19.0437523636843,
5.40618910968218E-15));
#123184=CARTESIAN_POINT('Ctrl Pts',(-16.4555251966164,-19.0648084381479,
-2.52575738102223E-15));
#123185=CARTESIAN_POINT('Ctrl Pts',(-16.4546316923203,-19.0802652803004,
-8.37958959373255E-15));
#123186=CARTESIAN_POINT('Ctrl Pts',(-16.4538946607534,-19.0957348924738,
-2.64516391872053E-16));
#123187=CARTESIAN_POINT('Ctrl Pts',(-16.4533151797917,-19.1112149436894,
-8.82627304576999E-15));
#123188=CARTESIAN_POINT('Ctrl Pts',(-16.4528674697077,-19.1231749138822,
-1.55251639105376E-14));
#123189=CARTESIAN_POINT('Ctrl Pts',(-16.4525139746189,-19.1351378160613,
-1.99942219331142E-14));
#123190=CARTESIAN_POINT('Ctrl Pts',(-16.4522551154433,-19.1470940326229,
-1.58206781009085E-14));
#123191=CARTESIAN_POINT('Ctrl Pts',(-16.450448336251,-19.23054575209,1.4416882724211E-14));
#123192=CARTESIAN_POINT('Ctrl Pts',(-16.4532433905666,-19.3137912323742,
1.21306277354053E-14));
#123193=CARTESIAN_POINT('Ctrl Pts',(-16.4606965224471,-19.3964498394684,
8.65973959207622E-15));
#123194=CARTESIAN_POINT('Ctrl Pts',(-16.4681353636814,-19.4789499568243,
5.1686934198692E-15));
#123195=CARTESIAN_POINT('Ctrl Pts',(-16.4802140623254,-19.560866453353,
1.07908903342738E-14));
#123196=CARTESIAN_POINT('Ctrl Pts',(-16.4970379007565,-19.6418365052423,
-5.4678483962789E-15));
#123197=CARTESIAN_POINT('Ctrl Pts',(-16.5134756240274,-19.7209482556099,
-2.11473992649223E-14));
#123198=CARTESIAN_POINT('Ctrl Pts',(-16.5344429618587,-19.7991574576156,
-2.06891388249104E-14));
#123199=CARTESIAN_POINT('Ctrl Pts',(-16.5596742522225,-19.8762376297952,
-9.24260668000443E-15));
#123200=CARTESIAN_POINT('Ctrl Pts',(-16.5700716763688,-19.9080011754509,
-4.62300519733931E-15));
#123201=CARTESIAN_POINT('Ctrl Pts',(-16.5811937949009,-19.9395729260017,
5.7031583328198E-15));
#123202=CARTESIAN_POINT('Ctrl Pts',(-16.593024502045,-19.9709365575929,
-9.27036225562006E-15));
#123203=CARTESIAN_POINT('Ctrl Pts',(-16.599575769931,-19.9883042051838,
-1.76032698893732E-14));
#123204=CARTESIAN_POINT('Ctrl Pts',(-16.6063465654584,-20.005613174688,
-7.16344049788605E-15));
#123205=CARTESIAN_POINT('Ctrl Pts',(-16.6133217610784,-20.0228306160632,
-1.08524300657109E-14));
#123206=CARTESIAN_POINT('Ctrl Pts',(-16.6442809363235,-20.0992496606094,
-2.70898603106819E-14));
#123207=CARTESIAN_POINT('Ctrl Pts',(-16.6792960167752,-20.1739619594251,
-1.89218150302011E-14));
#123208=CARTESIAN_POINT('Ctrl Pts',(-16.7180389842821,-20.246743899253,
-5.16253706450698E-15));
#123209=CARTESIAN_POINT('Ctrl Pts',(-16.7588459173261,-20.3234031728317,
9.3297429751869E-15));
#123210=CARTESIAN_POINT('Ctrl Pts',(-16.803788552284,-20.3979217843379,
7.49644749155628E-15));
#123211=CARTESIAN_POINT('Ctrl Pts',(-16.8525440995263,-20.4700328123178,
-7.60502771868232E-15));
#123212=CARTESIAN_POINT('Ctrl Pts',(-16.9012996467686,-20.5421438402977,
-2.27065029289209E-14));
#123213=CARTESIAN_POINT('Ctrl Pts',(-16.9538687049381,-20.6118481705157,
-1.06758067088701E-14));
#123214=CARTESIAN_POINT('Ctrl Pts',(-17.009981736112,-20.6788601850433,
4.96824803519758E-15));
#123215=CARTESIAN_POINT('Ctrl Pts',(-17.0318954596463,-20.7050302694089,
1.09555345227255E-14));
#123216=CARTESIAN_POINT('Ctrl Pts',(-17.0543502078806,-20.7307894693846,
-3.37511572030332E-15));
#123217=CARTESIAN_POINT('Ctrl Pts',(-17.0773318266369,-20.7561195433156,
-1.82909243306995E-14));
#123218=CARTESIAN_POINT('Ctrl Pts',(-17.0864635878594,-20.7661844647356,
-2.42397533361988E-14));
#123219=CARTESIAN_POINT('Ctrl Pts',(-17.0956793012105,-20.776182428681,
-2.66883060451255E-15));
#123220=CARTESIAN_POINT('Ctrl Pts',(-17.1049757714685,-20.7861097474567,
-2.1094237467878E-15));
#123221=CARTESIAN_POINT('Ctrl Pts',(-17.1654853800672,-20.8507254733048,
1.12948522341814E-15));
#123222=CARTESIAN_POINT('Ctrl Pts',(-17.2292147782235,-20.9121401114294,
-1.67082407375528E-14));
#123223=CARTESIAN_POINT('Ctrl Pts',(-17.2958558788046,-20.9700792980957,
-2.3037127760972E-15));
#123224=CARTESIAN_POINT('Ctrl Pts',(-17.3510487696017,-21.018065168297,
9.62627535178633E-15));
#123225=CARTESIAN_POINT('Ctrl Pts',(-17.4082400170084,-21.063667078019,
-2.71614749528282E-14));
#123226=CARTESIAN_POINT('Ctrl Pts',(-17.4672777570143,-21.1067151950334,
-5.6621374255883E-15));
#123227=CARTESIAN_POINT('Ctrl Pts',(-17.4867746670186,-21.1209316142798,
1.51004478036007E-15));
#123228=CARTESIAN_POINT('Ctrl Pts',(-17.5064731111025,-21.1348693857667,
-3.24941689518543E-14));
#123229=CARTESIAN_POINT('Ctrl Pts',(-17.5263680478785,-21.1485219846966,
-2.4008572907519E-14));
#123230=CARTESIAN_POINT('Ctrl Pts',(-17.5422931318004,-21.1594503322534,
-1.70799939015646E-14));
#123231=CARTESIAN_POINT('Ctrl Pts',(-17.5583454808324,-21.1701967133747,
-2.25387075678082E-14));
#123232=CARTESIAN_POINT('Ctrl Pts',(-17.574506564613,-21.1807476004758,
-2.41195952099815E-14));
#123233=CARTESIAN_POINT('Ctrl Pts',(-17.6490343637846,-21.2294036439462,
-3.11874514914714E-14));
#123234=CARTESIAN_POINT('Ctrl Pts',(-17.7259442979181,-21.2739559986071,
-3.29361491763752E-14));
#123235=CARTESIAN_POINT('Ctrl Pts',(-17.804955500985,-21.3141140597646,
-1.57651669496772E-14));
#123236=CARTESIAN_POINT('Ctrl Pts',(-17.8827967354047,-21.3536774752179,
1.60414781620485E-15));
#123237=CARTESIAN_POINT('Ctrl Pts',(-17.9626781499771,-21.3889764950412,
-4.80502357855522E-15));
#123238=CARTESIAN_POINT('Ctrl Pts',(-18.0443636118602,-21.4196958725292,
4.32986979603811E-15));
#123239=CARTESIAN_POINT('Ctrl Pts',(-18.0530583776972,-21.4229657052236,
5.14226553249037E-15));
#123240=CARTESIAN_POINT('Ctrl Pts',(-18.0617736083461,-21.4261836096314,
1.19766446651732E-14));
#123241=CARTESIAN_POINT('Ctrl Pts',(-18.0705088883292,-21.4293497159892,
-1.11022302462516E-16));
#123242=CARTESIAN_POINT('Ctrl Pts',(-19.3965839546295,-21.4281590740807,
-0.00189110722368073));
#123243=CARTESIAN_POINT('Ctrl Pts',(-20.2210099343281,-21.207554739066,
-0.0442830427841589));
#123244=CARTESIAN_POINT('Ctrl Pts',(-21.6178066866466,-19.8817246731204,
-0.129066913905115));
#123245=CARTESIAN_POINT('Ctrl Pts',(-21.0759341432978,-17.0248100445211,
-0.25624272058655));
#123246=CARTESIAN_POINT('Ctrl Pts',(-18.381492106794,-15.9424338299618,
-0.383418527267984));
#123247=CARTESIAN_POINT('Ctrl Pts',(-16.0124741472572,-17.6179524340247,
-0.510594333949419));
#123248=CARTESIAN_POINT('Ctrl Pts',(-16.1392442377966,-20.5190185688902,
-0.637770140630851));
#123249=CARTESIAN_POINT('Ctrl Pts',(-18.6470824574045,-21.9815921336573,
-0.764945947312287));
#123250=CARTESIAN_POINT('Ctrl Pts',(-21.2343815212355,-20.6651440828081,
-0.892121753993719));
#123251=CARTESIAN_POINT('Ctrl Pts',(-21.5278813636115,-17.7767637319101,
-1.01929756067515));
#123252=CARTESIAN_POINT('Ctrl Pts',(-19.2580928773362,-15.966708532015,
-1.14647336735659));
#123253=CARTESIAN_POINT('Ctrl Pts',(-16.5075209349949,-16.8954112973593,
-1.27364917403802));
#123254=CARTESIAN_POINT('Ctrl Pts',(-15.7995849828837,-19.7109385580857,
-1.40082498071946));
#123255=CARTESIAN_POINT('Ctrl Pts',(-17.7838032463622,-21.8301701846349,
-1.52800078740089));
#123256=CARTESIAN_POINT('Ctrl Pts',(-20.6397625706149,-21.308867928169,
-1.65517659408233));
#123257=CARTESIAN_POINT('Ctrl Pts',(-21.7473058680115,-18.6252811563658,
-1.78235240076376));
#123258=CARTESIAN_POINT('Ctrl Pts',(-20.0903265808676,-16.2414409677205,
-1.9095282074452));
#123259=CARTESIAN_POINT('Ctrl Pts',(-17.1890026057441,-16.3443692494651,
-2.03670401412663));
#123260=CARTESIAN_POINT('Ctrl Pts',(-15.7051174484919,-18.8396375226619,
-2.16387982080806));
#123261=CARTESIAN_POINT('Ctrl Pts',(-17.000044245167,-21.4379910700896,
-2.2910556274895));
#123262=CARTESIAN_POINT('Ctrl Pts',(-19.8857677182557,-21.7556022772552,
-2.41823143417093));
#123263=CARTESIAN_POINT('Ctrl Pts',(-21.7148158522574,-19.5010823187472,
-2.54540724085237));
#123264=CARTESIAN_POINT('Ctrl Pts',(-20.8091504232289,-16.7428134580815,
-2.6725830475338));
#123265=CARTESIAN_POINT('Ctrl Pts',(-17.9996632942386,-16.0113361084815,
-2.79975885421524));
#123266=CARTESIAN_POINT('Ctrl Pts',(-15.8638845069282,-17.9777353733943,
-2.92693466089667));
#123267=CARTESIAN_POINT('Ctrl Pts',(-16.3612585490912,-20.837961957188,
-3.0541104675781));
#123268=CARTESIAN_POINT('Ctrl Pts',(-19.035475601424,-21.9679355045566,
-3.18128627425954));
#123269=CARTESIAN_POINT('Ctrl Pts',(-21.433107502224,-20.3309754148531,
-3.30846208094097));
#123270=CARTESIAN_POINT('Ctrl Pts',(-21.354475794674,-17.4288909717763,
-3.43563788762241));
#123271=CARTESIAN_POINT('Ctrl Pts',(-18.8717201908742,-15.9241645268262,
-3.56281369430384));
#123272=CARTESIAN_POINT('Ctrl Pts',(-16.2626148596744,-17.1972892000883,
-3.68998950098528));
#123273=CARTESIAN_POINT('Ctrl Pts',(-15.920852003341,-20.0802521225103,
-3.8171653076667));
#123274=CARTESIAN_POINT('Ctrl Pts',(-18.1599778302449,-21.9281137498178,
-3.94434111434815));
#123275=CARTESIAN_POINT('Ctrl Pts',(-20.9257333700864,-21.0455757300857,
-4.07151692102957));
#123276=CARTESIAN_POINT('Ctrl Pts',(-21.6807095771773,-18.2423119199819,
-4.19869272771102));
#123277=CARTESIAN_POINT('Ctrl Pts',(-19.7322626406366,-16.0901428750757,
-4.32586853439245));
#123278=CARTESIAN_POINT('Ctrl Pts',(-16.867971690476,-16.5635501154064,
-4.45304434107388));
#123279=CARTESIAN_POINT('Ctrl Pts',(-15.7156458955264,-19.2282118809307,
-4.58022014775532));
#123280=CARTESIAN_POINT('Ctrl Pts',(-17.3324726512467,-21.639466389345,
-4.70739595443675));
#123281=CARTESIAN_POINT('Ctrl Pts',(-20.2351137608509,-21.5851372885107,
-4.83457176111819));
#123282=CARTESIAN_POINT('Ctrl Pts',(-21.7605761645016,-19.1150681563997,
-4.96174756779962));
#123283=CARTESIAN_POINT('Ctrl Pts',(-20.5093427877246,-16.4953941119431,
-5.08892337448106));
#123284=CARTESIAN_POINT('Ctrl Pts',(-17.6293425934107,-16.1295034956214,
-5.21609918116249));
#123285=CARTESIAN_POINT('Ctrl Pts',(-15.7627970068714,-18.353078238177,
-5.34327498784392));
#123286=CARTESIAN_POINT('Ctrl Pts',(-16.6221457528718,-21.1261265239282,
-5.47045079452535));
#123287=CARTESIAN_POINT('Ctrl Pts',(-19.418989694155,-21.904548665486,-5.5976266012068));
#123288=CARTESIAN_POINT('Ctrl Pts',(-21.5873981063063,-19.9741906622979,
-5.72480240788822));
#123289=CARTESIAN_POINT('Ctrl Pts',(-21.1379908577814,-17.1060361707592,
-5.85197821456966));
#123290=CARTESIAN_POINT('Ctrl Pts',(-18.4830712057421,-15.9314389191122,
-5.97915402125109));
#123291=CARTESIAN_POINT('Ctrl Pts',(-16.0583631480371,-17.5280189820156,
-6.10632982793253));
#123292=CARTESIAN_POINT('Ctrl Pts',(-16.0883858332559,-20.43101324669,-6.23350563461397));
#123293=CARTESIAN_POINT('Ctrl Pts',(-18.5455953111282,-21.9771046554413,
-6.3606814412954));
#123294=CARTESIAN_POINT('Ctrl Pts',(-21.1756543973266,-20.7478503019954,
-6.48785724797683));
#123295=CARTESIAN_POINT('Ctrl Pts',(-21.5656471201409,-17.8710147595092,
-6.61503305465826));
#123296=CARTESIAN_POINT('Ctrl Pts',(-19.3577793620672,-15.9859160816625,
-6.74220886133971));
#123297=CARTESIAN_POINT('Ctrl Pts',(-16.5776327554104,-16.8220153029603,
-6.86938466802113));
#123298=CARTESIAN_POINT('Ctrl Pts',(-15.7758192564191,-19.6122432820323,
-6.99656047470258));
#123299=CARTESIAN_POINT('Ctrl Pts',(-17.6879529842593,-21.7967390291592,
-7.123736281384));
#123300=CARTESIAN_POINT('Ctrl Pts',(-20.5597699240417,-21.3713632814495,
-7.25091208806544));
#123301=CARTESIAN_POINT('Ctrl Pts',(-21.7565562785773,-18.7263718856303,
-7.37808789474687));
#123302=CARTESIAN_POINT('Ctrl Pts',(-20.1803348485183,-16.2883802806852,
-7.50526370142831));
#123303=CARTESIAN_POINT('Ctrl Pts',(-17.2771909646086,-16.2940944453266,
-7.63243950810973));
#123304=CARTESIAN_POINT('Ctrl Pts',(-15.7105789509042,-18.7382719881573,
-7.75961531479118));
#123305=CARTESIAN_POINT('Ctrl Pts',(-16.9177680950714,-21.3785317163971,
-7.8867911214726));
#123306=CARTESIAN_POINT('Ctrl Pts',(-19.7912372839452,-21.7925992023863,
-8.01396692815404));
#123307=CARTESIAN_POINT('Ctrl Pts',(-21.6947568843456,-19.6005932276563,
-8.14114273483548));
#123308=CARTESIAN_POINT('Ctrl Pts',(-20.8819658086561,-16.8135432227874,
-8.26831854151691));
#123309=CARTESIAN_POINT('Ctrl Pts',(-18.098549421318,-15.9883945834145,
-8.39549434819835));
#123310=CARTESIAN_POINT('Ctrl Pts',(-15.8981194994098,-17.8821699716618,
-8.52267015487978));
#123311=CARTESIAN_POINT('Ctrl Pts',(-16.2994339221984,-20.7574480097691,
-8.64984596156122));
#123312=CARTESIAN_POINT('Ctrl Pts',(-18.9343116151575,-21.9763395576547,
-8.77702176824265));
#123313=CARTESIAN_POINT('Ctrl Pts',(-21.3854158339506,-20.4205872730748,
-8.90419757492408));
#123314=CARTESIAN_POINT('Ctrl Pts',(-21.4040105905201,-17.5174973162549,
-9.03137338160553));
#123315=CARTESIAN_POINT('Ctrl Pts',(-18.9730363498343,-15.9304745364933,
-9.15854918828694));
#123316=CARTESIAN_POINT('Ctrl Pts',(-16.3227610944446,-17.1155138324785,
-9.28572499496839));
#123317=CARTESIAN_POINT('Ctrl Pts',(-15.884647876537,-19.985415201978,-9.41290080164982));
#123318=CARTESIAN_POINT('Ctrl Pts',(-18.060638381169,-21.9072222646439,
-9.54007660833126));
#123319=CARTESIAN_POINT('Ctrl Pts',(-20.8543963775427,-21.1177963212788,
-9.66725241501268));
#123320=CARTESIAN_POINT('Ctrl Pts',(-21.7028223041627,-18.3413866776205,
-9.79442822169412));
#123321=CARTESIAN_POINT('Ctrl Pts',(-19.8275380326068,-16.1251768583083,
-9.92160402837556));
#123322=CARTESIAN_POINT('Ctrl Pts',(-16.949000488759,-16.5024018190668,
-10.048779835057));
#123323=CARTESIAN_POINT('Ctrl Pts',(-15.7080892069104,-19.1269810716216,
-10.1759556417385));
#123324=CARTESIAN_POINT('Ctrl Pts',(-17.2432632685167,-21.5910260515137,
-10.3031314484199));
#123325=CARTESIAN_POINT('Ctrl Pts',(-20.1460957557023,-21.6339284255716,
-10.4303072551013));
#123326=CARTESIAN_POINT('Ctrl Pts',(-21.7534180315782,-19.2163279284187,
-10.5574830617828));
#123327=CARTESIAN_POINT('Ctrl Pts',(-20.5906116696995,-16.5562229629832,
-10.6846588684642));
#123328=CARTESIAN_POINT('Ctrl Pts',(-17.7244793351877,-16.0940947303175,
-10.8118346751456));
#123329=CARTESIAN_POINT('Ctrl Pts',(-15.7845195527222,-18.2539172009796,
-10.9390104818271));
#123330=CARTESIAN_POINT('Ctrl Pts',(-16.5505250152316,-21.0541873118379,
-11.0661862885085));
#123331=CARTESIAN_POINT('Ctrl Pts',(-19.3197332545243,-21.9258310405445,
-11.1933620951899));
#123332=CARTESIAN_POINT('Ctrl Pts',(-21.5515675874969,-20.0691693663223,
-11.3205379018714));
#123333=CARTESIAN_POINT('Ctrl Pts',(-21.1984585369079,-17.1875741378502,
-11.4477137085528));
#123334=CARTESIAN_POINT('Ctrl Pts',(-18.5843617402537,-15.9247301252809,
-11.5748895152342));
#123335=CARTESIAN_POINT('Ctrl Pts',(-16.1075487593188,-17.4392183292074,
-11.7020653219157));
#123336=CARTESIAN_POINT('Ctrl Pts',(-16.04034177576,-20.3415898222665,-11.8292411285971));
#123337=CARTESIAN_POINT('Ctrl Pts',(-18.4443990256569,-21.9690989010672,
-11.9564169352785));
#123338=CARTESIAN_POINT('Ctrl Pts',(-21.1141471948498,-20.828607000416,
-12.08359274196));
#123339=CARTESIAN_POINT('Ctrl Pts',(-21.6002580413636,-17.9664446522494,
-12.2107685486414));
#123340=CARTESIAN_POINT('Ctrl Pts',(-19.4567550349637,-16.0084681651805,
-12.3379443553228));
#123341=CARTESIAN_POINT('Ctrl Pts',(-16.6501691432213,-16.7509994403685,
-12.4651201620043));
#123342=CARTESIAN_POINT('Ctrl Pts',(-15.7553687254437,-19.5128121195169,
-12.5922959686857));
#123343=CARTESIAN_POINT('Ctrl Pts',(-17.5932776273647,-21.7601144869345,
-12.7194717753671));
#123344=CARTESIAN_POINT('Ctrl Pts',(-20.4777285049632,-21.4311461038309,
-12.8466475820486));
#123345=CARTESIAN_POINT('Ctrl Pts',(-21.7624167072548,-18.8277150436234,
-12.97382338873));
#123346=CARTESIAN_POINT('Ctrl Pts',(-20.2687205453794,-16.3383077168971,
-13.1009991954114));
#123347=CARTESIAN_POINT('Ctrl Pts',(-17.3670135386182,-16.2468008358791,
-13.2281750020929));
#123348=CARTESIAN_POINT('Ctrl Pts',(-15.7194317654263,-18.6371462843459,
-13.3553508087743));
#123349=CARTESIAN_POINT('Ctrl Pts',(-16.8375292422496,-21.3163504748999,
-13.4825266154557));
#123350=CARTESIAN_POINT('Ctrl Pts',(-19.6955209310585,-21.8264098528738,
-13.6097024221372));
#123351=CARTESIAN_POINT('Ctrl Pts',(-21.6713768443407,-19.699376596832,
-13.7368782288186));
#123352=CARTESIAN_POINT('Ctrl Pts',(-20.9523718171085,-16.8866717006199,
-13.8640540355001));
#123353=CARTESIAN_POINT('Ctrl Pts',(-18.1981483353623,-15.9687773303578,
-13.9912298421815));
#123354=CARTESIAN_POINT('Ctrl Pts',(-15.9355354972161,-17.7878045998115,
-14.1184056488629));
#123355=CARTESIAN_POINT('Ctrl Pts',(-16.240340148078,-20.6749088908223,
-14.2455814555443));
#123356=CARTESIAN_POINT('Ctrl Pts',(-18.8329229390928,-21.9813512102896,
-14.3727572622258));
#123357=CARTESIAN_POINT('Ctrl Pts',(-21.3347500733399,-20.5085518170573,
-14.4999330689072));
#123358=CARTESIAN_POINT('Ctrl Pts',(-21.450550436052,-17.6077127421763,
-14.6271088755887));
#123359=CARTESIAN_POINT('Ctrl Pts',(-19.0740843818219,-15.9401737904716,
-14.7542846822701));
#123360=CARTESIAN_POINT('Ctrl Pts',(-16.3856120152874,-17.0357984509923,
-14.8814604889515));
#123361=CARTESIAN_POINT('Ctrl Pts',(-15.85163986733,-19.8894190998463,-15.008636295633));
#123362=CARTESIAN_POINT('Ctrl Pts',(-17.9620542416513,-21.8830159073825,
-15.1358121023144));
#123363=CARTESIAN_POINT('Ctrl Pts',(-20.7806809369002,-21.1875875392591,
-15.2629879089958));
#123364=CARTESIAN_POINT('Ctrl Pts',(-21.7216049038886,-18.4411463600769,
-15.3901637156773));
#123365=CARTESIAN_POINT('Ctrl Pts',(-19.9215868032322,-16.1633816883713,
-15.5173395223587));
#123366=CARTESIAN_POINT('Ctrl Pts',(-17.0320315205603,-16.4440012364127,
-15.6445153290401));
#123367=CARTESIAN_POINT('Ctrl Pts',(-15.7039266816969,-19.0255539860864,
-15.7716911357216));
#123368=CARTESIAN_POINT('Ctrl Pts',(-17.1557260448163,-21.5396255188012,
-15.898866942403));
#123369=CARTESIAN_POINT('Ctrl Pts',(-20.0554938030874,-21.6797112441684,
-16.0260427490844));
#123370=CARTESIAN_POINT('Ctrl Pts',(-21.7428730181815,-19.3172912038646,
-16.1532185557659));
#123371=CARTESIAN_POINT('Ctrl Pts',(-20.6697979908152,-16.6197391565441,
-16.2803943624473));
#123372=CARTESIAN_POINT('Ctrl Pts',(-17.8207484560495,-16.0618916766609,
-16.4075701691287));
#123373=CARTESIAN_POINT('Ctrl Pts',(-15.8095505300749,-18.1555392030885,
-16.5347459758102));
#123374=CARTESIAN_POINT('Ctrl Pts',(-16.4813534809519,-20.9798900767501,
-16.6619217824916));
#123375=CARTESIAN_POINT('Ctrl Pts',(-19.2198197980441,-21.9437776700467,
-16.789097589173));
#123376=CARTESIAN_POINT('Ctrl Pts',(-21.5125766038083,-20.1628949417396,
-16.9162733958545));
#123377=CARTESIAN_POINT('Ctrl Pts',(-21.2561618334919,-17.2710912610025,
-17.0434492025359));
#123378=CARTESIAN_POINT('Ctrl Pts',(-18.6858201239648,-15.9214170193332,
-17.1706250092173));
#123379=CARTESIAN_POINT('Ctrl Pts',(-16.1596804603196,-17.3521145632324,
-17.2978008158988));
#123380=CARTESIAN_POINT('Ctrl Pts',(-15.9953191940406,-20.2506076952764,
-17.4249766225802));
#123381=CARTESIAN_POINT('Ctrl Pts',(-18.3435275855282,-21.9577088675884,
-17.5521524292616));
#123382=CARTESIAN_POINT('Ctrl Pts',(-21.0499701818423,-20.9072587092191,
-17.6793282359431));
#123383=CARTESIAN_POINT('Ctrl Pts',(-21.631653881637,-18.0629800421848,
-17.8065040426245));
#123384=CARTESIAN_POINT('Ctrl Pts',(-19.5549199937129,-16.0343220076414,
-17.933679849306));
#123385=CARTESIAN_POINT('Ctrl Pts',(-16.725042963598,-16.6824524395731,
-18.0608556559873));
#123386=CARTESIAN_POINT('Ctrl Pts',(-15.7382593244464,-19.4127518941776,
-18.1880314626688));
#123387=CARTESIAN_POINT('Ctrl Pts',(-17.4998818184781,-21.7203400833824,
-18.3152072693502));
#123388=CARTESIAN_POINT('Ctrl Pts',(-20.3937311460449,-21.4881480686078,
-18.4423830760317));
#123389=CARTESIAN_POINT('Ctrl Pts',(-21.7648801616449,-18.9291976120636,
-18.5695588827131));
#123390=CARTESIAN_POINT('Ctrl Pts',(-20.3553847465806,-16.3911669310282,
-18.6967346893946));
#123391=CARTESIAN_POINT('Ctrl Pts',(-17.4583694610031,-16.2025416478318,
-18.823910496076));
#123392=CARTESIAN_POINT('Ctrl Pts',(-15.7316660204183,-18.5363737515732,
-18.9510863027574));
#123393=CARTESIAN_POINT('Ctrl Pts',(-16.7594176601915,-21.2515171426226,
-19.0782621094388));
#123394=CARTESIAN_POINT('Ctrl Pts',(-19.5987260404249,-21.8569962774213,
-19.2054379161203));
#123395=CARTESIAN_POINT('Ctrl Pts',(-21.6447019493503,-19.7973216359904,
-19.3326137228017));
#123396=CARTESIAN_POINT('Ctrl Pts',(-21.0202894786101,-16.9621168526002,
-19.4597895294832));
#123397=CARTESIAN_POINT('Ctrl Pts',(-18.2983483137461,-15.9525063653534,
-19.5869653361646));
#123398=CARTESIAN_POINT('Ctrl Pts',(-15.9760905326363,-17.6947450904228,
-19.714141142846));
#123399=CARTESIAN_POINT('Ctrl Pts',(-16.184043510336,-20.5904372147467,
-19.8413169495275));
#123400=CARTESIAN_POINT('Ctrl Pts',(-18.7314233036429,-21.9829647838468,
-19.9684927562089));
#123401=CARTESIAN_POINT('Ctrl Pts',(-21.2811670472796,-20.5947704862203,
-20.0956685628903));
#123402=CARTESIAN_POINT('Ctrl Pts',(-21.49404313672,-17.6994358448221,-20.2228443695718));
#123403=CARTESIAN_POINT('Ctrl Pts',(-19.1747509237061,-15.9532518137242,
-20.3500201762532));
#123404=CARTESIAN_POINT('Ctrl Pts',(-16.4510971561478,-16.9582316928714,
-20.4771959829346));
#123405=CARTESIAN_POINT('Ctrl Pts',(-15.8218649356901,-19.7923729967134,
-20.6043717896161));
#123406=CARTESIAN_POINT('Ctrl Pts',(-17.8643361189216,-21.8555189367891,
-20.7315475962975));
#123407=CARTESIAN_POINT('Ctrl Pts',(-20.704669493102,-21.2548766742021,
-20.8587234029789));
#123408=CARTESIAN_POINT('Ctrl Pts',(-21.7370367735022,-18.5414683255483,
-20.9858992096604));
#123409=CARTESIAN_POINT('Ctrl Pts',(-20.0143025609789,-16.2047352065647,
-21.1130750163418));
#123410=CARTESIAN_POINT('Ctrl Pts',(-17.1169733783673,-16.3883740006192,
-21.2402508230232));
#123411=CARTESIAN_POINT('Ctrl Pts',(-15.7031596587772,-18.9241212228848,
-21.3674266297047));
#123412=CARTESIAN_POINT('Ctrl Pts',(-17.0699655881192,-21.4851744179203,
-21.4946024363861));
#123413=CARTESIAN_POINT('Ctrl Pts',(-19.963397156019,-21.7227196345909,
-21.6217782430676));
#123414=CARTESIAN_POINT('Ctrl Pts',(-21.7289768951727,-19.4172948235399,
-21.748954049749));
#123415=CARTESIAN_POINT('Ctrl Pts',(-20.7467658607354,-16.6869340105708,
-21.8761298564304));
#123416=CARTESIAN_POINT('Ctrl Pts',(-17.9181415113151,-16.0308544058051,
-22.0033056631118));
#123417=CARTESIAN_POINT('Ctrl Pts',(-15.8372814923396,-18.0626244799711,
-22.1305001261329));
#123418=CARTESIAN_POINT('Ctrl Pts',(-16.2233207480177,-19.9500078885456,
-22.2153026535935));
#123419=CARTESIAN_POINT('Ctrl Pts',(-16.7733104792501,-20.6030838137515,
-22.2577132454937));
#123420=CARTESIAN_POINT('Ctrl Pts',(-19.3578031896578,-21.2832305070458,
0.0847272843464291));
#123421=CARTESIAN_POINT('Ctrl Pts',(-20.1339758575579,-21.0755380525683,
0.042335348785951));
#123422=CARTESIAN_POINT('Ctrl Pts',(-21.4490186733577,-19.8273082723234,
-0.0424485223350051));
#123423=CARTESIAN_POINT('Ctrl Pts',(-20.9388617059771,-17.1376076759719,
-0.169624329016439));
#123424=CARTESIAN_POINT('Ctrl Pts',(-18.4021242480669,-16.1185824938284,
-0.296800135697873));
#123425=CARTESIAN_POINT('Ctrl Pts',(-16.1717639304198,-17.6960336866052,
-0.423975942379309));
#123426=CARTESIAN_POINT('Ctrl Pts',(-16.2911142199628,-20.4273016198123,
-0.551151749060742));
#123427=CARTESIAN_POINT('Ctrl Pts',(-18.6521697052435,-21.8042713584183,
-0.678327555742178));
#123428=CARTESIAN_POINT('Ctrl Pts',(-21.0880352243816,-20.5648744678046,
-0.80550336242361));
#123429=CARTESIAN_POINT('Ctrl Pts',(-21.3643566423075,-17.8455498248734,
-0.932679169105046));
#123430=CARTESIAN_POINT('Ctrl Pts',(-19.2274179378702,-16.1414364076047,
-1.05985497578648));
#123431=CARTESIAN_POINT('Ctrl Pts',(-16.6378358343089,-17.0157825839918,
-1.18703078246792));
#123432=CARTESIAN_POINT('Ctrl Pts',(-15.9713350808349,-19.6665181980038,
-1.31420658914935));
#123433=CARTESIAN_POINT('Ctrl Pts',(-17.8394178695693,-21.6617120734788,
-1.44138239583079));
#123434=CARTESIAN_POINT('Ctrl Pts',(-20.5282190751429,-21.1709214225929,
-1.56855820251222));
#123435=CARTESIAN_POINT('Ctrl Pts',(-21.5709383211685,-18.6444038752278,
-1.69573400919365));
#123436=CARTESIAN_POINT('Ctrl Pts',(-20.0109413467548,-16.4000888674147,
-1.82290981587509));
#123437=CARTESIAN_POINT('Ctrl Pts',(-17.2794306645736,-16.4969927993764,
-1.95008562255652));
#123438=CARTESIAN_POINT('Ctrl Pts',(-15.882396692181,-18.8462140520133,
-2.07726142923796));
#123439=CARTESIAN_POINT('Ctrl Pts',(-17.1015319587312,-21.2924870403926,
-2.20443723591939));
#123440=CARTESIAN_POINT('Ctrl Pts',(-19.8183552298129,-21.5915085948938,
-2.33161304260083));
#123441=CARTESIAN_POINT('Ctrl Pts',(-21.5403499326061,-19.4689447576054,
-2.45878884928226));
#123442=CARTESIAN_POINT('Ctrl Pts',(-20.6876927267632,-16.8721162331674,
-2.5859646559637));
#123443=CARTESIAN_POINT('Ctrl Pts',(-18.0426437180737,-16.1834519504684,
-2.71314046264513));
#123444=CARTESIAN_POINT('Ctrl Pts',(-16.0318711803166,-18.0347586792573,
-2.84031626932657));
#123445=CARTESIAN_POINT('Ctrl Pts',(-16.5001341253916,-20.7275773834348,
-2.967492076008));
#123446=CARTESIAN_POINT('Ctrl Pts',(-19.0178303590937,-21.7914140461736,
-3.09466788268943));
#123447=CARTESIAN_POINT('Ctrl Pts',(-21.2751298558503,-20.2502645538495,
-3.22184368937087));
#123448=CARTESIAN_POINT('Ctrl Pts',(-21.201100429639,-17.5180379135899,
-3.3490194960523));
#123449=CARTESIAN_POINT('Ctrl Pts',(-18.8636594850319,-16.1013824854533,
-3.47619530273374));
#123450=CARTESIAN_POINT('Ctrl Pts',(-16.40726401034,-17.2999916978614,-3.60337110941517));
#123451=CARTESIAN_POINT('Ctrl Pts',(-16.0855043927131,-20.0142159921659,
-3.73054691609661));
#123452=CARTESIAN_POINT('Ctrl Pts',(-18.1935751105569,-21.7539230422786,
-3.85772272277804));
#123453=CARTESIAN_POINT('Ctrl Pts',(-20.7974521219332,-20.9230396080263,
-3.98489852945948));
#123454=CARTESIAN_POINT('Ctrl Pts',(-21.5082398837079,-18.2838496699412,
-4.11207433614091));
#123455=CARTESIAN_POINT('Ctrl Pts',(-19.6738347409324,-16.2576461895902,
-4.23925014282234));
#123456=CARTESIAN_POINT('Ctrl Pts',(-16.9771895560713,-16.703345099837,
-4.36642594950377));
#123457=CARTESIAN_POINT('Ctrl Pts',(-15.8923089135627,-19.2120453137177,
-4.49360175618521));
#123458=CARTESIAN_POINT('Ctrl Pts',(-17.4145034676192,-21.482170092496,
-4.62077756286664));
#123459=CARTESIAN_POINT('Ctrl Pts',(-20.1472541929444,-21.4310208514753,
-4.74795336954808));
#123460=CARTESIAN_POINT('Ctrl Pts',(-21.5834319126906,-19.1055238446132,
-4.87512917622951));
#123461=CARTESIAN_POINT('Ctrl Pts',(-20.4054327082334,-16.6391782390827,
-5.00230498291095));
#123462=CARTESIAN_POINT('Ctrl Pts',(-17.6939977347856,-16.2947030492859,
-5.12948078959238));
#123463=CARTESIAN_POINT('Ctrl Pts',(-15.9367002898516,-18.3881328813199,
-5.25665659627382));
#123464=CARTESIAN_POINT('Ctrl Pts',(-16.7457517089779,-20.9988757972025,
-5.38383240295525));
#123465=CARTESIAN_POINT('Ctrl Pts',(-19.3788975305108,-21.7317372125915,
-5.51100820963669));
#123466=CARTESIAN_POINT('Ctrl Pts',(-21.4203898946547,-19.914362265377,
-5.63818401631812));
#123467=CARTESIAN_POINT('Ctrl Pts',(-20.9972862666143,-17.2140796706178,
-5.76535982299955));
#123468=CARTESIAN_POINT('Ctrl Pts',(-18.4977579643435,-16.1082311105657,
-5.89253562968099));
#123469=CARTESIAN_POINT('Ctrl Pts',(-16.2149670669532,-17.6113640023665,
-6.01971143636243));
#123470=CARTESIAN_POINT('Ctrl Pts',(-16.2432325368166,-20.3444472127417,
-6.14688724304385));
#123471=CARTESIAN_POINT('Ctrl Pts',(-18.5566225596869,-21.8000465304473,
-6.2740630497253));
#123472=CARTESIAN_POINT('Ctrl Pts',(-21.0327453747589,-20.6427399261711,
-6.40123885640672));
#123473=CARTESIAN_POINT('Ctrl Pts',(-21.3999119847184,-17.9342843787876,
-6.52841466308816));
#123474=CARTESIAN_POINT('Ctrl Pts',(-19.3212698138575,-16.1595197473112,
-6.6555904697696));
#123475=CARTESIAN_POINT('Ctrl Pts',(-16.7038440388577,-16.9466824268052,
-6.78276627645102));
#123476=CARTESIAN_POINT('Ctrl Pts',(-15.9489603525162,-19.57359951566,-6.90994208313247));
#123477=CARTESIAN_POINT('Ctrl Pts',(-17.7491776836857,-21.6302376297137,
-7.03711788981389));
#123478=CARTESIAN_POINT('Ctrl Pts',(-20.452908365107,-21.2297589486797,
-7.16429369649533));
#123479=CARTESIAN_POINT('Ctrl Pts',(-21.5796473090278,-18.7395778058964,
-7.29146950317678));
#123480=CARTESIAN_POINT('Ctrl Pts',(-20.0956814677067,-16.4442808417949,
-7.41864530985819));
#123481=CARTESIAN_POINT('Ctrl Pts',(-17.3624573952481,-16.4496605587419,
-7.54582111653964));
#123482=CARTESIAN_POINT('Ctrl Pts',(-15.8875385351148,-18.7507814003416,
-7.67299692322106));
#123483=CARTESIAN_POINT('Ctrl Pts',(-17.0240713976901,-21.236507818093,
-7.80017272990251));
#123484=CARTESIAN_POINT('Ctrl Pts',(-19.7293576227465,-21.6263401052905,
-7.92734853658393));
#123485=CARTESIAN_POINT('Ctrl Pts',(-21.5214650077943,-19.5626313341509,
-8.05452434326538));
#123486=CARTESIAN_POINT('Ctrl Pts',(-20.756246257781,-16.9387062139828,
-8.1817001499468));
#123487=CARTESIAN_POINT('Ctrl Pts',(-18.1357420810118,-16.1618531833802,
-8.30887595662825));
#123488=CARTESIAN_POINT('Ctrl Pts',(-16.06410241284,-17.9447866809843,-8.43605176330966));
#123489=CARTESIAN_POINT('Ctrl Pts',(-16.4419280683544,-20.6517758840762,
-8.56322756999113));
#123490=CARTESIAN_POINT('Ctrl Pts',(-18.9225874591253,-21.7993262135178,
-8.69040337667253));
#123491=CARTESIAN_POINT('Ctrl Pts',(-21.2302295612066,-20.3346314670524,
-8.81757918335398));
#123492=CARTESIAN_POINT('Ctrl Pts',(-21.2477359743606,-17.6014581653534,
-8.9447549900354));
#123493=CARTESIAN_POINT('Ctrl Pts',(-18.9590456510891,-16.1073231728629,
-9.07193079671685));
#123494=CARTESIAN_POINT('Ctrl Pts',(-16.4638899108517,-17.2230026087143,
-9.19910660339828));
#123495=CARTESIAN_POINT('Ctrl Pts',(-16.0514192784853,-19.9249298373897,
-9.3262824100797));
#123496=CARTESIAN_POINT('Ctrl Pts',(-18.1000499583713,-21.7342543270959,
-9.45345821676116));
#123497=CARTESIAN_POINT('Ctrl Pts',(-20.7302904540745,-20.9910331578707,
-9.58063402344258));
#123498=CARTESIAN_POINT('Ctrl Pts',(-21.5290583619236,-18.3771256229697,
-9.70780983012403));
#123499=CARTESIAN_POINT('Ctrl Pts',(-19.7635337035947,-16.2906296482662,
-9.83498563680543));
#123500=CARTESIAN_POINT('Ctrl Pts',(-17.0534757722859,-16.6457757880052,
-9.9621614434869));
#123501=CARTESIAN_POINT('Ctrl Pts',(-15.8851945148077,-19.1167395018316,
-10.0893372501683));
#123502=CARTESIAN_POINT('Ctrl Pts',(-17.3305154731838,-21.4365649476141,
-10.2165130568498));
#123503=CARTESIAN_POINT('Ctrl Pts',(-20.0634463748397,-21.4769562634529,
-10.3436888635312));
#123504=CARTESIAN_POINT('Ctrl Pts',(-21.5766927423282,-19.2008569240337,
-10.4708646702126));
#123505=CARTESIAN_POINT('Ctrl Pts',(-20.4819449561405,-16.6964468026162,
-10.598040476894));
#123506=CARTESIAN_POINT('Ctrl Pts',(-17.7835661623932,-16.2613667443784,
-10.7252162835755));
#123507=CARTESIAN_POINT('Ctrl Pts',(-15.9571514240733,-18.2947756986395,
-10.8523920902569));
#123508=CARTESIAN_POINT('Ctrl Pts',(-16.678322903506,-20.9311471574582,
-10.9795678969384));
#123509=CARTESIAN_POINT('Ctrl Pts',(-19.2854505292619,-21.7517739390354,
-11.1067437036198));
#123510=CARTESIAN_POINT('Ctrl Pts',(-21.3866565212999,-20.0037819051163,
-11.2339195103012));
#123511=CARTESIAN_POINT('Ctrl Pts',(-21.0542147974772,-17.2908452542003,
-11.3610953169827));
#123512=CARTESIAN_POINT('Ctrl Pts',(-18.5931200057406,-16.1019149796642,
-11.4882711236641));
#123513=CARTESIAN_POINT('Ctrl Pts',(-16.2612738647384,-17.5277608150597,
-11.6154469303455));
#123514=CARTESIAN_POINT('Ctrl Pts',(-16.198000478146,-20.2602577043845,
-11.742622737027));
#123515=CARTESIAN_POINT('Ctrl Pts',(-18.4613492509727,-21.7925093495675,
-11.8697985437084));
#123516=CARTESIAN_POINT('Ctrl Pts',(-20.9748381634178,-20.7187699684155,
-11.9969743503898));
#123517=CARTESIAN_POINT('Ctrl Pts',(-21.4324971430291,-18.0241287993538,
-12.1241501570713));
#123518=CARTESIAN_POINT('Ctrl Pts',(-19.4144524815328,-16.1807518667032,
-12.2513259637527));
#123519=CARTESIAN_POINT('Ctrl Pts',(-16.7721349018743,-16.879823093295,
-12.3785017704341));
#123520=CARTESIAN_POINT('Ctrl Pts',(-15.9297067826652,-19.4799880179848,
-12.5056775771156));
#123521=CARTESIAN_POINT('Ctrl Pts',(-17.6600436362941,-21.5957567068059,
-12.632853383797));
#123522=CARTESIAN_POINT('Ctrl Pts',(-20.3756687963737,-21.2860427071796,
-12.7600291904784));
#123523=CARTESIAN_POINT('Ctrl Pts',(-21.5851647292373,-18.8349893907445,
-12.8872049971599));
#123524=CARTESIAN_POINT('Ctrl Pts',(-20.1788939862666,-16.4912860458039,
-13.0143808038413));
#123525=CARTESIAN_POINT('Ctrl Pts',(-17.4470226911311,-16.4051350247055,
-13.1415566105228));
#123526=CARTESIAN_POINT('Ctrl Pts',(-15.8958731980624,-18.6555745421719,
-13.2687324172041));
#123527=CARTESIAN_POINT('Ctrl Pts',(-16.9485288917557,-21.1779660189567,
-13.3959082238856));
#123528=CARTESIAN_POINT('Ctrl Pts',(-19.6392435084281,-21.6581718323812,
-13.523084030567));
#123529=CARTESIAN_POINT('Ctrl Pts',(-21.4994533918664,-19.6556329535628,
-13.6502598372485));
#123530=CARTESIAN_POINT('Ctrl Pts',(-20.8225314316626,-17.0075545122368,
-13.7774356439299));
#123531=CARTESIAN_POINT('Ctrl Pts',(-18.2295115117883,-16.1433841200358,
-13.9046114506113));
#123532=CARTESIAN_POINT('Ctrl Pts',(-16.0993284677614,-17.8559444753405,
-14.0317872572928));
#123533=CARTESIAN_POINT('Ctrl Pts',(-16.3862930284057,-20.5740677456421,
-14.1589630639742));
#123534=CARTESIAN_POINT('Ctrl Pts',(-18.8271330203595,-21.8040445361958,
-14.2861388706557));
#123535=CARTESIAN_POINT('Ctrl Pts',(-21.1825292466206,-20.4174474826375,
-14.4133146773371));
#123536=CARTESIAN_POINT('Ctrl Pts',(-21.2915518619716,-17.686393319688,
-14.5404904840185));
#123537=CARTESIAN_POINT('Ctrl Pts',(-19.0541793835346,-16.1164547335152,
-14.6676662907));
#123538=CARTESIAN_POINT('Ctrl Pts',(-16.5230621932784,-17.1479529355545,
-14.7948420973814));
#123539=CARTESIAN_POINT('Ctrl Pts',(-16.0203432144126,-19.8345523474337,
-14.9220179040628));
#123540=CARTESIAN_POINT('Ctrl Pts',(-18.0072359077879,-21.7114647579188,
-15.0491937107442));
#123541=CARTESIAN_POINT('Ctrl Pts',(-20.6608895477009,-21.0567395247122,
-15.1763695174257));
#123542=CARTESIAN_POINT('Ctrl Pts',(-21.5467416238517,-18.4710464124499,
-15.3035453241071));
#123543=CARTESIAN_POINT('Ctrl Pts',(-19.8520778385523,-16.3265983654185,
-15.4307211307886));
#123544=CARTESIAN_POINT('Ctrl Pts',(-17.1316470321183,-16.5907933673128,
-15.55789693747));
#123545=CARTESIAN_POINT('Ctrl Pts',(-15.8812756204742,-19.0212489016859,
-15.6850727441514));
#123546=CARTESIAN_POINT('Ctrl Pts',(-17.2481017670014,-21.3881728668337,
-15.8122485508329));
#123547=CARTESIAN_POINT('Ctrl Pts',(-19.9781473170593,-21.5200594326025,
-15.9394243575143));
#123548=CARTESIAN_POINT('Ctrl Pts',(-21.5667649242067,-19.295910860703,
-16.0666001641957));
#123549=CARTESIAN_POINT('Ctrl Pts',(-20.5564965346144,-16.7562454196237,
-16.1937759708772));
#123550=CARTESIAN_POINT('Ctrl Pts',(-17.8742006914056,-16.2310485221405,
-16.3209517775586));
#123551=CARTESIAN_POINT('Ctrl Pts',(-15.9807173486685,-18.2021557242983,
-16.44812758424));
#123552=CARTESIAN_POINT('Ctrl Pts',(-16.6131999505341,-20.8611985088279,
-16.5753033909215));
#123553=CARTESIAN_POINT('Ctrl Pts',(-19.1913849660881,-21.7686701597314,
-16.7024791976029));
#123554=CARTESIAN_POINT('Ctrl Pts',(-21.349947663769,-20.0920217613478,
-16.8296550042843));
#123555=CARTESIAN_POINT('Ctrl Pts',(-21.1085407439649,-17.369474154658,
-16.9568308109658));
#123556=CARTESIAN_POINT('Ctrl Pts',(-18.688640072193,-16.0987957884381,
-17.0840066176472));
#123557=CARTESIAN_POINT('Ctrl Pts',(-16.3103543188293,-17.4457551965009,
-17.2111824243287));
#123558=CARTESIAN_POINT('Ctrl Pts',(-16.1556130495236,-20.174600723678,
-17.3383582310101));
#123559=CARTESIAN_POINT('Ctrl Pts',(-18.3663817745373,-21.7817859700398,
-17.4655340376915));
#123560=CARTESIAN_POINT('Ctrl Pts',(-20.9144174044528,-20.7928182252147,
-17.5927098443729));
#123561=CARTESIAN_POINT('Ctrl Pts',(-21.4620553977494,-18.1150140128212,
-17.7198856510544));
#123562=CARTESIAN_POINT('Ctrl Pts',(-19.506871885825,-16.2050924944522,
-17.8470614577358));
#123563=CARTESIAN_POINT('Ctrl Pts',(-16.8426263884951,-16.8152881201209,
-17.9742372644172));
#123564=CARTESIAN_POINT('Ctrl Pts',(-15.9135987878357,-19.3857842762726,
-18.1014130710987));
#123565=CARTESIAN_POINT('Ctrl Pts',(-17.5721142454945,-21.5583102826521,
-18.2285888777801));
#123566=CARTESIAN_POINT('Ctrl Pts',(-20.2965877681507,-21.339708370521,
-18.3557646844615));
#123567=CARTESIAN_POINT('Ctrl Pts',(-21.5874839986603,-18.9305322264037,
-18.482940491143));
#123568=CARTESIAN_POINT('Ctrl Pts',(-20.2604857675958,-16.5410514319824,
-18.6101162978244));
#123569=CARTESIAN_POINT('Ctrl Pts',(-17.5330315891426,-16.3634663086393,
-18.7372921045058));
#123570=CARTESIAN_POINT('Ctrl Pts',(-15.907391387167,-18.560700184086,-18.8644679111873));
#123571=CARTESIAN_POINT('Ctrl Pts',(-16.8749891483064,-21.1169273548174,
-18.9916437178687));
#123572=CARTESIAN_POINT('Ctrl Pts',(-19.5481139827311,-21.6869680461436,
-19.1188195245502));
#123573=CARTESIAN_POINT('Ctrl Pts',(-21.4743397674531,-19.7478453100669,
-19.2459953312316));
#123574=CARTESIAN_POINT('Ctrl Pts',(-20.8864739005117,-17.0785838906586,
-19.373171137913));
#123575=CARTESIAN_POINT('Ctrl Pts',(-18.323846826857,-16.1280654878871,
-19.5003469445945));
#123576=CARTESIAN_POINT('Ctrl Pts',(-16.1375098337227,-17.7683317005682,
-19.6275227512759));
#123577=CARTESIAN_POINT('Ctrl Pts',(-16.3332914095993,-20.4945401618491,
-19.7546985579573));
#123578=CARTESIAN_POINT('Ctrl Pts',(-18.7315741166155,-21.8055636679596,
-19.8818743646388));
#123579=CARTESIAN_POINT('Ctrl Pts',(-21.1320824129259,-20.4986198087347,
-20.0090501713202));
#123580=CARTESIAN_POINT('Ctrl Pts',(-21.3324989528482,-17.7727479070516,
-20.1362259780016));
#123581=CARTESIAN_POINT('Ctrl Pts',(-19.1489539543349,-16.1287673054729,
-20.2634017846831));
#123582=CARTESIAN_POINT('Ctrl Pts',(-16.5847145159137,-17.0749261277227,
-20.3905775913645));
#123583=CARTESIAN_POINT('Ctrl Pts',(-15.9923109972134,-19.7431863126012,
-20.5177533980459));
#123584=CARTESIAN_POINT('Ctrl Pts',(-17.9152371863878,-21.6855771736479,
-20.6449292047274));
#123585=CARTESIAN_POINT('Ctrl Pts',(-20.5893270222873,-21.1200902544022,
-20.7721050114088));
#123586=CARTESIAN_POINT('Ctrl Pts',(-21.5612702725159,-18.5654965747524,
-20.8992808180902));
#123587=CARTESIAN_POINT('Ctrl Pts',(-19.9393669813241,-16.3655314792863,
-21.0264566247717));
#123588=CARTESIAN_POINT('Ctrl Pts',(-17.2116172781004,-16.5384219706357,
-21.1536324314531));
#123589=CARTESIAN_POINT('Ctrl Pts',(-15.8805534910891,-18.9257529561851,
-21.2808082381345));
#123590=CARTESIAN_POINT('Ctrl Pts',(-17.1673608343839,-21.3369087663789,
-21.407984044816));
#123591=CARTESIAN_POINT('Ctrl Pts',(-19.8914410486737,-21.560550559712,
-21.5351598514974));
#123592=CARTESIAN_POINT('Ctrl Pts',(-21.5536821355334,-19.3900613098573,
-21.6623356581788));
#123593=CARTESIAN_POINT('Ctrl Pts',(-20.6289595069245,-16.8195073866206,
-21.7895114648603));
#123594=CARTESIAN_POINT('Ctrl Pts',(-17.965893371406,-16.2018278499181,
-21.9166872715417));
#123595=CARTESIAN_POINT('Ctrl Pts',(-16.006825229175,-18.1146792615168,
-22.0438817345628));
#123596=CARTESIAN_POINT('Ctrl Pts',(-16.3702697667955,-19.8915948993761,
-22.1286842620234));
#123597=CARTESIAN_POINT('Ctrl Pts',(-16.8880688264085,-20.506446560642,
-22.1710948539236));
#123598=CARTESIAN_POINT('Ctrl Pts',(-19.3190224246859,-21.138301940011,
0.171345675916539));
#123599=CARTESIAN_POINT('Ctrl Pts',(-20.0469417807877,-20.9435213660705,
0.128953740356061));
#123600=CARTESIAN_POINT('Ctrl Pts',(-21.2802306600689,-19.7728918715264,
0.0441698692351047));
#123601=CARTESIAN_POINT('Ctrl Pts',(-20.8017892686562,-17.2504053074226,
-0.0830059374463295));
#123602=CARTESIAN_POINT('Ctrl Pts',(-18.42275638934,-16.2947311576948,-0.210181744127763));
#123603=CARTESIAN_POINT('Ctrl Pts',(-16.3310537135823,-17.7741149391859,
-0.337357550809198));
#123604=CARTESIAN_POINT('Ctrl Pts',(-16.4429842021291,-20.3355846707344,
-0.464533357490632));
#123605=CARTESIAN_POINT('Ctrl Pts',(-18.6572569530825,-21.6269505831793,
-0.591709164172067));
#123606=CARTESIAN_POINT('Ctrl Pts',(-20.9416889275276,-20.4646048528009,
-0.718884970853501));
#123607=CARTESIAN_POINT('Ctrl Pts',(-21.2008319210033,-17.9143359178367,
-0.846060777534935));
#123608=CARTESIAN_POINT('Ctrl Pts',(-19.1967429984043,-16.3161642831945,
-0.973236584216371));
#123609=CARTESIAN_POINT('Ctrl Pts',(-16.7681507336229,-17.1361538706243,
-1.1004123908978));
#123610=CARTESIAN_POINT('Ctrl Pts',(-16.1430851787862,-19.6220978379218,
-1.22758819757924));
#123611=CARTESIAN_POINT('Ctrl Pts',(-17.8950324927765,-21.4932539623228,
-1.35476400426067));
#123612=CARTESIAN_POINT('Ctrl Pts',(-20.4166755796707,-21.0329749170169,
-1.48193981094211));
#123613=CARTESIAN_POINT('Ctrl Pts',(-21.3945707743255,-18.6635265940897,
-1.60911561762354));
#123614=CARTESIAN_POINT('Ctrl Pts',(-19.9315561126419,-16.558736767109,
-1.73629142430498));
#123615=CARTESIAN_POINT('Ctrl Pts',(-17.369858723403,-16.6496163492876,
-1.86346723098641));
#123616=CARTESIAN_POINT('Ctrl Pts',(-16.0596759358701,-18.8527905813645,
-1.99064303766784));
#123617=CARTESIAN_POINT('Ctrl Pts',(-17.2030196722955,-21.1469830106956,
-2.11781884434928));
#123618=CARTESIAN_POINT('Ctrl Pts',(-19.7509427413702,-21.4274149125326,
-2.24499465103071));
#123619=CARTESIAN_POINT('Ctrl Pts',(-21.3658840129548,-19.4368071964635,
-2.37217045771215));
#123620=CARTESIAN_POINT('Ctrl Pts',(-20.5662350302976,-17.0014190082534,
-2.49934626439358));
#123621=CARTESIAN_POINT('Ctrl Pts',(-18.0856241419088,-16.3555677924553,
-2.62652207107501));
#123622=CARTESIAN_POINT('Ctrl Pts',(-16.1998578537051,-18.0917819851203,
-2.75369787775646));
#123623=CARTESIAN_POINT('Ctrl Pts',(-16.639009701692,-20.6171928096815,
-2.88087368443788));
#123624=CARTESIAN_POINT('Ctrl Pts',(-19.0001851167635,-21.6148925877907,
-3.00804949111932));
#123625=CARTESIAN_POINT('Ctrl Pts',(-21.1171522094764,-20.169553692846,
-3.13522529780075));
#123626=CARTESIAN_POINT('Ctrl Pts',(-21.0477250646041,-17.6071848554035,
-3.26240110448218));
#123627=CARTESIAN_POINT('Ctrl Pts',(-18.8555987791894,-16.2786004440803,
-3.38957691116362));
#123628=CARTESIAN_POINT('Ctrl Pts',(-16.5519131610055,-17.4026941956347,
-3.51675271784505));
#123629=CARTESIAN_POINT('Ctrl Pts',(-16.2501567820852,-19.9481798618215,
-3.64392852452649));
#123630=CARTESIAN_POINT('Ctrl Pts',(-18.2271723908689,-21.5797323347394,
-3.77110433120793));
#123631=CARTESIAN_POINT('Ctrl Pts',(-20.6691708737799,-20.8005034859668,
-3.89828013788936));
#123632=CARTESIAN_POINT('Ctrl Pts',(-21.3357701902385,-18.3253874199006,
-4.02545594457079));
#123633=CARTESIAN_POINT('Ctrl Pts',(-19.6154068412282,-16.4251495041048,
-4.15263175125223));
#123634=CARTESIAN_POINT('Ctrl Pts',(-17.0864074216668,-16.8431400842676,
-4.27980755793366));
#123635=CARTESIAN_POINT('Ctrl Pts',(-16.068971931599,-19.1958787465047,
-4.4069833646151));
#123636=CARTESIAN_POINT('Ctrl Pts',(-17.4965342839917,-21.3248737956469,
-4.53415917129653));
#123637=CARTESIAN_POINT('Ctrl Pts',(-20.0593946250379,-21.2769044144401,
-4.66133497797797));
#123638=CARTESIAN_POINT('Ctrl Pts',(-21.4062876608796,-19.0959795328267,
-4.7885107846594));
#123639=CARTESIAN_POINT('Ctrl Pts',(-20.3015226287422,-16.7829623662223,
-4.91568659134084));
#123640=CARTESIAN_POINT('Ctrl Pts',(-17.7586528761605,-16.4599026029505,
-5.04286239802226));
#123641=CARTESIAN_POINT('Ctrl Pts',(-16.1106035728318,-18.4231875244628,
-5.17003820470371));
#123642=CARTESIAN_POINT('Ctrl Pts',(-16.8693576650841,-20.8716250704767,
-5.29721401138513));
#123643=CARTESIAN_POINT('Ctrl Pts',(-19.3388053668663,-21.5589257596971,
-5.42438981806658));
#123644=CARTESIAN_POINT('Ctrl Pts',(-21.2533816830032,-19.8545338684562,
-5.551565624748));
#123645=CARTESIAN_POINT('Ctrl Pts',(-20.8565816754472,-17.3221231704762,
-5.67874143142944));
#123646=CARTESIAN_POINT('Ctrl Pts',(-18.5124447229449,-16.2850233020193,
-5.80591723811088));
#123647=CARTESIAN_POINT('Ctrl Pts',(-16.3715709858693,-17.6947090227174,
-5.93309304479231));
#123648=CARTESIAN_POINT('Ctrl Pts',(-16.3980792403773,-20.2578811787933,
-6.06026885147374));
#123649=CARTESIAN_POINT('Ctrl Pts',(-18.5676498082457,-21.6229884054533,
-6.18744465815518));
#123650=CARTESIAN_POINT('Ctrl Pts',(-20.8898363521913,-20.5376295503469,
-6.31462046483661));
#123651=CARTESIAN_POINT('Ctrl Pts',(-21.2341768492959,-17.9975539980662,
-6.44179627151804));
#123652=CARTESIAN_POINT('Ctrl Pts',(-19.2847602656477,-16.33312341296,-6.56897207819949));
#123653=CARTESIAN_POINT('Ctrl Pts',(-16.830055322305,-17.0713495506502,
-6.6961478848809));
#123654=CARTESIAN_POINT('Ctrl Pts',(-16.1221014486134,-19.5349557492877,
-6.82332369156236));
#123655=CARTESIAN_POINT('Ctrl Pts',(-17.810402383112,-21.4637362302682,
-6.95049949824377));
#123656=CARTESIAN_POINT('Ctrl Pts',(-20.3460468061722,-21.0881546159098,
-7.07767530492523));
#123657=CARTESIAN_POINT('Ctrl Pts',(-21.4027383394782,-18.7527837261624,
-7.20485111160664));
#123658=CARTESIAN_POINT('Ctrl Pts',(-20.0110280868951,-16.6001814029045,
-7.3320269182881));
#123659=CARTESIAN_POINT('Ctrl Pts',(-17.4477238258878,-16.6052266721572,
-7.45920272496951));
#123660=CARTESIAN_POINT('Ctrl Pts',(-16.0644981193252,-18.7632908125259,
-7.58637853165096));
#123661=CARTESIAN_POINT('Ctrl Pts',(-17.130374700309,-21.0944839197888,
-7.71355433833239));
#123662=CARTESIAN_POINT('Ctrl Pts',(-19.6674779615479,-21.4600810081947,
-7.84073014501382));
#123663=CARTESIAN_POINT('Ctrl Pts',(-21.3481731312431,-19.5246694406454,
-7.96790595169526));
#123664=CARTESIAN_POINT('Ctrl Pts',(-20.630526706906,-17.0638692051782,
-8.09508175837669));
#123665=CARTESIAN_POINT('Ctrl Pts',(-18.1729347407055,-16.3353117833461,
-8.22225756505813));
#123666=CARTESIAN_POINT('Ctrl Pts',(-16.2300853262702,-18.0074033903068,
-8.34943337173957));
#123667=CARTESIAN_POINT('Ctrl Pts',(-16.5844222145103,-20.5461037583834,
-8.47660917842099));
#123668=CARTESIAN_POINT('Ctrl Pts',(-18.910863303093,-21.622312869381,-8.60378498510243));
#123669=CARTESIAN_POINT('Ctrl Pts',(-21.0750432884624,-20.2486756610299,
-8.73096079178387));
#123670=CARTESIAN_POINT('Ctrl Pts',(-21.091461358201,-17.685419014452,-8.8581365984653));
#123671=CARTESIAN_POINT('Ctrl Pts',(-18.9450549523438,-16.2841718092325,
-8.98531240514673));
#123672=CARTESIAN_POINT('Ctrl Pts',(-16.6050187272589,-17.3304913849503,
-9.11248821182817));
#123673=CARTESIAN_POINT('Ctrl Pts',(-16.2181906804335,-19.8644444728012,
-9.2396640185096));
#123674=CARTESIAN_POINT('Ctrl Pts',(-18.1394615355737,-21.561286389548,
-9.36683982519104));
#123675=CARTESIAN_POINT('Ctrl Pts',(-20.6061845306062,-20.8642699944625,
-9.49401563187247));
#123676=CARTESIAN_POINT('Ctrl Pts',(-21.3552944196844,-18.4128645683191,
-9.62119143855391));
#123677=CARTESIAN_POINT('Ctrl Pts',(-19.6995293745825,-16.4560824382241,
-9.74836724523534));
#123678=CARTESIAN_POINT('Ctrl Pts',(-17.1579510558127,-16.7891497569436,
-9.87554305191677));
#123679=CARTESIAN_POINT('Ctrl Pts',(-16.062299822705,-19.1064979320416,
-10.0027188585982));
#123680=CARTESIAN_POINT('Ctrl Pts',(-17.417767677851,-21.2821038437145,
-10.1298946652796));
#123681=CARTESIAN_POINT('Ctrl Pts',(-19.9807969939772,-21.3199841013343,
-10.257070471961));
#123682=CARTESIAN_POINT('Ctrl Pts',(-21.3999674530782,-19.1853859196488,
-10.3842462786425));
#123683=CARTESIAN_POINT('Ctrl Pts',(-20.3732782425814,-16.8366706422493,
-10.5114220853239));
#123684=CARTESIAN_POINT('Ctrl Pts',(-17.8426529895985,-16.4286387584391,
-10.6385978920053));
#123685=CARTESIAN_POINT('Ctrl Pts',(-16.1297832954242,-18.3356341962992,
-10.7657736986868));
#123686=CARTESIAN_POINT('Ctrl Pts',(-16.8061207917803,-20.8081070030786,
-10.8929495053682));
#123687=CARTESIAN_POINT('Ctrl Pts',(-19.2511678039994,-21.5777168375263,
-11.0201253120496));
#123688=CARTESIAN_POINT('Ctrl Pts',(-21.221745455103,-19.9383944439102,
-11.1473011187311));
#123689=CARTESIAN_POINT('Ctrl Pts',(-20.9099710580464,-17.3941163705504,
-11.2744769254125));
#123690=CARTESIAN_POINT('Ctrl Pts',(-18.6018782712276,-16.2790998340474,
-11.401652732094));
#123691=CARTESIAN_POINT('Ctrl Pts',(-16.414998970158,-17.6163033009118,
-11.5288285387754));
#123692=CARTESIAN_POINT('Ctrl Pts',(-16.3556591805319,-20.1789255865028,
-11.6560043454568));
#123693=CARTESIAN_POINT('Ctrl Pts',(-18.4782994762885,-21.6159197980676,
-11.7831801521383));
#123694=CARTESIAN_POINT('Ctrl Pts',(-20.8355291319859,-20.6089329364152,
-11.9103559588197));
#123695=CARTESIAN_POINT('Ctrl Pts',(-21.2647362446946,-18.0818129464581,
-12.0375317655011));
#123696=CARTESIAN_POINT('Ctrl Pts',(-19.372149928102,-16.3530355682261,
-12.1647075721826));
#123697=CARTESIAN_POINT('Ctrl Pts',(-16.8941006605274,-17.0086467462216,
-12.291883378864));
#123698=CARTESIAN_POINT('Ctrl Pts',(-16.1040448398867,-19.4471639164526,
-12.4190591855454));
#123699=CARTESIAN_POINT('Ctrl Pts',(-17.7268096452235,-21.4313989266772,
-12.5462349922269));
#123700=CARTESIAN_POINT('Ctrl Pts',(-20.2736090877839,-21.1409393105282,
-12.6734107989083));
#123701=CARTESIAN_POINT('Ctrl Pts',(-21.4079127512197,-18.8422637378655,
-12.8005866055897));
#123702=CARTESIAN_POINT('Ctrl Pts',(-20.0890674271536,-16.6442643747106,
-12.9277624122712));
#123703=CARTESIAN_POINT('Ctrl Pts',(-17.5270318436439,-16.563469213532,
-13.0549382189526));
#123704=CARTESIAN_POINT('Ctrl Pts',(-16.0723146306984,-18.6740027999979,
-13.182114025634));
#123705=CARTESIAN_POINT('Ctrl Pts',(-17.0595285412618,-21.0395815630135,
-13.3092898323155));
#123706=CARTESIAN_POINT('Ctrl Pts',(-19.5829660857976,-21.4899338118888,
-13.4364656389969));
#123707=CARTESIAN_POINT('Ctrl Pts',(-21.3275299393921,-19.6118893102937,
-13.5636414456783));
#123708=CARTESIAN_POINT('Ctrl Pts',(-20.6926910462166,-17.1284373238537,
-13.6908172523598));
#123709=CARTESIAN_POINT('Ctrl Pts',(-18.2608746882143,-16.3179909097138,
-13.8179930590412));
#123710=CARTESIAN_POINT('Ctrl Pts',(-16.2631214383067,-17.9240843508695,
-13.9451688657226));
#123711=CARTESIAN_POINT('Ctrl Pts',(-16.5322459087333,-20.4732266004621,
-14.0723446724041));
#123712=CARTESIAN_POINT('Ctrl Pts',(-18.8213431016262,-21.6267378621019,
-14.1995204790855));
#123713=CARTESIAN_POINT('Ctrl Pts',(-21.0303084199013,-20.3263431482177,
-14.326696285767));
#123714=CARTESIAN_POINT('Ctrl Pts',(-21.1325532878912,-17.7650738971998,
-14.4538720924484));
#123715=CARTESIAN_POINT('Ctrl Pts',(-19.0342743852475,-16.2927356765588,
-14.5810478991298));
#123716=CARTESIAN_POINT('Ctrl Pts',(-16.6605123712694,-17.2601074201168,
-14.7082237058113));
#123717=CARTESIAN_POINT('Ctrl Pts',(-16.1890465614952,-19.779685595021,
-14.8353995124927));
#123718=CARTESIAN_POINT('Ctrl Pts',(-18.0524175739244,-21.5399136084552,
-14.9625753191741));
#123719=CARTESIAN_POINT('Ctrl Pts',(-20.5410981585017,-20.9258915101652,
-15.0897511258555));
#123720=CARTESIAN_POINT('Ctrl Pts',(-21.3718783438148,-18.5009464648227,
-15.216926932537));
#123721=CARTESIAN_POINT('Ctrl Pts',(-19.7825688738725,-16.4898150424656,
-15.3441027392184));
#123722=CARTESIAN_POINT('Ctrl Pts',(-17.2312625436763,-16.7375854982129,
-15.4712785458999));
#123723=CARTESIAN_POINT('Ctrl Pts',(-16.0586245592516,-19.0169438172852,
-15.5984543525813));
#123724=CARTESIAN_POINT('Ctrl Pts',(-17.3404774891864,-21.2367202148663,
-15.7256301592627));
#123725=CARTESIAN_POINT('Ctrl Pts',(-19.9008008310311,-21.3604076210367,
-15.8528059659442));
#123726=CARTESIAN_POINT('Ctrl Pts',(-21.3906568302317,-19.2745305175414,
-15.9799817726256));
#123727=CARTESIAN_POINT('Ctrl Pts',(-20.4431950784137,-16.8927516827034,
-16.107157579307));
#123728=CARTESIAN_POINT('Ctrl Pts',(-17.9276529267619,-16.40020536762,-16.2343333859885));
#123729=CARTESIAN_POINT('Ctrl Pts',(-16.1518841672621,-18.2487722455082,
-16.3615091926699));
#123730=CARTESIAN_POINT('Ctrl Pts',(-16.7450464201164,-20.7425069409056,
-16.4886849993513));
#123731=CARTESIAN_POINT('Ctrl Pts',(-19.1629501341323,-21.5935626494162,
-16.6158608060327));
#123732=CARTESIAN_POINT('Ctrl Pts',(-21.1873187237296,-20.0211485809561,
-16.7430366127142));
#123733=CARTESIAN_POINT('Ctrl Pts',(-20.9609196544379,-17.4678570483134,
-16.8702124193956));
#123734=CARTESIAN_POINT('Ctrl Pts',(-18.6914600204213,-16.276174557543,
-16.9973882260771));
#123735=CARTESIAN_POINT('Ctrl Pts',(-16.4610281773391,-17.5393958297695,
-17.1245640327585));
#123736=CARTESIAN_POINT('Ctrl Pts',(-16.3159069050066,-20.0985937520796,
-17.2517398394399));
#123737=CARTESIAN_POINT('Ctrl Pts',(-18.3892359635466,-21.6058630724912,
-17.3789156461214));
#123738=CARTESIAN_POINT('Ctrl Pts',(-20.7788646270633,-20.6783777412105,
-17.5060914528028));
#123739=CARTESIAN_POINT('Ctrl Pts',(-21.2924569138617,-18.1670479834574,
-17.6332672594842));
#123740=CARTESIAN_POINT('Ctrl Pts',(-19.458823777937,-16.3758629812631,
-17.7604430661657));
#123741=CARTESIAN_POINT('Ctrl Pts',(-16.9602098133921,-16.9481238006687,
-17.8876188728471));
#123742=CARTESIAN_POINT('Ctrl Pts',(-16.0889382512251,-19.3588166583677,
-18.0147946795285));
#123743=CARTESIAN_POINT('Ctrl Pts',(-17.6443466725109,-21.3962804819219,
-18.14197048621));
#123744=CARTESIAN_POINT('Ctrl Pts',(-20.1994443902567,-21.1912686724342,
-18.2691462928914));
#123745=CARTESIAN_POINT('Ctrl Pts',(-21.4100878356756,-18.9318668407438,
-18.3963220995729));
#123746=CARTESIAN_POINT('Ctrl Pts',(-20.1655867886111,-16.6909359329365,
-18.5234979062543));
#123747=CARTESIAN_POINT('Ctrl Pts',(-17.607693717282,-16.5243909694468,
-18.6506737129357));
#123748=CARTESIAN_POINT('Ctrl Pts',(-16.0831167539157,-18.5850266165988,
-18.7778495196171));
#123749=CARTESIAN_POINT('Ctrl Pts',(-16.9905606364213,-20.9823375670122,
-18.9050253262986));
#123750=CARTESIAN_POINT('Ctrl Pts',(-19.4975019250372,-21.5169398148659,
-19.03220113298));
#123751=CARTESIAN_POINT('Ctrl Pts',(-21.3039775855559,-19.6983689841434,
-19.1593769396615));
#123752=CARTESIAN_POINT('Ctrl Pts',(-20.7526583224132,-17.1950509287168,
-19.2865527463429));
#123753=CARTESIAN_POINT('Ctrl Pts',(-18.3493453399679,-16.3036246104209,
-19.4137285530243));
#123754=CARTESIAN_POINT('Ctrl Pts',(-16.2989291348091,-17.8419183107137,
-19.5409043597057));
#123755=CARTESIAN_POINT('Ctrl Pts',(-16.4825393088626,-20.3986431089516,
-19.6680801663872));
#123756=CARTESIAN_POINT('Ctrl Pts',(-18.7317249295881,-21.6281625520724,
-19.7952559730686));
#123757=CARTESIAN_POINT('Ctrl Pts',(-20.9829977785724,-20.402469131249,
-19.9224317797501));
#123758=CARTESIAN_POINT('Ctrl Pts',(-21.1709547689763,-17.8460599692811,
-20.0496075864315));
#123759=CARTESIAN_POINT('Ctrl Pts',(-19.1231569849638,-16.3042827972216,
-20.1767833931129));
#123760=CARTESIAN_POINT('Ctrl Pts',(-16.7183318756798,-17.191620562574,
-20.3039591997943));
#123761=CARTESIAN_POINT('Ctrl Pts',(-16.1627570587368,-19.6939996284889,
-20.4311350064758));
#123762=CARTESIAN_POINT('Ctrl Pts',(-17.9661382538539,-21.5156354105067,
-20.5583108131572));
#123763=CARTESIAN_POINT('Ctrl Pts',(-20.4739845514727,-20.9853038346024,
-20.6854866198387));
#123764=CARTESIAN_POINT('Ctrl Pts',(-21.3855037715295,-18.5895248239564,
-20.8126624265201));
#123765=CARTESIAN_POINT('Ctrl Pts',(-19.8644314016694,-16.5263277520078,
-20.9398382332015));
#123766=CARTESIAN_POINT('Ctrl Pts',(-17.3062611778333,-16.6884699406521,
-21.067014039883));
#123767=CARTESIAN_POINT('Ctrl Pts',(-16.0579473234008,-18.9273846894854,
-21.1941898465644));
#123768=CARTESIAN_POINT('Ctrl Pts',(-17.2647560806485,-21.1886431148375,
-21.3213656532458));
#123769=CARTESIAN_POINT('Ctrl Pts',(-19.8194849413283,-21.3983814848332,
-21.4485414599273));
#123770=CARTESIAN_POINT('Ctrl Pts',(-21.3783873758939,-19.3628277961746,
-21.5757172666087));
#123771=CARTESIAN_POINT('Ctrl Pts',(-20.5111531531137,-16.9520807626706,
-21.7028930732902));
#123772=CARTESIAN_POINT('Ctrl Pts',(-18.0136452314969,-16.3728012940309,
-21.8300688799716));
#123773=CARTESIAN_POINT('Ctrl Pts',(-16.1763689660104,-18.1667340430625,
-21.9572633429927));
#123774=CARTESIAN_POINT('Ctrl Pts',(-16.5172187855734,-19.8331819102064,
-22.0420658704533));
#123775=CARTESIAN_POINT('Ctrl Pts',(-17.0028271735668,-20.4098093075325,
-22.0844764623534));
#123776=CARTESIAN_POINT('Ctrl Pts',(-19.2802416597141,-20.9933733729761,
0.257964067486649));
#123777=CARTESIAN_POINT('Ctrl Pts',(-19.9599077040175,-20.8115046795727,
0.215572131926171));
#123778=CARTESIAN_POINT('Ctrl Pts',(-21.1114426467799,-19.7184754707294,
0.130788260805215));
#123779=CARTESIAN_POINT('Ctrl Pts',(-20.6647168313355,-17.3632029388733,
0.00361245412378029));
#123780=CARTESIAN_POINT('Ctrl Pts',(-18.4433885306129,-16.4708798215613,
-0.123563352557654));
#123781=CARTESIAN_POINT('Ctrl Pts',(-16.4903434967449,-17.8521961917666,
-0.250739159239088));
#123782=CARTESIAN_POINT('Ctrl Pts',(-16.5948541842955,-20.2438677216565,
-0.377914965920522));
#123783=CARTESIAN_POINT('Ctrl Pts',(-18.6623442009214,-21.4496298079404,
-0.505090772601956));
#123784=CARTESIAN_POINT('Ctrl Pts',(-20.7953426306735,-20.3643352377974,
-0.632266579283392));
#123785=CARTESIAN_POINT('Ctrl Pts',(-21.0373071996992,-17.9831220108,-0.759442385964825));
#123786=CARTESIAN_POINT('Ctrl Pts',(-19.1660680589383,-16.4908921587843,
-0.886618192646261));
#123787=CARTESIAN_POINT('Ctrl Pts',(-16.8984656329369,-17.2565251572569,
-1.0137939993277));
#123788=CARTESIAN_POINT('Ctrl Pts',(-16.3148352767375,-19.5776774778398,
-1.14096980600913));
#123789=CARTESIAN_POINT('Ctrl Pts',(-17.9506471159836,-21.3247958511667,
-1.26814561269057));
#123790=CARTESIAN_POINT('Ctrl Pts',(-20.3051320841986,-20.8950284114407,
-1.395321419372));
#123791=CARTESIAN_POINT('Ctrl Pts',(-21.2182032274825,-18.6826493129518,
-1.52249722605343));
#123792=CARTESIAN_POINT('Ctrl Pts',(-19.8521708785292,-16.7173846668031,
-1.64967303273487));
#123793=CARTESIAN_POINT('Ctrl Pts',(-17.4602867822325,-16.8022398991988,
-1.7768488394163));
#123794=CARTESIAN_POINT('Ctrl Pts',(-16.2369551795592,-18.8593671107158,
-1.90402464609774));
#123795=CARTESIAN_POINT('Ctrl Pts',(-17.3045073858597,-21.0014789809986,
-2.03120045277917));
#123796=CARTESIAN_POINT('Ctrl Pts',(-19.6835302529274,-21.2633212301712,
-2.15837625946061));
#123797=CARTESIAN_POINT('Ctrl Pts',(-21.1914180933035,-19.4046696353217,
-2.28555206614204));
#123798=CARTESIAN_POINT('Ctrl Pts',(-20.4447773338319,-17.1307217833394,
-2.41272787282348));
#123799=CARTESIAN_POINT('Ctrl Pts',(-18.1286045657439,-16.5276836344422,
-2.53990367950491));
#123800=CARTESIAN_POINT('Ctrl Pts',(-16.3678445270935,-18.1488052909833,
-2.66707948618633));
#123801=CARTESIAN_POINT('Ctrl Pts',(-16.7778852779924,-20.5068082359283,
-2.79425529286778));
#123802=CARTESIAN_POINT('Ctrl Pts',(-18.9825398744333,-21.4383711294077,
-2.92143109954921));
#123803=CARTESIAN_POINT('Ctrl Pts',(-20.9591745631026,-20.0888428318423,
-3.04860690623065));
#123804=CARTESIAN_POINT('Ctrl Pts',(-20.8943496995691,-17.6963317972172,
-3.17578271291207));
#123805=CARTESIAN_POINT('Ctrl Pts',(-18.847538073347,-16.4558184027074,
-3.30295851959352));
#123806=CARTESIAN_POINT('Ctrl Pts',(-16.6965623116711,-17.5053966934078,
-3.43013432627495));
#123807=CARTESIAN_POINT('Ctrl Pts',(-16.4148091714573,-19.8821437314771,
-3.55731013295638));
#123808=CARTESIAN_POINT('Ctrl Pts',(-18.2607696711808,-21.4055416272001,
-3.68448593963782));
#123809=CARTESIAN_POINT('Ctrl Pts',(-20.5408896256266,-20.6779673639072,
-3.81166174631925));
#123810=CARTESIAN_POINT('Ctrl Pts',(-21.163300496769,-18.3669251698599,
-3.93883755300069));
#123811=CARTESIAN_POINT('Ctrl Pts',(-19.5569789415241,-16.5926528186193,
-4.06601335968212));
#123812=CARTESIAN_POINT('Ctrl Pts',(-17.1956252872621,-16.9829350686982,
-4.19318916636356));
#123813=CARTESIAN_POINT('Ctrl Pts',(-16.2456349496354,-19.1797121792916,
-4.32036497304499));
#123814=CARTESIAN_POINT('Ctrl Pts',(-17.5785651003642,-21.1675774987978,
-4.44754077972642));
#123815=CARTESIAN_POINT('Ctrl Pts',(-19.9715350571314,-21.1227879774049,
-4.57471658640786));
#123816=CARTESIAN_POINT('Ctrl Pts',(-21.2291434090686,-19.0864352210401,
-4.70189239308929));
#123817=CARTESIAN_POINT('Ctrl Pts',(-20.197612549251,-16.9267464933619,
-4.82906819977073));
#123818=CARTESIAN_POINT('Ctrl Pts',(-17.8233080175354,-16.6251021566151,
-4.95624400645216));
#123819=CARTESIAN_POINT('Ctrl Pts',(-16.284506855812,-18.4582421676058,
-5.0834198131336));
#123820=CARTESIAN_POINT('Ctrl Pts',(-16.9929636211903,-20.7443743437509,
-5.21059561981502));
#123821=CARTESIAN_POINT('Ctrl Pts',(-19.298713203222,-21.3861143068026,
-5.33777142649647));
#123822=CARTESIAN_POINT('Ctrl Pts',(-21.0863734713516,-19.7947054715354,
-5.4649472331779));
#123823=CARTESIAN_POINT('Ctrl Pts',(-20.7158770842802,-17.4301666703347,
-5.59212303985933));
#123824=CARTESIAN_POINT('Ctrl Pts',(-18.5271314815462,-16.4618154934729,
-5.71929884654077));
#123825=CARTESIAN_POINT('Ctrl Pts',(-16.5281749047854,-17.7780540430683,
-5.8464746532222));
#123826=CARTESIAN_POINT('Ctrl Pts',(-16.552925943938,-20.171315144845,-5.97365045990364));
#123827=CARTESIAN_POINT('Ctrl Pts',(-18.5786770568045,-21.4459302804593,
-6.10082626658507));
#123828=CARTESIAN_POINT('Ctrl Pts',(-20.7469273296236,-20.4325191745226,
-6.22800207326651));
#123829=CARTESIAN_POINT('Ctrl Pts',(-21.0684417138734,-18.0608236173447,
-6.35517787994794));
#123830=CARTESIAN_POINT('Ctrl Pts',(-19.2482507174378,-16.5067270786087,
-6.48235368662938));
#123831=CARTESIAN_POINT('Ctrl Pts',(-16.9562666057522,-17.1960166744951,
-6.6095294933108));
#123832=CARTESIAN_POINT('Ctrl Pts',(-16.2952425447106,-19.4963119829154,
-6.73670529999224));
#123833=CARTESIAN_POINT('Ctrl Pts',(-17.8716270825383,-21.2972348308226,
-6.86388110667369));
#123834=CARTESIAN_POINT('Ctrl Pts',(-20.2391852472374,-20.94655028314,-6.9910569133551));
#123835=CARTESIAN_POINT('Ctrl Pts',(-21.2258293699287,-18.7659896464285,
-7.11823272003656));
#123836=CARTESIAN_POINT('Ctrl Pts',(-19.9263747060834,-16.7560819640143,
-7.24540852671797));
#123837=CARTESIAN_POINT('Ctrl Pts',(-17.5329902565274,-16.7607927855726,
-7.37258433339943));
#123838=CARTESIAN_POINT('Ctrl Pts',(-16.2414577035358,-18.7758002247102,
-7.49976014008084));
#123839=CARTESIAN_POINT('Ctrl Pts',(-17.2366780029277,-20.9524600214847,
-7.62693594676229));
#123840=CARTESIAN_POINT('Ctrl Pts',(-19.6055983003493,-21.293821911099,
-7.75411175344372));
#123841=CARTESIAN_POINT('Ctrl Pts',(-21.1748812546918,-19.48670754714,-7.88128756012516));
#123842=CARTESIAN_POINT('Ctrl Pts',(-20.5048071560311,-17.1890321963735,
-8.00846336680658));
#123843=CARTESIAN_POINT('Ctrl Pts',(-18.2101274003992,-16.5087703833118,
-8.13563917348801));
#123844=CARTESIAN_POINT('Ctrl Pts',(-16.3960682397005,-18.0700200996293,
-8.26281498016946));
#123845=CARTESIAN_POINT('Ctrl Pts',(-16.7269163606663,-20.4404316326905,
-8.38999078685089));
#123846=CARTESIAN_POINT('Ctrl Pts',(-18.8991391470608,-21.4452995252443,
-8.51716659353233));
#123847=CARTESIAN_POINT('Ctrl Pts',(-20.9198570157183,-20.1627198550076,
-8.64434240021374));
#123848=CARTESIAN_POINT('Ctrl Pts',(-20.9351867420414,-17.7693798635505,
-8.77151820689519));
#123849=CARTESIAN_POINT('Ctrl Pts',(-18.9310642535986,-16.4610204456021,
-8.89869401357662));
#123850=CARTESIAN_POINT('Ctrl Pts',(-16.7461475436661,-17.4379801611861,
-9.02586982025806));
#123851=CARTESIAN_POINT('Ctrl Pts',(-16.3849620823817,-19.8039591082128,
-9.15304562693949));
#123852=CARTESIAN_POINT('Ctrl Pts',(-18.1788731127761,-21.3883184520001,
-9.28022143362092));
#123853=CARTESIAN_POINT('Ctrl Pts',(-20.4820786071378,-20.7375068310543,
-9.40739724030236));
#123854=CARTESIAN_POINT('Ctrl Pts',(-21.1815304774453,-18.4486035136685,
-9.53457304698381));
#123855=CARTESIAN_POINT('Ctrl Pts',(-19.6355250455705,-16.6215352281822,
-9.66174885366522));
#123856=CARTESIAN_POINT('Ctrl Pts',(-17.2624263393396,-16.932523725882,
-9.78892466034668));
#123857=CARTESIAN_POINT('Ctrl Pts',(-16.2394051306023,-19.0962563622516,
-9.91610046702808));
#123858=CARTESIAN_POINT('Ctrl Pts',(-17.5050198825181,-21.1276427398149,
-10.0432762737096));
#123859=CARTESIAN_POINT('Ctrl Pts',(-19.8981476131147,-21.1630119392157,
-10.170452080391));
#123860=CARTESIAN_POINT('Ctrl Pts',(-21.2232421638282,-19.1699149152638,
-10.2976278870724));
#123861=CARTESIAN_POINT('Ctrl Pts',(-20.2646115290223,-16.9768944818824,
-10.4248036937539));
#123862=CARTESIAN_POINT('Ctrl Pts',(-17.901739816804,-16.5959107725,-10.5519795004353));
#123863=CARTESIAN_POINT('Ctrl Pts',(-16.3024151667752,-18.3764926939591,
-10.6791553071167));
#123864=CARTESIAN_POINT('Ctrl Pts',(-16.9339186800547,-20.6850668486988,
-10.8063311137982));
#123865=CARTESIAN_POINT('Ctrl Pts',(-19.2168850787369,-21.4036597360172,
-10.9335069204796));
#123866=CARTESIAN_POINT('Ctrl Pts',(-21.0568343889061,-19.8730069827043,
-11.0606827271611));
#123867=CARTESIAN_POINT('Ctrl Pts',(-20.7657273186155,-17.4973874869004,
-11.1878585338425));
#123868=CARTESIAN_POINT('Ctrl Pts',(-18.6106365367144,-16.4562846884308,
-11.3150343405239));
#123869=CARTESIAN_POINT('Ctrl Pts',(-16.5687240755777,-17.7048457867641,
-11.4422101472054));
#123870=CARTESIAN_POINT('Ctrl Pts',(-16.5133178829179,-20.0975934686209,
-11.5693859538868));
#123871=CARTESIAN_POINT('Ctrl Pts',(-18.4952497016042,-21.4393302465677,
-11.6965617605682));
#123872=CARTESIAN_POINT('Ctrl Pts',(-20.6962201005539,-20.4990959044147,
-11.8237375672497));
#123873=CARTESIAN_POINT('Ctrl Pts',(-21.09697534636,-18.1394970935624,-11.9509133739311));
#123874=CARTESIAN_POINT('Ctrl Pts',(-19.3298473746713,-16.5253192697488,
-12.0780891806125));
#123875=CARTESIAN_POINT('Ctrl Pts',(-17.0160664191804,-17.1374703991481,
-12.205264987294));
#123876=CARTESIAN_POINT('Ctrl Pts',(-16.2783828971083,-19.4143398149205,
-12.3324407939754));
#123877=CARTESIAN_POINT('Ctrl Pts',(-17.7935756541529,-21.2670411465485,
-12.4596166006568));
#123878=CARTESIAN_POINT('Ctrl Pts',(-20.1715493791944,-20.9958359138768,
-12.5867924073383));
#123879=CARTESIAN_POINT('Ctrl Pts',(-21.2306607732021,-18.8495380849864,
-12.7139682140197));
#123880=CARTESIAN_POINT('Ctrl Pts',(-19.9992408680408,-16.7972427036174,
-12.8411440207011));
#123881=CARTESIAN_POINT('Ctrl Pts',(-17.6070409961567,-16.7218034023586,
-12.9683198273826));
#123882=CARTESIAN_POINT('Ctrl Pts',(-16.2487560633345,-18.6924310578239,
-13.095495634064));
#123883=CARTESIAN_POINT('Ctrl Pts',(-17.1705281907678,-20.9011971070702,
-13.2226714407454));
#123884=CARTESIAN_POINT('Ctrl Pts',(-19.526688663167,-21.3216957913963,
-13.3498472474269));
#123885=CARTESIAN_POINT('Ctrl Pts',(-21.1556064869176,-19.5681456670245,
-13.4770230541083));
#123886=CARTESIAN_POINT('Ctrl Pts',(-20.5628506607707,-17.2493201354707,
-13.6041988607897));
#123887=CARTESIAN_POINT('Ctrl Pts',(-18.2922378646403,-16.4925976993917,
-13.7313746674712));
#123888=CARTESIAN_POINT('Ctrl Pts',(-16.426914408852,-17.9922242263985,
-13.8585504741526));
#123889=CARTESIAN_POINT('Ctrl Pts',(-16.6781987890609,-20.3723854552819,
-13.985726280834));
#123890=CARTESIAN_POINT('Ctrl Pts',(-18.8155531828929,-21.449431188008,
-14.1129020875155));
#123891=CARTESIAN_POINT('Ctrl Pts',(-20.878087593182,-20.2352388137978,
-14.2400778941968));
#123892=CARTESIAN_POINT('Ctrl Pts',(-20.973554713811,-17.8437544747116,
-14.3672537008784));
#123893=CARTESIAN_POINT('Ctrl Pts',(-19.0143693869603,-16.4690166196025,
-14.4944295075598));
#123894=CARTESIAN_POINT('Ctrl Pts',(-16.7979625492603,-17.372261904679,
-14.6216053142412));
#123895=CARTESIAN_POINT('Ctrl Pts',(-16.3577499085777,-19.7248188426085,
-14.7487811209226));
#123896=CARTESIAN_POINT('Ctrl Pts',(-18.097599240061,-21.3683624589916,
-14.8759569276041));
#123897=CARTESIAN_POINT('Ctrl Pts',(-20.4213067693024,-20.7950434956184,
-15.0031327342855));
#123898=CARTESIAN_POINT('Ctrl Pts',(-21.1970150637779,-18.5308465171956,
-15.130308540967));
#123899=CARTESIAN_POINT('Ctrl Pts',(-19.7130599091926,-16.6530317195128,
-15.2574843476484));
#123900=CARTESIAN_POINT('Ctrl Pts',(-17.3308780552345,-16.884377629113,
-15.3846601543298));
#123901=CARTESIAN_POINT('Ctrl Pts',(-16.2359734980291,-19.0126387328847,
-15.5118359610112));
#123902=CARTESIAN_POINT('Ctrl Pts',(-17.4328532113714,-21.0852675628988,
-15.6390117676927));
#123903=CARTESIAN_POINT('Ctrl Pts',(-19.823454345003,-21.2007558094709,
-15.7661875743741));
#123904=CARTESIAN_POINT('Ctrl Pts',(-21.2145487362569,-19.2531501743798,
-15.8933633810556));
#123905=CARTESIAN_POINT('Ctrl Pts',(-20.3298936222131,-17.0292579457831,
-16.020539187737));
#123906=CARTESIAN_POINT('Ctrl Pts',(-17.9811051621181,-16.5693622130996,
-16.1477149944184));
#123907=CARTESIAN_POINT('Ctrl Pts',(-16.3230509858558,-18.295388766718,
-16.2748908010999));
#123908=CARTESIAN_POINT('Ctrl Pts',(-16.8768928896987,-20.6238153729833,
-16.4020666077813));
#123909=CARTESIAN_POINT('Ctrl Pts',(-19.1345153021762,-21.418455139101,
-16.5292424144627));
#123910=CARTESIAN_POINT('Ctrl Pts',(-21.0246897836904,-19.9502754005642,
-16.6564182211442));
#123911=CARTESIAN_POINT('Ctrl Pts',(-20.8132985649108,-17.5662399419689,
-16.7835940278256));
#123912=CARTESIAN_POINT('Ctrl Pts',(-18.6942799686495,-16.4535533266478,
-16.910769834507));
#123913=CARTESIAN_POINT('Ctrl Pts',(-16.6117020358488,-17.6330364630381,
-17.0379456411885));
#123914=CARTESIAN_POINT('Ctrl Pts',(-16.4762007604896,-20.0225867804811,
-17.1651214478699));
#123915=CARTESIAN_POINT('Ctrl Pts',(-18.4120901525558,-21.4299401749425,
-17.2922972545513));
#123916=CARTESIAN_POINT('Ctrl Pts',(-20.6433118496738,-20.563937257206,
-17.4194730612328));
#123917=CARTESIAN_POINT('Ctrl Pts',(-21.1228584299742,-18.2190819540937,
-17.5466488679142));
#123918=CARTESIAN_POINT('Ctrl Pts',(-19.4107756700491,-16.5466334680738,
-17.6738246745956));
#123919=CARTESIAN_POINT('Ctrl Pts',(-17.0777932382892,-17.0809594812165,
-17.8010004812771));
#123920=CARTESIAN_POINT('Ctrl Pts',(-16.2642777146144,-19.3318490404626,
-17.9281762879585));
#123921=CARTESIAN_POINT('Ctrl Pts',(-17.7165790995274,-21.2342506811916,
-18.05535209464));
#123922=CARTESIAN_POINT('Ctrl Pts',(-20.1023010123624,-21.0428289743473,
-18.1825279013214));
#123923=CARTESIAN_POINT('Ctrl Pts',(-21.2326916726909,-18.9332014550839,
-18.3097037080028));
#123924=CARTESIAN_POINT('Ctrl Pts',(-20.0706878096263,-16.8408204338905,
-18.4368795146842));
#123925=CARTESIAN_POINT('Ctrl Pts',(-17.6823558454215,-16.6853156302542,
-18.5640553213657));
#123926=CARTESIAN_POINT('Ctrl Pts',(-16.2588421206643,-18.6093530491115,
-18.6912311280471));
#123927=CARTESIAN_POINT('Ctrl Pts',(-17.1061321245363,-20.8477477792071,
-18.8184069347286));
#123928=CARTESIAN_POINT('Ctrl Pts',(-19.4468898673433,-21.3469115835881,
-18.94558274141));
#123929=CARTESIAN_POINT('Ctrl Pts',(-21.1336154036588,-19.6488926582199,
-19.0727585480914));
#123930=CARTESIAN_POINT('Ctrl Pts',(-20.6188427443147,-17.3115179667752,
-19.1999343547728));
#123931=CARTESIAN_POINT('Ctrl Pts',(-18.3748438530787,-16.4791837329545,
-19.3271101614543));
#123932=CARTESIAN_POINT('Ctrl Pts',(-16.4603484358955,-17.9155049208591,
-19.4542859681357));
#123933=CARTESIAN_POINT('Ctrl Pts',(-16.6317872081259,-20.302746056054,
-19.5814617748171));
#123934=CARTESIAN_POINT('Ctrl Pts',(-18.7318757425608,-21.4507614361853,
-19.7086375814986));
#123935=CARTESIAN_POINT('Ctrl Pts',(-20.8339131442188,-20.3063184537634,
-19.83581338818));
#123936=CARTESIAN_POINT('Ctrl Pts',(-21.0094105851045,-17.9193720315106,
-19.9629891948615));
#123937=CARTESIAN_POINT('Ctrl Pts',(-19.0973600155928,-16.4797982889704,
-20.0901650015429));
#123938=CARTESIAN_POINT('Ctrl Pts',(-16.8519492354458,-17.3083149974252,
-20.2173408082243));
#123939=CARTESIAN_POINT('Ctrl Pts',(-16.3332031202602,-19.6448129443766,
-20.3445166149058));
#123940=CARTESIAN_POINT('Ctrl Pts',(-18.01703932132,-21.3456936473654,-20.4716924215872));
#123941=CARTESIAN_POINT('Ctrl Pts',(-20.358642080658,-20.8505174148026,
-20.5988682282686));
#123942=CARTESIAN_POINT('Ctrl Pts',(-21.2097372705433,-18.6135530731602,
-20.72604403495));
#123943=CARTESIAN_POINT('Ctrl Pts',(-19.7894958220145,-16.6871240247294,
-20.8532198416315));
#123944=CARTESIAN_POINT('Ctrl Pts',(-17.4009050775665,-16.8385179106685,
-20.9803956483129));
#123945=CARTESIAN_POINT('Ctrl Pts',(-16.2353411557127,-18.9290164227857,
-21.1075714549944));
#123946=CARTESIAN_POINT('Ctrl Pts',(-17.3621513269132,-21.0403774632962,
-21.2347472616758));
#123947=CARTESIAN_POINT('Ctrl Pts',(-19.7475288339831,-21.2362124099542,
-21.3619230683572));
#123948=CARTESIAN_POINT('Ctrl Pts',(-21.2030926162545,-19.335594282492,
-21.4890988750387));
#123949=CARTESIAN_POINT('Ctrl Pts',(-20.3933467993028,-17.0846541387204,
-21.6162746817201));
#123950=CARTESIAN_POINT('Ctrl Pts',(-18.0613970915878,-16.5437747381437,
-21.7434504884015));
#123951=CARTESIAN_POINT('Ctrl Pts',(-16.3459127028459,-18.2187888246082,
-21.8706449514226));
#123952=CARTESIAN_POINT('Ctrl Pts',(-16.6641678043512,-19.7747689210369,
-21.9554474788832));
#123953=CARTESIAN_POINT('Ctrl Pts',(-17.117585520725,-20.3131720544228,
-21.9978580707833));
#123954=CARTESIAN_POINT('Ctrl Pts',(-19.3957372685685,-21.4249949024184,
1.39406715338186E-15));
#123955=CARTESIAN_POINT('Ctrl Pts',(-19.4773891020297,-21.3954306668132,
-2.3809056499643E-15));
#123956=CARTESIAN_POINT('Ctrl Pts',(-19.5571492231821,-21.3614659991419,
-1.69827097432457E-14));
#123957=CARTESIAN_POINT('Ctrl Pts',(-19.6348156046203,-21.3234187284543,
-1.60947644101128E-14));
#123958=CARTESIAN_POINT('Ctrl Pts',(-19.7143272588125,-21.2844674940355,
-1.51857224158522E-14));
#123959=CARTESIAN_POINT('Ctrl Pts',(-19.791645221547,-21.2412367046734,
-5.29650342682161E-15));
#123960=CARTESIAN_POINT('Ctrl Pts',(-19.8665232792573,-21.1940209467373,
-3.49026363366534E-15));
#123961=CARTESIAN_POINT('Ctrl Pts',(-19.9365886939582,-21.1498398907462,
-1.80011642596993E-15));
#123962=CARTESIAN_POINT('Ctrl Pts',(-20.0045179028423,-21.1021686855571,
-2.11652109659911E-15));
#123963=CARTESIAN_POINT('Ctrl Pts',(-20.0700783470716,-21.0512211850772,
1.8249290967276E-14));
#123964=CARTESIAN_POINT('Ctrl Pts',(-20.0997467345518,-21.0281656642803,
2.73184124025687E-14));
#123965=CARTESIAN_POINT('Ctrl Pts',(-20.128929580841,-21.0044388940273,
-8.16471876178969E-16));
#123966=CARTESIAN_POINT('Ctrl Pts',(-20.1576029444589,-20.9800594108908,
-2.27595720048157E-15));
#123967=CARTESIAN_POINT('Ctrl Pts',(-20.1753081557669,-20.9650055823179,
-2.81404609490192E-15));
#123968=CARTESIAN_POINT('Ctrl Pts',(-20.1928190804462,-20.9497028729833,
1.46191299131089E-14));
#123969=CARTESIAN_POINT('Ctrl Pts',(-20.2101297684373,-20.9341555341053,
1.78954073781767E-14));
#123970=CARTESIAN_POINT('Ctrl Pts',(-20.2222918053998,-20.923232380144,
1.99869058837013E-14));
#123971=CARTESIAN_POINT('Ctrl Pts',(-20.2343567785502,-20.9121866751007,
2.10812009255155E-14));
#123972=CARTESIAN_POINT('Ctrl Pts',(-20.2463057260566,-20.9010359825867,
1.90611415540332E-14));
#123973=CARTESIAN_POINT('Ctrl Pts',(-20.3097375112913,-20.8418417872492,
8.08726206506259E-15));
#123974=CARTESIAN_POINT('Ctrl Pts',(-20.3700069578684,-20.7796002467127,
1.56207924856702E-14));
#123975=CARTESIAN_POINT('Ctrl Pts',(-20.4268835059677,-20.7145895545046,
1.22124532708767E-15));
#123976=CARTESIAN_POINT('Ctrl Pts',(-20.4830376461181,-20.6504045847144,
-1.29954083951569E-14));
#123977=CARTESIAN_POINT('Ctrl Pts',(-20.5358849804727,-20.5835195230904,
3.31732538375231E-14));
#123978=CARTESIAN_POINT('Ctrl Pts',(-20.5851611052576,-20.5141759583256,
1.8623991238087E-14));
#123979=CARTESIAN_POINT('Ctrl Pts',(-20.6305983443472,-20.4502346450567,
5.20819756122576E-15));
#123980=CARTESIAN_POINT('Ctrl Pts',(-20.6729990002148,-20.3842022515032,
1.20148051242741E-14));
#123981=CARTESIAN_POINT('Ctrl Pts',(-20.7121180817081,-20.3162569684087,
1.55847557081756E-14));
#123982=CARTESIAN_POINT('Ctrl Pts',(-20.7284901400346,-20.2878206121505,
1.73076904422733E-14));
#123983=CARTESIAN_POINT('Ctrl Pts',(-20.7442869378835,-20.2590491139325,
1.78194106763539E-15));
#123984=CARTESIAN_POINT('Ctrl Pts',(-20.7594884026036,-20.2299553026624,
-7.7715611723761E-16));
#123985=CARTESIAN_POINT('Ctrl Pts',(-20.7693451022676,-20.2110907415789,
-2.78913582753658E-15));
#123986=CARTESIAN_POINT('Ctrl Pts',(-20.7789514808442,-20.1920906691223,
5.3858075104116E-15));
#123987=CARTESIAN_POINT('Ctrl Pts',(-20.7883017662921,-20.1729585792041,
1.33226762955019E-14));
#123988=CARTESIAN_POINT('Ctrl Pts',(-20.7942277139279,-20.1608331993265,
1.81940072510115E-14));
#123989=CARTESIAN_POINT('Ctrl Pts',(-20.8000469683619,-20.1486625665028,
-1.84110758617763E-14));
#123990=CARTESIAN_POINT('Ctrl Pts',(-20.8057568610096,-20.1364512427194,
-1.45439216225896E-14));
#123991=CARTESIAN_POINT('Ctrl Pts',(-20.8408823973353,-20.0613308641761,
8.50303143961268E-15));
#123992=CARTESIAN_POINT('Ctrl Pts',(-20.8718944952827,-19.9846287385395,
-1.36466997584689E-15));
#123993=CARTESIAN_POINT('Ctrl Pts',(-20.8985463569486,-19.9065734343537,
8.02136135291676E-15));
#123994=CARTESIAN_POINT('Ctrl Pts',(-20.9251982186144,-19.8285181301678,
1.71371673297255E-14));
#123995=CARTESIAN_POINT('Ctrl Pts',(-20.9474903161071,-19.7491089176507,
2.28815957419719E-14));
#123996=CARTESIAN_POINT('Ctrl Pts',(-20.9651215428786,-19.6685651028304,
1.17683640610267E-14));
#123997=CARTESIAN_POINT('Ctrl Pts',(-20.9829460124324,-19.5871385070737,
3.68731748262102E-16));
#123998=CARTESIAN_POINT('Ctrl Pts',(-20.9960061448808,-19.5045510760419,
8.47281867687301E-15));
#123999=CARTESIAN_POINT('Ctrl Pts',(-21.0043775994437,-19.4211942605515,
5.24580379135386E-15));
#124000=CARTESIAN_POINT('Ctrl Pts',(-21.0078360662703,-19.3867573799617,
3.88824530893464E-15));
#124001=CARTESIAN_POINT('Ctrl Pts',(-21.0104937056419,-19.3521893421996,
-6.81493208789715E-15));
#124002=CARTESIAN_POINT('Ctrl Pts',(-21.0123534306943,-19.3175186761032,
-9.90874049477952E-15));
#124003=CARTESIAN_POINT('Ctrl Pts',(-21.0130853886539,-19.3038728578793,
-1.11360150531808E-14));
#124004=CARTESIAN_POINT('Ctrl Pts',(-21.0136937288726,-19.2902091507495,
-9.58524568179392E-15));
#124005=CARTESIAN_POINT('Ctrl Pts',(-21.0141781582269,-19.2765469516024,
-8.40993941153556E-15));
#124006=CARTESIAN_POINT('Ctrl Pts',(-21.0170629175674,-19.1951890482203,
2.39772407460705E-16));
#124007=CARTESIAN_POINT('Ctrl Pts',(-21.0155663596031,-19.1137544906502,
-4.57265169201993E-15));
#124008=CARTESIAN_POINT('Ctrl Pts',(-21.0098211098971,-19.032600466024,
-7.49400541621981E-15));
#124009=CARTESIAN_POINT('Ctrl Pts',(-21.0040551996084,-18.9511546021348,
-1.04258646664422E-14));
#124010=CARTESIAN_POINT('Ctrl Pts',(-20.9940096109022,-18.8699902747511,
-7.23578815300704E-16));
#124011=CARTESIAN_POINT('Ctrl Pts',(-20.9797677234152,-18.7894801122778,
-9.63118473862323E-15));
#124012=CARTESIAN_POINT('Ctrl Pts',(-20.9656475490784,-18.7096580008453,
-1.84626650234184E-14));
#124013=CARTESIAN_POINT('Ctrl Pts',(-20.9474020559163,-18.6304779977825,
4.37978233446551E-15));
#124014=CARTESIAN_POINT('Ctrl Pts',(-20.9250689772833,-18.5523290403031,
3.24740234702858E-15));
#124015=CARTESIAN_POINT('Ctrl Pts',(-20.9157717581042,-18.5197957743688,
2.84403675857501E-15));
#124016=CARTESIAN_POINT('Ctrl Pts',(-20.9057656579654,-18.487441581366,
-8.15092194160927E-15));
#124017=CARTESIAN_POINT('Ctrl Pts',(-20.895051417118,-18.4552964308102,
9.54791801177635E-15));
#124018=CARTESIAN_POINT('Ctrl Pts',(-20.8895107429844,-18.4386731528066,
1.8801206371564E-14));
#124019=CARTESIAN_POINT('Ctrl Pts',(-20.8837798116562,-18.4221037461655,
4.8672899678328E-15));
#124020=CARTESIAN_POINT('Ctrl Pts',(-20.8778666087312,-18.4056137222238,
3.1641356201817E-15));
#124021=CARTESIAN_POINT('Ctrl Pts',(-20.8511334397242,-18.3310634991803,
-4.87055585791377E-15));
#124022=CARTESIAN_POINT('Ctrl Pts',(-20.820647395102,-18.2580374311815,
9.31417420162474E-15));
#124023=CARTESIAN_POINT('Ctrl Pts',(-20.7864673279414,-18.1868947789178,
2.85882428840978E-15));
#124024=CARTESIAN_POINT('Ctrl Pts',(-20.7601551114488,-18.1321283309931,
-2.11057976962231E-15));
#124025=CARTESIAN_POINT('Ctrl Pts',(-20.7316528702852,-18.0784783891692,
-2.19989686484456E-15));
#124026=CARTESIAN_POINT('Ctrl Pts',(-20.7009722503935,-18.0261235328628,
-1.56819002228303E-14));
#124027=CARTESIAN_POINT('Ctrl Pts',(-20.6917379810896,-18.0103657403473,
-1.98295234918966E-14));
#124028=CARTESIAN_POINT('Ctrl Pts',(-20.6823062897647,-17.9947253717853,
-1.79315186665554E-14));
#124029=CARTESIAN_POINT('Ctrl Pts',(-20.6726772825947,-17.9792075775192,
-1.94011473553246E-14));
#124030=CARTESIAN_POINT('Ctrl Pts',(-20.6644523726372,-17.9659525805787,
-2.06245694983287E-14));
#124031=CARTESIAN_POINT('Ctrl Pts',(-20.6560857633015,-17.9527907829532,
-9.64091344835667E-16));
#124032=CARTESIAN_POINT('Ctrl Pts',(-20.6475820647203,-17.939731697129,
-8.60422844084496E-16));
#124033=CARTESIAN_POINT('Ctrl Pts',(-20.6064305493276,-17.8765355282888,
-2.54369252641912E-16));
#124034=CARTESIAN_POINT('Ctrl Pts',(-20.5620419163801,-17.8156943120762,
-1.60673095715126E-14));
#124035=CARTESIAN_POINT('Ctrl Pts',(-20.5144495416444,-17.7575477797155,
-1.36834987785051E-14));
#124036=CARTESIAN_POINT('Ctrl Pts',(-20.4703172832204,-17.7036286843383,
-1.20256236272586E-14));
#124037=CARTESIAN_POINT('Ctrl Pts',(-20.4234296462928,-17.6520265735113,
9.73448774144503E-15));
#124038=CARTESIAN_POINT('Ctrl Pts',(-20.3737906735959,-17.6030455128839,
2.54796184151473E-14));
#124039=CARTESIAN_POINT('Ctrl Pts',(-20.368202112649,-17.5975310224002,
2.72370406592353E-14));
#124040=CARTESIAN_POINT('Ctrl Pts',(-20.3625786573857,-17.5920497923538,
1.54409020709891E-15));
#124041=CARTESIAN_POINT('Ctrl Pts',(-20.3569206763285,-17.5866019717796,
-2.72004641033163E-15));
#124042=CARTESIAN_POINT('Origin',(23.734,9.62950000000001,-14.8));
#124043=CARTESIAN_POINT('',(23.734,10.6295,-14.8));
#124044=CARTESIAN_POINT('',(23.734,9.62950000000001,-14.8));
#124045=CARTESIAN_POINT('',(23.734,14.42025,-14.8));
#124046=CARTESIAN_POINT('',(23.534,10.6295,-14.8));
#124047=CARTESIAN_POINT('',(23.734,10.6295,-14.8));
#124048=CARTESIAN_POINT('',(23.534,9.62950000000001,-14.8));
#124049=CARTESIAN_POINT('',(23.534,10.6295,-14.8));
#124050=CARTESIAN_POINT('',(23.734,9.62950000000001,-14.8));
#124051=CARTESIAN_POINT('Origin',(23.734,9.62950000000001,-17.2));
#124052=CARTESIAN_POINT('',(23.734,9.62950000000001,-17.2));
#124053=CARTESIAN_POINT('',(23.734,9.62950000000001,-8.6));
#124054=CARTESIAN_POINT('',(23.534,9.62950000000001,-17.2));
#124055=CARTESIAN_POINT('',(23.534,9.62950000000001,-14.8));
#124056=CARTESIAN_POINT('',(23.734,9.62950000000001,-17.2));
#124057=CARTESIAN_POINT('Origin',(23.734,9.12950000000001,-17.2));
#124058=CARTESIAN_POINT('',(23.734,9.12950000000001,-17.2));
#124059=CARTESIAN_POINT('',(23.734,14.17025,-17.2));
#124060=CARTESIAN_POINT('',(23.534,9.12950000000001,-17.2));
#124061=CARTESIAN_POINT('',(23.534,9.62950000000001,-17.2));
#124062=CARTESIAN_POINT('',(23.734,9.12950000000001,-17.2));
#124063=CARTESIAN_POINT('Origin',(23.734,10.1295,-19.2));
#124064=CARTESIAN_POINT('',(23.734,10.1295,-19.2));
#124065=CARTESIAN_POINT('',(23.734,7.19765,-13.3363));
#124066=CARTESIAN_POINT('',(23.534,10.1295,-19.2));
#124067=CARTESIAN_POINT('',(23.534,9.12950000000001,-17.2));
#124068=CARTESIAN_POINT('',(23.734,10.1295,-19.2));
#124069=CARTESIAN_POINT('Origin',(23.734,11.1295,-17.2));
#124070=CARTESIAN_POINT('',(23.734,11.1295,-17.2));
#124071=CARTESIAN_POINT('',(23.734,15.37765,-8.7037));
#124072=CARTESIAN_POINT('',(23.534,11.1295,-17.2));
#124073=CARTESIAN_POINT('',(23.534,11.1295,-17.2));
#124074=CARTESIAN_POINT('',(23.734,11.1295,-17.2));
#124075=CARTESIAN_POINT('Origin',(23.734,10.6295,-17.2));
#124076=CARTESIAN_POINT('',(23.734,10.6295,-17.2));
#124077=CARTESIAN_POINT('',(23.734,14.92025,-17.2));
#124078=CARTESIAN_POINT('',(23.534,10.6295,-17.2));
#124079=CARTESIAN_POINT('',(23.534,10.6295,-17.2));
#124080=CARTESIAN_POINT('',(23.734,10.6295,-17.2));
#124081=CARTESIAN_POINT('Origin',(23.734,10.6295,-14.8));
#124082=CARTESIAN_POINT('',(23.734,10.6295,-7.4));
#124083=CARTESIAN_POINT('',(23.534,10.6295,-14.8));
#124084=CARTESIAN_POINT('Origin',(23.734,10.1295,-17.));
#124085=CARTESIAN_POINT('',(23.534,10.1295,-20.));
#124086=CARTESIAN_POINT('Origin',(23.534,10.1295,-17.));
#124087=CARTESIAN_POINT('',(23.734,10.1295,-20.));
#124088=CARTESIAN_POINT('',(23.734,10.1295,-20.));
#124089=CARTESIAN_POINT('Origin',(23.734,10.1295,-17.));
#124090=CARTESIAN_POINT('Origin',(23.534,10.1295,-17.));
#124091=CARTESIAN_POINT('Origin',(23.734,-9.8705,-7.));
#124092=CARTESIAN_POINT('',(23.734,-5.8705,-11.4721359549996));
#124093=CARTESIAN_POINT('',(23.734,-3.8705,-7.));
#124094=CARTESIAN_POINT('Origin',(23.734,-9.8705,-7.));
#124095=CARTESIAN_POINT('',(23.534,-5.8705,-11.4721359549996));
#124096=CARTESIAN_POINT('',(23.734,-5.8705,-11.4721359549996));
#124097=CARTESIAN_POINT('',(23.534,-3.87049999999999,-7.));
#124098=CARTESIAN_POINT('Origin',(23.534,-9.8705,-7.));
#124099=CARTESIAN_POINT('',(23.734,-3.8705,-7.));
#124100=CARTESIAN_POINT('Origin',(23.734,4.1295,-7.));
#124101=CARTESIAN_POINT('',(23.734,4.1295,-7.));
#124102=CARTESIAN_POINT('',(23.734,11.67025,-7.));
#124103=CARTESIAN_POINT('',(23.534,4.1295,-7.));
#124104=CARTESIAN_POINT('',(23.534,4.1295,-7.));
#124105=CARTESIAN_POINT('',(23.734,4.1295,-7.));
#124106=CARTESIAN_POINT('Origin',(23.734,10.1295,-7.));
#124107=CARTESIAN_POINT('',(23.734,6.1295,-11.4721359549996));
#124108=CARTESIAN_POINT('Origin',(23.734,10.1295,-7.));
#124109=CARTESIAN_POINT('',(23.534,6.1295,-11.4721359549996));
#124110=CARTESIAN_POINT('Origin',(23.534,10.1295,-7.));
#124111=CARTESIAN_POINT('',(23.734,6.1295,-11.4721359549996));
#124112=CARTESIAN_POINT('Origin',(23.734,6.1295,-22.));
#124113=CARTESIAN_POINT('',(23.734,6.1295,-11.));
#124114=CARTESIAN_POINT('',(23.534,6.1295,-22.));
#124115=CARTESIAN_POINT('Origin',(23.734,-5.8705,-11.4721359549996));
#124116=CARTESIAN_POINT('',(23.734,-5.8705,-5.73606797749979));
#124117=CARTESIAN_POINT('',(23.534,-5.8705,-22.));
#124118=CARTESIAN_POINT('Origin',(23.534,0.129500000000005,-11.5));
#124119=CARTESIAN_POINT('',(23.534,0.129500000000002,-21.));
#124120=CARTESIAN_POINT('Origin',(23.534,0.129500000000004,-17.));
#124121=CARTESIAN_POINT('',(23.534,-9.8705,-12.));
#124122=CARTESIAN_POINT('Origin',(23.534,-9.8705,-7.));
#124123=CARTESIAN_POINT('Origin',(23.734,-9.37049999999999,-16.8));
#124124=CARTESIAN_POINT('',(23.734,-9.37049999999999,-19.2));
#124125=CARTESIAN_POINT('',(23.734,-9.37049999999999,-16.8));
#124126=CARTESIAN_POINT('',(23.734,-9.37049999999999,-8.4));
#124127=CARTESIAN_POINT('',(23.534,-9.37049999999999,-19.2));
#124128=CARTESIAN_POINT('',(23.734,-9.37049999999999,-19.2));
#124129=CARTESIAN_POINT('',(23.534,-9.37049999999999,-16.8));
#124130=CARTESIAN_POINT('',(23.534,-9.37049999999999,-19.2));
#124131=CARTESIAN_POINT('',(23.734,-9.37049999999999,-16.8));
#124132=CARTESIAN_POINT('Origin',(23.734,-8.87049999999999,-16.8));
#124133=CARTESIAN_POINT('',(23.734,-8.87049999999999,-16.8));
#124134=CARTESIAN_POINT('',(23.734,5.17025,-16.8));
#124135=CARTESIAN_POINT('',(23.534,-8.87049999999999,-16.8));
#124136=CARTESIAN_POINT('',(23.534,-9.37049999999999,-16.8));
#124137=CARTESIAN_POINT('',(23.734,-8.87049999999999,-16.8));
#124138=CARTESIAN_POINT('Origin',(23.734,-9.8705,-14.8));
#124139=CARTESIAN_POINT('',(23.734,-9.8705,-14.8));
#124140=CARTESIAN_POINT('',(23.734,-9.92234999999999,-14.6963));
#124141=CARTESIAN_POINT('',(23.534,-9.8705,-14.8));
#124142=CARTESIAN_POINT('',(23.534,-8.87049999999999,-16.8));
#124143=CARTESIAN_POINT('',(23.734,-9.8705,-14.8));
#124144=CARTESIAN_POINT('Origin',(23.734,-10.8705,-16.8));
#124145=CARTESIAN_POINT('',(23.734,-10.8705,-16.8));
#124146=CARTESIAN_POINT('',(23.734,-4.50234999999999,-4.0637));
#124147=CARTESIAN_POINT('',(23.534,-10.8705,-16.8));
#124148=CARTESIAN_POINT('',(23.534,-10.8705,-16.8));
#124149=CARTESIAN_POINT('',(23.734,-10.8705,-16.8));
#124150=CARTESIAN_POINT('Origin',(23.734,-10.3705,-16.8));
#124151=CARTESIAN_POINT('',(23.734,-10.3705,-16.8));
#124152=CARTESIAN_POINT('',(23.734,4.42025,-16.8));
#124153=CARTESIAN_POINT('',(23.534,-10.3705,-16.8));
#124154=CARTESIAN_POINT('',(23.534,-10.3705,-16.8));
#124155=CARTESIAN_POINT('',(23.734,-10.3705,-16.8));
#124156=CARTESIAN_POINT('Origin',(23.734,-10.3705,-19.2));
#124157=CARTESIAN_POINT('',(23.734,-10.3705,-19.2));
#124158=CARTESIAN_POINT('',(23.734,-10.3705,-9.6));
#124159=CARTESIAN_POINT('',(23.534,-10.3705,-19.2));
#124160=CARTESIAN_POINT('',(23.534,-10.3705,-19.2));
#124161=CARTESIAN_POINT('',(23.734,-10.3705,-19.2));
#124162=CARTESIAN_POINT('Origin',(23.734,-9.37049999999999,-19.2));
#124163=CARTESIAN_POINT('',(23.734,4.92025,-19.2));
#124164=CARTESIAN_POINT('',(23.534,-9.37049999999999,-19.2));
#124165=CARTESIAN_POINT('Origin',(23.734,-9.8705,-17.));
#124166=CARTESIAN_POINT('',(23.534,-9.8705,-20.));
#124167=CARTESIAN_POINT('Origin',(23.534,-9.8705,-17.));
#124168=CARTESIAN_POINT('',(23.734,-9.8705,-20.));
#124169=CARTESIAN_POINT('',(23.734,-9.8705,-20.));
#124170=CARTESIAN_POINT('Origin',(23.734,-9.8705,-17.));
#124171=CARTESIAN_POINT('Origin',(23.534,-9.8705,-17.));
#124172=CARTESIAN_POINT('Origin',(23.734,19.211,0.));
#124173=CARTESIAN_POINT('Origin',(23.734,19.211,0.));
#124174=CARTESIAN_POINT('Origin',(23.734,0.129500000000004,-17.));
#124175=CARTESIAN_POINT('',(17.734,0.129500000000003,-21.));
#124176=CARTESIAN_POINT('Origin',(17.734,0.129500000000004,-17.));
#124177=CARTESIAN_POINT('',(23.734,0.129500000000005,-21.));
#124178=CARTESIAN_POINT('Origin',(17.734,0.129500000000004,-17.));
#124179=CARTESIAN_POINT('Origin',(17.734,10.1295,-7.));
#124180=CARTESIAN_POINT('Origin',(23.734,-9.8705,-7.));
#124181=CARTESIAN_POINT('',(17.734,-9.8705,-12.));
#124182=CARTESIAN_POINT('Origin',(17.734,-9.8705,-7.));
#124183=CARTESIAN_POINT('',(23.734,-9.8705,-12.));
#124184=CARTESIAN_POINT('Origin',(17.734,-9.8705,-7.));
#124185=CARTESIAN_POINT('Origin',(-23.734,-9.8705,-7.));
#124186=CARTESIAN_POINT('',(-23.734,-3.8705,-7.));
#124187=CARTESIAN_POINT('',(-23.734,-5.8705,-11.4721359549996));
#124188=CARTESIAN_POINT('Origin',(-23.734,-9.8705,-7.));
#124189=CARTESIAN_POINT('',(-23.534,-3.87049999999999,-7.));
#124190=CARTESIAN_POINT('',(-23.734,-3.8705,-7.));
#124191=CARTESIAN_POINT('',(-23.534,-5.8705,-11.4721359549996));
#124192=CARTESIAN_POINT('Origin',(-23.534,-9.8705,-7.));
#124193=CARTESIAN_POINT('',(-23.734,-5.8705,-11.4721359549996));
#124194=CARTESIAN_POINT('Origin',(-23.734,4.1295,-7.));
#124195=CARTESIAN_POINT('',(-23.734,4.1295,-7.));
#124196=CARTESIAN_POINT('',(-23.734,-7.41125,-7.));
#124197=CARTESIAN_POINT('',(-23.534,4.1295,-7.));
#124198=CARTESIAN_POINT('',(-23.734,4.1295,-7.));
#124199=CARTESIAN_POINT('',(-23.534,4.1295,-7.));
#124200=CARTESIAN_POINT('Origin',(-23.734,10.1295,-7.));
#124201=CARTESIAN_POINT('',(-23.734,6.1295,-11.4721359549996));
#124202=CARTESIAN_POINT('Origin',(-23.734,10.1295,-7.));
#124203=CARTESIAN_POINT('',(-23.534,6.1295,-11.4721359549996));
#124204=CARTESIAN_POINT('',(-23.734,6.1295,-11.4721359549996));
#124205=CARTESIAN_POINT('Origin',(-23.534,10.1295,-7.));
#124206=CARTESIAN_POINT('Origin',(-23.734,6.1295,-22.));
#124207=CARTESIAN_POINT('',(-23.734,6.1295,-11.));
#124208=CARTESIAN_POINT('',(-23.534,6.1295,-22.));
#124209=CARTESIAN_POINT('Origin',(-23.734,-5.8705,-11.4721359549996));
#124210=CARTESIAN_POINT('',(-23.734,-5.8705,-5.73606797749979));
#124211=CARTESIAN_POINT('',(-23.534,-5.8705,-22.));
#124212=CARTESIAN_POINT('Origin',(-23.534,0.129500000000005,-11.5));
#124213=CARTESIAN_POINT('',(-23.534,0.129500000000002,-21.));
#124214=CARTESIAN_POINT('Origin',(-23.534,0.129500000000004,-17.));
#124215=CARTESIAN_POINT('',(-23.534,-9.8705,-12.));
#124216=CARTESIAN_POINT('Origin',(-23.534,-9.8705,-7.));
#124217=CARTESIAN_POINT('Origin',(-23.734,-9.37049999999999,-16.8));
#124218=CARTESIAN_POINT('',(-23.734,-9.37049999999999,-16.8));
#124219=CARTESIAN_POINT('',(-23.734,-9.37049999999999,-19.2));
#124220=CARTESIAN_POINT('',(-23.734,-9.3705,-8.4));
#124221=CARTESIAN_POINT('',(-23.534,-9.37049999999999,-16.8));
#124222=CARTESIAN_POINT('',(-23.734,-9.37049999999999,-16.8));
#124223=CARTESIAN_POINT('',(-23.534,-9.37049999999999,-19.2));
#124224=CARTESIAN_POINT('',(-23.534,-9.37049999999999,-19.2));
#124225=CARTESIAN_POINT('',(-23.734,-9.37049999999999,-19.2));
#124226=CARTESIAN_POINT('Origin',(-23.734,-8.87049999999999,-16.8));
#124227=CARTESIAN_POINT('',(-23.734,-8.87049999999999,-16.8));
#124228=CARTESIAN_POINT('',(-23.734,-13.91125,-16.8));
#124229=CARTESIAN_POINT('',(-23.534,-8.87049999999999,-16.8));
#124230=CARTESIAN_POINT('',(-23.734,-8.87049999999999,-16.8));
#124231=CARTESIAN_POINT('',(-23.534,-9.37049999999999,-16.8));
#124232=CARTESIAN_POINT('Origin',(-23.734,-9.8705,-14.8));
#124233=CARTESIAN_POINT('',(-23.734,-9.8705,-14.8));
#124234=CARTESIAN_POINT('',(-23.734,-13.73865,-7.0637));
#124235=CARTESIAN_POINT('',(-23.534,-9.8705,-14.8));
#124236=CARTESIAN_POINT('',(-23.734,-9.8705,-14.8));
#124237=CARTESIAN_POINT('',(-23.534,-8.87049999999999,-16.8));
#124238=CARTESIAN_POINT('Origin',(-23.734,-10.8705,-16.8));
#124239=CARTESIAN_POINT('',(-23.734,-10.8705,-16.8));
#124240=CARTESIAN_POINT('',(-23.734,-8.31864999999999,-11.6963));
#124241=CARTESIAN_POINT('',(-23.534,-10.8705,-16.8));
#124242=CARTESIAN_POINT('',(-23.734,-10.8705,-16.8));
#124243=CARTESIAN_POINT('',(-23.534,-10.8705,-16.8));
#124244=CARTESIAN_POINT('Origin',(-23.734,-10.3705,-16.8));
#124245=CARTESIAN_POINT('',(-23.734,-10.3705,-16.8));
#124246=CARTESIAN_POINT('',(-23.734,-14.66125,-16.8));
#124247=CARTESIAN_POINT('',(-23.534,-10.3705,-16.8));
#124248=CARTESIAN_POINT('',(-23.734,-10.3705,-16.8));
#124249=CARTESIAN_POINT('',(-23.534,-10.3705,-16.8));
#124250=CARTESIAN_POINT('Origin',(-23.734,-10.3705,-19.2));
#124251=CARTESIAN_POINT('',(-23.734,-10.3705,-19.2));
#124252=CARTESIAN_POINT('',(-23.734,-10.3705,-9.6));
#124253=CARTESIAN_POINT('',(-23.534,-10.3705,-19.2));
#124254=CARTESIAN_POINT('',(-23.734,-10.3705,-19.2));
#124255=CARTESIAN_POINT('',(-23.534,-10.3705,-19.2));
#124256=CARTESIAN_POINT('Origin',(-23.734,-9.37049999999999,-19.2));
#124257=CARTESIAN_POINT('',(-23.734,-14.16125,-19.2));
#124258=CARTESIAN_POINT('',(-23.534,-9.37049999999999,-19.2));
#124259=CARTESIAN_POINT('Origin',(-23.734,-9.8705,-17.));
#124260=CARTESIAN_POINT('',(-23.734,-9.8705,-20.));
#124261=CARTESIAN_POINT('Origin',(-23.734,-9.8705,-17.));
#124262=CARTESIAN_POINT('',(-23.534,-9.8705,-20.));
#124263=CARTESIAN_POINT('',(-23.734,-9.8705,-20.));
#124264=CARTESIAN_POINT('Origin',(-23.534,-9.8705,-17.));
#124265=CARTESIAN_POINT('Origin',(-23.534,-9.8705,-17.));
#124266=CARTESIAN_POINT('Origin',(-23.734,9.62950000000001,-14.8));
#124267=CARTESIAN_POINT('',(-23.734,9.62950000000001,-14.8));
#124268=CARTESIAN_POINT('',(-23.734,10.6295,-14.8));
#124269=CARTESIAN_POINT('',(-23.734,-4.66124999999999,-14.8));
#124270=CARTESIAN_POINT('',(-23.534,9.62950000000001,-14.8));
#124271=CARTESIAN_POINT('',(-23.734,9.62950000000001,-14.8));
#124272=CARTESIAN_POINT('',(-23.534,10.6295,-14.8));
#124273=CARTESIAN_POINT('',(-23.534,10.6295,-14.8));
#124274=CARTESIAN_POINT('',(-23.734,10.6295,-14.8));
#124275=CARTESIAN_POINT('Origin',(-23.734,9.62950000000001,-17.2));
#124276=CARTESIAN_POINT('',(-23.734,9.62950000000001,-17.2));
#124277=CARTESIAN_POINT('',(-23.734,9.62950000000001,-8.6));
#124278=CARTESIAN_POINT('',(-23.534,9.62950000000001,-17.2));
#124279=CARTESIAN_POINT('',(-23.734,9.62950000000001,-17.2));
#124280=CARTESIAN_POINT('',(-23.534,9.62950000000001,-14.8));
#124281=CARTESIAN_POINT('Origin',(-23.734,9.12950000000001,-17.2));
#124282=CARTESIAN_POINT('',(-23.734,9.12950000000001,-17.2));
#124283=CARTESIAN_POINT('',(-23.734,-4.91124999999999,-17.2));
#124284=CARTESIAN_POINT('',(-23.534,9.12950000000001,-17.2));
#124285=CARTESIAN_POINT('',(-23.734,9.12950000000001,-17.2));
#124286=CARTESIAN_POINT('',(-23.534,9.62950000000001,-17.2));
#124287=CARTESIAN_POINT('Origin',(-23.734,10.1295,-19.2));
#124288=CARTESIAN_POINT('',(-23.734,10.1295,-19.2));
#124289=CARTESIAN_POINT('',(-23.734,3.38135000000002,-5.7037));
#124290=CARTESIAN_POINT('',(-23.534,10.1295,-19.2));
#124291=CARTESIAN_POINT('',(-23.734,10.1295,-19.2));
#124292=CARTESIAN_POINT('',(-23.534,9.12950000000001,-17.2));
#124293=CARTESIAN_POINT('Origin',(-23.734,11.1295,-17.2));
#124294=CARTESIAN_POINT('',(-23.734,11.1295,-17.2));
#124295=CARTESIAN_POINT('',(-23.734,11.56135,-16.3363));
#124296=CARTESIAN_POINT('',(-23.534,11.1295,-17.2));
#124297=CARTESIAN_POINT('',(-23.734,11.1295,-17.2));
#124298=CARTESIAN_POINT('',(-23.534,11.1295,-17.2));
#124299=CARTESIAN_POINT('Origin',(-23.734,10.6295,-17.2));
#124300=CARTESIAN_POINT('',(-23.734,10.6295,-17.2));
#124301=CARTESIAN_POINT('',(-23.734,-4.16125,-17.2));
#124302=CARTESIAN_POINT('',(-23.534,10.6295,-17.2));
#124303=CARTESIAN_POINT('',(-23.734,10.6295,-17.2));
#124304=CARTESIAN_POINT('',(-23.534,10.6295,-17.2));
#124305=CARTESIAN_POINT('Origin',(-23.734,10.6295,-14.8));
#124306=CARTESIAN_POINT('',(-23.734,10.6295,-7.4));
#124307=CARTESIAN_POINT('',(-23.534,10.6295,-14.8));
#124308=CARTESIAN_POINT('Origin',(-23.734,10.1295,-17.));
#124309=CARTESIAN_POINT('',(-23.734,10.1295,-20.));
#124310=CARTESIAN_POINT('Origin',(-23.734,10.1295,-17.));
#124311=CARTESIAN_POINT('',(-23.534,10.1295,-20.));
#124312=CARTESIAN_POINT('',(-23.734,10.1295,-20.));
#124313=CARTESIAN_POINT('Origin',(-23.534,10.1295,-17.));
#124314=CARTESIAN_POINT('Origin',(-23.534,10.1295,-17.));
#124315=CARTESIAN_POINT('Origin',(-23.734,-18.952,0.));
#124316=CARTESIAN_POINT('Origin',(-23.734,-18.952,0.));
#124317=CARTESIAN_POINT('Origin',(-23.734,-18.952,0.));
#124318=CARTESIAN_POINT('',(-23.734,-18.952,0.));
#124319=CARTESIAN_POINT('',(-23.734,-18.952,0.));
#124320=CARTESIAN_POINT('',(-23.734,19.211,0.));
#124321=CARTESIAN_POINT('',(-23.734,19.211,0.));
#124322=CARTESIAN_POINT('',(-23.734,19.211,0.));
#124323=CARTESIAN_POINT('Origin',(-17.734,10.1295,-7.));
#124324=CARTESIAN_POINT('Origin',(-23.734,-9.8705,-7.));
#124325=CARTESIAN_POINT('',(-17.734,-9.8705,-12.));
#124326=CARTESIAN_POINT('',(-23.734,-9.8705,-12.));
#124327=CARTESIAN_POINT('Origin',(-17.734,-9.8705,-7.));
#124328=CARTESIAN_POINT('Origin',(-17.734,-9.8705,-7.));
#124329=CARTESIAN_POINT('Origin',(-23.734,0.129500000000004,-17.));
#124330=CARTESIAN_POINT('',(-17.734,0.129500000000003,-21.));
#124331=CARTESIAN_POINT('',(-23.734,0.129500000000005,-21.));
#124332=CARTESIAN_POINT('Origin',(-17.734,0.129500000000004,-17.));
#124333=CARTESIAN_POINT('Origin',(-17.734,0.129500000000004,-17.));
#124334=CARTESIAN_POINT('Origin',(-18.734,0.12950000000008,-22.));
#124335=CARTESIAN_POINT('',(-21.234,0.12950000000008,-21.5));
#124336=CARTESIAN_POINT('',(-21.234,0.12950000000008,-22.));
#124337=CARTESIAN_POINT('Origin',(-18.734,0.12950000000008,-21.5));
#124338=CARTESIAN_POINT('Origin',(0.,0.12950000000008,-21.5));
#124339=CARTESIAN_POINT('Origin',(18.734,0.12950000000008,-22.));
#124340=CARTESIAN_POINT('',(16.234,0.12950000000008,-21.5));
#124341=CARTESIAN_POINT('',(16.234,0.12950000000008,-22.));
#124342=CARTESIAN_POINT('Origin',(18.734,0.12950000000008,-21.5));
#124343=CARTESIAN_POINT('Origin',(0.,0.12950000000008,-21.5));
#124344=CARTESIAN_POINT('Origin',(-7.0995,19.4175,0.));
#124345=CARTESIAN_POINT('',(-7.0995,19.4175,0.));
#124346=CARTESIAN_POINT('',(-7.0995,19.4175,0.));
#124347=CARTESIAN_POINT('',(-7.0995,16.8045,0.));
#124348=CARTESIAN_POINT('Origin',(-10.7505,17.8045,0.));
#124349=CARTESIAN_POINT('Origin',(-10.7505,17.8045,0.));
#124350=CARTESIAN_POINT('Origin',(-9.06658668237251,24.2952266006623,0.));
#124351=CARTESIAN_POINT('',(-9.06658668237251,24.4862266006622,0.));
#124352=CARTESIAN_POINT('Origin',(-9.06658668237251,24.2952266006623,0.));
#124353=CARTESIAN_POINT('',(-9.06658668237251,24.4862266006622,0.));
#124354=CARTESIAN_POINT('Origin',(-7.30158668237251,24.4862266006622,0.));
#124355=CARTESIAN_POINT('',(-7.30158668237251,24.4862266006622,0.));
#124356=CARTESIAN_POINT('',(-9.06658668237251,24.4862266006622,0.));
#124357=CARTESIAN_POINT('',(-7.30158668237251,24.4862266006622,0.));
#124358=CARTESIAN_POINT('Origin',(-7.30158668237251,24.6772266006623,0.));
#124359=CARTESIAN_POINT('',(-7.11058668237251,24.6772266006623,0.));
#124360=CARTESIAN_POINT('Origin',(-7.30158668237251,24.6772266006623,0.));
#124361=CARTESIAN_POINT('',(-7.11058668237251,24.6772266006623,0.));
#124362=CARTESIAN_POINT('Origin',(-7.11058668237251,25.8032266006623,0.));
#124363=CARTESIAN_POINT('',(-7.11058668237251,25.8032266006623,0.));
#124364=CARTESIAN_POINT('',(-7.11058668237251,24.6772266006623,0.));
#124365=CARTESIAN_POINT('',(-7.11058668237251,25.8032266006623,0.));
#124366=CARTESIAN_POINT('Origin',(-7.36458668237251,25.8032266006623,0.));
#124367=CARTESIAN_POINT('',(-7.36458668237251,26.0572266006623,0.));
#124368=CARTESIAN_POINT('Origin',(-7.36458668237251,25.8032266006623,0.));
#124369=CARTESIAN_POINT('',(-7.36458668237251,26.0572266006623,0.));
#124370=CARTESIAN_POINT('Origin',(-18.734,24.211,0.));
#124371=CARTESIAN_POINT('',(-18.734,24.211,0.));
#124372=CARTESIAN_POINT('',(-7.36458668237251,26.0572266006622,0.));
#124373=CARTESIAN_POINT('',(-18.734,24.211,0.));
#124374=CARTESIAN_POINT('Origin',(-18.734,19.211,0.));
#124375=CARTESIAN_POINT('Origin',(-18.734,19.211,0.));
#124376=CARTESIAN_POINT('Origin',(-18.734,-18.952,0.));
#124377=CARTESIAN_POINT('',(-18.734,-23.952,0.));
#124378=CARTESIAN_POINT('Origin',(-18.734,-18.952,0.));
#124379=CARTESIAN_POINT('',(-18.734,-23.952,0.));
#124380=CARTESIAN_POINT('Origin',(18.734,-23.952,0.));
#124381=CARTESIAN_POINT('',(18.734,-23.952,0.));
#124382=CARTESIAN_POINT('',(-18.734,-23.952,0.));
#124383=CARTESIAN_POINT('',(18.734,-23.952,0.));
#124384=CARTESIAN_POINT('Origin',(18.734,-18.952,0.));
#124385=CARTESIAN_POINT('',(23.734,-18.952,0.));
#124386=CARTESIAN_POINT('Origin',(18.734,-18.952,0.));
#124387=CARTESIAN_POINT('',(23.734,-18.952,0.));
#124388=CARTESIAN_POINT('Origin',(23.734,19.211,0.));
#124389=CARTESIAN_POINT('',(23.734,19.211,0.));
#124390=CARTESIAN_POINT('',(23.734,19.211,0.));
#124391=CARTESIAN_POINT('',(23.734,19.211,0.));
#124392=CARTESIAN_POINT('Origin',(18.734,19.211,0.));
#124393=CARTESIAN_POINT('',(18.734,24.211,0.));
#124394=CARTESIAN_POINT('Origin',(18.734,19.211,0.));
#124395=CARTESIAN_POINT('',(18.734,24.211,0.));
#124396=CARTESIAN_POINT('Origin',(7.36458668237251,26.0572266006622,0.));
#124397=CARTESIAN_POINT('',(7.36458668237251,26.0572266006622,0.));
#124398=CARTESIAN_POINT('',(7.36458668237251,26.0572266006622,0.));
#124399=CARTESIAN_POINT('',(7.36458668237251,26.0572266006622,0.));
#124400=CARTESIAN_POINT('Origin',(7.36458668237251,25.8032266006622,0.));
#124401=CARTESIAN_POINT('',(7.11058668237251,25.8032266006622,0.));
#124402=CARTESIAN_POINT('Origin',(7.36458668237251,25.8032266006622,0.));
#124403=CARTESIAN_POINT('',(7.11058668237251,25.8032266006622,0.));
#124404=CARTESIAN_POINT('Origin',(7.11058668237251,24.6772266006623,0.));
#124405=CARTESIAN_POINT('',(7.11058668237251,24.6772266006623,0.));
#124406=CARTESIAN_POINT('',(7.11058668237251,24.6772266006623,0.));
#124407=CARTESIAN_POINT('',(7.11058668237251,24.6772266006623,0.));
#124408=CARTESIAN_POINT('Origin',(7.30158668237251,24.6772266006623,0.));
#124409=CARTESIAN_POINT('',(7.30158668237251,24.4862266006622,0.));
#124410=CARTESIAN_POINT('Origin',(7.30158668237251,24.6772266006623,0.));
#124411=CARTESIAN_POINT('',(7.30158668237251,24.4862266006622,0.));
#124412=CARTESIAN_POINT('Origin',(9.06658668237251,24.4862266006622,0.));
#124413=CARTESIAN_POINT('',(9.06658668237251,24.4862266006622,0.));
#124414=CARTESIAN_POINT('',(9.06658668237251,24.4862266006622,0.));
#124415=CARTESIAN_POINT('',(9.06658668237251,24.4862266006622,0.));
#124416=CARTESIAN_POINT('Origin',(9.06658668237251,24.2952266006623,0.));
#124417=CARTESIAN_POINT('',(9.25758668237251,24.2952266006623,0.));
#124418=CARTESIAN_POINT('Origin',(9.06658668237251,24.2952266006623,0.));
#124419=CARTESIAN_POINT('',(9.25758668237251,24.2952266006623,0.));
#124420=CARTESIAN_POINT('Origin',(9.25758668237251,21.5062266006623,0.));
#124421=CARTESIAN_POINT('',(9.25758668237251,21.5062266006623,0.));
#124422=CARTESIAN_POINT('',(9.25758668237251,21.5062266006623,0.));
#124423=CARTESIAN_POINT('',(9.25758668237251,21.5062266006623,0.));
#124424=CARTESIAN_POINT('Origin',(10.7505,17.8045,0.));
#124425=CARTESIAN_POINT('Origin',(10.7505,17.8045,0.));
#124426=CARTESIAN_POINT('Origin',(0.,1.05261330033112,0.));
#124427=CARTESIAN_POINT('',(0.,0.,0.));
#124428=CARTESIAN_POINT('',(0.,0.,0.));
#124429=CARTESIAN_POINT('Origin',(25.9997814655409,18.8808065108639,21.5));
#124430=CARTESIAN_POINT('',(22.9997814655409,18.8808065108619,18.5));
#124431=CARTESIAN_POINT('Origin',(22.9997814655409,18.8808065108619,21.5));
#124432=CARTESIAN_POINT('',(25.9997805061207,18.8808065108639,18.5));
#124433=CARTESIAN_POINT('',(25.9997814655409,18.8808065108639,18.5));
#124434=CARTESIAN_POINT('Origin',(25.9997805061207,18.8808065108639,21.5));
#124435=CARTESIAN_POINT('Origin',(22.9997814655409,18.8808065108619,21.5));
#124436=CARTESIAN_POINT('Origin',(-26.0001963416363,18.8817346167756,21.5));
#124437=CARTESIAN_POINT('',(-26.0001963416363,18.8817346167756,18.5));
#124438=CARTESIAN_POINT('Origin',(-26.0001963416363,18.8817346167756,21.5));
#124439=CARTESIAN_POINT('',(-23.0001963435476,18.8816275275843,18.5));
#124440=CARTESIAN_POINT('',(-26.0001963416363,18.8817346167756,18.5));
#124441=CARTESIAN_POINT('Origin',(-23.0001963435476,18.8816275275843,21.5));
#124442=CARTESIAN_POINT('Origin',(-23.0001963435476,18.8816275275843,21.5));
#124443=CARTESIAN_POINT('Origin',(-6.00033197323811,24.630714186474,25.5));
#124444=CARTESIAN_POINT('',(-15.7502284469069,24.1310622223319,25.5));
#124445=CARTESIAN_POINT('',(-12.0002284492961,24.1309283608428,25.5));
#124446=CARTESIAN_POINT('',(-6.00034982143666,24.1307141867926,25.5));
#124447=CARTESIAN_POINT('',(-12.0002106010975,24.6309283605242,26.));
#124448=CARTESIAN_POINT('Origin',(-12.0002106010975,24.6309283605242,25.5));
#124449=CARTESIAN_POINT('',(-15.8748746000505,24.631066672069,26.));
#124450=CARTESIAN_POINT('',(-6.00033197323811,24.630714186474,26.));
#124451=CARTESIAN_POINT('Origin',(-15.8748746000505,24.631066672069,25.5));
#124452=CARTESIAN_POINT('Origin',(5.99980902926158,24.6306070926795,25.5));
#124453=CARTESIAN_POINT('',(12.,24.1305,25.5));
#124454=CARTESIAN_POINT('',(5.9998001051623,24.1306070927591,25.5));
#124455=CARTESIAN_POINT('',(12.0000089240993,24.6304999999204,26.));
#124456=CARTESIAN_POINT('Origin',(12.0000089240993,24.6304999999204,25.5));
#124457=CARTESIAN_POINT('',(5.99980902926158,24.6306070926795,26.));
#124458=CARTESIAN_POINT('Origin',(15.5005576038968,36.3806823573572,25.5));
#124459=CARTESIAN_POINT('',(16.0005576038968,44.6304565378295,25.5));
#124460=CARTESIAN_POINT('',(15.5005576038968,44.6304565378295,26.));
#124461=CARTESIAN_POINT('Origin',(15.5005576038968,44.6304565378295,25.5));
#124462=CARTESIAN_POINT('',(15.5005576038968,36.1384565378295,26.));
#124463=CARTESIAN_POINT('',(15.5005576038968,36.3806823573572,26.));
#124464=CARTESIAN_POINT('',(16.0005576038968,36.1384565378295,25.5));
#124465=CARTESIAN_POINT('Origin',(15.5005576038968,36.1384565378295,25.5));
#124466=CARTESIAN_POINT('',(16.0005576038968,36.3806823573572,25.5));
#124467=CARTESIAN_POINT('Origin',(16.5085576038968,36.1384565378295,25.5));
#124468=CARTESIAN_POINT('',(16.5085576038968,35.1304565378295,26.));
#124469=CARTESIAN_POINT('',(16.5085576038968,35.6304565378295,25.5));
#124470=CARTESIAN_POINT('Origin',(16.5085576038968,35.1304565378295,25.5));
#124471=CARTESIAN_POINT('Origin',(16.5085576038968,36.1384565378295,25.5));
#124472=CARTESIAN_POINT('Origin',(16.5085576038968,36.1384565378295,26.));
#124473=CARTESIAN_POINT('Origin',(8.25411460523903,35.1304565378295,25.5));
#124474=CARTESIAN_POINT('',(16.8285576038968,35.1304565378295,26.));
#124475=CARTESIAN_POINT('',(16.8285576038968,35.6304565378295,25.5));
#124476=CARTESIAN_POINT('Origin',(16.8285576038968,35.1304565378295,25.5));
#124477=CARTESIAN_POINT('',(8.25411460523903,35.6304565378295,25.5));
#124478=CARTESIAN_POINT('',(8.25411460523903,35.1304565378295,26.));
#124479=CARTESIAN_POINT('Origin',(16.8285576038968,32.6304565378295,25.5));
#124480=CARTESIAN_POINT('',(18.5963245568632,34.3982234907959,26.));
#124481=CARTESIAN_POINT('',(18.9498779474565,34.7517768813891,25.5));
#124482=CARTESIAN_POINT('Origin',(18.5963245568632,34.3982234907959,25.5));
#124483=CARTESIAN_POINT('Origin',(16.8285576038968,32.6304565378295,25.5));
#124484=CARTESIAN_POINT('Origin',(16.8285576038968,32.6304565378295,26.));
#124485=CARTESIAN_POINT('Origin',(15.5139901477705,37.4805578998886,25.5));
#124486=CARTESIAN_POINT('',(24.1817610214557,28.8127870262033,26.));
#124487=CARTESIAN_POINT('',(24.535314412049,29.1663404167966,25.5));
#124488=CARTESIAN_POINT('Origin',(24.1817610214557,28.8127870262033,25.5));
#124489=CARTESIAN_POINT('',(15.8675435383638,37.8341112904819,25.5));
#124490=CARTESIAN_POINT('',(15.5139901477705,37.4805578998886,26.));
#124491=CARTESIAN_POINT('Origin',(20.9997805061163,25.6308065108639,25.5));
#124492=CARTESIAN_POINT('',(25.4997805061163,25.6308065108639,26.));
#124493=CARTESIAN_POINT('',(25.9997805061163,25.6308065108639,25.5));
#124494=CARTESIAN_POINT('Origin',(25.4997805061163,25.6308065108639,25.5));
#124495=CARTESIAN_POINT('Origin',(20.9997805061163,25.6308065108639,25.5));
#124496=CARTESIAN_POINT('Origin',(20.9997805061163,25.6308065108639,26.));
#124497=CARTESIAN_POINT('Origin',(25.4997805061163,26.8808573438743,25.5));
#124498=CARTESIAN_POINT('',(25.4997805061163,12.1308065108639,26.));
#124499=CARTESIAN_POINT('',(25.9997805061163,12.1308065108639,25.5));
#124500=CARTESIAN_POINT('Origin',(25.4997805061163,12.1308065108639,25.5));
#124501=CARTESIAN_POINT('',(25.9997805061163,26.8808573438743,25.5));
#124502=CARTESIAN_POINT('',(25.4997805061163,26.8808573438743,26.));
#124503=CARTESIAN_POINT('Ctrl Pts',(25.4997805061163,12.1308065108638,26.));
#124504=CARTESIAN_POINT('Ctrl Pts',(25.4997805061163,11.6308065108639,26.));
#124505=CARTESIAN_POINT('Ctrl Pts',(24.9997805061164,11.630806510864,26.));
#124506=CARTESIAN_POINT('Ctrl Pts',(25.9997805061163,12.1308065108638,26.));
#124507=CARTESIAN_POINT('Ctrl Pts',(25.9997805061164,11.1308065108638,26.));
#124508=CARTESIAN_POINT('Ctrl Pts',(24.9997805061164,11.1308065108639,26.));
#124509=CARTESIAN_POINT('Ctrl Pts',(25.9997805061163,12.1308065108638,25.5));
#124510=CARTESIAN_POINT('Ctrl Pts',(25.9997805061164,11.1308065108638,25.5));
#124511=CARTESIAN_POINT('Ctrl Pts',(24.9997805061164,11.1308065108639,25.5));
#124512=CARTESIAN_POINT('',(24.9997805061163,11.6308065108639,26.));
#124513=CARTESIAN_POINT('',(24.9997805061163,11.1308065108639,25.5));
#124514=CARTESIAN_POINT('Origin',(24.9997805061163,11.6308065108639,25.5));
#124515=CARTESIAN_POINT('Origin',(24.9997805061163,12.1308065108639,25.5));
#124516=CARTESIAN_POINT('Origin',(24.9997805061163,12.1308065108639,26.));
#124517=CARTESIAN_POINT('Origin',(12.4997260563488,11.6308065108639,25.5));
#124518=CARTESIAN_POINT('',(20.4997805061163,11.1308065108639,25.5));
#124519=CARTESIAN_POINT('',(12.4997260563488,11.1308065108639,25.5));
#124520=CARTESIAN_POINT('',(20.7068872873028,11.6308065108639,26.));
#124521=CARTESIAN_POINT('',(12.4997260563488,11.6308065108639,26.));
#124522=CARTESIAN_POINT('Origin',(20.7068872873028,11.6308065108639,25.5));
#124523=CARTESIAN_POINT('Origin',(11.4782812553205,20.8594125428461,25.5));
#124524=CARTESIAN_POINT('',(19.0000070232196,12.6305799937605,25.5));
#124525=CARTESIAN_POINT('',(11.1247278647273,20.5058591522529,25.5));
#124526=CARTESIAN_POINT('',(19.5000070232196,12.8376867749471,26.));
#124527=CARTESIAN_POINT('',(11.4782812553205,20.8594125428461,26.));
#124528=CARTESIAN_POINT('Origin',(19.5000070232196,12.8376867749471,25.5));
#124529=CARTESIAN_POINT('Origin',(19.5000070232196,20.3807440853227,25.5));
#124530=CARTESIAN_POINT('',(19.5000070232196,21.8015799937605,26.));
#124531=CARTESIAN_POINT('',(19.5000070232196,20.3807440853227,26.));
#124532=CARTESIAN_POINT('',(19.0000070232196,21.8015799937605,25.5));
#124533=CARTESIAN_POINT('Origin',(19.5000070232196,21.8015799937605,25.5));
#124534=CARTESIAN_POINT('',(19.0000070232196,20.3807440853227,25.5));
#124535=CARTESIAN_POINT('Origin',(18.0000070232196,21.8015799937605,25.5));
#124536=CARTESIAN_POINT('',(18.7042143673984,23.1260013830489,26.));
#124537=CARTESIAN_POINT('',(18.4694785860055,22.6845275866195,25.5));
#124538=CARTESIAN_POINT('Origin',(18.7042143673984,23.1260013830489,25.5));
#124539=CARTESIAN_POINT('Origin',(18.0000070232196,21.8015799937605,25.5));
#124540=CARTESIAN_POINT('Origin',(18.0000070232196,21.8015799937605,26.));
#124541=CARTESIAN_POINT('Origin',(10.3759028387591,27.5542431726415,25.5));
#124542=CARTESIAN_POINT('',(15.75,24.1305,25.5));
#124543=CARTESIAN_POINT('',(10.1411670573662,27.112769376212,25.5));
#124544=CARTESIAN_POINT('',(15.8746640014216,24.6305,26.));
#124545=CARTESIAN_POINT('',(10.3759028387591,27.5542431726415,26.));
#124546=CARTESIAN_POINT('Origin',(15.8746640014216,24.6305,25.5));
#124547=CARTESIAN_POINT('Origin',(7.87483580329061,24.6305,25.5));
#124548=CARTESIAN_POINT('',(7.87483580329061,24.1305,25.5));
#124549=CARTESIAN_POINT('',(7.87483580329061,24.6305,26.));
#124550=CARTESIAN_POINT('Origin',(-9.01646660547503,28.2774328600768,25.5));
#124551=CARTESIAN_POINT('',(-18.7044786694047,23.12666906083,26.));
#124552=CARTESIAN_POINT('',(-9.01646660547503,28.2774328600768,26.));
#124553=CARTESIAN_POINT('',(-18.4697586471852,22.6851868854601,25.5));
#124554=CARTESIAN_POINT('Origin',(-18.7044786694047,23.12666906083,25.5));
#124555=CARTESIAN_POINT('',(-8.78174658325559,27.8359506847069,25.5));
#124556=CARTESIAN_POINT('Origin',(-18.0003186027463,21.8022225347204,25.5));
#124557=CARTESIAN_POINT('',(-19.5003186017906,21.8022760793161,26.));
#124558=CARTESIAN_POINT('',(-19.0003186021092,21.8022582311175,25.5));
#124559=CARTESIAN_POINT('Origin',(-19.5003186017906,21.8022760793161,25.5));
#124560=CARTESIAN_POINT('Origin',(-18.0003186027463,21.8022225347204,25.5));
#124561=CARTESIAN_POINT('Origin',(-18.0003186027463,21.8022225347204,26.));
#124562=CARTESIAN_POINT('Origin',(-19.5002056346847,24.9669401637651,25.5));
#124563=CARTESIAN_POINT('',(-19.000645973767,12.6312582369605,25.5));
#124564=CARTESIAN_POINT('',(-19.0002056350033,24.9669223155665,25.5));
#124565=CARTESIAN_POINT('',(-19.5006385804826,12.8383828662136,26.));
#124566=CARTESIAN_POINT('',(-19.5002056346847,24.9669401637651,26.));
#124567=CARTESIAN_POINT('Origin',(-19.5006385804826,12.8383828662136,25.5));
#124568=CARTESIAN_POINT('Origin',(-10.7288557519193,21.609539475044,25.5));
#124569=CARTESIAN_POINT('',(-20.707561925074,11.6315456841765,26.));
#124570=CARTESIAN_POINT('',(-10.7288557519193,21.609539475044,26.));
#124571=CARTESIAN_POINT('',(-20.500472992218,11.1315382915292,25.5));
#124572=CARTESIAN_POINT('Origin',(-20.707561925074,11.6315456841765,25.5));
#124573=CARTESIAN_POINT('',(-10.3753149821335,21.2559734640938,25.5));
#124574=CARTESIAN_POINT('Origin',(-10.2506862658096,11.6311724113903,25.5));
#124575=CARTESIAN_POINT('',(-25.0004551411524,11.6316989249976,26.));
#124576=CARTESIAN_POINT('',(-10.2506862658096,11.6311724113903,26.));
#124577=CARTESIAN_POINT('',(-25.0004729893509,11.1316989253161,25.5));
#124578=CARTESIAN_POINT('Origin',(-25.0004551411524,11.6316989249976,25.5));
#124579=CARTESIAN_POINT('',(-10.2507041140081,11.1311724117089,25.5));
#124580=CARTESIAN_POINT('Ctrl Pts',(-25.0004551411524,11.6316989249976,
26.));
#124581=CARTESIAN_POINT('Ctrl Pts',(-25.5004551408338,11.6317167731961,
26.));
#124582=CARTESIAN_POINT('Ctrl Pts',(-25.5004372926352,12.1317167728775,
26.));
#124583=CARTESIAN_POINT('Ctrl Pts',(-25.0004729893508,11.1316989253161,
26.));
#124584=CARTESIAN_POINT('Ctrl Pts',(-26.000472988714,11.131734621713,26.0000000000001));
#124585=CARTESIAN_POINT('Ctrl Pts',(-26.0004372923167,12.1317346210762,
26.));
#124586=CARTESIAN_POINT('Ctrl Pts',(-25.0004729893509,11.1316989253161,
25.5));
#124587=CARTESIAN_POINT('Ctrl Pts',(-26.000472988714,11.131734621713,25.5));
#124588=CARTESIAN_POINT('Ctrl Pts',(-26.0004372923167,12.1317346210762,
25.5));
#124589=CARTESIAN_POINT('',(-25.5004372926353,12.1317167728775,26.));
#124590=CARTESIAN_POINT('',(-26.0004372923167,12.1317346210761,25.5));
#124591=CARTESIAN_POINT('Origin',(-25.5004372926353,12.1317167728775,25.5));
#124592=CARTESIAN_POINT('Origin',(-25.0004372929538,12.131698924679,25.5));
#124593=CARTESIAN_POINT('Origin',(-25.0004372929538,12.131698924679,26.));
#124594=CARTESIAN_POINT('Origin',(-25.5001517196441,20.1317675956942,25.5));
#124595=CARTESIAN_POINT('',(-25.4999553912744,25.6317167642765,26.));
#124596=CARTESIAN_POINT('',(-25.9999553909559,25.631734612475,25.5));
#124597=CARTESIAN_POINT('Origin',(-25.4999553912744,25.6317167642765,25.5));
#124598=CARTESIAN_POINT('',(-26.0001517193255,20.1317854438928,25.5));
#124599=CARTESIAN_POINT('',(-25.5001517196441,20.1317675956942,26.));
#124600=CARTESIAN_POINT('Origin',(-20.9999553941414,25.6315561304895,25.5));
#124601=CARTESIAN_POINT('',(-24.1818223222136,28.8136502290417,26.));
#124602=CARTESIAN_POINT('',(-24.5353630919994,29.167216239992,25.5));
#124603=CARTESIAN_POINT('Origin',(-24.1818223222136,28.8136502290417,25.5));
#124604=CARTESIAN_POINT('Origin',(-20.9999553941414,25.6315561304895,25.5));
#124605=CARTESIAN_POINT('Origin',(-20.9999553941414,25.6315561304895,26.));
#124606=CARTESIAN_POINT('Origin',(-18.3067027565145,34.6883503685105,25.5));
#124607=CARTESIAN_POINT('',(-18.5961864812216,34.3988873101177,26.));
#124608=CARTESIAN_POINT('',(-18.9497272510074,34.7524533210679,25.5));
#124609=CARTESIAN_POINT('Origin',(-18.5961864812216,34.3988873101177,25.5));
#124610=CARTESIAN_POINT('',(-18.6602435263003,35.0419163794607,25.5));
#124611=CARTESIAN_POINT('',(-18.3067027565145,34.6883503685105,26.));
#124612=CARTESIAN_POINT('Origin',(-16.8284826322926,32.6310572553665,25.5));
#124613=CARTESIAN_POINT('',(-16.8283933912999,35.1310572537737,26.));
#124614=CARTESIAN_POINT('',(-16.8283755431013,35.6310572534551,25.5));
#124615=CARTESIAN_POINT('Origin',(-16.8283933912999,35.1310572537737,25.5));
#124616=CARTESIAN_POINT('Origin',(-16.8284826322926,32.6310572553665,25.5));
#124617=CARTESIAN_POINT('Origin',(-16.8284826322926,32.6310572553665,26.));
#124618=CARTESIAN_POINT('Origin',(-8.41423596303023,35.1307568986686,25.5));
#124619=CARTESIAN_POINT('',(-16.5083933915038,35.1310458309266,26.));
#124620=CARTESIAN_POINT('',(-16.5083755433052,35.631045830608,25.5));
#124621=CARTESIAN_POINT('Origin',(-16.5083933915038,35.1310458309266,25.5));
#124622=CARTESIAN_POINT('',(-8.41421811483168,35.6307568983501,25.5));
#124623=CARTESIAN_POINT('',(-8.41423596303023,35.1307568986686,26.));
#124624=CARTESIAN_POINT('Origin',(-16.5083574095355,36.1390458302844,25.5));
#124625=CARTESIAN_POINT('',(-15.5003574101777,36.1390098483161,26.));
#124626=CARTESIAN_POINT('',(-16.0003574098591,36.1390276965147,25.5));
#124627=CARTESIAN_POINT('Origin',(-15.5003574101777,36.1390098483161,25.5));
#124628=CARTESIAN_POINT('Origin',(-16.5083574095355,36.1390458302844,25.5));
#124629=CARTESIAN_POINT('Origin',(-16.5083574095355,36.1390458302844,26.));
#124630=CARTESIAN_POINT('Origin',(-15.5005003304909,32.1352356652978,25.5));
#124631=CARTESIAN_POINT('',(-15.5000542763735,44.6310098429057,26.));
#124632=CARTESIAN_POINT('',(-16.0000542760549,44.6310276911043,25.5));
#124633=CARTESIAN_POINT('Origin',(-15.5000542763735,44.6310098429057,25.5));
#124634=CARTESIAN_POINT('',(-16.0005003301724,32.1352535134963,25.5));
#124635=CARTESIAN_POINT('',(-15.5005003304909,32.1352356652978,26.));
#124636=CARTESIAN_POINT('Origin',(6.40011460523903,44.6304565378295,25.5));
#124637=CARTESIAN_POINT('',(12.8005576038968,45.1304565378295,25.5));
#124638=CARTESIAN_POINT('',(12.8005576038968,44.6304565378295,26.));
#124639=CARTESIAN_POINT('Origin',(12.8005576038968,44.6304565378295,25.5));
#124640=CARTESIAN_POINT('',(6.40011460523903,44.6304565378295,26.));
#124641=CARTESIAN_POINT('',(15.5005576038968,45.1304565378295,25.5));
#124642=CARTESIAN_POINT('Origin',(15.5005576038968,44.6304565378295,25.5));
#124643=CARTESIAN_POINT('',(6.40011460523903,45.1304565378295,25.5));
#124644=CARTESIAN_POINT('Origin',(-6.40003962806013,44.6307992338217,25.5));
#124645=CARTESIAN_POINT('',(-12.8000364298952,45.130913462315,25.5));
#124646=CARTESIAN_POINT('',(-6.40003070396085,45.130799233742,25.5));
#124647=CARTESIAN_POINT('',(-12.8000453539944,44.6309134623946,26.));
#124648=CARTESIAN_POINT('Origin',(-12.8000453539944,44.6309134623946,25.5));
#124649=CARTESIAN_POINT('',(-6.40003962806013,44.6307992338217,26.));
#124650=CARTESIAN_POINT('Origin',(-7.74989684768079,44.6307331902084,25.5));
#124651=CARTESIAN_POINT('',(-15.5000364281749,45.1310098425872,25.5));
#124652=CARTESIAN_POINT('',(-7.74987899948224,45.1307331898898,25.5));
#124653=CARTESIAN_POINT('Origin',(-15.5000542763735,44.6310098429057,25.5));
#124654=CARTESIAN_POINT('',(-7.74989684768079,44.6307331902084,26.));
#124655=CARTESIAN_POINT('Origin',(-15.5000542763735,44.6310098429057,25.5));
#124656=CARTESIAN_POINT('Origin',(-15.5000542763735,44.6310098429057,25.5));
#124657=CARTESIAN_POINT('Origin',(15.5005576038968,44.6304565378295,25.5));
#124658=CARTESIAN_POINT('Origin',(15.5005576038968,44.6304565378295,25.5));
#124659=CARTESIAN_POINT('Origin',(-15.7502284469069,24.1310622223319,26.));
#124660=CARTESIAN_POINT('',(-18.4697586471852,22.6851868854601,12.5));
#124661=CARTESIAN_POINT('',(-18.4697586471852,22.6851868854601,26.));
#124662=CARTESIAN_POINT('',(-15.7502284469069,24.1310622223319,12.5));
#124663=CARTESIAN_POINT('',(-8.78174658325559,27.8359506847069,12.5));
#124664=CARTESIAN_POINT('',(-15.7502284469069,24.1310622223319,26.));
#124665=CARTESIAN_POINT('Origin',(-18.0003186027463,21.8022225347204,26.));
#124666=CARTESIAN_POINT('',(-19.0003186021092,21.8022582311175,12.5));
#124667=CARTESIAN_POINT('',(-19.0003186021092,21.8022582311175,26.));
#124668=CARTESIAN_POINT('Origin',(-18.0003186027463,21.8022225347204,12.5));
#124669=CARTESIAN_POINT('Origin',(-19.0003186021092,21.8022582311175,26.));
#124670=CARTESIAN_POINT('',(-19.000645973767,12.6312582369605,12.5));
#124671=CARTESIAN_POINT('',(-19.000645973767,12.6312582369605,26.));
#124672=CARTESIAN_POINT('',(-19.0002056350033,24.9669223155665,12.5));
#124673=CARTESIAN_POINT('Origin',(-19.000645973767,12.6312582369605,26.));
#124674=CARTESIAN_POINT('',(-20.500472992218,11.1315382915292,12.5));
#124675=CARTESIAN_POINT('',(-20.500472992218,11.1315382915292,26.));
#124676=CARTESIAN_POINT('',(-10.3753149821335,21.2559734640938,12.5));
#124677=CARTESIAN_POINT('Origin',(-20.500472992218,11.1315382915292,26.));
#124678=CARTESIAN_POINT('',(-25.0004729893509,11.1316989253161,12.5));
#124679=CARTESIAN_POINT('',(-25.0004729893509,11.1316989253161,26.));
#124680=CARTESIAN_POINT('',(-10.2507041140081,11.1311724117089,12.5));
#124681=CARTESIAN_POINT('Origin',(-25.0004372929538,12.131698924679,26.));
#124682=CARTESIAN_POINT('',(-26.0004372923167,12.1317346210761,12.5));
#124683=CARTESIAN_POINT('',(-26.0004372923167,12.1317346210761,26.));
#124684=CARTESIAN_POINT('Origin',(-25.0004372929538,12.131698924679,12.5));
#124685=CARTESIAN_POINT('Origin',(-26.0004372923167,12.1317346210761,26.));
#124686=CARTESIAN_POINT('',(-25.9999553909559,25.631734612475,12.5));
#124687=CARTESIAN_POINT('',(-25.9999553909559,25.631734612475,26.));
#124688=CARTESIAN_POINT('',(-26.0001517193255,20.1317854438928,12.5));
#124689=CARTESIAN_POINT('Origin',(-20.9999553941414,25.6315561304895,26.));
#124690=CARTESIAN_POINT('',(-24.5353630919994,29.167216239992,12.5));
#124691=CARTESIAN_POINT('',(-24.5353630919994,29.167216239992,26.));
#124692=CARTESIAN_POINT('Origin',(-20.9999553941414,25.6315561304895,12.5));
#124693=CARTESIAN_POINT('Origin',(-24.5353630919994,29.167216239992,26.));
#124694=CARTESIAN_POINT('',(-18.9497272510074,34.7524533210679,12.5));
#124695=CARTESIAN_POINT('',(-18.9497272510074,34.7524533210679,26.));
#124696=CARTESIAN_POINT('',(-18.6602435263003,35.0419163794607,12.5));
#124697=CARTESIAN_POINT('Origin',(-16.8284826322926,32.6310572553665,26.));
#124698=CARTESIAN_POINT('',(-16.8283755431013,35.6310572534551,15.));
#124699=CARTESIAN_POINT('',(-16.8283755431013,35.6310572534551,26.));
#124700=CARTESIAN_POINT('',(-18.7486119524321,34.9360742604969,15.));
#124701=CARTESIAN_POINT('Origin',(-16.8284826322926,32.6310572553665,15.));
#124702=CARTESIAN_POINT('',(-18.7486119524321,34.9360742604969,12.5));
#124703=CARTESIAN_POINT('',(-18.7486119524321,34.9360742604969,12.));
#124704=CARTESIAN_POINT('Origin',(-16.8284826322926,32.6310572553665,12.5));
#124705=CARTESIAN_POINT('Origin',(-16.8283755431013,35.6310572534551,26.));
#124706=CARTESIAN_POINT('',(-16.5083755433052,35.631045830608,15.));
#124707=CARTESIAN_POINT('',(-16.5083755433052,35.631045830608,26.));
#124708=CARTESIAN_POINT('',(-16.3514391790885,35.6310402285453,15.));
#124709=CARTESIAN_POINT('Origin',(-16.5083574095355,36.1390458302844,26.));
#124710=CARTESIAN_POINT('',(-16.0003574098591,36.1390276965147,15.));
#124711=CARTESIAN_POINT('',(-16.0003574098591,36.1390276965147,26.));
#124712=CARTESIAN_POINT('Origin',(-16.5083574095355,36.1390458302844,15.));
#124713=CARTESIAN_POINT('Origin',(-16.0003574098591,36.1390276965147,26.));
#124714=CARTESIAN_POINT('',(-16.0000542760549,44.6310276911043,12.5));
#124715=CARTESIAN_POINT('',(-16.0000542760549,44.6310276911043,26.));
#124716=CARTESIAN_POINT('',(-16.0002503206678,39.1390276946033,12.5));
#124717=CARTESIAN_POINT('',(-16.0005003301724,32.1352535134963,12.5));
#124718=CARTESIAN_POINT('',(-16.0002503206678,39.1390276946033,15.));
#124719=CARTESIAN_POINT('',(-16.0002503206678,39.1390276946033,12.));
#124720=CARTESIAN_POINT('',(-16.0003574097789,36.1390299426383,15.));
#124721=CARTESIAN_POINT('Origin',(-15.5000542763735,44.6310098429057,26.));
#124722=CARTESIAN_POINT('',(-15.5000364281749,45.1310098425872,12.5));
#124723=CARTESIAN_POINT('',(-15.5000364281749,45.1310098425872,26.));
#124724=CARTESIAN_POINT('Origin',(-15.5000542763735,44.6310098429057,12.5));
#124725=CARTESIAN_POINT('Origin',(-15.5000364281749,45.1310098425872,26.));
#124726=CARTESIAN_POINT('',(-12.8000364298952,45.130913462315,12.5));
#124727=CARTESIAN_POINT('',(-12.8000364298952,45.130913462315,26.));
#124728=CARTESIAN_POINT('',(-7.74987899948224,45.1307331898898,12.5));
#124729=CARTESIAN_POINT('Origin',(-12.8000364298952,45.130913462315,26.));
#124730=CARTESIAN_POINT('',(12.8005576038968,45.1304565378295,12.5));
#124731=CARTESIAN_POINT('',(12.8005576038968,45.1304565378295,26.));
#124732=CARTESIAN_POINT('',(-6.40003070396085,45.130799233742,12.5));
#124733=CARTESIAN_POINT('Origin',(12.8005576038968,45.1304565378295,26.));
#124734=CARTESIAN_POINT('',(15.5005576038968,45.1304565378295,12.5));
#124735=CARTESIAN_POINT('',(15.5005576038968,45.1304565378295,26.));
#124736=CARTESIAN_POINT('',(6.40011460523903,45.1304565378295,12.5));
#124737=CARTESIAN_POINT('Origin',(-0.000328393418778106,28.1309081768848,
26.));
#124738=CARTESIAN_POINT('Origin',(-15.5005003304909,32.1352356652978,12.5));
#124739=CARTESIAN_POINT('',(-15.5000542763735,44.6310098429057,12.));
#124740=CARTESIAN_POINT('Origin',(-15.5000542763735,44.6310098429057,12.5));
#124741=CARTESIAN_POINT('',(-15.5002337542308,39.6031114612468,12.));
#124742=CARTESIAN_POINT('',(-15.5005003304909,32.1352356652978,12.));
#124743=CARTESIAN_POINT('Ctrl Pts',(-15.5002337542308,39.6031114612469,
12.));
#124744=CARTESIAN_POINT('Ctrl Pts',(-15.5012802807782,39.6022052080442,
12.));
#124745=CARTESIAN_POINT('Ctrl Pts',(-15.5023266329781,39.6012987501675,
12.0000032854501));
#124746=CARTESIAN_POINT('Ctrl Pts',(-15.5262620426631,39.580555287795,12.0001535475902));
#124747=CARTESIAN_POINT('Ctrl Pts',(-15.549079071856,39.5606097425883,12.0018685097915));
#124748=CARTESIAN_POINT('Ctrl Pts',(-15.6555915595815,39.4666813170044,
12.0172417791965));
#124749=CARTESIAN_POINT('Ctrl Pts',(-15.7342867260662,39.3947272458287,
12.0503680939609));
#124750=CARTESIAN_POINT('Ctrl Pts',(-15.8544463319837,39.2818437637677,
12.1407858340455));
#124751=CARTESIAN_POINT('Ctrl Pts',(-15.8992348499764,39.2385644267119,
12.1913094880828));
#124752=CARTESIAN_POINT('Ctrl Pts',(-15.9582815856617,39.1808059783461,
12.2931553699351));
#124753=CARTESIAN_POINT('Ctrl Pts',(-15.9780823063818,39.1611342110301,
12.3427321807669));
#124754=CARTESIAN_POINT('Ctrl Pts',(-15.996608615715,39.1426753037105,12.4305871755406));
#124755=CARTESIAN_POINT('Ctrl Pts',(-16.0002503206678,39.1390276946034,
12.4651445835938));
#124756=CARTESIAN_POINT('Ctrl Pts',(-16.0002503206678,39.1390276946034,
12.5));
#124757=CARTESIAN_POINT('Origin',(-16.0003574098591,36.1390276965147,12.5));
#124758=CARTESIAN_POINT('',(-18.8658210632966,34.1292719773217,12.));
#124759=CARTESIAN_POINT('Origin',(-16.0003574098591,36.1390276965147,12.));
#124760=CARTESIAN_POINT('',(-18.810086036752,34.6128021370802,12.1018952060707));
#124761=CARTESIAN_POINT('Ctrl Pts',(-18.8658210632966,34.1292719773218,
12.));
#124762=CARTESIAN_POINT('Ctrl Pts',(-18.8656807480304,34.1308827000774,
12.));
#124763=CARTESIAN_POINT('Ctrl Pts',(-18.8655400049988,34.1324933903515,
12.0000032434225));
#124764=CARTESIAN_POINT('Ctrl Pts',(-18.8573778375603,34.2256175041316,
12.0003779495169));
#124765=CARTESIAN_POINT('Ctrl Pts',(-18.8478563981534,34.3178692956092,
12.0111952320961));
#124766=CARTESIAN_POINT('Ctrl Pts',(-18.8288764025859,34.4771426650498,
12.048491997422));
#124767=CARTESIAN_POINT('Ctrl Pts',(-18.8196146553393,34.5470501977567,
12.0716841972469));
#124768=CARTESIAN_POINT('Ctrl Pts',(-18.810086036752,34.6128021370802,12.1018952060707));
#124769=CARTESIAN_POINT('Ctrl Pts',(-18.810086036752,34.6128021370802,12.1018952060707));
#124770=CARTESIAN_POINT('Ctrl Pts',(-18.8089992232141,34.6203016604522,
12.1053410081124));
#124771=CARTESIAN_POINT('Ctrl Pts',(-18.8078973392296,34.6277440210717,
12.1088851897267));
#124772=CARTESIAN_POINT('Ctrl Pts',(-18.7957307106799,34.7082643255815,
12.1486504715915));
#124773=CARTESIAN_POINT('Ctrl Pts',(-18.784159852527,34.7702166242448,12.1921413513201));
#124774=CARTESIAN_POINT('Ctrl Pts',(-18.7672884639414,34.8535445163286,
12.2764946297254));
#124775=CARTESIAN_POINT('Ctrl Pts',(-18.7606689443804,34.8835886882299,
12.3169287768681));
#124776=CARTESIAN_POINT('Ctrl Pts',(-18.7520329511296,34.9216311139679,
12.3986190308673));
#124777=CARTESIAN_POINT('Ctrl Pts',(-18.7494922500063,34.9323419849364,
12.4373510176214));
#124778=CARTESIAN_POINT('Ctrl Pts',(-18.7486753311664,34.9358059214554,
12.4851148185871));
#124779=CARTESIAN_POINT('Ctrl Pts',(-18.7486119524321,34.936074260497,12.4925693313125));
#124780=CARTESIAN_POINT('Ctrl Pts',(-18.7486119524321,34.936074260497,12.5));
#124781=CARTESIAN_POINT('Origin',(-16.0003574098591,36.1390276965147,12.5));
#124782=CARTESIAN_POINT('Origin',(-7.74989684768079,44.6307331902083,12.5));
#124783=CARTESIAN_POINT('',(-12.8000542780937,44.6309134626335,12.));
#124784=CARTESIAN_POINT('Origin',(-12.8000542780937,44.6309134626335,12.5));
#124785=CARTESIAN_POINT('',(-7.74989684768079,44.6307331902083,12.));
#124786=CARTESIAN_POINT('Origin',(-15.5000542763735,44.6310098429057,12.5));
#124787=CARTESIAN_POINT('Origin',(-6.40003962806013,44.6307992338217,12.5));
#124788=CARTESIAN_POINT('',(12.8005486797976,44.6304565379091,12.));
#124789=CARTESIAN_POINT('Origin',(12.8005486797976,44.6304565379091,12.5));
#124790=CARTESIAN_POINT('',(-6.40003962806013,44.6307992338217,12.));
#124791=CARTESIAN_POINT('Origin',(6.40011460523903,44.6304565378295,12.5));
#124792=CARTESIAN_POINT('',(15.5005576038968,44.6304565378295,12.));
#124793=CARTESIAN_POINT('Origin',(15.5005576038968,44.6304565378295,12.5));
#124794=CARTESIAN_POINT('',(6.40011460523903,44.6304565378295,12.));
#124795=CARTESIAN_POINT('Origin',(-15.5000542763735,44.6310098429057,12.5));
#124796=CARTESIAN_POINT('Origin',(16.0005576038968,36.1384565378295,12.5));
#124797=CARTESIAN_POINT('',(16.0005576038968,39.1384565378295,12.5));
#124798=CARTESIAN_POINT('',(18.7487692036153,34.9354049997927,12.5));
#124799=CARTESIAN_POINT('Origin',(16.0005576038968,36.1384565378295,12.5));
#124800=CARTESIAN_POINT('',(18.8102317482459,34.6121306821786,12.1018952060707));
#124801=CARTESIAN_POINT('Ctrl Pts',(18.7487692036153,34.9354049997927,12.5));
#124802=CARTESIAN_POINT('Ctrl Pts',(18.7487692036153,34.9354049997927,12.4925693313125));
#124803=CARTESIAN_POINT('Ctrl Pts',(18.7488325727708,34.9351366584889,12.4851148185871));
#124804=CARTESIAN_POINT('Ctrl Pts',(18.7496493679601,34.9316726928111,12.4373510176214));
#124805=CARTESIAN_POINT('Ctrl Pts',(18.7521896867423,34.9209617311555,12.3986190308672));
#124806=CARTESIAN_POINT('Ctrl Pts',(18.7608243220101,34.8829189971679,12.3169287768681));
#124807=CARTESIAN_POINT('Ctrl Pts',(18.7674427690982,34.8528745889928,12.2764946297254));
#124808=CARTESIAN_POINT('Ctrl Pts',(18.7843111831675,34.7695460947143,12.1921413513201));
#124809=CARTESIAN_POINT('Ctrl Pts',(18.7958798298391,34.7075933830526,12.1486504715916));
#124810=CARTESIAN_POINT('Ctrl Pts',(18.8080435840964,34.6270726442891,12.1088851897267));
#124811=CARTESIAN_POINT('Ctrl Pts',(18.8091452024147,34.6196302443412,12.1053410081124));
#124812=CARTESIAN_POINT('Ctrl Pts',(18.8102317482459,34.6121306821786,12.1018952060707));
#124813=CARTESIAN_POINT('',(18.8659495144705,34.1285985331886,12.));
#124814=CARTESIAN_POINT('Ctrl Pts',(18.8102317482459,34.6121306821786,12.1018952060707));
#124815=CARTESIAN_POINT('Ctrl Pts',(18.8197580197198,34.5463784027596,12.0716841972469));
#124816=CARTESIAN_POINT('Ctrl Pts',(18.8290172715136,34.4764705394863,12.048491997422));
#124817=CARTESIAN_POINT('Ctrl Pts',(18.8479915815834,34.31719649263,12.0111952320961));
#124818=CARTESIAN_POINT('Ctrl Pts',(18.8575097279275,34.2249443613316,12.0003779495169));
#124819=CARTESIAN_POINT('Ctrl Pts',(18.8656685711657,34.1318199562489,12.0000032434225));
#124820=CARTESIAN_POINT('Ctrl Pts',(18.8658092567013,34.1302092609521,12.));
#124821=CARTESIAN_POINT('Ctrl Pts',(18.8659495144705,34.1285985331886,12.));
#124822=CARTESIAN_POINT('',(15.5005576038968,39.6025581529673,12.));
#124823=CARTESIAN_POINT('Origin',(16.0005576038968,36.1384565378295,12.));
#124824=CARTESIAN_POINT('Ctrl Pts',(15.5005576038968,39.6025581529673,12.));
#124825=CARTESIAN_POINT('Ctrl Pts',(15.5016040980935,39.601651862408,12.));
#124826=CARTESIAN_POINT('Ctrl Pts',(15.5026504179355,39.6007453671807,12.0000032854501));
#124827=CARTESIAN_POINT('Ctrl Pts',(15.5265850871382,39.5800010504138,12.0001535475902));
#124828=CARTESIAN_POINT('Ctrl Pts',(15.5494014043324,39.5600546907341,12.0018685097915));
#124829=CARTESIAN_POINT('Ctrl Pts',(15.6559105390839,39.4661224630977,12.0172417791965));
#124830=CARTESIAN_POINT('Ctrl Pts',(15.7346031370174,39.394165582834,12.050368093961));
#124831=CARTESIAN_POINT('Ctrl Pts',(15.8547587133248,39.2812778115798,12.1407858340455));
#124832=CARTESIAN_POINT('Ctrl Pts',(15.8995456863726,39.2379968757629,12.1913094880829));
#124833=CARTESIAN_POINT('Ctrl Pts',(15.9585903602516,39.1802363196783,12.2931553699351));
#124834=CARTESIAN_POINT('Ctrl Pts',(15.9783903787479,39.1605638455604,12.3427321807669));
#124835=CARTESIAN_POINT('Ctrl Pts',(15.9969160291529,39.1421042769301,12.4305871755405));
#124836=CARTESIAN_POINT('Ctrl Pts',(16.0005576038968,39.1384565378295,12.4651445835938));
#124837=CARTESIAN_POINT('Ctrl Pts',(16.0005576038968,39.1384565378295,12.5));
#124838=CARTESIAN_POINT('Origin',(15.5005576038968,36.3806823573572,12.5));
#124839=CARTESIAN_POINT('',(15.5005576038968,36.3806823573572,12.));
#124840=CARTESIAN_POINT('',(16.0005576038968,44.6304565378295,12.5));
#124841=CARTESIAN_POINT('Origin',(15.5005576038968,44.6304565378295,12.5));
#124842=CARTESIAN_POINT('',(16.0005576038968,36.3806823573572,12.5));
#124843=CARTESIAN_POINT('Origin',(15.5005576038968,44.6304565378295,12.5));
#124844=CARTESIAN_POINT('Origin',(15.5005576038968,44.6304565378295,12.5));
#124845=CARTESIAN_POINT('Origin',(-18.3067027565145,34.6883503685105,12.5));
#124846=CARTESIAN_POINT('',(-24.1818223222136,28.8136502290417,12.));
#124847=CARTESIAN_POINT('',(-18.3067027565145,34.6883503685105,12.));
#124848=CARTESIAN_POINT('Origin',(-24.1818223222136,28.8136502290417,12.5));
#124849=CARTESIAN_POINT('Origin',(-18.5961864812216,34.3988873101177,12.5));
#124850=CARTESIAN_POINT('Origin',(-0.000328393418778106,28.1309081768848,
12.));
#124851=CARTESIAN_POINT('',(24.1817610214557,28.8127870262033,12.));
#124852=CARTESIAN_POINT('',(15.5139901477705,37.4805578998886,12.));
#124853=CARTESIAN_POINT('',(25.4997805061163,25.6308065108639,12.));
#124854=CARTESIAN_POINT('Origin',(20.9997805061163,25.6308065108639,12.));
#124855=CARTESIAN_POINT('',(25.4997805061163,12.1308065108639,12.));
#124856=CARTESIAN_POINT('',(25.4997805061163,26.8808573438743,12.));
#124857=CARTESIAN_POINT('',(24.9997805061163,11.6308065108639,12.));
#124858=CARTESIAN_POINT('Origin',(24.9997805061163,12.1308065108639,12.));
#124859=CARTESIAN_POINT('',(20.7068872873028,11.6308065108639,12.));
#124860=CARTESIAN_POINT('',(12.4997260563488,11.6308065108639,12.));
#124861=CARTESIAN_POINT('',(19.5000070232196,12.8376867749471,12.));
#124862=CARTESIAN_POINT('',(11.4782812553205,20.8594125428461,12.));
#124863=CARTESIAN_POINT('',(19.5000070232196,21.8015799937605,12.));
#124864=CARTESIAN_POINT('',(19.5000070232196,20.3807440853227,12.));
#124865=CARTESIAN_POINT('',(18.7042143673984,23.1260013830489,12.));
#124866=CARTESIAN_POINT('Origin',(18.0000070232196,21.8015799937605,12.));
#124867=CARTESIAN_POINT('',(15.8746640014216,24.6305,12.));
#124868=CARTESIAN_POINT('',(10.3759028387591,27.5542431726415,12.));
#124869=CARTESIAN_POINT('',(12.,24.6305,12.));
#124870=CARTESIAN_POINT('',(7.87483580329061,24.6305,12.));
#124871=CARTESIAN_POINT('',(-12.0002195251968,24.6309283607631,12.));
#124872=CARTESIAN_POINT('',(5.99980902926158,24.6306070926795,12.));
#124873=CARTESIAN_POINT('',(-15.8748746000505,24.631066672069,12.));
#124874=CARTESIAN_POINT('',(-6.00033197323811,24.630714186474,12.));
#124875=CARTESIAN_POINT('',(-18.7044786694047,23.12666906083,12.));
#124876=CARTESIAN_POINT('',(-9.01646660547503,28.2774328600768,12.));
#124877=CARTESIAN_POINT('',(-19.5003186017906,21.8022760793161,12.));
#124878=CARTESIAN_POINT('Origin',(-18.0003186027463,21.8022225347204,12.));
#124879=CARTESIAN_POINT('',(-19.5006385804826,12.8383828662136,12.));
#124880=CARTESIAN_POINT('',(-19.5002056346847,24.9669401637651,12.));
#124881=CARTESIAN_POINT('',(-20.707561925074,11.6315456841765,12.));
#124882=CARTESIAN_POINT('',(-10.7288557519193,21.609539475044,12.));
#124883=CARTESIAN_POINT('',(-25.0004551411524,11.6316989249976,12.));
#124884=CARTESIAN_POINT('',(-10.2506862658096,11.6311724113903,12.));
#124885=CARTESIAN_POINT('',(-25.5004372926353,12.1317167728775,12.));
#124886=CARTESIAN_POINT('Origin',(-25.0004372929538,12.131698924679,12.));
#124887=CARTESIAN_POINT('',(-25.4999553912744,25.6317167642765,12.));
#124888=CARTESIAN_POINT('',(-25.5001517196441,20.1317675956942,12.));
#124889=CARTESIAN_POINT('Origin',(-20.9999553941414,25.6315561304895,12.));
#124890=CARTESIAN_POINT('Origin',(15.5139901477705,37.4805578998886,12.5));
#124891=CARTESIAN_POINT('',(18.9498779474565,34.7517768813891,12.5));
#124892=CARTESIAN_POINT('Origin',(18.5963245568632,34.3982234907959,12.5));
#124893=CARTESIAN_POINT('',(24.535314412049,29.1663404167966,12.5));
#124894=CARTESIAN_POINT('',(15.8675435383638,37.8341112904819,12.5));
#124895=CARTESIAN_POINT('Origin',(24.1817610214557,28.8127870262033,12.5));
#124896=CARTESIAN_POINT('Origin',(16.8285576038968,32.6304565378295,12.5));
#124897=CARTESIAN_POINT('Origin',(16.8285576038968,32.6304565378295,12.5));
#124898=CARTESIAN_POINT('Origin',(-10.2506862658096,11.6311724113903,12.5));
#124899=CARTESIAN_POINT('Origin',(-25.0004551411524,11.6316989249976,12.5));
#124900=CARTESIAN_POINT('Origin',(-20.707561925074,11.6315456841765,12.5));
#124901=CARTESIAN_POINT('Ctrl Pts',(-25.0004729893509,11.1316989253161,
12.5000000000001));
#124902=CARTESIAN_POINT('Ctrl Pts',(-26.0004729887137,11.1317346217133,
12.5000000000001));
#124903=CARTESIAN_POINT('Ctrl Pts',(-26.0004372923167,12.1317346210761,
12.5));
#124904=CARTESIAN_POINT('Ctrl Pts',(-25.0004729893509,11.131698925316,11.9999999999999));
#124905=CARTESIAN_POINT('Ctrl Pts',(-26.0004729887137,11.1317346217132,
12.));
#124906=CARTESIAN_POINT('Ctrl Pts',(-26.0004372923168,12.131734621076,11.9999999999999));
#124907=CARTESIAN_POINT('Ctrl Pts',(-25.0004551411523,11.6316989249976,
12.));
#124908=CARTESIAN_POINT('Ctrl Pts',(-25.5004551408337,11.6317167731962,
12.));
#124909=CARTESIAN_POINT('Ctrl Pts',(-25.5004372926352,12.1317167728776,
12.));
#124910=CARTESIAN_POINT('Origin',(-25.5004372926353,12.1317167728775,12.5));
#124911=CARTESIAN_POINT('Origin',(-25.5001517196441,20.1317675956942,12.5));
#124912=CARTESIAN_POINT('Origin',(-25.4999553912744,25.6317167642765,12.5));
#124913=CARTESIAN_POINT('Origin',(-20.9999553941414,25.6315561304895,12.5));
#124914=CARTESIAN_POINT('Origin',(-16.8284826322926,32.6310572553665,12.5));
#124915=CARTESIAN_POINT('Origin',(-10.7288557519193,21.609539475044,12.5));
#124916=CARTESIAN_POINT('Origin',(-19.5006385804826,12.8383828662136,12.5));
#124917=CARTESIAN_POINT('Origin',(-9.01646660547503,28.2774328600768,12.5));
#124918=CARTESIAN_POINT('Origin',(-18.7044786694047,23.12666906083,12.5));
#124919=CARTESIAN_POINT('Origin',(-15.8748746000505,24.631066672069,12.5));
#124920=CARTESIAN_POINT('Origin',(-18.0003186027463,21.8022225347204,12.5));
#124921=CARTESIAN_POINT('Origin',(-19.5003186017906,21.8022760793161,12.5));
#124922=CARTESIAN_POINT('Origin',(-19.5002056346847,24.9669401637651,12.5));
#124923=CARTESIAN_POINT('Origin',(7.87483580329061,24.6305,12.5));
#124924=CARTESIAN_POINT('',(15.75,24.1305,12.5));
#124925=CARTESIAN_POINT('',(12.,24.1305,12.5));
#124926=CARTESIAN_POINT('',(7.87483580329061,24.1305,12.5));
#124927=CARTESIAN_POINT('Origin',(12.,24.6305,12.5));
#124928=CARTESIAN_POINT('Origin',(15.8746640014216,24.6305,12.5));
#124929=CARTESIAN_POINT('Origin',(5.99980902926158,24.6306070926795,12.5));
#124930=CARTESIAN_POINT('',(-12.0002284492961,24.1309283608428,12.5));
#124931=CARTESIAN_POINT('Origin',(-12.0002195251968,24.6309283607631,12.5));
#124932=CARTESIAN_POINT('',(5.9998001051623,24.1306070927591,12.5));
#124933=CARTESIAN_POINT('Origin',(-6.00033197323811,24.630714186474,12.5));
#124934=CARTESIAN_POINT('',(-6.00034982143666,24.1307141867926,12.5));
#124935=CARTESIAN_POINT('Origin',(19.5000070232196,20.3807440853227,12.5));
#124936=CARTESIAN_POINT('',(19.0000070232196,12.6305799937605,12.5));
#124937=CARTESIAN_POINT('',(19.0000070232196,21.8015799937605,12.5));
#124938=CARTESIAN_POINT('',(19.0000070232196,20.3807440853227,12.5));
#124939=CARTESIAN_POINT('Origin',(19.5000070232196,21.8015799937605,12.5));
#124940=CARTESIAN_POINT('Origin',(19.5000070232196,12.8376867749471,12.5));
#124941=CARTESIAN_POINT('Origin',(18.0000070232196,21.8015799937605,12.5));
#124942=CARTESIAN_POINT('',(18.4694785860055,22.6845275866195,12.5));
#124943=CARTESIAN_POINT('Origin',(18.7042143673984,23.1260013830489,12.5));
#124944=CARTESIAN_POINT('Origin',(18.0000070232196,21.8015799937605,12.5));
#124945=CARTESIAN_POINT('Origin',(10.3759028387591,27.5542431726415,12.5));
#124946=CARTESIAN_POINT('',(10.1411670573662,27.112769376212,12.5));
#124947=CARTESIAN_POINT('Origin',(11.4782812553205,20.8594125428461,12.5));
#124948=CARTESIAN_POINT('',(20.4997805061163,11.1308065108639,12.5));
#124949=CARTESIAN_POINT('',(11.1247278647273,20.5058591522529,12.5));
#124950=CARTESIAN_POINT('Origin',(20.7068872873028,11.6308065108639,12.5));
#124951=CARTESIAN_POINT('Origin',(20.9997805061163,25.6308065108639,12.5));
#124952=CARTESIAN_POINT('',(25.9997805061163,25.6308065108639,12.5));
#124953=CARTESIAN_POINT('Origin',(25.4997805061163,25.6308065108639,12.5));
#124954=CARTESIAN_POINT('Origin',(20.9997805061163,25.6308065108639,12.5));
#124955=CARTESIAN_POINT('Origin',(25.4997805061163,26.8808573438743,12.5));
#124956=CARTESIAN_POINT('',(25.9997805061163,12.1308065108639,12.5));
#124957=CARTESIAN_POINT('Origin',(25.4997805061163,12.1308065108639,12.5));
#124958=CARTESIAN_POINT('',(25.9997805061163,26.8808573438743,12.5));
#124959=CARTESIAN_POINT('Ctrl Pts',(25.9997805061163,12.1308065108639,12.5));
#124960=CARTESIAN_POINT('Ctrl Pts',(25.9997805061163,11.1308065108639,12.5));
#124961=CARTESIAN_POINT('Ctrl Pts',(24.9997805061163,11.1308065108639,12.5));
#124962=CARTESIAN_POINT('Ctrl Pts',(25.9997805061163,12.1308065108639,12.));
#124963=CARTESIAN_POINT('Ctrl Pts',(25.9997805061163,11.1308065108639,12.));
#124964=CARTESIAN_POINT('Ctrl Pts',(24.9997805061163,11.1308065108639,12.));
#124965=CARTESIAN_POINT('Ctrl Pts',(25.4997805061163,12.1308065108639,12.));
#124966=CARTESIAN_POINT('Ctrl Pts',(25.4997805061163,11.6308065108639,12.));
#124967=CARTESIAN_POINT('Ctrl Pts',(24.9997805061163,11.6308065108639,12.));
#124968=CARTESIAN_POINT('',(24.9997805061163,11.1308065108639,12.5));
#124969=CARTESIAN_POINT('Origin',(24.9997805061163,11.6308065108639,12.5));
#124970=CARTESIAN_POINT('Origin',(24.9997805061163,12.1308065108639,12.5));
#124971=CARTESIAN_POINT('Origin',(12.4997260563488,11.6308065108639,12.5));
#124972=CARTESIAN_POINT('',(12.4997260563488,11.1308065108639,12.5));
#124973=CARTESIAN_POINT('Origin',(-12.0002284492961,24.1309283608428,26.));
#124974=CARTESIAN_POINT('',(-12.0002284492961,24.1309283608428,26.));
#124975=CARTESIAN_POINT('Origin',(12.,24.1305,26.));
#124976=CARTESIAN_POINT('',(12.,24.1305,26.));
#124977=CARTESIAN_POINT('Origin',(15.75,24.1305,26.));
#124978=CARTESIAN_POINT('',(15.75,24.1305,26.));
#124979=CARTESIAN_POINT('Origin',(18.4694785860055,22.6845275866195,26.));
#124980=CARTESIAN_POINT('',(18.4694785860055,22.6845275866195,26.));
#124981=CARTESIAN_POINT('Origin',(18.0000070232196,21.8015799937605,26.));
#124982=CARTESIAN_POINT('',(19.0000070232196,21.8015799937605,26.));
#124983=CARTESIAN_POINT('Origin',(19.0000070232196,12.6305799937605,26.));
#124984=CARTESIAN_POINT('',(19.0000070232196,12.6305799937605,26.));
#124985=CARTESIAN_POINT('Origin',(20.4997805061163,11.1308065108639,26.));
#124986=CARTESIAN_POINT('',(20.4997805061163,11.1308065108639,26.));
#124987=CARTESIAN_POINT('Origin',(24.9997805061163,11.1308065108639,26.));
#124988=CARTESIAN_POINT('',(24.9997805061163,11.1308065108639,26.));
#124989=CARTESIAN_POINT('Origin',(24.9997805061163,12.1308065108639,26.));
#124990=CARTESIAN_POINT('',(25.9997805061163,12.1308065108639,26.));
#124991=CARTESIAN_POINT('Origin',(25.9997805061163,25.6308065108639,26.));
#124992=CARTESIAN_POINT('',(25.9997805061163,25.6308065108639,26.));
#124993=CARTESIAN_POINT('Origin',(20.9997805061163,25.6308065108639,26.));
#124994=CARTESIAN_POINT('',(24.535314412049,29.1663404167966,26.));
#124995=CARTESIAN_POINT('Origin',(18.9498779474565,34.7517768813891,26.));
#124996=CARTESIAN_POINT('',(18.9498779474565,34.7517768813891,26.));
#124997=CARTESIAN_POINT('Origin',(16.8285576038968,32.6304565378295,26.));
#124998=CARTESIAN_POINT('',(18.7487692036153,34.9354049997927,15.));
#124999=CARTESIAN_POINT('',(18.7487692036153,34.9354049997927,12.));
#125000=CARTESIAN_POINT('',(16.8285576038968,35.6304565378295,15.));
#125001=CARTESIAN_POINT('Origin',(16.8285576038968,32.6304565378295,15.));
#125002=CARTESIAN_POINT('',(16.8285576038968,35.6304565378295,26.));
#125003=CARTESIAN_POINT('Origin',(16.0005576038968,36.1384565378295,12.));
#125004=CARTESIAN_POINT('',(16.0005576038968,39.1384565378295,15.));
#125005=CARTESIAN_POINT('',(16.0005576038968,39.1384565378295,12.));
#125006=CARTESIAN_POINT('Origin',(16.0005576038968,36.1384565378295,15.));
#125007=CARTESIAN_POINT('Origin',(-16.0003574098591,36.1390276965147,12.));
#125008=CARTESIAN_POINT('Origin',(-16.0003574098591,36.1390276965147,15.));
#125009=CARTESIAN_POINT('Origin',(-15.8744846811456,36.139027695559,15.));
#125010=CARTESIAN_POINT('Origin',(15.8746634037561,36.1384565378295,15.));
#125011=CARTESIAN_POINT('',(16.5085576038968,35.6304565378295,15.));
#125012=CARTESIAN_POINT('',(16.1916105038265,35.6304565378295,15.));
#125013=CARTESIAN_POINT('',(16.0005576038968,36.1384565378295,15.));
#125014=CARTESIAN_POINT('',(16.0005576038968,40.3844565378295,15.));
#125015=CARTESIAN_POINT('Origin',(16.5085576038968,36.1384565378295,15.));
#125016=CARTESIAN_POINT('Origin',(16.5085576038968,35.6304565378295,26.));
#125017=CARTESIAN_POINT('',(16.5085576038968,35.6304565378295,26.));
#125018=CARTESIAN_POINT('Origin',(16.5085576038968,36.1384565378295,26.));
#125019=CARTESIAN_POINT('',(16.0005576038968,36.1384565378295,26.));
#125020=CARTESIAN_POINT('Origin',(16.0005576038968,44.6304565378295,26.));
#125021=CARTESIAN_POINT('',(16.0005576038968,44.6304565378295,26.));
#125022=CARTESIAN_POINT('Origin',(15.5005576038968,44.6304565378295,26.));
#125023=CARTESIAN_POINT('',(0.,0.,0.));
#125024=CARTESIAN_POINT('Origin',(25.9997814655409,18.8808065108639,-21.5));
#125025=CARTESIAN_POINT('',(25.9997805061207,18.8808065108639,-18.5));
#125026=CARTESIAN_POINT('Origin',(25.9997805061207,18.8808065108639,-21.5));
#125027=CARTESIAN_POINT('',(22.9997814655409,18.8808065108619,-18.5));
#125028=CARTESIAN_POINT('',(25.9997814655409,18.8808065108639,-18.5));
#125029=CARTESIAN_POINT('Origin',(22.9997814655409,18.8808065108619,-21.5));
#125030=CARTESIAN_POINT('Origin',(22.9997814655409,18.8808065108619,-21.5));
#125031=CARTESIAN_POINT('Origin',(-26.0001963416363,18.8817346167756,-21.5));
#125032=CARTESIAN_POINT('',(-23.0001963435476,18.8816275275843,-18.5));
#125033=CARTESIAN_POINT('Origin',(-23.0001963435476,18.8816275275843,-21.5));
#125034=CARTESIAN_POINT('',(-26.0001963416363,18.8817346167756,-18.5));
#125035=CARTESIAN_POINT('',(-26.0001963416363,18.8817346167756,-18.5));
#125036=CARTESIAN_POINT('Origin',(-26.0001963416363,18.8817346167756,-21.5));
#125037=CARTESIAN_POINT('Origin',(-23.0001963435476,18.8816275275843,-21.5));
#125038=CARTESIAN_POINT('Origin',(-6.00033197323811,24.630714186474,-25.5));
#125039=CARTESIAN_POINT('',(-15.7502284469069,24.1310622223319,-25.5));
#125040=CARTESIAN_POINT('',(-12.0002284492961,24.1309283608428,-25.5));
#125041=CARTESIAN_POINT('',(-6.00034982143666,24.1307141867926,-25.5));
#125042=CARTESIAN_POINT('',(-15.8748746000505,24.631066672069,-26.));
#125043=CARTESIAN_POINT('Origin',(-15.8748746000505,24.631066672069,-25.5));
#125044=CARTESIAN_POINT('',(-12.0002106010975,24.6309283605242,-26.));
#125045=CARTESIAN_POINT('',(-6.00033197323811,24.630714186474,-26.));
#125046=CARTESIAN_POINT('Origin',(-12.0002106010975,24.6309283605242,-25.5));
#125047=CARTESIAN_POINT('Origin',(5.99980902926158,24.6306070926795,-25.5));
#125048=CARTESIAN_POINT('',(12.0000089240993,24.6304999999204,-26.));
#125049=CARTESIAN_POINT('',(5.99980902926158,24.6306070926795,-26.));
#125050=CARTESIAN_POINT('',(12.,24.1305,-25.5));
#125051=CARTESIAN_POINT('Origin',(12.0000089240993,24.6304999999204,-25.5));
#125052=CARTESIAN_POINT('',(5.9998001051623,24.1306070927591,-25.5));
#125053=CARTESIAN_POINT('Origin',(15.5005576038968,36.3806823573572,-25.5));
#125054=CARTESIAN_POINT('',(16.0005576038968,44.6304565378295,-25.5));
#125055=CARTESIAN_POINT('',(15.5005576038968,44.6304565378295,-26.));
#125056=CARTESIAN_POINT('Origin',(15.5005576038968,44.6304565378295,-25.5));
#125057=CARTESIAN_POINT('',(16.0005576038968,36.1384565378295,-25.5));
#125058=CARTESIAN_POINT('',(16.0005576038968,36.3806823573572,-25.5));
#125059=CARTESIAN_POINT('',(15.5005576038968,36.1384565378295,-26.));
#125060=CARTESIAN_POINT('Origin',(15.5005576038968,36.1384565378295,-25.5));
#125061=CARTESIAN_POINT('',(15.5005576038968,36.3806823573572,-26.));
#125062=CARTESIAN_POINT('Origin',(16.5085576038968,36.1384565378295,-25.5));
#125063=CARTESIAN_POINT('',(16.5085576038968,35.1304565378295,-26.));
#125064=CARTESIAN_POINT('',(16.5085576038968,35.6304565378295,-25.5));
#125065=CARTESIAN_POINT('Origin',(16.5085576038968,35.1304565378295,-25.5));
#125066=CARTESIAN_POINT('Origin',(16.5085576038968,36.1384565378295,-26.));
#125067=CARTESIAN_POINT('Origin',(16.5085576038968,36.1384565378295,-25.5));
#125068=CARTESIAN_POINT('Origin',(8.25411460523903,35.1304565378295,-25.5));
#125069=CARTESIAN_POINT('',(16.8285576038968,35.1304565378295,-26.));
#125070=CARTESIAN_POINT('',(16.8285576038968,35.6304565378295,-25.5));
#125071=CARTESIAN_POINT('Origin',(16.8285576038968,35.1304565378295,-25.5));
#125072=CARTESIAN_POINT('',(8.25411460523903,35.1304565378295,-26.));
#125073=CARTESIAN_POINT('',(8.25411460523903,35.6304565378295,-25.5));
#125074=CARTESIAN_POINT('Origin',(16.8285576038968,32.6304565378295,-25.5));
#125075=CARTESIAN_POINT('',(18.5963245568632,34.3982234907959,-26.));
#125076=CARTESIAN_POINT('',(18.9498779474565,34.7517768813891,-25.5));
#125077=CARTESIAN_POINT('Origin',(18.5963245568632,34.3982234907959,-25.5));
#125078=CARTESIAN_POINT('Origin',(16.8285576038968,32.6304565378295,-26.));
#125079=CARTESIAN_POINT('Origin',(16.8285576038968,32.6304565378295,-25.5));
#125080=CARTESIAN_POINT('Origin',(15.5139901477705,37.4805578998886,-25.5));
#125081=CARTESIAN_POINT('',(24.1817610214557,28.8127870262033,-26.));
#125082=CARTESIAN_POINT('',(24.535314412049,29.1663404167966,-25.5));
#125083=CARTESIAN_POINT('Origin',(24.1817610214557,28.8127870262033,-25.5));
#125084=CARTESIAN_POINT('',(15.5139901477705,37.4805578998886,-26.));
#125085=CARTESIAN_POINT('',(15.8675435383638,37.8341112904819,-25.5));
#125086=CARTESIAN_POINT('Origin',(20.9997805061163,25.6308065108639,-25.5));
#125087=CARTESIAN_POINT('',(25.4997805061163,25.6308065108639,-26.));
#125088=CARTESIAN_POINT('',(25.9997805061163,25.6308065108639,-25.5));
#125089=CARTESIAN_POINT('Origin',(25.4997805061163,25.6308065108639,-25.5));
#125090=CARTESIAN_POINT('Origin',(20.9997805061163,25.6308065108639,-26.));
#125091=CARTESIAN_POINT('Origin',(20.9997805061163,25.6308065108639,-25.5));
#125092=CARTESIAN_POINT('Origin',(25.4997805061163,26.8808573438743,-25.5));
#125093=CARTESIAN_POINT('',(25.4997805061163,12.1308065108639,-26.));
#125094=CARTESIAN_POINT('',(25.9997805061163,12.1308065108639,-25.5));
#125095=CARTESIAN_POINT('Origin',(25.4997805061163,12.1308065108639,-25.5));
#125096=CARTESIAN_POINT('',(25.4997805061163,26.8808573438743,-26.));
#125097=CARTESIAN_POINT('',(25.9997805061163,26.8808573438743,-25.5));
#125098=CARTESIAN_POINT('Ctrl Pts',(25.9997805061163,12.1308065108638,-25.5));
#125099=CARTESIAN_POINT('Ctrl Pts',(25.9997805061164,11.1308065108638,-25.5));
#125100=CARTESIAN_POINT('Ctrl Pts',(24.9997805061164,11.1308065108639,-25.5));
#125101=CARTESIAN_POINT('Ctrl Pts',(25.9997805061163,12.1308065108638,-26.));
#125102=CARTESIAN_POINT('Ctrl Pts',(25.9997805061164,11.1308065108638,-26.));
#125103=CARTESIAN_POINT('Ctrl Pts',(24.9997805061164,11.1308065108639,-26.));
#125104=CARTESIAN_POINT('Ctrl Pts',(25.4997805061163,12.1308065108638,-26.));
#125105=CARTESIAN_POINT('Ctrl Pts',(25.4997805061163,11.6308065108639,-26.));
#125106=CARTESIAN_POINT('Ctrl Pts',(24.9997805061164,11.630806510864,-26.));
#125107=CARTESIAN_POINT('',(24.9997805061163,11.6308065108639,-26.));
#125108=CARTESIAN_POINT('',(24.9997805061163,11.1308065108639,-25.5));
#125109=CARTESIAN_POINT('Origin',(24.9997805061163,11.6308065108639,-25.5));
#125110=CARTESIAN_POINT('Origin',(24.9997805061163,12.1308065108639,-26.));
#125111=CARTESIAN_POINT('Origin',(24.9997805061163,12.1308065108639,-25.5));
#125112=CARTESIAN_POINT('Origin',(12.4997260563488,11.6308065108639,-25.5));
#125113=CARTESIAN_POINT('',(20.4997805061163,11.1308065108639,-25.5));
#125114=CARTESIAN_POINT('',(12.4997260563488,11.1308065108639,-25.5));
#125115=CARTESIAN_POINT('',(20.7068872873028,11.6308065108639,-26.));
#125116=CARTESIAN_POINT('Origin',(20.7068872873028,11.6308065108639,-25.5));
#125117=CARTESIAN_POINT('',(12.4997260563488,11.6308065108639,-26.));
#125118=CARTESIAN_POINT('Origin',(11.4782812553205,20.8594125428461,-25.5));
#125119=CARTESIAN_POINT('',(19.0000070232196,12.6305799937605,-25.5));
#125120=CARTESIAN_POINT('',(11.1247278647273,20.5058591522529,-25.5));
#125121=CARTESIAN_POINT('',(19.5000070232196,12.8376867749471,-26.));
#125122=CARTESIAN_POINT('Origin',(19.5000070232196,12.8376867749471,-25.5));
#125123=CARTESIAN_POINT('',(11.4782812553205,20.8594125428461,-26.));
#125124=CARTESIAN_POINT('Origin',(19.5000070232196,20.3807440853227,-25.5));
#125125=CARTESIAN_POINT('',(19.5000070232196,21.8015799937605,-26.));
#125126=CARTESIAN_POINT('',(19.5000070232196,20.3807440853227,-26.));
#125127=CARTESIAN_POINT('',(19.0000070232196,21.8015799937605,-25.5));
#125128=CARTESIAN_POINT('',(19.0000070232196,20.3807440853227,-25.5));
#125129=CARTESIAN_POINT('Origin',(19.5000070232196,21.8015799937605,-25.5));
#125130=CARTESIAN_POINT('Origin',(18.0000070232196,21.8015799937605,-25.5));
#125131=CARTESIAN_POINT('',(18.7042143673984,23.1260013830489,-26.));
#125132=CARTESIAN_POINT('',(18.4694785860055,22.6845275866195,-25.5));
#125133=CARTESIAN_POINT('Origin',(18.7042143673984,23.1260013830489,-25.5));
#125134=CARTESIAN_POINT('Origin',(18.0000070232196,21.8015799937605,-26.));
#125135=CARTESIAN_POINT('Origin',(18.0000070232196,21.8015799937605,-25.5));
#125136=CARTESIAN_POINT('Origin',(10.3759028387591,27.5542431726415,-25.5));
#125137=CARTESIAN_POINT('',(15.75,24.1305,-25.5));
#125138=CARTESIAN_POINT('',(10.1411670573662,27.112769376212,-25.5));
#125139=CARTESIAN_POINT('',(15.8746640014216,24.6305,-26.));
#125140=CARTESIAN_POINT('Origin',(15.8746640014216,24.6305,-25.5));
#125141=CARTESIAN_POINT('',(10.3759028387591,27.5542431726415,-26.));
#125142=CARTESIAN_POINT('Origin',(7.87483580329061,24.6305,-25.5));
#125143=CARTESIAN_POINT('',(7.87483580329061,24.6305,-26.));
#125144=CARTESIAN_POINT('',(7.87483580329061,24.1305,-25.5));
#125145=CARTESIAN_POINT('Origin',(-9.01646660547503,28.2774328600768,-25.5));
#125146=CARTESIAN_POINT('',(-18.7044786694047,23.12666906083,-26.));
#125147=CARTESIAN_POINT('',(-9.01646660547503,28.2774328600768,-26.));
#125148=CARTESIAN_POINT('',(-18.4697586471852,22.6851868854601,-25.5));
#125149=CARTESIAN_POINT('',(-8.78174658325559,27.8359506847069,-25.5));
#125150=CARTESIAN_POINT('Origin',(-18.7044786694047,23.12666906083,-25.5));
#125151=CARTESIAN_POINT('Origin',(-18.0003186027463,21.8022225347204,-25.5));
#125152=CARTESIAN_POINT('',(-19.5003186017906,21.8022760793161,-26.));
#125153=CARTESIAN_POINT('',(-19.0003186021092,21.8022582311175,-25.5));
#125154=CARTESIAN_POINT('Origin',(-19.5003186017906,21.8022760793161,-25.5));
#125155=CARTESIAN_POINT('Origin',(-18.0003186027463,21.8022225347204,-26.));
#125156=CARTESIAN_POINT('Origin',(-18.0003186027463,21.8022225347204,-25.5));
#125157=CARTESIAN_POINT('Origin',(-19.5002056346847,24.9669401637651,-25.5));
#125158=CARTESIAN_POINT('',(-19.000645973767,12.6312582369605,-25.5));
#125159=CARTESIAN_POINT('',(-19.0002056350033,24.9669223155665,-25.5));
#125160=CARTESIAN_POINT('',(-19.5006385804826,12.8383828662136,-26.));
#125161=CARTESIAN_POINT('Origin',(-19.5006385804826,12.8383828662136,-25.5));
#125162=CARTESIAN_POINT('',(-19.5002056346847,24.9669401637651,-26.));
#125163=CARTESIAN_POINT('Origin',(-10.7288557519193,21.609539475044,-25.5));
#125164=CARTESIAN_POINT('',(-20.707561925074,11.6315456841765,-26.));
#125165=CARTESIAN_POINT('',(-10.7288557519193,21.609539475044,-26.));
#125166=CARTESIAN_POINT('',(-20.500472992218,11.1315382915292,-25.5));
#125167=CARTESIAN_POINT('',(-10.3753149821335,21.2559734640938,-25.5));
#125168=CARTESIAN_POINT('Origin',(-20.707561925074,11.6315456841765,-25.5));
#125169=CARTESIAN_POINT('Origin',(-10.2506862658096,11.6311724113903,-25.5));
#125170=CARTESIAN_POINT('',(-25.0004551411524,11.6316989249976,-26.));
#125171=CARTESIAN_POINT('',(-10.2506862658096,11.6311724113903,-26.));
#125172=CARTESIAN_POINT('',(-25.0004729893509,11.1316989253161,-25.5));
#125173=CARTESIAN_POINT('',(-10.2507041140081,11.1311724117089,-25.5));
#125174=CARTESIAN_POINT('Origin',(-25.0004551411524,11.6316989249976,-25.5));
#125175=CARTESIAN_POINT('Ctrl Pts',(-25.0004729893509,11.1316989253161,
-25.5));
#125176=CARTESIAN_POINT('Ctrl Pts',(-26.000472988714,11.131734621713,-25.5));
#125177=CARTESIAN_POINT('Ctrl Pts',(-26.0004372923167,12.1317346210762,
-25.5));
#125178=CARTESIAN_POINT('Ctrl Pts',(-25.0004729893508,11.1316989253161,
-26.));
#125179=CARTESIAN_POINT('Ctrl Pts',(-26.000472988714,11.131734621713,-26.0000000000001));
#125180=CARTESIAN_POINT('Ctrl Pts',(-26.0004372923167,12.1317346210762,
-26.));
#125181=CARTESIAN_POINT('Ctrl Pts',(-25.0004551411524,11.6316989249976,
-26.));
#125182=CARTESIAN_POINT('Ctrl Pts',(-25.5004551408338,11.6317167731961,
-26.));
#125183=CARTESIAN_POINT('Ctrl Pts',(-25.5004372926352,12.1317167728775,
-26.));
#125184=CARTESIAN_POINT('',(-25.5004372926353,12.1317167728775,-26.));
#125185=CARTESIAN_POINT('',(-26.0004372923167,12.1317346210761,-25.5));
#125186=CARTESIAN_POINT('Origin',(-25.5004372926353,12.1317167728775,-25.5));
#125187=CARTESIAN_POINT('Origin',(-25.0004372929538,12.131698924679,-26.));
#125188=CARTESIAN_POINT('Origin',(-25.0004372929538,12.131698924679,-25.5));
#125189=CARTESIAN_POINT('Origin',(-25.5001517196441,20.1317675956942,-25.5));
#125190=CARTESIAN_POINT('',(-25.4999553912744,25.6317167642765,-26.));
#125191=CARTESIAN_POINT('',(-25.9999553909559,25.631734612475,-25.5));
#125192=CARTESIAN_POINT('Origin',(-25.4999553912744,25.6317167642765,-25.5));
#125193=CARTESIAN_POINT('',(-25.5001517196441,20.1317675956942,-26.));
#125194=CARTESIAN_POINT('',(-26.0001517193255,20.1317854438928,-25.5));
#125195=CARTESIAN_POINT('Origin',(-20.9999553941414,25.6315561304895,-25.5));
#125196=CARTESIAN_POINT('',(-24.1818223222136,28.8136502290417,-26.));
#125197=CARTESIAN_POINT('',(-24.5353630919994,29.167216239992,-25.5));
#125198=CARTESIAN_POINT('Origin',(-24.1818223222136,28.8136502290417,-25.5));
#125199=CARTESIAN_POINT('Origin',(-20.9999553941414,25.6315561304895,-26.));
#125200=CARTESIAN_POINT('Origin',(-20.9999553941414,25.6315561304895,-25.5));
#125201=CARTESIAN_POINT('Origin',(-18.3067027565145,34.6883503685105,-25.5));
#125202=CARTESIAN_POINT('',(-18.5961864812216,34.3988873101177,-26.));
#125203=CARTESIAN_POINT('',(-18.9497272510074,34.7524533210679,-25.5));
#125204=CARTESIAN_POINT('Origin',(-18.5961864812216,34.3988873101177,-25.5));
#125205=CARTESIAN_POINT('',(-18.3067027565145,34.6883503685105,-26.));
#125206=CARTESIAN_POINT('',(-18.6602435263003,35.0419163794607,-25.5));
#125207=CARTESIAN_POINT('Origin',(-16.8284826322926,32.6310572553665,-25.5));
#125208=CARTESIAN_POINT('',(-16.8283933912999,35.1310572537737,-26.));
#125209=CARTESIAN_POINT('',(-16.8283755431013,35.6310572534551,-25.5));
#125210=CARTESIAN_POINT('Origin',(-16.8283933912999,35.1310572537737,-25.5));
#125211=CARTESIAN_POINT('Origin',(-16.8284826322926,32.6310572553665,-26.));
#125212=CARTESIAN_POINT('Origin',(-16.8284826322926,32.6310572553665,-25.5));
#125213=CARTESIAN_POINT('Origin',(-8.41423596303023,35.1307568986686,-25.5));
#125214=CARTESIAN_POINT('',(-16.5083933915038,35.1310458309266,-26.));
#125215=CARTESIAN_POINT('',(-16.5083755433052,35.631045830608,-25.5));
#125216=CARTESIAN_POINT('Origin',(-16.5083933915038,35.1310458309266,-25.5));
#125217=CARTESIAN_POINT('',(-8.41423596303023,35.1307568986686,-26.));
#125218=CARTESIAN_POINT('',(-8.41421811483168,35.6307568983501,-25.5));
#125219=CARTESIAN_POINT('Origin',(-16.5083574095355,36.1390458302844,-25.5));
#125220=CARTESIAN_POINT('',(-15.5003574101777,36.1390098483161,-26.));
#125221=CARTESIAN_POINT('',(-16.0003574098591,36.1390276965147,-25.5));
#125222=CARTESIAN_POINT('Origin',(-15.5003574101777,36.1390098483161,-25.5));
#125223=CARTESIAN_POINT('Origin',(-16.5083574095355,36.1390458302844,-26.));
#125224=CARTESIAN_POINT('Origin',(-16.5083574095355,36.1390458302844,-25.5));
#125225=CARTESIAN_POINT('Origin',(-15.5005003304909,32.1352356652978,-25.5));
#125226=CARTESIAN_POINT('',(-15.5000542763735,44.6310098429057,-26.));
#125227=CARTESIAN_POINT('',(-16.0000542760549,44.6310276911043,-25.5));
#125228=CARTESIAN_POINT('Origin',(-15.5000542763735,44.6310098429057,-25.5));
#125229=CARTESIAN_POINT('',(-15.5005003304909,32.1352356652978,-26.));
#125230=CARTESIAN_POINT('',(-16.0005003301724,32.1352535134963,-25.5));
#125231=CARTESIAN_POINT('Origin',(6.40011460523903,44.6304565378295,-25.5));
#125232=CARTESIAN_POINT('',(12.8005576038968,45.1304565378295,-25.5));
#125233=CARTESIAN_POINT('',(12.8005576038968,44.6304565378295,-26.));
#125234=CARTESIAN_POINT('Origin',(12.8005576038968,44.6304565378295,-25.5));
#125235=CARTESIAN_POINT('',(15.5005576038968,45.1304565378295,-25.5));
#125236=CARTESIAN_POINT('',(6.40011460523903,45.1304565378295,-25.5));
#125237=CARTESIAN_POINT('Origin',(15.5005576038968,44.6304565378295,-25.5));
#125238=CARTESIAN_POINT('',(6.40011460523903,44.6304565378295,-26.));
#125239=CARTESIAN_POINT('Origin',(-6.40003962806013,44.6307992338217,-25.5));
#125240=CARTESIAN_POINT('',(-12.8000453539944,44.6309134623946,-26.));
#125241=CARTESIAN_POINT('',(-6.40003962806013,44.6307992338217,-26.));
#125242=CARTESIAN_POINT('',(-12.8000364298952,45.130913462315,-25.5));
#125243=CARTESIAN_POINT('Origin',(-12.8000453539944,44.6309134623946,-25.5));
#125244=CARTESIAN_POINT('',(-6.40003070396085,45.130799233742,-25.5));
#125245=CARTESIAN_POINT('Origin',(-7.74989684768079,44.6307331902084,-25.5));
#125246=CARTESIAN_POINT('',(-7.74989684768079,44.6307331902084,-26.));
#125247=CARTESIAN_POINT('',(-15.5000364281749,45.1310098425872,-25.5));
#125248=CARTESIAN_POINT('Origin',(-15.5000542763735,44.6310098429057,-25.5));
#125249=CARTESIAN_POINT('',(-7.74987899948224,45.1307331898898,-25.5));
#125250=CARTESIAN_POINT('Origin',(-15.5000542763735,44.6310098429057,-25.5));
#125251=CARTESIAN_POINT('Origin',(-15.5000542763735,44.6310098429057,-25.5));
#125252=CARTESIAN_POINT('Origin',(15.5005576038968,44.6304565378295,-25.5));
#125253=CARTESIAN_POINT('Origin',(15.5005576038968,44.6304565378295,-25.5));
#125254=CARTESIAN_POINT('Origin',(-15.7502284469069,24.1310622223319,-26.));
#125255=CARTESIAN_POINT('',(-15.7502284469069,24.1310622223319,-12.5));
#125256=CARTESIAN_POINT('',(-15.7502284469069,24.1310622223319,-26.));
#125257=CARTESIAN_POINT('',(-18.4697586471852,22.6851868854601,-12.5));
#125258=CARTESIAN_POINT('',(-8.78174658325559,27.8359506847069,-12.5));
#125259=CARTESIAN_POINT('',(-18.4697586471852,22.6851868854601,-26.));
#125260=CARTESIAN_POINT('Origin',(-18.0003186027463,21.8022225347204,-26.));
#125261=CARTESIAN_POINT('',(-19.0003186021092,21.8022582311175,-12.5));
#125262=CARTESIAN_POINT('Origin',(-18.0003186027463,21.8022225347204,-12.5));
#125263=CARTESIAN_POINT('',(-19.0003186021092,21.8022582311175,-26.));
#125264=CARTESIAN_POINT('Origin',(-19.0003186021092,21.8022582311175,-26.));
#125265=CARTESIAN_POINT('',(-19.000645973767,12.6312582369605,-12.5));
#125266=CARTESIAN_POINT('',(-19.0002056350033,24.9669223155665,-12.5));
#125267=CARTESIAN_POINT('',(-19.000645973767,12.6312582369605,-26.));
#125268=CARTESIAN_POINT('Origin',(-19.000645973767,12.6312582369605,-26.));
#125269=CARTESIAN_POINT('',(-20.500472992218,11.1315382915292,-12.5));
#125270=CARTESIAN_POINT('',(-10.3753149821335,21.2559734640938,-12.5));
#125271=CARTESIAN_POINT('',(-20.500472992218,11.1315382915292,-26.));
#125272=CARTESIAN_POINT('Origin',(-20.500472992218,11.1315382915292,-26.));
#125273=CARTESIAN_POINT('',(-25.0004729893509,11.1316989253161,-12.5));
#125274=CARTESIAN_POINT('',(-10.2507041140081,11.1311724117089,-12.5));
#125275=CARTESIAN_POINT('',(-25.0004729893509,11.1316989253161,-26.));
#125276=CARTESIAN_POINT('Origin',(-25.0004372929538,12.131698924679,-26.));
#125277=CARTESIAN_POINT('',(-26.0004372923167,12.1317346210761,-12.5));
#125278=CARTESIAN_POINT('Origin',(-25.0004372929538,12.131698924679,-12.5));
#125279=CARTESIAN_POINT('',(-26.0004372923167,12.1317346210761,-26.));
#125280=CARTESIAN_POINT('Origin',(-26.0004372923167,12.1317346210761,-26.));
#125281=CARTESIAN_POINT('',(-25.9999553909559,25.631734612475,-12.5));
#125282=CARTESIAN_POINT('',(-26.0001517193255,20.1317854438928,-12.5));
#125283=CARTESIAN_POINT('',(-25.9999553909559,25.631734612475,-26.));
#125284=CARTESIAN_POINT('Origin',(-20.9999553941414,25.6315561304895,-26.));
#125285=CARTESIAN_POINT('',(-24.5353630919994,29.167216239992,-12.5));
#125286=CARTESIAN_POINT('Origin',(-20.9999553941414,25.6315561304895,-12.5));
#125287=CARTESIAN_POINT('',(-24.5353630919994,29.167216239992,-26.));
#125288=CARTESIAN_POINT('Origin',(-24.5353630919994,29.167216239992,-26.));
#125289=CARTESIAN_POINT('',(-18.9497272510074,34.7524533210679,-12.5));
#125290=CARTESIAN_POINT('',(-18.6602435263003,35.0419163794607,-12.5));
#125291=CARTESIAN_POINT('',(-18.9497272510074,34.7524533210679,-26.));
#125292=CARTESIAN_POINT('Origin',(-16.8284826322926,32.6310572553665,-26.));
#125293=CARTESIAN_POINT('',(-18.7486119524321,34.9360742604969,-12.5));
#125294=CARTESIAN_POINT('Origin',(-16.8284826322926,32.6310572553665,-12.5));
#125295=CARTESIAN_POINT('',(-18.7486119524321,34.9360742604969,-15.));
#125296=CARTESIAN_POINT('',(-18.7486119524321,34.9360742604969,-12.));
#125297=CARTESIAN_POINT('',(-16.8283755431013,35.6310572534551,-15.));
#125298=CARTESIAN_POINT('Origin',(-16.8284826322926,32.6310572553665,-15.));
#125299=CARTESIAN_POINT('',(-16.8283755431013,35.6310572534551,-26.));
#125300=CARTESIAN_POINT('Origin',(-16.8283755431013,35.6310572534551,-26.));
#125301=CARTESIAN_POINT('',(-16.5083755433052,35.631045830608,-15.));
#125302=CARTESIAN_POINT('',(-16.3514391790885,35.6310402285453,-15.));
#125303=CARTESIAN_POINT('',(-16.5083755433052,35.631045830608,-26.));
#125304=CARTESIAN_POINT('Origin',(-16.5083574095355,36.1390458302844,-26.));
#125305=CARTESIAN_POINT('',(-16.0003574098591,36.1390276965147,-15.));
#125306=CARTESIAN_POINT('Origin',(-16.5083574095355,36.1390458302844,-15.));
#125307=CARTESIAN_POINT('',(-16.0003574098591,36.1390276965147,-26.));
#125308=CARTESIAN_POINT('Origin',(-16.0003574098591,36.1390276965147,-26.));
#125309=CARTESIAN_POINT('',(-16.0002503206678,39.1390276946033,-15.));
#125310=CARTESIAN_POINT('',(-16.0003574097789,36.1390299426383,-15.));
#125311=CARTESIAN_POINT('',(-16.0002503206678,39.1390276946033,-12.5));
#125312=CARTESIAN_POINT('',(-16.0002503206678,39.1390276946033,-12.));
#125313=CARTESIAN_POINT('',(-16.0000542760549,44.6310276911043,-12.5));
#125314=CARTESIAN_POINT('',(-16.0005003301724,32.1352535134963,-12.5));
#125315=CARTESIAN_POINT('',(-16.0000542760549,44.6310276911043,-26.));
#125316=CARTESIAN_POINT('Origin',(-15.5000542763735,44.6310098429057,-26.));
#125317=CARTESIAN_POINT('',(-15.5000364281749,45.1310098425872,-12.5));
#125318=CARTESIAN_POINT('Origin',(-15.5000542763735,44.6310098429057,-12.5));
#125319=CARTESIAN_POINT('',(-15.5000364281749,45.1310098425872,-26.));
#125320=CARTESIAN_POINT('Origin',(-15.5000364281749,45.1310098425872,-26.));
#125321=CARTESIAN_POINT('',(-12.8000364298952,45.130913462315,-12.5));
#125322=CARTESIAN_POINT('',(-7.74987899948224,45.1307331898898,-12.5));
#125323=CARTESIAN_POINT('',(-12.8000364298952,45.130913462315,-26.));
#125324=CARTESIAN_POINT('Origin',(-12.8000364298952,45.130913462315,-26.));
#125325=CARTESIAN_POINT('',(12.8005576038968,45.1304565378295,-12.5));
#125326=CARTESIAN_POINT('',(-6.40003070396085,45.130799233742,-12.5));
#125327=CARTESIAN_POINT('',(12.8005576038968,45.1304565378295,-26.));
#125328=CARTESIAN_POINT('Origin',(12.8005576038968,45.1304565378295,-26.));
#125329=CARTESIAN_POINT('',(15.5005576038968,45.1304565378295,-12.5));
#125330=CARTESIAN_POINT('',(6.40011460523903,45.1304565378295,-12.5));
#125331=CARTESIAN_POINT('',(15.5005576038968,45.1304565378295,-26.));
#125332=CARTESIAN_POINT('Origin',(-0.000328393418778106,28.1309081768848,
-26.));
#125333=CARTESIAN_POINT('Origin',(-15.5005003304909,32.1352356652978,-12.5));
#125334=CARTESIAN_POINT('',(-15.5002337542308,39.6031114612468,-12.));
#125335=CARTESIAN_POINT('Ctrl Pts',(-15.5002337542308,39.6031114612469,
-12.));
#125336=CARTESIAN_POINT('Ctrl Pts',(-15.5012802807782,39.6022052080442,
-12.));
#125337=CARTESIAN_POINT('Ctrl Pts',(-15.5023266329781,39.6012987501675,
-12.0000032854501));
#125338=CARTESIAN_POINT('Ctrl Pts',(-15.5262620426631,39.580555287795,-12.0001535475902));
#125339=CARTESIAN_POINT('Ctrl Pts',(-15.549079071856,39.5606097425883,-12.0018685097915));
#125340=CARTESIAN_POINT('Ctrl Pts',(-15.6555915595815,39.4666813170044,
-12.0172417791965));
#125341=CARTESIAN_POINT('Ctrl Pts',(-15.7342867260662,39.3947272458287,
-12.0503680939609));
#125342=CARTESIAN_POINT('Ctrl Pts',(-15.8544463319837,39.2818437637677,
-12.1407858340455));
#125343=CARTESIAN_POINT('Ctrl Pts',(-15.8992348499764,39.2385644267119,
-12.1913094880828));
#125344=CARTESIAN_POINT('Ctrl Pts',(-15.9582815856617,39.1808059783461,
-12.2931553699351));
#125345=CARTESIAN_POINT('Ctrl Pts',(-15.9780823063818,39.1611342110301,
-12.3427321807669));
#125346=CARTESIAN_POINT('Ctrl Pts',(-15.996608615715,39.1426753037105,-12.4305871755405));
#125347=CARTESIAN_POINT('Ctrl Pts',(-16.0002503206678,39.1390276946034,
-12.4651445835938));
#125348=CARTESIAN_POINT('Ctrl Pts',(-16.0002503206678,39.1390276946034,
-12.5));
#125349=CARTESIAN_POINT('',(-15.5000542763735,44.6310098429057,-12.));
#125350=CARTESIAN_POINT('',(-15.5005003304909,32.1352356652978,-12.));
#125351=CARTESIAN_POINT('Origin',(-15.5000542763735,44.6310098429057,-12.5));
#125352=CARTESIAN_POINT('Origin',(-16.0003574098591,36.1390276965147,-12.5));
#125353=CARTESIAN_POINT('',(-18.8658210632966,34.1292719773217,-12.));
#125354=CARTESIAN_POINT('Origin',(-16.0003574098591,36.1390276965147,-12.));
#125355=CARTESIAN_POINT('Origin',(-16.0003574098591,36.1390276965147,-12.5));
#125356=CARTESIAN_POINT('',(-18.810086036752,34.6128021370802,-12.1018952060707));
#125357=CARTESIAN_POINT('Ctrl Pts',(-18.810086036752,34.6128021370802,-12.1018952060707));
#125358=CARTESIAN_POINT('Ctrl Pts',(-18.8089992232141,34.6203016604522,
-12.1053410081124));
#125359=CARTESIAN_POINT('Ctrl Pts',(-18.8078973392296,34.6277440210717,
-12.1088851897267));
#125360=CARTESIAN_POINT('Ctrl Pts',(-18.7957307106799,34.7082643255815,
-12.1486504715915));
#125361=CARTESIAN_POINT('Ctrl Pts',(-18.784159852527,34.7702166242448,-12.1921413513201));
#125362=CARTESIAN_POINT('Ctrl Pts',(-18.7672884639414,34.8535445163286,
-12.2764946297254));
#125363=CARTESIAN_POINT('Ctrl Pts',(-18.7606689443804,34.8835886882299,
-12.3169287768681));
#125364=CARTESIAN_POINT('Ctrl Pts',(-18.7520329511296,34.9216311139679,
-12.3986190308673));
#125365=CARTESIAN_POINT('Ctrl Pts',(-18.7494922500063,34.9323419849364,
-12.4373510176214));
#125366=CARTESIAN_POINT('Ctrl Pts',(-18.7486753311664,34.9358059214554,
-12.4851148185871));
#125367=CARTESIAN_POINT('Ctrl Pts',(-18.7486119524321,34.936074260497,-12.4925693313125));
#125368=CARTESIAN_POINT('Ctrl Pts',(-18.7486119524321,34.936074260497,-12.5));
#125369=CARTESIAN_POINT('Ctrl Pts',(-18.8658210632966,34.1292719773218,
-12.));
#125370=CARTESIAN_POINT('Ctrl Pts',(-18.8656807480304,34.1308827000775,
-12.));
#125371=CARTESIAN_POINT('Ctrl Pts',(-18.8655400049988,34.1324933903514,
-12.0000032434225));
#125372=CARTESIAN_POINT('Ctrl Pts',(-18.8573778375601,34.2256175041334,
-12.0003779495169));
#125373=CARTESIAN_POINT('Ctrl Pts',(-18.8478563981533,34.3178692956096,
-12.0111952320962));
#125374=CARTESIAN_POINT('Ctrl Pts',(-18.8288764025859,34.4771426650498,
-12.048491997422));
#125375=CARTESIAN_POINT('Ctrl Pts',(-18.8196146553393,34.5470501977567,
-12.0716841972469));
#125376=CARTESIAN_POINT('Ctrl Pts',(-18.810086036752,34.6128021370802,-12.1018952060707));
#125377=CARTESIAN_POINT('Origin',(-7.74989684768079,44.6307331902083,-12.5));
#125378=CARTESIAN_POINT('',(-12.8000542780937,44.6309134626335,-12.));
#125379=CARTESIAN_POINT('Origin',(-12.8000542780937,44.6309134626335,-12.5));
#125380=CARTESIAN_POINT('Origin',(-15.5000542763735,44.6310098429057,-12.5));
#125381=CARTESIAN_POINT('',(-7.74989684768079,44.6307331902083,-12.));
#125382=CARTESIAN_POINT('Origin',(-6.40003962806013,44.6307992338217,-12.5));
#125383=CARTESIAN_POINT('',(12.8005486797976,44.6304565379091,-12.));
#125384=CARTESIAN_POINT('Origin',(12.8005486797976,44.6304565379091,-12.5));
#125385=CARTESIAN_POINT('',(-6.40003962806013,44.6307992338217,-12.));
#125386=CARTESIAN_POINT('Origin',(6.40011460523903,44.6304565378295,-12.5));
#125387=CARTESIAN_POINT('',(15.5005576038968,44.6304565378295,-12.));
#125388=CARTESIAN_POINT('',(6.40011460523903,44.6304565378295,-12.));
#125389=CARTESIAN_POINT('Origin',(15.5005576038968,44.6304565378295,-12.5));
#125390=CARTESIAN_POINT('Origin',(-15.5000542763735,44.6310098429057,-12.5));
#125391=CARTESIAN_POINT('Origin',(16.0005576038968,36.1384565378295,-12.5));
#125392=CARTESIAN_POINT('',(16.0005576038968,39.1384565378295,-12.5));
#125393=CARTESIAN_POINT('',(18.7487692036153,34.9354049997927,-12.5));
#125394=CARTESIAN_POINT('Origin',(16.0005576038968,36.1384565378295,-12.5));
#125395=CARTESIAN_POINT('',(15.5005576038968,39.6025581529673,-12.));
#125396=CARTESIAN_POINT('Ctrl Pts',(15.5005576038968,39.6025581529673,-12.));
#125397=CARTESIAN_POINT('Ctrl Pts',(15.5016040980935,39.601651862408,-12.));
#125398=CARTESIAN_POINT('Ctrl Pts',(15.5026504179355,39.6007453671807,-12.0000032854501));
#125399=CARTESIAN_POINT('Ctrl Pts',(15.5265850871382,39.5800010504138,-12.0001535475902));
#125400=CARTESIAN_POINT('Ctrl Pts',(15.5494014043324,39.5600546907341,-12.0018685097915));
#125401=CARTESIAN_POINT('Ctrl Pts',(15.6559105390839,39.4661224630978,-12.0172417791965));
#125402=CARTESIAN_POINT('Ctrl Pts',(15.7346031370173,39.394165582834,-12.0503680939609));
#125403=CARTESIAN_POINT('Ctrl Pts',(15.8547587133249,39.2812778115798,-12.1407858340455));
#125404=CARTESIAN_POINT('Ctrl Pts',(15.8995456863726,39.2379968757629,-12.1913094880829));
#125405=CARTESIAN_POINT('Ctrl Pts',(15.9585903602516,39.1802363196783,-12.2931553699351));
#125406=CARTESIAN_POINT('Ctrl Pts',(15.9783903787479,39.1605638455604,-12.3427321807669));
#125407=CARTESIAN_POINT('Ctrl Pts',(15.9969160291529,39.1421042769301,-12.4305871755405));
#125408=CARTESIAN_POINT('Ctrl Pts',(16.0005576038968,39.1384565378295,-12.4651445835938));
#125409=CARTESIAN_POINT('Ctrl Pts',(16.0005576038968,39.1384565378295,-12.5));
#125410=CARTESIAN_POINT('',(18.8659495144705,34.1285985331886,-12.));
#125411=CARTESIAN_POINT('Origin',(16.0005576038968,36.1384565378295,-12.));
#125412=CARTESIAN_POINT('',(18.8102317482459,34.6121306821786,-12.1018952060707));
#125413=CARTESIAN_POINT('Ctrl Pts',(18.8102317482459,34.6121306821786,-12.1018952060707));
#125414=CARTESIAN_POINT('Ctrl Pts',(18.8197580197198,34.5463784027596,-12.0716841972469));
#125415=CARTESIAN_POINT('Ctrl Pts',(18.8290172715136,34.4764705394863,-12.048491997422));
#125416=CARTESIAN_POINT('Ctrl Pts',(18.8479915815835,34.3171964926297,-12.0111952320961));
#125417=CARTESIAN_POINT('Ctrl Pts',(18.8575097279277,34.2249443613295,-12.0003779495169));
#125418=CARTESIAN_POINT('Ctrl Pts',(18.8656685711657,34.131819956249,-12.0000032434225));
#125419=CARTESIAN_POINT('Ctrl Pts',(18.8658092567013,34.130209260952,-12.));
#125420=CARTESIAN_POINT('Ctrl Pts',(18.8659495144705,34.1285985331886,-12.));
#125421=CARTESIAN_POINT('Ctrl Pts',(18.7487692036153,34.9354049997927,-12.5));
#125422=CARTESIAN_POINT('Ctrl Pts',(18.7487692036153,34.9354049997927,-12.4925693313125));
#125423=CARTESIAN_POINT('Ctrl Pts',(18.7488325727708,34.9351366584889,-12.4851148185871));
#125424=CARTESIAN_POINT('Ctrl Pts',(18.7496493679601,34.9316726928111,-12.4373510176214));
#125425=CARTESIAN_POINT('Ctrl Pts',(18.7521896867423,34.9209617311555,-12.3986190308672));
#125426=CARTESIAN_POINT('Ctrl Pts',(18.7608243220101,34.8829189971679,-12.3169287768681));
#125427=CARTESIAN_POINT('Ctrl Pts',(18.7674427690982,34.8528745889928,-12.2764946297254));
#125428=CARTESIAN_POINT('Ctrl Pts',(18.7843111831676,34.769546094714,-12.1921413513198));
#125429=CARTESIAN_POINT('Ctrl Pts',(18.7958798298392,34.7075933830521,-12.1486504715914));
#125430=CARTESIAN_POINT('Ctrl Pts',(18.8080435840964,34.6270726442891,-12.1088851897267));
#125431=CARTESIAN_POINT('Ctrl Pts',(18.8091452024147,34.6196302443412,-12.1053410081124));
#125432=CARTESIAN_POINT('Ctrl Pts',(18.8102317482459,34.6121306821786,-12.1018952060707));
#125433=CARTESIAN_POINT('Origin',(15.5005576038968,36.3806823573572,-12.5));
#125434=CARTESIAN_POINT('',(15.5005576038968,36.3806823573572,-12.));
#125435=CARTESIAN_POINT('',(16.0005576038968,44.6304565378295,-12.5));
#125436=CARTESIAN_POINT('',(16.0005576038968,36.3806823573572,-12.5));
#125437=CARTESIAN_POINT('Origin',(15.5005576038968,44.6304565378295,-12.5));
#125438=CARTESIAN_POINT('Origin',(15.5005576038968,44.6304565378295,-12.5));
#125439=CARTESIAN_POINT('Origin',(15.5005576038968,44.6304565378295,-12.5));
#125440=CARTESIAN_POINT('Origin',(-18.3067027565145,34.6883503685105,-12.5));
#125441=CARTESIAN_POINT('Origin',(-18.5961864812216,34.3988873101177,-12.5));
#125442=CARTESIAN_POINT('',(-24.1818223222136,28.8136502290417,-12.));
#125443=CARTESIAN_POINT('Origin',(-24.1818223222136,28.8136502290417,-12.5));
#125444=CARTESIAN_POINT('',(-18.3067027565145,34.6883503685105,-12.));
#125445=CARTESIAN_POINT('Origin',(-0.000328393418778106,28.1309081768848,
-12.));
#125446=CARTESIAN_POINT('',(-25.4999553912744,25.6317167642765,-12.));
#125447=CARTESIAN_POINT('Origin',(-20.9999553941414,25.6315561304895,-12.));
#125448=CARTESIAN_POINT('',(-25.5004372926353,12.1317167728775,-12.));
#125449=CARTESIAN_POINT('',(-25.5001517196441,20.1317675956942,-12.));
#125450=CARTESIAN_POINT('',(-25.0004551411524,11.6316989249976,-12.));
#125451=CARTESIAN_POINT('Origin',(-25.0004372929538,12.131698924679,-12.));
#125452=CARTESIAN_POINT('',(-20.707561925074,11.6315456841765,-12.));
#125453=CARTESIAN_POINT('',(-10.2506862658096,11.6311724113903,-12.));
#125454=CARTESIAN_POINT('',(-19.5006385804826,12.8383828662136,-12.));
#125455=CARTESIAN_POINT('',(-10.7288557519193,21.609539475044,-12.));
#125456=CARTESIAN_POINT('',(-19.5003186017906,21.8022760793161,-12.));
#125457=CARTESIAN_POINT('',(-19.5002056346847,24.9669401637651,-12.));
#125458=CARTESIAN_POINT('',(-18.7044786694047,23.12666906083,-12.));
#125459=CARTESIAN_POINT('Origin',(-18.0003186027463,21.8022225347204,-12.));
#125460=CARTESIAN_POINT('',(-15.8748746000505,24.631066672069,-12.));
#125461=CARTESIAN_POINT('',(-9.01646660547503,28.2774328600768,-12.));
#125462=CARTESIAN_POINT('',(-12.0002195251968,24.6309283607631,-12.));
#125463=CARTESIAN_POINT('',(-6.00033197323811,24.630714186474,-12.));
#125464=CARTESIAN_POINT('',(12.,24.6305,-12.));
#125465=CARTESIAN_POINT('',(5.99980902926158,24.6306070926795,-12.));
#125466=CARTESIAN_POINT('',(15.8746640014216,24.6305,-12.));
#125467=CARTESIAN_POINT('',(7.87483580329061,24.6305,-12.));
#125468=CARTESIAN_POINT('',(18.7042143673984,23.1260013830489,-12.));
#125469=CARTESIAN_POINT('',(10.3759028387591,27.5542431726415,-12.));
#125470=CARTESIAN_POINT('',(19.5000070232196,21.8015799937605,-12.));
#125471=CARTESIAN_POINT('Origin',(18.0000070232196,21.8015799937605,-12.));
#125472=CARTESIAN_POINT('',(19.5000070232196,12.8376867749471,-12.));
#125473=CARTESIAN_POINT('',(19.5000070232196,20.3807440853227,-12.));
#125474=CARTESIAN_POINT('',(20.7068872873028,11.6308065108639,-12.));
#125475=CARTESIAN_POINT('',(11.4782812553205,20.8594125428461,-12.));
#125476=CARTESIAN_POINT('',(24.9997805061163,11.6308065108639,-12.));
#125477=CARTESIAN_POINT('',(12.4997260563488,11.6308065108639,-12.));
#125478=CARTESIAN_POINT('',(25.4997805061163,12.1308065108639,-12.));
#125479=CARTESIAN_POINT('Origin',(24.9997805061163,12.1308065108639,-12.));
#125480=CARTESIAN_POINT('',(25.4997805061163,25.6308065108639,-12.));
#125481=CARTESIAN_POINT('',(25.4997805061163,26.8808573438743,-12.));
#125482=CARTESIAN_POINT('',(24.1817610214557,28.8127870262033,-12.));
#125483=CARTESIAN_POINT('Origin',(20.9997805061163,25.6308065108639,-12.));
#125484=CARTESIAN_POINT('',(15.5139901477705,37.4805578998886,-12.));
#125485=CARTESIAN_POINT('Origin',(15.5139901477705,37.4805578998886,-12.5));
#125486=CARTESIAN_POINT('',(24.535314412049,29.1663404167966,-12.5));
#125487=CARTESIAN_POINT('Origin',(24.1817610214557,28.8127870262033,-12.5));
#125488=CARTESIAN_POINT('',(18.9498779474565,34.7517768813891,-12.5));
#125489=CARTESIAN_POINT('',(15.8675435383638,37.8341112904819,-12.5));
#125490=CARTESIAN_POINT('Origin',(18.5963245568632,34.3982234907959,-12.5));
#125491=CARTESIAN_POINT('Origin',(16.8285576038968,32.6304565378295,-12.5));
#125492=CARTESIAN_POINT('Origin',(16.8285576038968,32.6304565378295,-12.5));
#125493=CARTESIAN_POINT('Origin',(-10.2506862658096,11.6311724113903,-12.5));
#125494=CARTESIAN_POINT('Origin',(-20.707561925074,11.6315456841765,-12.5));
#125495=CARTESIAN_POINT('Origin',(-25.0004551411524,11.6316989249976,-12.5));
#125496=CARTESIAN_POINT('Ctrl Pts',(-25.0004551411523,11.6316989249976,
-12.));
#125497=CARTESIAN_POINT('Ctrl Pts',(-25.5004551408337,11.6317167731962,
-12.));
#125498=CARTESIAN_POINT('Ctrl Pts',(-25.5004372926352,12.1317167728776,
-12.));
#125499=CARTESIAN_POINT('Ctrl Pts',(-25.0004729893509,11.131698925316,-11.9999999999999));
#125500=CARTESIAN_POINT('Ctrl Pts',(-26.0004729887137,11.1317346217132,
-12.));
#125501=CARTESIAN_POINT('Ctrl Pts',(-26.0004372923168,12.131734621076,-11.9999999999999));
#125502=CARTESIAN_POINT('Ctrl Pts',(-25.0004729893509,11.1316989253161,
-12.5000000000001));
#125503=CARTESIAN_POINT('Ctrl Pts',(-26.0004729887137,11.1317346217133,
-12.5000000000001));
#125504=CARTESIAN_POINT('Ctrl Pts',(-26.0004372923167,12.1317346210761,
-12.5));
#125505=CARTESIAN_POINT('Origin',(-25.5004372926353,12.1317167728775,-12.5));
#125506=CARTESIAN_POINT('Origin',(-25.5001517196441,20.1317675956942,-12.5));
#125507=CARTESIAN_POINT('Origin',(-25.4999553912744,25.6317167642765,-12.5));
#125508=CARTESIAN_POINT('Origin',(-20.9999553941414,25.6315561304895,-12.5));
#125509=CARTESIAN_POINT('Origin',(-16.8284826322926,32.6310572553665,-12.5));
#125510=CARTESIAN_POINT('Origin',(-10.7288557519193,21.609539475044,-12.5));
#125511=CARTESIAN_POINT('Origin',(-19.5006385804826,12.8383828662136,-12.5));
#125512=CARTESIAN_POINT('Origin',(-9.01646660547503,28.2774328600768,-12.5));
#125513=CARTESIAN_POINT('Origin',(-15.8748746000505,24.631066672069,-12.5));
#125514=CARTESIAN_POINT('Origin',(-18.7044786694047,23.12666906083,-12.5));
#125515=CARTESIAN_POINT('Origin',(-18.0003186027463,21.8022225347204,-12.5));
#125516=CARTESIAN_POINT('Origin',(-19.5003186017906,21.8022760793161,-12.5));
#125517=CARTESIAN_POINT('Origin',(-19.5002056346847,24.9669401637651,-12.5));
#125518=CARTESIAN_POINT('Origin',(7.87483580329061,24.6305,-12.5));
#125519=CARTESIAN_POINT('',(15.75,24.1305,-12.5));
#125520=CARTESIAN_POINT('',(12.,24.1305,-12.5));
#125521=CARTESIAN_POINT('',(7.87483580329061,24.1305,-12.5));
#125522=CARTESIAN_POINT('Origin',(15.8746640014216,24.6305,-12.5));
#125523=CARTESIAN_POINT('Origin',(12.,24.6305,-12.5));
#125524=CARTESIAN_POINT('Origin',(5.99980902926158,24.6306070926795,-12.5));
#125525=CARTESIAN_POINT('',(-12.0002284492961,24.1309283608428,-12.5));
#125526=CARTESIAN_POINT('Origin',(-12.0002195251968,24.6309283607631,-12.5));
#125527=CARTESIAN_POINT('',(5.9998001051623,24.1306070927591,-12.5));
#125528=CARTESIAN_POINT('Origin',(-6.00033197323811,24.630714186474,-12.5));
#125529=CARTESIAN_POINT('',(-6.00034982143666,24.1307141867926,-12.5));
#125530=CARTESIAN_POINT('Origin',(19.5000070232196,20.3807440853227,-12.5));
#125531=CARTESIAN_POINT('',(19.0000070232196,12.6305799937605,-12.5));
#125532=CARTESIAN_POINT('',(19.0000070232196,21.8015799937605,-12.5));
#125533=CARTESIAN_POINT('',(19.0000070232196,20.3807440853227,-12.5));
#125534=CARTESIAN_POINT('Origin',(19.5000070232196,12.8376867749471,-12.5));
#125535=CARTESIAN_POINT('Origin',(19.5000070232196,21.8015799937605,-12.5));
#125536=CARTESIAN_POINT('Origin',(18.0000070232196,21.8015799937605,-12.5));
#125537=CARTESIAN_POINT('',(18.4694785860055,22.6845275866195,-12.5));
#125538=CARTESIAN_POINT('Origin',(18.7042143673984,23.1260013830489,-12.5));
#125539=CARTESIAN_POINT('Origin',(18.0000070232196,21.8015799937605,-12.5));
#125540=CARTESIAN_POINT('Origin',(10.3759028387591,27.5542431726415,-12.5));
#125541=CARTESIAN_POINT('',(10.1411670573662,27.112769376212,-12.5));
#125542=CARTESIAN_POINT('Origin',(11.4782812553205,20.8594125428461,-12.5));
#125543=CARTESIAN_POINT('',(20.4997805061163,11.1308065108639,-12.5));
#125544=CARTESIAN_POINT('',(11.1247278647273,20.5058591522529,-12.5));
#125545=CARTESIAN_POINT('Origin',(20.7068872873028,11.6308065108639,-12.5));
#125546=CARTESIAN_POINT('Origin',(20.9997805061163,25.6308065108639,-12.5));
#125547=CARTESIAN_POINT('',(25.9997805061163,25.6308065108639,-12.5));
#125548=CARTESIAN_POINT('Origin',(25.4997805061163,25.6308065108639,-12.5));
#125549=CARTESIAN_POINT('Origin',(20.9997805061163,25.6308065108639,-12.5));
#125550=CARTESIAN_POINT('Origin',(25.4997805061163,26.8808573438743,-12.5));
#125551=CARTESIAN_POINT('',(25.9997805061163,12.1308065108639,-12.5));
#125552=CARTESIAN_POINT('Origin',(25.4997805061163,12.1308065108639,-12.5));
#125553=CARTESIAN_POINT('',(25.9997805061163,26.8808573438743,-12.5));
#125554=CARTESIAN_POINT('Ctrl Pts',(25.4997805061163,12.1308065108639,-12.));
#125555=CARTESIAN_POINT('Ctrl Pts',(25.4997805061163,11.6308065108639,-12.));
#125556=CARTESIAN_POINT('Ctrl Pts',(24.9997805061163,11.6308065108639,-12.));
#125557=CARTESIAN_POINT('Ctrl Pts',(25.9997805061163,12.1308065108639,-12.));
#125558=CARTESIAN_POINT('Ctrl Pts',(25.9997805061163,11.1308065108639,-12.));
#125559=CARTESIAN_POINT('Ctrl Pts',(24.9997805061163,11.1308065108639,-12.));
#125560=CARTESIAN_POINT('Ctrl Pts',(25.9997805061163,12.1308065108639,-12.5));
#125561=CARTESIAN_POINT('Ctrl Pts',(25.9997805061163,11.1308065108639,-12.5));
#125562=CARTESIAN_POINT('Ctrl Pts',(24.9997805061163,11.1308065108639,-12.5));
#125563=CARTESIAN_POINT('',(24.9997805061163,11.1308065108639,-12.5));
#125564=CARTESIAN_POINT('Origin',(24.9997805061163,11.6308065108639,-12.5));
#125565=CARTESIAN_POINT('Origin',(24.9997805061163,12.1308065108639,-12.5));
#125566=CARTESIAN_POINT('Origin',(12.4997260563488,11.6308065108639,-12.5));
#125567=CARTESIAN_POINT('',(12.4997260563488,11.1308065108639,-12.5));
#125568=CARTESIAN_POINT('Origin',(-12.0002284492961,24.1309283608428,-26.));
#125569=CARTESIAN_POINT('',(-12.0002284492961,24.1309283608428,-26.));
#125570=CARTESIAN_POINT('Origin',(12.,24.1305,-26.));
#125571=CARTESIAN_POINT('',(12.,24.1305,-26.));
#125572=CARTESIAN_POINT('Origin',(15.75,24.1305,-26.));
#125573=CARTESIAN_POINT('',(15.75,24.1305,-26.));
#125574=CARTESIAN_POINT('Origin',(18.4694785860055,22.6845275866195,-26.));
#125575=CARTESIAN_POINT('',(18.4694785860055,22.6845275866195,-26.));
#125576=CARTESIAN_POINT('Origin',(18.0000070232196,21.8015799937605,-26.));
#125577=CARTESIAN_POINT('',(19.0000070232196,21.8015799937605,-26.));
#125578=CARTESIAN_POINT('Origin',(19.0000070232196,12.6305799937605,-26.));
#125579=CARTESIAN_POINT('',(19.0000070232196,12.6305799937605,-26.));
#125580=CARTESIAN_POINT('Origin',(20.4997805061163,11.1308065108639,-26.));
#125581=CARTESIAN_POINT('',(20.4997805061163,11.1308065108639,-26.));
#125582=CARTESIAN_POINT('Origin',(24.9997805061163,11.1308065108639,-26.));
#125583=CARTESIAN_POINT('',(24.9997805061163,11.1308065108639,-26.));
#125584=CARTESIAN_POINT('Origin',(24.9997805061163,12.1308065108639,-26.));
#125585=CARTESIAN_POINT('',(25.9997805061163,12.1308065108639,-26.));
#125586=CARTESIAN_POINT('Origin',(25.9997805061163,25.6308065108639,-26.));
#125587=CARTESIAN_POINT('',(25.9997805061163,25.6308065108639,-26.));
#125588=CARTESIAN_POINT('Origin',(20.9997805061163,25.6308065108639,-26.));
#125589=CARTESIAN_POINT('',(24.535314412049,29.1663404167966,-26.));
#125590=CARTESIAN_POINT('Origin',(18.9498779474565,34.7517768813891,-26.));
#125591=CARTESIAN_POINT('',(18.9498779474565,34.7517768813891,-26.));
#125592=CARTESIAN_POINT('Origin',(16.8285576038968,32.6304565378295,-26.));
#125593=CARTESIAN_POINT('',(16.8285576038968,35.6304565378295,-15.));
#125594=CARTESIAN_POINT('',(16.8285576038968,35.6304565378295,-26.));
#125595=CARTESIAN_POINT('',(18.7487692036153,34.9354049997927,-15.));
#125596=CARTESIAN_POINT('Origin',(16.8285576038968,32.6304565378295,-15.));
#125597=CARTESIAN_POINT('',(18.7487692036153,34.9354049997927,-12.));
#125598=CARTESIAN_POINT('Origin',(16.0005576038968,36.1384565378295,-12.));
#125599=CARTESIAN_POINT('',(16.0005576038968,39.1384565378295,-15.));
#125600=CARTESIAN_POINT('Origin',(16.0005576038968,36.1384565378295,-15.));
#125601=CARTESIAN_POINT('',(16.0005576038968,39.1384565378295,-12.));
#125602=CARTESIAN_POINT('Origin',(-16.0003574098591,36.1390276965147,-12.));
#125603=CARTESIAN_POINT('Origin',(-16.0003574098591,36.1390276965147,-15.));
#125604=CARTESIAN_POINT('Origin',(-15.8744846811456,36.139027695559,-15.));
#125605=CARTESIAN_POINT('Origin',(15.8746634037561,36.1384565378295,-15.));
#125606=CARTESIAN_POINT('',(16.5085576038968,35.6304565378295,-15.));
#125607=CARTESIAN_POINT('',(16.1916105038265,35.6304565378295,-15.));
#125608=CARTESIAN_POINT('',(16.0005576038968,36.1384565378295,-15.));
#125609=CARTESIAN_POINT('Origin',(16.5085576038968,36.1384565378295,-15.));
#125610=CARTESIAN_POINT('',(16.0005576038968,40.3844565378295,-15.));
#125611=CARTESIAN_POINT('Origin',(16.5085576038968,35.6304565378295,-26.));
#125612=CARTESIAN_POINT('',(16.5085576038968,35.6304565378295,-26.));
#125613=CARTESIAN_POINT('Origin',(16.5085576038968,36.1384565378295,-26.));
#125614=CARTESIAN_POINT('',(16.0005576038968,36.1384565378295,-26.));
#125615=CARTESIAN_POINT('Origin',(16.0005576038968,44.6304565378295,-26.));
#125616=CARTESIAN_POINT('',(16.0005576038968,44.6304565378295,-26.));
#125617=CARTESIAN_POINT('Origin',(15.5005576038968,44.6304565378295,-26.));
#125618=CARTESIAN_POINT('Origin',(0.000260570142325415,45.1297404501394,
36.));
#125619=CARTESIAN_POINT('',(0.00026057014232539,45.1297404501426,32.9999999993629));
#125620=CARTESIAN_POINT('',(0.00026057014232539,45.1297404501426,39.0000000006371));
#125621=CARTESIAN_POINT('Origin',(0.000260570142325415,45.1297404501395,
36.));
#125622=CARTESIAN_POINT('Origin',(0.000260570142325751,45.1297404501489,
36.));
#125623=CARTESIAN_POINT('',(0.000117784559150455,41.1297404526879,39.));
#125624=CARTESIAN_POINT('',(0.000260570142325048,45.1297404501394,39.));
#125625=CARTESIAN_POINT('Origin',(0.000117784559150088,41.1297404526879,
36.));
#125626=CARTESIAN_POINT('Origin',(0.000117784559149936,41.1297404526879,
36.));
#125627=CARTESIAN_POINT('Origin',(0.000260570142326236,45.1297404501394,
96.));
#125628=CARTESIAN_POINT('',(0.00026057014232539,45.1297404501426,92.9999999993629));
#125629=CARTESIAN_POINT('',(0.00026057014232539,45.1297404501426,99.0000000006371));
#125630=CARTESIAN_POINT('Origin',(0.000260570142326236,45.1297404501395,
96.));
#125631=CARTESIAN_POINT('Origin',(0.000260570142326572,45.1297404501489,
96.));
#125632=CARTESIAN_POINT('',(0.000117784559151277,41.1297404526879,99.));
#125633=CARTESIAN_POINT('',(0.000260570142325869,45.1297404501394,99.));
#125634=CARTESIAN_POINT('Origin',(0.000117784559150909,41.1297404526879,
96.));
#125635=CARTESIAN_POINT('Origin',(0.000117784559151046,41.1297404526879,
96.));
#125636=CARTESIAN_POINT('Origin',(7.20026057014233,45.1297404501395,26.));
#125637=CARTESIAN_POINT('',(0.000260570142325278,45.1297404501395,26.));
#125638=CARTESIAN_POINT('',(0.000260570142325278,45.1297404501395,106.));
#125639=CARTESIAN_POINT('',(0.000260570142325278,45.1297404501395,26.));
#125640=CARTESIAN_POINT('',(7.20026057014233,45.1297404501395,106.));
#125641=CARTESIAN_POINT('',(7.20026057014233,45.1297404501395,106.));
#125642=CARTESIAN_POINT('',(7.20026057014233,45.1297404501395,26.));
#125643=CARTESIAN_POINT('',(7.20026057014233,45.1297404501395,26.));
#125644=CARTESIAN_POINT('',(0.000260570142325278,45.1297404501395,26.));
#125645=CARTESIAN_POINT('',(7.20026057014233,45.1297404501395,26.));
#125646=CARTESIAN_POINT('',(0.000260570142325278,45.1297404501395,26.));
#125647=CARTESIAN_POINT('Origin',(16.0005712344353,40.3838853813626,46.));
#125648=CARTESIAN_POINT('',(16.0005576038968,40.0020390449739,43.0244003328805));
#125649=CARTESIAN_POINT('',(16.0005576038968,40.0020390449739,48.9755996671195));
#125650=CARTESIAN_POINT('',(16.0005576038968,40.0020390450537,36.));
#125651=CARTESIAN_POINT('Origin',(16.0005712344353,40.3838853813626,46.));
#125652=CARTESIAN_POINT('Origin',(-25.9994287388058,40.3853846300409,46.));
#125653=CARTESIAN_POINT('',(-16.000205842957,40.3850276938095,43.));
#125654=CARTESIAN_POINT('Origin',(-16.000205842957,40.3850276938095,46.));
#125655=CARTESIAN_POINT('',(-14.1509424007594,40.3849616818491,43.));
#125656=CARTESIAN_POINT('',(-25.9994287388058,40.3853846300409,43.));
#125657=CARTESIAN_POINT('',(-14.2001947782207,40.6949634400972,43.0160596520708));
#125658=CARTESIAN_POINT('Ctrl Pts',(-14.1509424007594,40.384961681931,43.));
#125659=CARTESIAN_POINT('Ctrl Pts',(-14.1842343067511,40.4870767337193,
43.0000000000056));
#125660=CARTESIAN_POINT('Ctrl Pts',(-14.2001983851187,40.5939196884095,
43.0055622696198));
#125661=CARTESIAN_POINT('Ctrl Pts',(-14.2001947782208,40.6949634400972,
43.0160596520708));
#125662=CARTESIAN_POINT('',(-14.200125669996,42.6309634388637,44.0111601371654));
#125663=CARTESIAN_POINT('Origin',(-14.2002058441038,40.3849634402947,46.));
#125664=CARTESIAN_POINT('',(-13.700107822116,43.1309455903466,44.7919089438291));
#125665=CARTESIAN_POINT('Ctrl Pts',(-13.700107822116,43.1309455903466,44.7919089438292));
#125666=CARTESIAN_POINT('Ctrl Pts',(-13.7287138176145,43.1309466114776,
44.7919089438292));
#125667=CARTESIAN_POINT('Ctrl Pts',(-13.7588198896061,43.1282901354821,
44.7858171356271));
#125668=CARTESIAN_POINT('Ctrl Pts',(-13.8150242028358,43.1184187630571,
44.7637668516514));
#125669=CARTESIAN_POINT('Ctrl Pts',(-13.8411536038327,43.1112169321056,
44.7478820248202));
#125670=CARTESIAN_POINT('Ctrl Pts',(-13.942146077159,43.0763467034421,44.6731422398802));
#125671=CARTESIAN_POINT('Ctrl Pts',(-14.0082080214715,43.0299667749565,
44.5814744645503));
#125672=CARTESIAN_POINT('Ctrl Pts',(-14.1423359864052,42.8958483854512,
44.3486366205185));
#125673=CARTESIAN_POINT('Ctrl Pts',(-14.2001209716938,42.7625818225232,
44.1597969859191));
#125674=CARTESIAN_POINT('Ctrl Pts',(-14.2001256699959,42.6309634388638,
44.0111601371654));
#125675=CARTESIAN_POINT('',(-12.8001078226894,43.1309134635892,44.7919089438291));
#125676=CARTESIAN_POINT('',(-25.9993307164994,43.1313846282914,44.7919089438291));
#125677=CARTESIAN_POINT('',(-12.8001078226894,43.1309134635892,47.2080910561709));
#125678=CARTESIAN_POINT('Ctrl Pts',(-12.8001078226893,43.1309134635892,
47.2080910561709));
#125679=CARTESIAN_POINT('Ctrl Pts',(-12.7874290218161,43.1309130110017,
47.2080910561709));
#125680=CARTESIAN_POINT('Ctrl Pts',(-12.7747450872089,43.1317310514822,
47.2062354373186));
#125681=CARTESIAN_POINT('Ctrl Pts',(-12.7501661862404,43.1348375455173,
47.199133868969));
#125682=CARTESIAN_POINT('Ctrl Pts',(-12.7382804382214,43.1371385398321,
47.193861533145));
#125683=CARTESIAN_POINT('Ctrl Pts',(-12.7046747516163,43.1455281504129,
47.1743800110828));
#125684=CARTESIAN_POINT('Ctrl Pts',(-12.6851453672407,43.1532658613644,
47.1561143770981));
#125685=CARTESIAN_POINT('Ctrl Pts',(-12.6471649980075,43.1716314784724,
47.111298056684));
#125686=CARTESIAN_POINT('Ctrl Pts',(-12.6264424973877,43.1855881094717,
47.0757741121274));
#125687=CARTESIAN_POINT('Ctrl Pts',(-12.5778499600881,43.224674918756,46.9705448594992));
#125688=CARTESIAN_POINT('Ctrl Pts',(-12.5550921166024,43.2558293923731,
46.8746617707269));
#125689=CARTESIAN_POINT('Ctrl Pts',(-12.5029059493652,43.3441575831397,
46.5522053662921));
#125690=CARTESIAN_POINT('Ctrl Pts',(-12.5036463989442,43.3849028811463,
46.2522550206409));
#125691=CARTESIAN_POINT('Ctrl Pts',(-12.5036463989442,43.3849028811463,
45.7477449793591));
#125692=CARTESIAN_POINT('Ctrl Pts',(-12.5029059493652,43.3441575831397,
45.4477946337079));
#125693=CARTESIAN_POINT('Ctrl Pts',(-12.5550921166024,43.2558293923731,
45.1253382292731));
#125694=CARTESIAN_POINT('Ctrl Pts',(-12.5778499600881,43.224674918756,45.0294551405009));
#125695=CARTESIAN_POINT('Ctrl Pts',(-12.6264424973877,43.1855881094717,
44.9242258878726));
#125696=CARTESIAN_POINT('Ctrl Pts',(-12.6471649980075,43.1716314784724,
44.888701943316));
#125697=CARTESIAN_POINT('Ctrl Pts',(-12.6851453672407,43.1532658613644,
44.8438856229019));
#125698=CARTESIAN_POINT('Ctrl Pts',(-12.7046747516163,43.1455281504129,
44.8256199889173));
#125699=CARTESIAN_POINT('Ctrl Pts',(-12.7382804382214,43.1371385398321,
44.806138466855));
#125700=CARTESIAN_POINT('Ctrl Pts',(-12.7501661862404,43.1348375455173,
44.800866131031));
#125701=CARTESIAN_POINT('Ctrl Pts',(-12.7747450872089,43.1317310514822,
44.7937645626814));
#125702=CARTESIAN_POINT('Ctrl Pts',(-12.7874290218161,43.1309130110017,
44.7919089438292));
#125703=CARTESIAN_POINT('Ctrl Pts',(-12.8001078226893,43.1309134635892,
44.7919089438292));
#125704=CARTESIAN_POINT('',(-13.700107822116,43.1309455903466,47.2080910561709));
#125705=CARTESIAN_POINT('',(-25.9993307164994,43.1313846282914,47.2080910561709));
#125706=CARTESIAN_POINT('',(-14.200125669996,42.6309634388637,47.9888398628346));
#125707=CARTESIAN_POINT('Ctrl Pts',(-14.2001256699959,42.6309634388638,
47.9888398628346));
#125708=CARTESIAN_POINT('Ctrl Pts',(-14.2001209716939,42.7625818225232,
47.8402030140809));
#125709=CARTESIAN_POINT('Ctrl Pts',(-14.1423359864052,42.8958483854512,
47.6513633794815));
#125710=CARTESIAN_POINT('Ctrl Pts',(-14.0082080214715,43.0299667749565,
47.4185255354497));
#125711=CARTESIAN_POINT('Ctrl Pts',(-13.942146077159,43.0763467034421,47.3268577601199));
#125712=CARTESIAN_POINT('Ctrl Pts',(-13.8411536038327,43.1112169321056,
47.2521179751798));
#125713=CARTESIAN_POINT('Ctrl Pts',(-13.8150242028358,43.1184187630571,
47.2362331483486));
#125714=CARTESIAN_POINT('Ctrl Pts',(-13.7588198896061,43.1282901354821,
47.2141828643729));
#125715=CARTESIAN_POINT('Ctrl Pts',(-13.7287138176144,43.1309466114776,
47.2080910561708));
#125716=CARTESIAN_POINT('Ctrl Pts',(-13.7001078221159,43.1309455903466,
47.2080910561708));
#125717=CARTESIAN_POINT('',(-14.2001947782207,40.6949634400972,48.9839403479292));
#125718=CARTESIAN_POINT('Origin',(-14.2002058441038,40.3849634402947,46.));
#125719=CARTESIAN_POINT('',(-13.9073268007583,39.9878462041285,48.9736015544009));
#125720=CARTESIAN_POINT('Ctrl Pts',(-13.9073268007584,39.9878462041285,
48.973601554401));
#125721=CARTESIAN_POINT('Ctrl Pts',(-13.9960100566734,40.076535791615,48.9854450979406));
#125722=CARTESIAN_POINT('Ctrl Pts',(-14.0730534099154,40.1890412751135,
48.9961344807684));
#125723=CARTESIAN_POINT('Ctrl Pts',(-14.1751560019799,40.435594122051,49.0021062582817));
#125724=CARTESIAN_POINT('Ctrl Pts',(-14.2001992511613,40.5696583440676,
48.9969582287394));
#125725=CARTESIAN_POINT('Ctrl Pts',(-14.2001947782208,40.6949634400972,
48.9839403479292));
#125726=CARTESIAN_POINT('',(-13.0856980517762,39.1661587946801,48.7412793024013));
#125727=CARTESIAN_POINT('Origin',(-14.3044194064105,40.3849671603434,46.));
#125728=CARTESIAN_POINT('',(-11.6715054007694,38.5803218750975,48.3965797735301));
#125729=CARTESIAN_POINT('Ctrl Pts',(-11.6715054007694,38.5803218750975,
48.3965797735301));
#125730=CARTESIAN_POINT('Ctrl Pts',(-11.9310804859103,38.5803311409929,
48.3965797735301));
#125731=CARTESIAN_POINT('Ctrl Pts',(-12.2008654839661,38.6335041042047,
48.4388004161354));
#125732=CARTESIAN_POINT('Ctrl Pts',(-12.6901619533851,38.8388876989633,
48.5738923324279));
#125733=CARTESIAN_POINT('Ctrl Pts',(-12.9106059326522,38.9910541747943,
48.6634310729608));
#125734=CARTESIAN_POINT('Ctrl Pts',(-13.0856980517762,39.1661587946801,
48.7412793024013));
#125735=CARTESIAN_POINT('',(-9.57050540210797,38.5802468769672,48.3965797735301));
#125736=CARTESIAN_POINT('',(-25.9994931547856,38.5808333326384,48.3965797735301));
#125737=CARTESIAN_POINT('',(-6.03491922226453,40.0445867642791,48.980661345019));
#125738=CARTESIAN_POINT('Ctrl Pts',(-6.03491922226454,40.0445867642791,
48.980661345019));
#125739=CARTESIAN_POINT('Ctrl Pts',(-6.46491979272285,39.6146168916673,
48.9316012220604));
#125740=CARTESIAN_POINT('Ctrl Pts',(-6.98352950944328,39.2568425175939,
48.7941482303742));
#125741=CARTESIAN_POINT('Ctrl Pts',(-8.18737580567769,38.7250267702563,
48.519101496493));
#125742=CARTESIAN_POINT('Ctrl Pts',(-8.88897256914252,38.5802225487005,
48.3965797735301));
#125743=CARTESIAN_POINT('Ctrl Pts',(-9.57050540210795,38.5802468769672,
48.3965797735301));
#125744=CARTESIAN_POINT('',(-4.31517414500253,41.7642090685172,48.6639647170471));
#125745=CARTESIAN_POINT('Origin',(-5.69482187817972,40.3846598287309,46.));
#125746=CARTESIAN_POINT('',(-4.88081081954212,43.1299146855279,47.2097174218851));
#125747=CARTESIAN_POINT('Ctrl Pts',(-4.88081081954212,43.1299146855279,
47.2097174218852));
#125748=CARTESIAN_POINT('Ctrl Pts',(-4.82482221472671,43.1299126869364,
47.2097174218852));
#125749=CARTESIAN_POINT('Ctrl Pts',(-4.77320031795728,43.1241916785181,
47.2228273668612));
#125750=CARTESIAN_POINT('Ctrl Pts',(-4.67621148812538,43.104869821818,47.2652368623581));
#125751=CARTESIAN_POINT('Ctrl Pts',(-4.63083615831866,43.0912259898174,
47.2944976062002));
#125752=CARTESIAN_POINT('Ctrl Pts',(-4.50299531310249,43.0409837535405,
47.3962229005734));
#125753=CARTESIAN_POINT('Ctrl Pts',(-4.42918588082232,42.9947395232464,
47.4819738279894));
#125754=CARTESIAN_POINT('Ctrl Pts',(-4.28473708613121,42.8747600616692,
47.6785381778342));
#125755=CARTESIAN_POINT('Ctrl Pts',(-4.21173521992966,42.7838888359608,
47.808410822416));
#125756=CARTESIAN_POINT('Ctrl Pts',(-4.10948896604543,42.5724250222423,
48.0592085197964));
#125757=CARTESIAN_POINT('Ctrl Pts',(-4.08083503287425,42.4515873535033,
48.1801672395615));
#125758=CARTESIAN_POINT('Ctrl Pts',(-4.08084269258332,42.2370080209205,
48.3629383226615));
#125759=CARTESIAN_POINT('Ctrl Pts',(-4.09805029004739,42.1312231898084,
48.4421976606013));
#125760=CARTESIAN_POINT('Ctrl Pts',(-4.17859647402362,41.9330114055893,
48.5720688356092));
#125761=CARTESIAN_POINT('Ctrl Pts',(-4.23902256544589,41.8403552115939,
48.6245291895113));
#125762=CARTESIAN_POINT('Ctrl Pts',(-4.31517414500251,41.7642090685172,
48.6639647170472));
#125763=CARTESIAN_POINT('',(-7.19981081806464,43.1299974654728,47.209717421885));
#125764=CARTESIAN_POINT('',(-25.9993307420611,43.1306685406019,47.2097174218847));
#125765=CARTESIAN_POINT('',(-7.19981081806464,43.1299974654728,44.790282578115));
#125766=CARTESIAN_POINT('Ctrl Pts',(-7.19981081806464,43.1299974654728,
44.790282578115));
#125767=CARTESIAN_POINT('Ctrl Pts',(-7.21250680486427,43.1299979186738,
44.790282578115));
#125768=CARTESIAN_POINT('Ctrl Pts',(-7.22520787530932,43.1308190809083,
44.7921402324464));
#125769=CARTESIAN_POINT('Ctrl Pts',(-7.24981968793656,43.1339357989149,
44.7992497365215));
#125770=CARTESIAN_POINT('Ctrl Pts',(-7.26172119707253,43.13624393064,44.8045280031557));
#125771=CARTESIAN_POINT('Ctrl Pts',(-7.29537069273696,43.1446590481209,
44.8240319462818));
#125772=CARTESIAN_POINT('Ctrl Pts',(-7.31492435500479,43.1524197100444,
44.8423192550511));
#125773=CARTESIAN_POINT('Ctrl Pts',(-7.35294574461562,43.1708382902919,
44.8871870557474));
#125774=CARTESIAN_POINT('Ctrl Pts',(-7.37368596111585,43.1848338692446,
44.9227502546591));
#125775=CARTESIAN_POINT('Ctrl Pts',(-7.42230928437433,43.2240280671579,
45.0280938938583));
#125776=CARTESIAN_POINT('Ctrl Pts',(-7.44506219926235,43.2552667477377,
45.1240810706962));
#125777=CARTESIAN_POINT('Ctrl Pts',(-7.49721225591251,43.34385822923,45.4469741746507));
#125778=CARTESIAN_POINT('Ctrl Pts',(-7.49636431121142,43.3847241392164,
45.7473663615792));
#125779=CARTESIAN_POINT('Ctrl Pts',(-7.49636431121142,43.3847241392164,
46.2526336384208));
#125780=CARTESIAN_POINT('Ctrl Pts',(-7.49721225591251,43.34385822923,46.5530258253493));
#125781=CARTESIAN_POINT('Ctrl Pts',(-7.44506219926235,43.2552667477377,
46.8759189293038));
#125782=CARTESIAN_POINT('Ctrl Pts',(-7.42230928437433,43.2240280671579,
46.9719061061417));
#125783=CARTESIAN_POINT('Ctrl Pts',(-7.37368596111585,43.1848338692446,
47.0772497453409));
#125784=CARTESIAN_POINT('Ctrl Pts',(-7.35294574461562,43.1708382902919,
47.1128129442526));
#125785=CARTESIAN_POINT('Ctrl Pts',(-7.31492435500479,43.1524197100444,
47.1576807449489));
#125786=CARTESIAN_POINT('Ctrl Pts',(-7.29537069273696,43.1446590481209,
47.1759680537182));
#125787=CARTESIAN_POINT('Ctrl Pts',(-7.26172119707253,43.13624393064,47.1954719968443));
#125788=CARTESIAN_POINT('Ctrl Pts',(-7.24981968793656,43.1339357989149,
47.2007502634786));
#125789=CARTESIAN_POINT('Ctrl Pts',(-7.22520787530932,43.1308190809083,
47.2078597675536));
#125790=CARTESIAN_POINT('Ctrl Pts',(-7.21250680486427,43.1299979186738,
47.209717421885));
#125791=CARTESIAN_POINT('Ctrl Pts',(-7.19981081806464,43.1299974654728,
47.209717421885));
#125792=CARTESIAN_POINT('',(-4.88081081954212,43.1299146855279,44.7902825781149));
#125793=CARTESIAN_POINT('',(-25.9993307420611,43.1306685406019,44.7902825781153));
#125794=CARTESIAN_POINT('',(-4.31517414500253,41.7642090685172,43.3360352829528));
#125795=CARTESIAN_POINT('Ctrl Pts',(-4.31517414500254,41.7642090685172,
43.3360352829528));
#125796=CARTESIAN_POINT('Ctrl Pts',(-4.2390225654459,41.8403552115938,43.3754708104887));
#125797=CARTESIAN_POINT('Ctrl Pts',(-4.17859647402362,41.9330114055893,
43.4279311643908));
#125798=CARTESIAN_POINT('Ctrl Pts',(-4.09805029004739,42.1312231898084,
43.5578023393987));
#125799=CARTESIAN_POINT('Ctrl Pts',(-4.08084269258332,42.2370080209205,
43.6370616773385));
#125800=CARTESIAN_POINT('Ctrl Pts',(-4.08083503287425,42.4515873535033,
43.8198327604385));
#125801=CARTESIAN_POINT('Ctrl Pts',(-4.10948896604543,42.5724250222423,
43.9407914802036));
#125802=CARTESIAN_POINT('Ctrl Pts',(-4.21173521992966,42.7838888359608,
44.191589177584));
#125803=CARTESIAN_POINT('Ctrl Pts',(-4.28473708613121,42.8747600616692,
44.3214618221658));
#125804=CARTESIAN_POINT('Ctrl Pts',(-4.42918588082232,42.9947395232464,
44.5180261720106));
#125805=CARTESIAN_POINT('Ctrl Pts',(-4.50299531310249,43.0409837535405,
44.6037770994266));
#125806=CARTESIAN_POINT('Ctrl Pts',(-4.63083615831866,43.0912259898174,
44.7055023937998));
#125807=CARTESIAN_POINT('Ctrl Pts',(-4.67621148812537,43.104869821818,44.7347631376419));
#125808=CARTESIAN_POINT('Ctrl Pts',(-4.77320031795728,43.1241916785181,
44.7771726331388));
#125809=CARTESIAN_POINT('Ctrl Pts',(-4.82482221472671,43.1299126869364,
44.7902825781148));
#125810=CARTESIAN_POINT('Ctrl Pts',(-4.88081081954212,43.1299146855279,
44.7902825781148));
#125811=CARTESIAN_POINT('',(-5.69482187817968,40.384659828731,43.));
#125812=CARTESIAN_POINT('Origin',(-5.69482187817972,40.3846598287309,46.));
#125813=CARTESIAN_POINT('',(5.69537693071232,40.384253239671,43.));
#125814=CARTESIAN_POINT('',(-25.9994287388058,40.3853846300409,43.));
#125815=CARTESIAN_POINT('',(4.3155751451931,41.7640550251902,43.3361150636597));
#125816=CARTESIAN_POINT('Origin',(5.69537693071237,40.3842532396709,46.));
#125817=CARTESIAN_POINT('',(4.88126057014233,43.1297404501394,44.7906780580687));
#125818=CARTESIAN_POINT('Ctrl Pts',(4.88126057014233,43.1297404501394,44.7906780580686));
#125819=CARTESIAN_POINT('Ctrl Pts',(4.82527855129633,43.1297404501394,44.7906735213083));
#125820=CARTESIAN_POINT('Ctrl Pts',(4.77366641546815,43.1240229215084,44.7775580917314));
#125821=CARTESIAN_POINT('Ctrl Pts',(4.6766881693441,43.1047100794269,44.7351374178226));
#125822=CARTESIAN_POINT('Ctrl Pts',(4.63131473335929,43.0910704365374,44.7058682945448));
#125823=CARTESIAN_POINT('Ctrl Pts',(4.50347730469684,43.040841140764,44.6041166977585));
#125824=CARTESIAN_POINT('Ctrl Pts',(4.42966809762419,42.9946063244288,44.5183478507339));
#125825=CARTESIAN_POINT('Ctrl Pts',(4.28521059479939,42.8746430433406,44.3217402796909));
#125826=CARTESIAN_POINT('Ctrl Pts',(4.21219885970608,42.7837779689826,44.1918390912013));
#125827=CARTESIAN_POINT('Ctrl Pts',(4.10993073305515,42.5723177386494,43.9409875062198));
#125828=CARTESIAN_POINT('Ctrl Pts',(4.08126491520575,42.4514774729932,43.8200033709792));
#125829=CARTESIAN_POINT('Ctrl Pts',(4.08125725528774,42.2368922872938,43.6371990515189));
#125830=CARTESIAN_POINT('Ctrl Pts',(4.09845674449903,42.1311064778841,43.5579277928478));
#125831=CARTESIAN_POINT('Ctrl Pts',(4.17899207419104,41.9328803074183,43.4280312090116));
#125832=CARTESIAN_POINT('Ctrl Pts',(4.23941854432906,41.8402116260542,43.375558776258));
#125833=CARTESIAN_POINT('Ctrl Pts',(4.31557514519307,41.7640550251902,43.3361150636597));
#125834=CARTESIAN_POINT('',(7.20026057014233,43.1297404501395,44.7908660063353));
#125835=CARTESIAN_POINT('',(6.04076057014233,43.1297404501395,44.790772032202));
#125836=CARTESIAN_POINT('',(7.20026057014233,43.1297404501395,47.2091339936647));
#125837=CARTESIAN_POINT('Ctrl Pts',(7.20026057014233,43.1297404501395,47.2091339936647));
#125838=CARTESIAN_POINT('Ctrl Pts',(7.21294682501949,43.1297404501395,47.2091329653848));
#125839=CARTESIAN_POINT('Ctrl Pts',(7.22563810372133,43.1305598955788,47.2072760701667));
#125840=CARTESIAN_POINT('Ctrl Pts',(7.25023479260245,43.1336713801016,47.2001704115751));
#125841=CARTESIAN_POINT('Ctrl Pts',(7.26213075345329,43.1359764055222,47.1948942718855));
#125842=CARTESIAN_POINT('Ctrl Pts',(7.29576491915057,43.144380828481,47.1753983698309));
#125843=CARTESIAN_POINT('Ctrl Pts',(7.31531022822448,43.152132358212,47.1571188348341));
#125844=CARTESIAN_POINT('Ctrl Pts',(7.35331775020092,43.1705301900497,47.1122694969576));
#125845=CARTESIAN_POINT('Ctrl Pts',(7.3740522567382,43.1845108420159,47.0767203752737));
#125846=CARTESIAN_POINT('Ctrl Pts',(7.4226663467744,43.2236642757062,46.9714177547315));
#125847=CARTESIAN_POINT('Ctrl Pts',(7.44542247694709,43.2548716957552,46.8754679026737));
#125848=CARTESIAN_POINT('Ctrl Pts',(7.49758960390303,43.3433662832606,46.5527314566462));
#125849=CARTESIAN_POINT('Ctrl Pts',(7.49678217092917,43.3841889379055,46.2524977920887));
#125850=CARTESIAN_POINT('Ctrl Pts',(7.49678217092917,43.3841889379055,45.7475022079113));
#125851=CARTESIAN_POINT('Ctrl Pts',(7.49758960390303,43.3433662832606,45.4472685433538));
#125852=CARTESIAN_POINT('Ctrl Pts',(7.44542247694709,43.2548716957552,45.1245320973263));
#125853=CARTESIAN_POINT('Ctrl Pts',(7.4226663467744,43.2236642757062,45.0285822452685));
#125854=CARTESIAN_POINT('Ctrl Pts',(7.3740522567382,43.1845108420159,44.9232796247263));
#125855=CARTESIAN_POINT('Ctrl Pts',(7.35331775020092,43.1705301900497,44.8877305030425));
#125856=CARTESIAN_POINT('Ctrl Pts',(7.31531022822448,43.152132358212,44.8428811651659));
#125857=CARTESIAN_POINT('Ctrl Pts',(7.29576491915057,43.144380828481,44.8246016301691));
#125858=CARTESIAN_POINT('Ctrl Pts',(7.26213075345329,43.1359764055222,44.8051057281145));
#125859=CARTESIAN_POINT('Ctrl Pts',(7.25023479260246,43.1336713801016,44.7998295884249));
#125860=CARTESIAN_POINT('Ctrl Pts',(7.22563810372133,43.1305598955788,44.7927239298333));
#125861=CARTESIAN_POINT('Ctrl Pts',(7.2129468250195,43.1297404501395,44.7908670346152));
#125862=CARTESIAN_POINT('Ctrl Pts',(7.20026057014233,43.1297404501395,44.7908660063354));
#125863=CARTESIAN_POINT('',(4.88126057014233,43.1297404501394,47.2093219419313));
#125864=CARTESIAN_POINT('',(6.04076057014233,43.1297404501395,47.209227967798));
#125865=CARTESIAN_POINT('',(4.3155751451931,41.7640550251902,48.6638849363403));
#125866=CARTESIAN_POINT('Ctrl Pts',(4.31557514519307,41.7640550251902,48.6638849363403));
#125867=CARTESIAN_POINT('Ctrl Pts',(4.23941854432905,41.8402116260542,48.624441223742));
#125868=CARTESIAN_POINT('Ctrl Pts',(4.17899207419104,41.9328803074183,48.5719687909884));
#125869=CARTESIAN_POINT('Ctrl Pts',(4.09845674449903,42.1311064778841,48.4420722071522));
#125870=CARTESIAN_POINT('Ctrl Pts',(4.08125725528774,42.2368922872938,48.3628009484811));
#125871=CARTESIAN_POINT('Ctrl Pts',(4.08126491520575,42.4514774729932,48.1799966290209));
#125872=CARTESIAN_POINT('Ctrl Pts',(4.10993073305514,42.5723177386493,48.0590124937802));
#125873=CARTESIAN_POINT('Ctrl Pts',(4.21219885970608,42.7837779689826,47.8081609087987));
#125874=CARTESIAN_POINT('Ctrl Pts',(4.28521059479939,42.8746430433406,47.6782597203091));
#125875=CARTESIAN_POINT('Ctrl Pts',(4.42966809762419,42.9946063244288,47.4816521492661));
#125876=CARTESIAN_POINT('Ctrl Pts',(4.50347730469684,43.040841140764,47.3958833022415));
#125877=CARTESIAN_POINT('Ctrl Pts',(4.63131473335929,43.0910704365374,47.2941317054552));
#125878=CARTESIAN_POINT('Ctrl Pts',(4.6766881693441,43.1047100794269,47.2648625821774));
#125879=CARTESIAN_POINT('Ctrl Pts',(4.77366641546815,43.1240229215084,47.2224419082686));
#125880=CARTESIAN_POINT('Ctrl Pts',(4.82527855129632,43.1297404501394,47.2093264786917));
#125881=CARTESIAN_POINT('Ctrl Pts',(4.88126057014233,43.1297404501394,47.2093219419314));
#125882=CARTESIAN_POINT('',(6.03525883703878,40.0443713333445,48.9806859172054));
#125883=CARTESIAN_POINT('Origin',(5.69537693071237,40.3842532396709,46.));
#125884=CARTESIAN_POINT('',(9.57079274297153,38.5799052392773,48.3968369781132));
#125885=CARTESIAN_POINT('Ctrl Pts',(9.57079274297153,38.5799052392773,48.3968369781133));
#125886=CARTESIAN_POINT('Ctrl Pts',(9.5707332488234,38.5799052392773,48.3968369765146));
#125887=CARTESIAN_POINT('Ctrl Pts',(9.5706737548282,38.5799052403392,48.3968369757153));
#125888=CARTESIAN_POINT('Ctrl Pts',(8.88909486927775,38.5799295702497,48.3968369757153));
#125889=CARTESIAN_POINT('Ctrl Pts',(8.1875100639932,38.724779883745,48.519320896401));
#125890=CARTESIAN_POINT('Ctrl Pts',(6.98374971135328,39.2566553618154,48.7942694455703));
#125891=CARTESIAN_POINT('Ctrl Pts',(6.4652044862175,39.6144256841659,48.9316635383853));
#125892=CARTESIAN_POINT('Ctrl Pts',(6.03525883703881,40.0443713333445,48.9806859172054));
#125893=CARTESIAN_POINT('',(11.6717927429715,38.5799052392773,48.3968934308243));
#125894=CARTESIAN_POINT('',(10.6212927429715,38.5799052392773,48.3968652044688));
#125895=CARTESIAN_POINT('',(13.0860063053446,39.1656916769042,48.7414869339534));
#125896=CARTESIAN_POINT('Ctrl Pts',(13.0860063053446,39.1656916769042,48.7414869339534));
#125897=CARTESIAN_POINT('Ctrl Pts',(12.9115776150688,38.9912629866284,48.663969269128));
#125898=CARTESIAN_POINT('Ctrl Pts',(12.6925492447761,38.8399015743528,48.5750351340623));
#125899=CARTESIAN_POINT('Ctrl Pts',(12.2039210685268,38.6336428861301,48.4395838913209));
#125900=CARTESIAN_POINT('Ctrl Pts',(11.9328135534399,38.5799052392773,48.3969004440812));
#125901=CARTESIAN_POINT('Ctrl Pts',(11.6717927429715,38.5799052392773,48.3968934308244));
#125902=CARTESIAN_POINT('',(13.9076643850834,39.987349756643,48.973667809827));
#125903=CARTESIAN_POINT('Origin',(14.3042605619825,40.383945933542,46.));
#125904=CARTESIAN_POINT('',(14.2005576038968,40.6944565378947,48.9838876432241));
#125905=CARTESIAN_POINT('Ctrl Pts',(14.2005576038968,40.6944565378295,48.9838876425972));
#125906=CARTESIAN_POINT('Ctrl Pts',(14.2005576038968,40.6944446389709,48.9838888808066));
#125907=CARTESIAN_POINT('Ctrl Pts',(14.2005576036844,40.6944327401719,48.9838901189378));
#125908=CARTESIAN_POINT('Ctrl Pts',(14.2005531444961,40.5695128967916,48.996887916041));
#125909=CARTESIAN_POINT('Ctrl Pts',(14.1756575752172,40.4358460629751,49.0020722846323));
#125910=CARTESIAN_POINT('Ctrl Pts',(14.0741268986634,40.1899012740497,48.9962434199587));
#125911=CARTESIAN_POINT('Ctrl Pts',(13.9975074091711,40.0776069665203,48.9856559212044));
#125912=CARTESIAN_POINT('Ctrl Pts',(13.9087580506029,39.988444692808,48.9738136974118));
#125913=CARTESIAN_POINT('Ctrl Pts',(13.9082116449317,39.9878970164913,48.9737408027343));
#125914=CARTESIAN_POINT('Ctrl Pts',(13.9076643850834,39.987349756643,48.973667809827));
#125915=CARTESIAN_POINT('',(14.2005576038968,42.6304565378295,47.9882672716729));
#125916=CARTESIAN_POINT('Origin',(14.2005576038968,40.383949635364,46.));
#125917=CARTESIAN_POINT('',(13.7005576038968,43.1304565378295,47.2069788251679));
#125918=CARTESIAN_POINT('Ctrl Pts',(13.7005576038968,43.1304565378295,47.206978825168));
#125919=CARTESIAN_POINT('Ctrl Pts',(13.7005635533611,43.1304565378295,47.2069788246847));
#125920=CARTESIAN_POINT('Ctrl Pts',(13.7005695027606,43.1304565377233,47.2069788244431));
#125921=CARTESIAN_POINT('Ctrl Pts',(13.7349434333177,43.1304553106978,47.2069788244431));
#125922=CARTESIAN_POINT('Ctrl Pts',(13.7667215268191,43.1269938687308,47.2149030662356));
#125923=CARTESIAN_POINT('Ctrl Pts',(13.8263020113281,43.1153320791706,47.240899990775));
#125924=CARTESIAN_POINT('Ctrl Pts',(13.8540993385831,43.1071092325231,47.2589741809338));
#125925=CARTESIAN_POINT('Ctrl Pts',(13.9319395673727,43.0771707831725,47.3224216534088));
#125926=CARTESIAN_POINT('Ctrl Pts',(13.9761986813102,43.0500508066361,47.3767434803275));
#125927=CARTESIAN_POINT('Ctrl Pts',(14.070024541769,42.9755247782782,47.5143570677025));
#125928=CARTESIAN_POINT('Ctrl Pts',(14.1174300227276,42.916521123884,47.6124763023577));
#125929=CARTESIAN_POINT('Ctrl Pts',(14.1829744042219,42.7817463851036,47.8068079086529));
#125930=CARTESIAN_POINT('Ctrl Pts',(14.2005576038968,42.7058286960662,47.9031056458044));
#125931=CARTESIAN_POINT('Ctrl Pts',(14.2005576038968,42.6304565378295,47.9882672716729));
#125932=CARTESIAN_POINT('',(12.8005576038968,43.1304565378295,47.2070519271956));
#125933=CARTESIAN_POINT('',(13.2505576038968,43.1304565378295,47.2070153761818));
#125934=CARTESIAN_POINT('',(12.8005576038968,43.1304565378295,44.7929480728044));
#125935=CARTESIAN_POINT('Ctrl Pts',(12.8005576038968,43.1304565378295,44.7929480728044));
#125936=CARTESIAN_POINT('Ctrl Pts',(12.8005540342567,43.1304565378295,44.7929480725144));
#125937=CARTESIAN_POINT('Ctrl Pts',(12.800550464617,43.1304565378932,44.7929480723695));
#125938=CARTESIAN_POINT('Ctrl Pts',(12.8005468949777,43.1304565380206,44.7929480723695));
#125939=CARTESIAN_POINT('Ctrl Pts',(12.7878790745653,43.1304569902162,44.7929480723695));
#125940=CARTESIAN_POINT('Ctrl Pts',(12.775206184161,43.1312745218071,44.7948023896052));
#125941=CARTESIAN_POINT('Ctrl Pts',(12.7506486750991,43.1343773655443,44.801898883713));
#125942=CARTESIAN_POINT('Ctrl Pts',(12.738773266856,43.1366751949132,44.8071674273607));
#125943=CARTESIAN_POINT('Ctrl Pts',(12.7051965550664,43.1450524580709,44.826634614644));
#125944=CARTESIAN_POINT('Ctrl Pts',(12.6856835914487,43.1527778071505,44.8448863925531));
#125945=CARTESIAN_POINT('Ctrl Pts',(12.6477316006356,43.1711140657731,44.8896697992274));
#125946=CARTESIAN_POINT('Ctrl Pts',(12.6270220730305,43.1850482619964,44.9251686425469));
#125947=CARTESIAN_POINT('Ctrl Pts',(12.5784538537086,43.2240722091775,45.0303247407441));
#125948=CARTESIAN_POINT('Ctrl Pts',(12.5556965844494,43.2551755942419,45.126141257432));
#125949=CARTESIAN_POINT('Ctrl Pts',(12.5034979555493,43.3433419209884,45.4483186441275));
#125950=CARTESIAN_POINT('Ctrl Pts',(12.5041748497398,43.3840101920279,45.7479867774995));
#125951=CARTESIAN_POINT('Ctrl Pts',(12.5041748497398,43.3840101920279,46.2520132225005));
#125952=CARTESIAN_POINT('Ctrl Pts',(12.5034979555493,43.3433419209884,46.5516813558725));
#125953=CARTESIAN_POINT('Ctrl Pts',(12.5556965844494,43.2551755942419,46.873858742568));
#125954=CARTESIAN_POINT('Ctrl Pts',(12.5784538537086,43.2240722091775,46.9696752592559));
#125955=CARTESIAN_POINT('Ctrl Pts',(12.6270220730305,43.1850482619964,47.0748313574531));
#125956=CARTESIAN_POINT('Ctrl Pts',(12.6477316006356,43.1711140657731,47.1103302007727));
#125957=CARTESIAN_POINT('Ctrl Pts',(12.6856835914487,43.1527778071505,47.1551136074469));
#125958=CARTESIAN_POINT('Ctrl Pts',(12.7051965550664,43.1450524580709,47.173365385356));
#125959=CARTESIAN_POINT('Ctrl Pts',(12.738773266856,43.1366751949132,47.1928325726393));
#125960=CARTESIAN_POINT('Ctrl Pts',(12.7506486750991,43.1343773655443,47.198101116287));
#125961=CARTESIAN_POINT('Ctrl Pts',(12.775206184161,43.1312745218071,47.2051976103948));
#125962=CARTESIAN_POINT('Ctrl Pts',(12.7878790745653,43.1304569902162,47.2070519276305));
#125963=CARTESIAN_POINT('Ctrl Pts',(12.800550464617,43.1304565378932,47.2070519276305));
#125964=CARTESIAN_POINT('Ctrl Pts',(12.8005540342567,43.1304565378295,47.2070519274856));
#125965=CARTESIAN_POINT('Ctrl Pts',(12.8005576038968,43.1304565378295,47.2070519271956));
#125966=CARTESIAN_POINT('',(13.7005576038968,43.1304565378295,44.7930211748321));
#125967=CARTESIAN_POINT('',(13.2505576038968,43.1304565378295,44.7929846238182));
#125968=CARTESIAN_POINT('',(14.2005576038968,42.6304565378295,44.0117327283271));
#125969=CARTESIAN_POINT('Ctrl Pts',(14.2005576038968,42.6304565378295,44.0117327283271));
#125970=CARTESIAN_POINT('Ctrl Pts',(14.2005576038968,42.7058286960662,44.0968943541956));
#125971=CARTESIAN_POINT('Ctrl Pts',(14.1829744042219,42.7817463851036,44.1931920913471));
#125972=CARTESIAN_POINT('Ctrl Pts',(14.1174300227276,42.916521123884,44.3875236976423));
#125973=CARTESIAN_POINT('Ctrl Pts',(14.070024541769,42.9755247782782,44.4856429322975));
#125974=CARTESIAN_POINT('Ctrl Pts',(13.9761986813102,43.0500508066361,44.6232565196725));
#125975=CARTESIAN_POINT('Ctrl Pts',(13.9319395673727,43.0771707831725,44.6775783465912));
#125976=CARTESIAN_POINT('Ctrl Pts',(13.8540993385831,43.1071092325231,44.7410258190662));
#125977=CARTESIAN_POINT('Ctrl Pts',(13.8263020113281,43.1153320791706,44.759100009225));
#125978=CARTESIAN_POINT('Ctrl Pts',(13.7667215268191,43.1269938687308,44.7850969337644));
#125979=CARTESIAN_POINT('Ctrl Pts',(13.7349434333177,43.1304553106978,44.7930211755569));
#125980=CARTESIAN_POINT('Ctrl Pts',(13.7005695027606,43.1304565377233,44.7930211755569));
#125981=CARTESIAN_POINT('Ctrl Pts',(13.7005635533611,43.1304565378295,44.7930211753153));
#125982=CARTESIAN_POINT('Ctrl Pts',(13.7005576038968,43.1304565378295,44.793021174832));
#125983=CARTESIAN_POINT('',(14.2005576038968,40.6944565378947,43.0161123567759));
#125984=CARTESIAN_POINT('Origin',(14.2005576038968,40.383949635364,46.));
#125985=CARTESIAN_POINT('',(14.1511293052103,40.3839513998532,43.));
#125986=CARTESIAN_POINT('Ctrl Pts',(14.1511293052103,40.3839513999301,43.));
#125987=CARTESIAN_POINT('Ctrl Pts',(14.184533612433,40.4862144071147,43.0000000000053));
#125988=CARTESIAN_POINT('Ctrl Pts',(14.2005539915515,40.5932423327881,43.0055811103851));
#125989=CARTESIAN_POINT('Ctrl Pts',(14.2005576036844,40.6944327401719,43.0161098810622));
#125990=CARTESIAN_POINT('Ctrl Pts',(14.2005576038968,40.6944446389709,43.0161111191934));
#125991=CARTESIAN_POINT('Ctrl Pts',(14.2005576038968,40.6944565378295,43.0161123574028));
#125992=CARTESIAN_POINT('',(16.0005576038968,40.3838853818492,42.9999999980887));
#125993=CARTESIAN_POINT('',(-25.9994287388058,40.3853846300409,43.));
#125994=CARTESIAN_POINT('Origin',(16.0005576038968,40.3838853818492,46.));
#125995=CARTESIAN_POINT('Origin',(16.0005576038968,40.3838853818492,46.));
#125996=CARTESIAN_POINT('',(13.9076643850834,39.987349756643,43.026332190173));
#125997=CARTESIAN_POINT('Ctrl Pts',(13.9076643850834,39.987349756643,43.026332190173));
#125998=CARTESIAN_POINT('Ctrl Pts',(13.9082116449317,39.9878970164913,43.0262591972657));
#125999=CARTESIAN_POINT('Ctrl Pts',(13.9087580506029,39.988444692808,43.0261863025882));
#126000=CARTESIAN_POINT('Ctrl Pts',(13.9975074091711,40.0776069665203,43.0143440787957));
#126001=CARTESIAN_POINT('Ctrl Pts',(14.0741268986634,40.1899012740497,43.0037565800413));
#126002=CARTESIAN_POINT('Ctrl Pts',(14.1345364020809,40.3362353976012,43.0002884772731));
#126003=CARTESIAN_POINT('Ctrl Pts',(14.1432949797111,40.3599676160584,42.9999999999988));
#126004=CARTESIAN_POINT('Ctrl Pts',(14.1511293052103,40.3839513999301,43.));
#126005=CARTESIAN_POINT('',(13.0860063053446,39.1656916769042,43.2585130660466));
#126006=CARTESIAN_POINT('Origin',(14.3042605619825,40.383945933542,46.));
#126007=CARTESIAN_POINT('',(11.6717927429715,38.5799052392773,43.6031065691757));
#126008=CARTESIAN_POINT('Ctrl Pts',(11.6717927429715,38.5799052392773,43.6031065691757));
#126009=CARTESIAN_POINT('Ctrl Pts',(11.9328135534399,38.5799052392773,43.6030995559188));
#126010=CARTESIAN_POINT('Ctrl Pts',(12.2039210685268,38.6336428861301,43.5604161086791));
#126011=CARTESIAN_POINT('Ctrl Pts',(12.6925492447761,38.8399015743528,43.4249648659377));
#126012=CARTESIAN_POINT('Ctrl Pts',(12.9115776150688,38.9912629866284,43.3360307308721));
#126013=CARTESIAN_POINT('Ctrl Pts',(13.0860063053446,39.1656916769042,43.2585130660466));
#126014=CARTESIAN_POINT('',(9.57079274297153,38.5799052392773,43.6031630218867));
#126015=CARTESIAN_POINT('',(10.6212927429715,38.5799052392773,43.6031347955312));
#126016=CARTESIAN_POINT('',(6.03525883703878,40.0443713333445,43.0193140827946));
#126017=CARTESIAN_POINT('Ctrl Pts',(6.03525883703881,40.0443713333445,43.0193140827946));
#126018=CARTESIAN_POINT('Ctrl Pts',(6.4652044862175,39.6144256841659,43.0683364616148));
#126019=CARTESIAN_POINT('Ctrl Pts',(6.98374971135328,39.2566553618154,43.2057305544297));
#126020=CARTESIAN_POINT('Ctrl Pts',(8.1875100639932,38.724779883745,43.480679103599));
#126021=CARTESIAN_POINT('Ctrl Pts',(8.88909486927775,38.5799295702497,43.6031630242847));
#126022=CARTESIAN_POINT('Ctrl Pts',(9.570614260986,38.5799052424629,43.6031630242847));
#126023=CARTESIAN_POINT('Ctrl Pts',(9.5706737548282,38.5799052403392,43.6031630242847));
#126024=CARTESIAN_POINT('Ctrl Pts',(9.5707332488234,38.5799052392773,43.6031630234854));
#126025=CARTESIAN_POINT('Ctrl Pts',(9.57079274297153,38.5799052392773,43.6031630218867));
#126026=CARTESIAN_POINT('Origin',(5.69537693071237,40.3842532396709,46.));
#126027=CARTESIAN_POINT('',(-6.03491922226453,40.0445867642791,43.019338654981));
#126028=CARTESIAN_POINT('Origin',(-5.69482187817972,40.3846598287309,46.));
#126029=CARTESIAN_POINT('',(-9.57050540210797,38.5802468769672,43.6034202264699));
#126030=CARTESIAN_POINT('Ctrl Pts',(-9.57050540210795,38.5802468769672,
43.60342022647));
#126031=CARTESIAN_POINT('Ctrl Pts',(-8.88897256914252,38.5802225487005,
43.60342022647));
#126032=CARTESIAN_POINT('Ctrl Pts',(-8.18737580567769,38.7250267702563,
43.480898503507));
#126033=CARTESIAN_POINT('Ctrl Pts',(-6.98352950944328,39.2568425175939,
43.2058517696258));
#126034=CARTESIAN_POINT('Ctrl Pts',(-6.46491979272286,39.6146168916673,
43.0683987779396));
#126035=CARTESIAN_POINT('Ctrl Pts',(-6.03491922226454,40.0445867642791,
43.019338654981));
#126036=CARTESIAN_POINT('',(-11.6715054007694,38.5803218750975,43.6034202264699));
#126037=CARTESIAN_POINT('',(-25.9994931547856,38.5808333326384,43.6034202264699));
#126038=CARTESIAN_POINT('',(-13.0856980517762,39.1661587946801,43.2587206975987));
#126039=CARTESIAN_POINT('Ctrl Pts',(-13.0856980517762,39.1661587946801,
43.2587206975987));
#126040=CARTESIAN_POINT('Ctrl Pts',(-12.9106059326522,38.9910541747943,
43.3365689270393));
#126041=CARTESIAN_POINT('Ctrl Pts',(-12.6901619533851,38.8388876989633,
43.4261076675721));
#126042=CARTESIAN_POINT('Ctrl Pts',(-12.2008654839661,38.6335041042048,
43.5611995838646));
#126043=CARTESIAN_POINT('Ctrl Pts',(-11.9310804859103,38.5803311409929,
43.6034202264699));
#126044=CARTESIAN_POINT('Ctrl Pts',(-11.6715054007694,38.5803218750975,
43.6034202264699));
#126045=CARTESIAN_POINT('',(-13.9073268007583,39.9878462041285,43.0263984455991));
#126046=CARTESIAN_POINT('Origin',(-14.3044194064105,40.3849671603434,46.));
#126047=CARTESIAN_POINT('Ctrl Pts',(-13.9073268007584,39.9878462041285,
43.0263984455991));
#126048=CARTESIAN_POINT('Ctrl Pts',(-13.9960100566734,40.076535791615,43.0145549020595));
#126049=CARTESIAN_POINT('Ctrl Pts',(-14.0730534099154,40.1890412751135,
43.0038655192316));
#126050=CARTESIAN_POINT('Ctrl Pts',(-14.1339891648514,40.3361862550399,
43.0003015081353));
#126051=CARTESIAN_POINT('Ctrl Pts',(-14.1429487704599,40.3604431105938,
42.9999999999987));
#126052=CARTESIAN_POINT('Ctrl Pts',(-14.1509424007594,40.384961681931,43.));
#126053=CARTESIAN_POINT('Origin',(16.0005712344353,40.3838853813626,66.));
#126054=CARTESIAN_POINT('',(16.0005576038968,40.0020390449739,63.0244003328805));
#126055=CARTESIAN_POINT('',(16.0005576038968,40.0020390449739,68.9755996671195));
#126056=CARTESIAN_POINT('',(16.0005576038968,40.0020390450537,46.));
#126057=CARTESIAN_POINT('Origin',(16.0005712344353,40.3838853813626,66.));
#126058=CARTESIAN_POINT('Origin',(-25.9994287388058,40.3853846300409,66.));
#126059=CARTESIAN_POINT('',(-16.000205842957,40.3850276938095,63.));
#126060=CARTESIAN_POINT('Origin',(-16.000205842957,40.3850276938095,66.));
#126061=CARTESIAN_POINT('',(-14.1509424007594,40.3849616818491,63.));
#126062=CARTESIAN_POINT('',(-25.9994287388058,40.3853846300409,63.));
#126063=CARTESIAN_POINT('',(-14.2001947782207,40.6949634400972,63.0160596520708));
#126064=CARTESIAN_POINT('Ctrl Pts',(-14.1509424007594,40.384961681931,63.));
#126065=CARTESIAN_POINT('Ctrl Pts',(-14.1842343067511,40.4870767337193,
63.0000000000056));
#126066=CARTESIAN_POINT('Ctrl Pts',(-14.2001983851187,40.5939196884095,
63.0055622696198));
#126067=CARTESIAN_POINT('Ctrl Pts',(-14.2001947782208,40.6949634400972,
63.0160596520708));
#126068=CARTESIAN_POINT('',(-14.200125669996,42.6309634388637,64.0111601371654));
#126069=CARTESIAN_POINT('Origin',(-14.2002058441038,40.3849634402947,66.));
#126070=CARTESIAN_POINT('',(-13.700107822116,43.1309455903466,64.7919089438291));
#126071=CARTESIAN_POINT('Ctrl Pts',(-13.700107822116,43.1309455903466,64.7919089438292));
#126072=CARTESIAN_POINT('Ctrl Pts',(-13.7287138176145,43.1309466114776,
64.7919089438292));
#126073=CARTESIAN_POINT('Ctrl Pts',(-13.7588198896061,43.1282901354821,
64.7858171356271));
#126074=CARTESIAN_POINT('Ctrl Pts',(-13.8150242028358,43.1184187630571,
64.7637668516514));
#126075=CARTESIAN_POINT('Ctrl Pts',(-13.8411536038327,43.1112169321056,
64.7478820248202));
#126076=CARTESIAN_POINT('Ctrl Pts',(-13.942146077159,43.0763467034421,64.6731422398801));
#126077=CARTESIAN_POINT('Ctrl Pts',(-14.0082080214715,43.0299667749565,
64.5814744645503));
#126078=CARTESIAN_POINT('Ctrl Pts',(-14.1423359864052,42.8958483854512,
64.3486366205185));
#126079=CARTESIAN_POINT('Ctrl Pts',(-14.2001209716938,42.7625818225232,
64.1597969859191));
#126080=CARTESIAN_POINT('Ctrl Pts',(-14.2001256699959,42.6309634388638,
64.0111601371654));
#126081=CARTESIAN_POINT('',(-12.8001078226894,43.1309134635892,64.7919089438291));
#126082=CARTESIAN_POINT('',(-25.9993307164994,43.1313846282914,64.7919089438291));
#126083=CARTESIAN_POINT('',(-12.8001078226894,43.1309134635892,67.2080910561709));
#126084=CARTESIAN_POINT('Ctrl Pts',(-12.8001078226893,43.1309134635892,
67.2080910561709));
#126085=CARTESIAN_POINT('Ctrl Pts',(-12.7874290218161,43.1309130110017,
67.2080910561709));
#126086=CARTESIAN_POINT('Ctrl Pts',(-12.7747450872089,43.1317310514822,
67.2062354373186));
#126087=CARTESIAN_POINT('Ctrl Pts',(-12.7501661862404,43.1348375455173,
67.199133868969));
#126088=CARTESIAN_POINT('Ctrl Pts',(-12.7382804382214,43.1371385398321,
67.193861533145));
#126089=CARTESIAN_POINT('Ctrl Pts',(-12.7046747516163,43.1455281504129,
67.1743800110828));
#126090=CARTESIAN_POINT('Ctrl Pts',(-12.6851453672407,43.1532658613644,
67.1561143770981));
#126091=CARTESIAN_POINT('Ctrl Pts',(-12.6471649980075,43.1716314784724,
67.111298056684));
#126092=CARTESIAN_POINT('Ctrl Pts',(-12.6264424973877,43.1855881094717,
67.0757741121274));
#126093=CARTESIAN_POINT('Ctrl Pts',(-12.5778499600881,43.224674918756,66.9705448594992));
#126094=CARTESIAN_POINT('Ctrl Pts',(-12.5550921166024,43.2558293923731,
66.8746617707269));
#126095=CARTESIAN_POINT('Ctrl Pts',(-12.5029059493652,43.3441575831397,
66.5522053662921));
#126096=CARTESIAN_POINT('Ctrl Pts',(-12.5036463989442,43.3849028811463,
66.2522550206409));
#126097=CARTESIAN_POINT('Ctrl Pts',(-12.5036463989442,43.3849028811463,
65.7477449793591));
#126098=CARTESIAN_POINT('Ctrl Pts',(-12.5029059493652,43.3441575831397,
65.4477946337079));
#126099=CARTESIAN_POINT('Ctrl Pts',(-12.5550921166024,43.2558293923731,
65.1253382292731));
#126100=CARTESIAN_POINT('Ctrl Pts',(-12.5778499600881,43.224674918756,65.0294551405009));
#126101=CARTESIAN_POINT('Ctrl Pts',(-12.6264424973877,43.1855881094717,
64.9242258878726));
#126102=CARTESIAN_POINT('Ctrl Pts',(-12.6471649980075,43.1716314784724,
64.888701943316));
#126103=CARTESIAN_POINT('Ctrl Pts',(-12.6851453672407,43.1532658613644,
64.8438856229019));
#126104=CARTESIAN_POINT('Ctrl Pts',(-12.7046747516163,43.1455281504129,
64.8256199889173));
#126105=CARTESIAN_POINT('Ctrl Pts',(-12.7382804382214,43.1371385398321,
64.806138466855));
#126106=CARTESIAN_POINT('Ctrl Pts',(-12.7501661862404,43.1348375455173,
64.800866131031));
#126107=CARTESIAN_POINT('Ctrl Pts',(-12.7747450872089,43.1317310514822,
64.7937645626814));
#126108=CARTESIAN_POINT('Ctrl Pts',(-12.7874290218161,43.1309130110017,
64.7919089438292));
#126109=CARTESIAN_POINT('Ctrl Pts',(-12.8001078226893,43.1309134635892,
64.7919089438292));
#126110=CARTESIAN_POINT('',(-13.700107822116,43.1309455903466,67.2080910561709));
#126111=CARTESIAN_POINT('',(-25.9993307164994,43.1313846282914,67.2080910561709));
#126112=CARTESIAN_POINT('',(-14.200125669996,42.6309634388637,67.9888398628346));
#126113=CARTESIAN_POINT('Ctrl Pts',(-14.2001256699959,42.6309634388638,
67.9888398628346));
#126114=CARTESIAN_POINT('Ctrl Pts',(-14.2001209716939,42.7625818225232,
67.8402030140809));
#126115=CARTESIAN_POINT('Ctrl Pts',(-14.1423359864052,42.8958483854512,
67.6513633794815));
#126116=CARTESIAN_POINT('Ctrl Pts',(-14.0082080214715,43.0299667749565,
67.4185255354497));
#126117=CARTESIAN_POINT('Ctrl Pts',(-13.942146077159,43.0763467034421,67.3268577601199));
#126118=CARTESIAN_POINT('Ctrl Pts',(-13.8411536038327,43.1112169321056,
67.2521179751798));
#126119=CARTESIAN_POINT('Ctrl Pts',(-13.8150242028358,43.1184187630571,
67.2362331483486));
#126120=CARTESIAN_POINT('Ctrl Pts',(-13.7588198896061,43.1282901354821,
67.2141828643729));
#126121=CARTESIAN_POINT('Ctrl Pts',(-13.7287138176144,43.1309466114776,
67.2080910561708));
#126122=CARTESIAN_POINT('Ctrl Pts',(-13.7001078221159,43.1309455903466,
67.2080910561708));
#126123=CARTESIAN_POINT('',(-14.2001947782207,40.6949634400972,68.9839403479292));
#126124=CARTESIAN_POINT('Origin',(-14.2002058441038,40.3849634402947,66.));
#126125=CARTESIAN_POINT('',(-13.9073268007583,39.9878462041285,68.9736015544009));
#126126=CARTESIAN_POINT('Ctrl Pts',(-13.9073268007584,39.9878462041285,
68.973601554401));
#126127=CARTESIAN_POINT('Ctrl Pts',(-13.9960100566734,40.076535791615,68.9854450979406));
#126128=CARTESIAN_POINT('Ctrl Pts',(-14.0730534099154,40.1890412751135,
68.9961344807684));
#126129=CARTESIAN_POINT('Ctrl Pts',(-14.1751560019799,40.435594122051,69.0021062582817));
#126130=CARTESIAN_POINT('Ctrl Pts',(-14.2001992511613,40.5696583440676,
68.9969582287394));
#126131=CARTESIAN_POINT('Ctrl Pts',(-14.2001947782208,40.6949634400972,
68.9839403479292));
#126132=CARTESIAN_POINT('',(-13.0856980517762,39.1661587946801,68.7412793024013));
#126133=CARTESIAN_POINT('Origin',(-14.3044194064105,40.3849671603434,66.));
#126134=CARTESIAN_POINT('',(-11.6715054007694,38.5803218750975,68.3965797735301));
#126135=CARTESIAN_POINT('Ctrl Pts',(-11.6715054007694,38.5803218750975,
68.3965797735301));
#126136=CARTESIAN_POINT('Ctrl Pts',(-11.9310804859103,38.5803311409929,
68.3965797735301));
#126137=CARTESIAN_POINT('Ctrl Pts',(-12.2008654839661,38.6335041042047,
68.4388004161354));
#126138=CARTESIAN_POINT('Ctrl Pts',(-12.6901619533851,38.8388876989633,
68.5738923324279));
#126139=CARTESIAN_POINT('Ctrl Pts',(-12.9106059326522,38.9910541747943,
68.6634310729608));
#126140=CARTESIAN_POINT('Ctrl Pts',(-13.0856980517762,39.1661587946801,
68.7412793024013));
#126141=CARTESIAN_POINT('',(-9.57050540210797,38.5802468769672,68.39657977353));
#126142=CARTESIAN_POINT('',(-25.9994931547856,38.5808333326384,68.3965797735301));
#126143=CARTESIAN_POINT('',(-6.03491922226453,40.0445867642791,68.980661345019));
#126144=CARTESIAN_POINT('Ctrl Pts',(-6.03491922226454,40.0445867642791,
68.980661345019));
#126145=CARTESIAN_POINT('Ctrl Pts',(-6.46491979272285,39.6146168916673,
68.9316012220604));
#126146=CARTESIAN_POINT('Ctrl Pts',(-6.98352950944328,39.2568425175939,
68.7941482303742));
#126147=CARTESIAN_POINT('Ctrl Pts',(-8.18737580567769,38.7250267702563,
68.519101496493));
#126148=CARTESIAN_POINT('Ctrl Pts',(-8.88897256914252,38.5802225487005,
68.39657977353));
#126149=CARTESIAN_POINT('Ctrl Pts',(-9.57050540210795,38.5802468769672,
68.39657977353));
#126150=CARTESIAN_POINT('',(-4.31517414500253,41.7642090685172,68.6639647170472));
#126151=CARTESIAN_POINT('Origin',(-5.69482187817972,40.3846598287309,66.));
#126152=CARTESIAN_POINT('',(-4.88081081954212,43.1299146855279,67.2097174218851));
#126153=CARTESIAN_POINT('Ctrl Pts',(-4.88081081954212,43.1299146855279,
67.2097174218852));
#126154=CARTESIAN_POINT('Ctrl Pts',(-4.82482221472671,43.1299126869364,
67.2097174218852));
#126155=CARTESIAN_POINT('Ctrl Pts',(-4.77320031795728,43.1241916785181,
67.2228273668612));
#126156=CARTESIAN_POINT('Ctrl Pts',(-4.67621148812539,43.104869821818,67.2652368623581));
#126157=CARTESIAN_POINT('Ctrl Pts',(-4.63083615831867,43.0912259898174,
67.2944976062002));
#126158=CARTESIAN_POINT('Ctrl Pts',(-4.5029953131025,43.0409837535405,67.3962229005734));
#126159=CARTESIAN_POINT('Ctrl Pts',(-4.42918588082232,42.9947395232464,
67.4819738279894));
#126160=CARTESIAN_POINT('Ctrl Pts',(-4.28473708613121,42.8747600616692,
67.6785381778342));
#126161=CARTESIAN_POINT('Ctrl Pts',(-4.21173521992966,42.7838888359608,
67.808410822416));
#126162=CARTESIAN_POINT('Ctrl Pts',(-4.10948896604543,42.5724250222423,
68.0592085197964));
#126163=CARTESIAN_POINT('Ctrl Pts',(-4.08083503287425,42.4515873535033,
68.1801672395615));
#126164=CARTESIAN_POINT('Ctrl Pts',(-4.08084269258332,42.2370080209205,
68.3629383226615));
#126165=CARTESIAN_POINT('Ctrl Pts',(-4.09805029004739,42.1312231898084,
68.4421976606013));
#126166=CARTESIAN_POINT('Ctrl Pts',(-4.17859647402362,41.9330114055893,
68.5720688356092));
#126167=CARTESIAN_POINT('Ctrl Pts',(-4.23902256544591,41.8403552115938,
68.6245291895113));
#126168=CARTESIAN_POINT('Ctrl Pts',(-4.31517414500254,41.7642090685172,
68.6639647170472));
#126169=CARTESIAN_POINT('',(-7.19981081806464,43.1299974654728,67.209717421885));
#126170=CARTESIAN_POINT('',(-25.9993307420611,43.1306685406019,67.2097174218847));
#126171=CARTESIAN_POINT('',(-7.19981081806464,43.1299974654728,64.790282578115));
#126172=CARTESIAN_POINT('Ctrl Pts',(-7.19981081806464,43.1299974654728,
64.790282578115));
#126173=CARTESIAN_POINT('Ctrl Pts',(-7.21250680486427,43.1299979186738,
64.790282578115));
#126174=CARTESIAN_POINT('Ctrl Pts',(-7.22520787530932,43.1308190809083,
64.7921402324464));
#126175=CARTESIAN_POINT('Ctrl Pts',(-7.24981968793656,43.1339357989149,
64.7992497365214));
#126176=CARTESIAN_POINT('Ctrl Pts',(-7.26172119707253,43.13624393064,64.8045280031557));
#126177=CARTESIAN_POINT('Ctrl Pts',(-7.29537069273696,43.1446590481209,
64.8240319462818));
#126178=CARTESIAN_POINT('Ctrl Pts',(-7.31492435500479,43.1524197100444,
64.8423192550511));
#126179=CARTESIAN_POINT('Ctrl Pts',(-7.35294574461562,43.1708382902919,
64.8871870557474));
#126180=CARTESIAN_POINT('Ctrl Pts',(-7.37368596111585,43.1848338692446,
64.9227502546591));
#126181=CARTESIAN_POINT('Ctrl Pts',(-7.42230928437433,43.2240280671579,
65.0280938938583));
#126182=CARTESIAN_POINT('Ctrl Pts',(-7.44506219926235,43.2552667477377,
65.1240810706962));
#126183=CARTESIAN_POINT('Ctrl Pts',(-7.49721225591251,43.34385822923,65.4469741746507));
#126184=CARTESIAN_POINT('Ctrl Pts',(-7.49636431121142,43.3847241392164,
65.7473663615792));
#126185=CARTESIAN_POINT('Ctrl Pts',(-7.49636431121142,43.3847241392164,
66.2526336384208));
#126186=CARTESIAN_POINT('Ctrl Pts',(-7.49721225591251,43.34385822923,66.5530258253493));
#126187=CARTESIAN_POINT('Ctrl Pts',(-7.44506219926235,43.2552667477377,
66.8759189293038));
#126188=CARTESIAN_POINT('Ctrl Pts',(-7.42230928437433,43.2240280671579,
66.9719061061417));
#126189=CARTESIAN_POINT('Ctrl Pts',(-7.37368596111585,43.1848338692446,
67.0772497453409));
#126190=CARTESIAN_POINT('Ctrl Pts',(-7.35294574461562,43.1708382902919,
67.1128129442526));
#126191=CARTESIAN_POINT('Ctrl Pts',(-7.31492435500479,43.1524197100444,
67.1576807449489));
#126192=CARTESIAN_POINT('Ctrl Pts',(-7.29537069273696,43.1446590481209,
67.1759680537182));
#126193=CARTESIAN_POINT('Ctrl Pts',(-7.26172119707253,43.13624393064,67.1954719968443));
#126194=CARTESIAN_POINT('Ctrl Pts',(-7.24981968793656,43.1339357989149,
67.2007502634786));
#126195=CARTESIAN_POINT('Ctrl Pts',(-7.22520787530932,43.1308190809083,
67.2078597675536));
#126196=CARTESIAN_POINT('Ctrl Pts',(-7.21250680486427,43.1299979186738,
67.209717421885));
#126197=CARTESIAN_POINT('Ctrl Pts',(-7.19981081806464,43.1299974654728,
67.209717421885));
#126198=CARTESIAN_POINT('',(-4.88081081954212,43.1299146855279,64.7902825781149));
#126199=CARTESIAN_POINT('',(-25.9993307420611,43.1306685406019,64.7902825781153));
#126200=CARTESIAN_POINT('',(-4.31517414500253,41.7642090685172,63.3360352829528));
#126201=CARTESIAN_POINT('Ctrl Pts',(-4.31517414500255,41.7642090685172,
63.3360352829528));
#126202=CARTESIAN_POINT('Ctrl Pts',(-4.23902256544591,41.8403552115938,
63.3754708104887));
#126203=CARTESIAN_POINT('Ctrl Pts',(-4.17859647402362,41.9330114055893,
63.4279311643908));
#126204=CARTESIAN_POINT('Ctrl Pts',(-4.09805029004739,42.1312231898084,
63.5578023393987));
#126205=CARTESIAN_POINT('Ctrl Pts',(-4.08084269258332,42.2370080209205,
63.6370616773385));
#126206=CARTESIAN_POINT('Ctrl Pts',(-4.08083503287425,42.4515873535033,
63.8198327604385));
#126207=CARTESIAN_POINT('Ctrl Pts',(-4.10948896604543,42.5724250222423,
63.9407914802036));
#126208=CARTESIAN_POINT('Ctrl Pts',(-4.21173521992966,42.7838888359608,
64.191589177584));
#126209=CARTESIAN_POINT('Ctrl Pts',(-4.28473708613121,42.8747600616692,
64.3214618221658));
#126210=CARTESIAN_POINT('Ctrl Pts',(-4.42918588082232,42.9947395232464,
64.5180261720106));
#126211=CARTESIAN_POINT('Ctrl Pts',(-4.50299531310249,43.0409837535405,
64.6037770994266));
#126212=CARTESIAN_POINT('Ctrl Pts',(-4.63083615831866,43.0912259898174,
64.7055023937998));
#126213=CARTESIAN_POINT('Ctrl Pts',(-4.67621148812537,43.104869821818,64.7347631376419));
#126214=CARTESIAN_POINT('Ctrl Pts',(-4.77320031795728,43.1241916785181,
64.7771726331388));
#126215=CARTESIAN_POINT('Ctrl Pts',(-4.82482221472671,43.1299126869364,
64.7902825781148));
#126216=CARTESIAN_POINT('Ctrl Pts',(-4.88081081954212,43.1299146855279,
64.7902825781148));
#126217=CARTESIAN_POINT('',(-5.69482187817968,40.384659828731,63.));
#126218=CARTESIAN_POINT('Origin',(-5.69482187817972,40.3846598287309,66.));
#126219=CARTESIAN_POINT('',(5.69537693071232,40.384253239671,63.));
#126220=CARTESIAN_POINT('',(-25.9994287388058,40.3853846300409,63.));
#126221=CARTESIAN_POINT('',(4.3155751451931,41.7640550251902,63.3361150636597));
#126222=CARTESIAN_POINT('Origin',(5.69537693071237,40.3842532396709,66.));
#126223=CARTESIAN_POINT('',(4.88126057014233,43.1297404501394,64.7906780580687));
#126224=CARTESIAN_POINT('Ctrl Pts',(4.88126057014233,43.1297404501394,64.7906780580686));
#126225=CARTESIAN_POINT('Ctrl Pts',(4.82527855129633,43.1297404501394,64.7906735213083));
#126226=CARTESIAN_POINT('Ctrl Pts',(4.77366641546815,43.1240229215084,64.7775580917314));
#126227=CARTESIAN_POINT('Ctrl Pts',(4.6766881693441,43.1047100794269,64.7351374178226));
#126228=CARTESIAN_POINT('Ctrl Pts',(4.63131473335929,43.0910704365374,64.7058682945448));
#126229=CARTESIAN_POINT('Ctrl Pts',(4.50347730469684,43.040841140764,64.6041166977585));
#126230=CARTESIAN_POINT('Ctrl Pts',(4.42966809762419,42.9946063244288,64.5183478507339));
#126231=CARTESIAN_POINT('Ctrl Pts',(4.28521059479939,42.8746430433406,64.3217402796909));
#126232=CARTESIAN_POINT('Ctrl Pts',(4.21219885970608,42.7837779689826,64.1918390912013));
#126233=CARTESIAN_POINT('Ctrl Pts',(4.10993073305515,42.5723177386493,63.9409875062198));
#126234=CARTESIAN_POINT('Ctrl Pts',(4.08126491520575,42.4514774729932,63.8200033709792));
#126235=CARTESIAN_POINT('Ctrl Pts',(4.08125725528774,42.2368922872938,63.6371990515189));
#126236=CARTESIAN_POINT('Ctrl Pts',(4.09845674449903,42.1311064778841,63.5579277928478));
#126237=CARTESIAN_POINT('Ctrl Pts',(4.17899207419104,41.9328803074183,63.4280312090116));
#126238=CARTESIAN_POINT('Ctrl Pts',(4.23941854432905,41.8402116260542,63.375558776258));
#126239=CARTESIAN_POINT('Ctrl Pts',(4.31557514519307,41.7640550251902,63.3361150636597));
#126240=CARTESIAN_POINT('',(7.20026057014233,43.1297404501395,64.7908660063353));
#126241=CARTESIAN_POINT('',(6.04076057014233,43.1297404501395,64.790772032202));
#126242=CARTESIAN_POINT('',(7.20026057014233,43.1297404501395,67.2091339936647));
#126243=CARTESIAN_POINT('Ctrl Pts',(7.20026057014233,43.1297404501395,67.2091339936646));
#126244=CARTESIAN_POINT('Ctrl Pts',(7.21294682501949,43.1297404501395,67.2091329653848));
#126245=CARTESIAN_POINT('Ctrl Pts',(7.22563810372133,43.1305598955788,67.2072760701667));
#126246=CARTESIAN_POINT('Ctrl Pts',(7.25023479260246,43.1336713801016,67.2001704115751));
#126247=CARTESIAN_POINT('Ctrl Pts',(7.26213075345329,43.1359764055222,67.1948942718855));
#126248=CARTESIAN_POINT('Ctrl Pts',(7.29576491915057,43.144380828481,67.1753983698309));
#126249=CARTESIAN_POINT('Ctrl Pts',(7.31531022822448,43.152132358212,67.1571188348341));
#126250=CARTESIAN_POINT('Ctrl Pts',(7.35331775020092,43.1705301900497,67.1122694969576));
#126251=CARTESIAN_POINT('Ctrl Pts',(7.3740522567382,43.1845108420159,67.0767203752738));
#126252=CARTESIAN_POINT('Ctrl Pts',(7.4226663467744,43.2236642757062,66.9714177547315));
#126253=CARTESIAN_POINT('Ctrl Pts',(7.44542247694709,43.2548716957552,66.8754679026737));
#126254=CARTESIAN_POINT('Ctrl Pts',(7.49758960390303,43.3433662832606,66.5527314566462));
#126255=CARTESIAN_POINT('Ctrl Pts',(7.49678217092917,43.3841889379055,66.2524977920887));
#126256=CARTESIAN_POINT('Ctrl Pts',(7.49678217092917,43.3841889379055,65.7475022079113));
#126257=CARTESIAN_POINT('Ctrl Pts',(7.49758960390303,43.3433662832606,65.4472685433538));
#126258=CARTESIAN_POINT('Ctrl Pts',(7.44542247694709,43.2548716957552,65.1245320973263));
#126259=CARTESIAN_POINT('Ctrl Pts',(7.4226663467744,43.2236642757062,65.0285822452685));
#126260=CARTESIAN_POINT('Ctrl Pts',(7.3740522567382,43.1845108420159,64.9232796247263));
#126261=CARTESIAN_POINT('Ctrl Pts',(7.35331775020091,43.1705301900497,64.8877305030424));
#126262=CARTESIAN_POINT('Ctrl Pts',(7.31531022822448,43.152132358212,64.8428811651659));
#126263=CARTESIAN_POINT('Ctrl Pts',(7.29576491915057,43.144380828481,64.8246016301691));
#126264=CARTESIAN_POINT('Ctrl Pts',(7.26213075345329,43.1359764055222,64.8051057281145));
#126265=CARTESIAN_POINT('Ctrl Pts',(7.25023479260246,43.1336713801016,64.7998295884249));
#126266=CARTESIAN_POINT('Ctrl Pts',(7.22563810372133,43.1305598955788,64.7927239298334));
#126267=CARTESIAN_POINT('Ctrl Pts',(7.21294682501949,43.1297404501395,64.7908670346152));
#126268=CARTESIAN_POINT('Ctrl Pts',(7.20026057014233,43.1297404501395,64.7908660063354));
#126269=CARTESIAN_POINT('',(4.88126057014233,43.1297404501394,67.2093219419313));
#126270=CARTESIAN_POINT('',(6.04076057014233,43.1297404501395,67.209227967798));
#126271=CARTESIAN_POINT('',(4.3155751451931,41.7640550251902,68.6638849363403));
#126272=CARTESIAN_POINT('Ctrl Pts',(4.31557514519307,41.7640550251902,68.6638849363403));
#126273=CARTESIAN_POINT('Ctrl Pts',(4.23941854432905,41.8402116260542,68.624441223742));
#126274=CARTESIAN_POINT('Ctrl Pts',(4.17899207419104,41.9328803074183,68.5719687909884));
#126275=CARTESIAN_POINT('Ctrl Pts',(4.09845674449903,42.1311064778841,68.4420722071522));
#126276=CARTESIAN_POINT('Ctrl Pts',(4.08125725528774,42.2368922872938,68.3628009484811));
#126277=CARTESIAN_POINT('Ctrl Pts',(4.08126491520575,42.4514774729932,68.1799966290208));
#126278=CARTESIAN_POINT('Ctrl Pts',(4.10993073305515,42.5723177386493,68.0590124937802));
#126279=CARTESIAN_POINT('Ctrl Pts',(4.21219885970608,42.7837779689826,67.8081609087987));
#126280=CARTESIAN_POINT('Ctrl Pts',(4.28521059479939,42.8746430433406,67.6782597203091));
#126281=CARTESIAN_POINT('Ctrl Pts',(4.42966809762419,42.9946063244288,67.4816521492661));
#126282=CARTESIAN_POINT('Ctrl Pts',(4.50347730469684,43.040841140764,67.3958833022415));
#126283=CARTESIAN_POINT('Ctrl Pts',(4.63131473335929,43.0910704365374,67.2941317054552));
#126284=CARTESIAN_POINT('Ctrl Pts',(4.6766881693441,43.1047100794269,67.2648625821774));
#126285=CARTESIAN_POINT('Ctrl Pts',(4.77366641546815,43.1240229215084,67.2224419082686));
#126286=CARTESIAN_POINT('Ctrl Pts',(4.82527855129632,43.1297404501394,67.2093264786917));
#126287=CARTESIAN_POINT('Ctrl Pts',(4.88126057014233,43.1297404501394,67.2093219419314));
#126288=CARTESIAN_POINT('',(6.03525883703878,40.0443713333445,68.9806859172054));
#126289=CARTESIAN_POINT('Origin',(5.69537693071237,40.3842532396709,66.));
#126290=CARTESIAN_POINT('',(9.57079274297153,38.5799052392773,68.3968369781133));
#126291=CARTESIAN_POINT('Ctrl Pts',(9.57079274297153,38.5799052392773,68.3968369781133));
#126292=CARTESIAN_POINT('Ctrl Pts',(9.5707332488234,38.5799052392773,68.3968369765146));
#126293=CARTESIAN_POINT('Ctrl Pts',(9.5706737548282,38.5799052403392,68.3968369757153));
#126294=CARTESIAN_POINT('Ctrl Pts',(8.88909486927775,38.5799295702497,68.3968369757153));
#126295=CARTESIAN_POINT('Ctrl Pts',(8.1875100639932,38.724779883745,68.5193208964011));
#126296=CARTESIAN_POINT('Ctrl Pts',(6.98374971135328,39.2566553618154,68.7942694455703));
#126297=CARTESIAN_POINT('Ctrl Pts',(6.46520448621751,39.6144256841658,68.9316635383853));
#126298=CARTESIAN_POINT('Ctrl Pts',(6.03525883703881,40.0443713333445,68.9806859172054));
#126299=CARTESIAN_POINT('',(11.6717927429715,38.5799052392773,68.3968934308243));
#126300=CARTESIAN_POINT('',(10.6212927429715,38.5799052392773,68.3968652044688));
#126301=CARTESIAN_POINT('',(13.0860063053446,39.1656916769042,68.7414869339534));
#126302=CARTESIAN_POINT('Ctrl Pts',(13.0860063053446,39.1656916769042,68.7414869339534));
#126303=CARTESIAN_POINT('Ctrl Pts',(12.9115776150688,38.9912629866284,68.663969269128));
#126304=CARTESIAN_POINT('Ctrl Pts',(12.6925492447761,38.8399015743528,68.5750351340623));
#126305=CARTESIAN_POINT('Ctrl Pts',(12.2039210685268,38.6336428861301,68.4395838913209));
#126306=CARTESIAN_POINT('Ctrl Pts',(11.9328135534399,38.5799052392773,68.3969004440812));
#126307=CARTESIAN_POINT('Ctrl Pts',(11.6717927429715,38.5799052392773,68.3968934308244));
#126308=CARTESIAN_POINT('',(13.9076643850834,39.987349756643,68.973667809827));
#126309=CARTESIAN_POINT('Origin',(14.3042605619825,40.383945933542,66.));
#126310=CARTESIAN_POINT('',(14.2005576038968,40.6944565378947,68.9838876432241));
#126311=CARTESIAN_POINT('Ctrl Pts',(14.2005576038968,40.6944565378295,68.9838876425972));
#126312=CARTESIAN_POINT('Ctrl Pts',(14.2005576038968,40.6944446389709,68.9838888808066));
#126313=CARTESIAN_POINT('Ctrl Pts',(14.2005576036844,40.6944327401719,68.9838901189378));
#126314=CARTESIAN_POINT('Ctrl Pts',(14.2005531444961,40.5695128967916,68.996887916041));
#126315=CARTESIAN_POINT('Ctrl Pts',(14.1756575752172,40.4358460629751,69.0020722846323));
#126316=CARTESIAN_POINT('Ctrl Pts',(14.0741268986634,40.1899012740497,68.9962434199587));
#126317=CARTESIAN_POINT('Ctrl Pts',(13.9975074091711,40.0776069665203,68.9856559212044));
#126318=CARTESIAN_POINT('Ctrl Pts',(13.9087580506029,39.988444692808,68.9738136974118));
#126319=CARTESIAN_POINT('Ctrl Pts',(13.9082116449317,39.9878970164913,68.9737408027343));
#126320=CARTESIAN_POINT('Ctrl Pts',(13.9076643850834,39.987349756643,68.973667809827));
#126321=CARTESIAN_POINT('',(14.2005576038968,42.6304565378295,67.9882672716729));
#126322=CARTESIAN_POINT('Origin',(14.2005576038968,40.383949635364,66.));
#126323=CARTESIAN_POINT('',(13.7005576038968,43.1304565378295,67.2069788251679));
#126324=CARTESIAN_POINT('Ctrl Pts',(13.7005576038968,43.1304565378295,67.206978825168));
#126325=CARTESIAN_POINT('Ctrl Pts',(13.7005635533611,43.1304565378295,67.2069788246847));
#126326=CARTESIAN_POINT('Ctrl Pts',(13.7005695027606,43.1304565377233,67.2069788244431));
#126327=CARTESIAN_POINT('Ctrl Pts',(13.7349434333177,43.1304553106978,67.2069788244431));
#126328=CARTESIAN_POINT('Ctrl Pts',(13.7667215268191,43.1269938687308,67.2149030662356));
#126329=CARTESIAN_POINT('Ctrl Pts',(13.8263020113281,43.1153320791706,67.240899990775));
#126330=CARTESIAN_POINT('Ctrl Pts',(13.8540993385831,43.1071092325231,67.2589741809338));
#126331=CARTESIAN_POINT('Ctrl Pts',(13.9319395673727,43.0771707831725,67.3224216534088));
#126332=CARTESIAN_POINT('Ctrl Pts',(13.9761986813102,43.0500508066361,67.3767434803275));
#126333=CARTESIAN_POINT('Ctrl Pts',(14.070024541769,42.9755247782782,67.5143570677025));
#126334=CARTESIAN_POINT('Ctrl Pts',(14.1174300227276,42.916521123884,67.6124763023577));
#126335=CARTESIAN_POINT('Ctrl Pts',(14.1829744042219,42.7817463851036,67.8068079086529));
#126336=CARTESIAN_POINT('Ctrl Pts',(14.2005576038968,42.7058286960662,67.9031056458045));
#126337=CARTESIAN_POINT('Ctrl Pts',(14.2005576038968,42.6304565378295,67.9882672716729));
#126338=CARTESIAN_POINT('',(12.8005576038968,43.1304565378295,67.2070519271956));
#126339=CARTESIAN_POINT('',(13.2505576038968,43.1304565378295,67.2070153761818));
#126340=CARTESIAN_POINT('',(12.8005576038968,43.1304565378295,64.7929480728044));
#126341=CARTESIAN_POINT('Ctrl Pts',(12.8005576038968,43.1304565378295,64.7929480728044));
#126342=CARTESIAN_POINT('Ctrl Pts',(12.8005540342567,43.1304565378295,64.7929480725144));
#126343=CARTESIAN_POINT('Ctrl Pts',(12.800550464617,43.1304565378932,64.7929480723695));
#126344=CARTESIAN_POINT('Ctrl Pts',(12.8005468949777,43.1304565380206,64.7929480723695));
#126345=CARTESIAN_POINT('Ctrl Pts',(12.7878790745653,43.1304569902162,64.7929480723695));
#126346=CARTESIAN_POINT('Ctrl Pts',(12.775206184161,43.1312745218071,64.7948023896052));
#126347=CARTESIAN_POINT('Ctrl Pts',(12.7506486750991,43.1343773655443,64.801898883713));
#126348=CARTESIAN_POINT('Ctrl Pts',(12.738773266856,43.1366751949132,64.8071674273607));
#126349=CARTESIAN_POINT('Ctrl Pts',(12.7051965550664,43.1450524580709,64.826634614644));
#126350=CARTESIAN_POINT('Ctrl Pts',(12.6856835914487,43.1527778071505,64.8448863925531));
#126351=CARTESIAN_POINT('Ctrl Pts',(12.6477316006356,43.1711140657731,64.8896697992273));
#126352=CARTESIAN_POINT('Ctrl Pts',(12.6270220730305,43.1850482619964,64.9251686425469));
#126353=CARTESIAN_POINT('Ctrl Pts',(12.5784538537086,43.2240722091775,65.0303247407441));
#126354=CARTESIAN_POINT('Ctrl Pts',(12.5556965844494,43.2551755942419,65.126141257432));
#126355=CARTESIAN_POINT('Ctrl Pts',(12.5034979555493,43.3433419209884,65.4483186441275));
#126356=CARTESIAN_POINT('Ctrl Pts',(12.5041748497398,43.3840101920279,65.7479867774995));
#126357=CARTESIAN_POINT('Ctrl Pts',(12.5041748497398,43.3840101920279,66.2520132225005));
#126358=CARTESIAN_POINT('Ctrl Pts',(12.5034979555493,43.3433419209884,66.5516813558725));
#126359=CARTESIAN_POINT('Ctrl Pts',(12.5556965844494,43.2551755942419,66.873858742568));
#126360=CARTESIAN_POINT('Ctrl Pts',(12.5784538537086,43.2240722091775,66.9696752592559));
#126361=CARTESIAN_POINT('Ctrl Pts',(12.6270220730305,43.1850482619964,67.0748313574531));
#126362=CARTESIAN_POINT('Ctrl Pts',(12.6477316006356,43.1711140657731,67.1103302007727));
#126363=CARTESIAN_POINT('Ctrl Pts',(12.6856835914487,43.1527778071505,67.1551136074469));
#126364=CARTESIAN_POINT('Ctrl Pts',(12.7051965550664,43.1450524580709,67.173365385356));
#126365=CARTESIAN_POINT('Ctrl Pts',(12.738773266856,43.1366751949132,67.1928325726393));
#126366=CARTESIAN_POINT('Ctrl Pts',(12.7506486750991,43.1343773655443,67.198101116287));
#126367=CARTESIAN_POINT('Ctrl Pts',(12.775206184161,43.1312745218071,67.2051976103948));
#126368=CARTESIAN_POINT('Ctrl Pts',(12.7878790745653,43.1304569902162,67.2070519276305));
#126369=CARTESIAN_POINT('Ctrl Pts',(12.800550464617,43.1304565378932,67.2070519276305));
#126370=CARTESIAN_POINT('Ctrl Pts',(12.8005540342567,43.1304565378295,67.2070519274856));
#126371=CARTESIAN_POINT('Ctrl Pts',(12.8005576038968,43.1304565378295,67.2070519271956));
#126372=CARTESIAN_POINT('',(13.7005576038968,43.1304565378295,64.7930211748321));
#126373=CARTESIAN_POINT('',(13.2505576038968,43.1304565378295,64.7929846238182));
#126374=CARTESIAN_POINT('',(14.2005576038968,42.6304565378295,64.0117327283271));
#126375=CARTESIAN_POINT('Ctrl Pts',(14.2005576038968,42.6304565378295,64.0117327283271));
#126376=CARTESIAN_POINT('Ctrl Pts',(14.2005576038968,42.7058286960662,64.0968943541956));
#126377=CARTESIAN_POINT('Ctrl Pts',(14.1829744042219,42.7817463851036,64.1931920913471));
#126378=CARTESIAN_POINT('Ctrl Pts',(14.1174300227276,42.916521123884,64.3875236976423));
#126379=CARTESIAN_POINT('Ctrl Pts',(14.070024541769,42.9755247782782,64.4856429322975));
#126380=CARTESIAN_POINT('Ctrl Pts',(13.9761986813102,43.0500508066361,64.6232565196725));
#126381=CARTESIAN_POINT('Ctrl Pts',(13.9319395673727,43.0771707831725,64.6775783465912));
#126382=CARTESIAN_POINT('Ctrl Pts',(13.8540993385831,43.1071092325231,64.7410258190662));
#126383=CARTESIAN_POINT('Ctrl Pts',(13.8263020113281,43.1153320791706,64.759100009225));
#126384=CARTESIAN_POINT('Ctrl Pts',(13.7667215268191,43.1269938687308,64.7850969337644));
#126385=CARTESIAN_POINT('Ctrl Pts',(13.7349434333177,43.1304553106978,64.7930211755569));
#126386=CARTESIAN_POINT('Ctrl Pts',(13.7005695027606,43.1304565377233,64.7930211755569));
#126387=CARTESIAN_POINT('Ctrl Pts',(13.7005635533611,43.1304565378295,64.7930211753153));
#126388=CARTESIAN_POINT('Ctrl Pts',(13.7005576038968,43.1304565378295,64.793021174832));
#126389=CARTESIAN_POINT('',(14.2005576038968,40.6944565378947,63.0161123567759));
#126390=CARTESIAN_POINT('Origin',(14.2005576038968,40.383949635364,66.));
#126391=CARTESIAN_POINT('',(14.1511293052103,40.3839513998532,63.));
#126392=CARTESIAN_POINT('Ctrl Pts',(14.1511293052103,40.3839513999301,63.));
#126393=CARTESIAN_POINT('Ctrl Pts',(14.184533612433,40.4862144071147,63.0000000000053));
#126394=CARTESIAN_POINT('Ctrl Pts',(14.2005539915515,40.5932423327881,63.0055811103851));
#126395=CARTESIAN_POINT('Ctrl Pts',(14.2005576036844,40.6944327401719,63.0161098810622));
#126396=CARTESIAN_POINT('Ctrl Pts',(14.2005576038968,40.6944446389709,63.0161111191934));
#126397=CARTESIAN_POINT('Ctrl Pts',(14.2005576038968,40.6944565378295,63.0161123574028));
#126398=CARTESIAN_POINT('',(16.0005576038968,40.3838853818492,62.9999999980887));
#126399=CARTESIAN_POINT('',(-25.9994287388058,40.3853846300409,63.));
#126400=CARTESIAN_POINT('Origin',(16.0005576038968,40.3838853818492,66.));
#126401=CARTESIAN_POINT('Origin',(16.0005576038968,40.3838853818492,66.));
#126402=CARTESIAN_POINT('',(13.9076643850834,39.987349756643,63.026332190173));
#126403=CARTESIAN_POINT('Ctrl Pts',(13.9076643850834,39.987349756643,63.026332190173));
#126404=CARTESIAN_POINT('Ctrl Pts',(13.9082116449317,39.9878970164913,63.0262591972657));
#126405=CARTESIAN_POINT('Ctrl Pts',(13.9087580506029,39.988444692808,63.0261863025882));
#126406=CARTESIAN_POINT('Ctrl Pts',(13.9975074091711,40.0776069665203,63.0143440787957));
#126407=CARTESIAN_POINT('Ctrl Pts',(14.0741268986634,40.1899012740497,63.0037565800413));
#126408=CARTESIAN_POINT('Ctrl Pts',(14.1345364020809,40.3362353976012,63.0002884772731));
#126409=CARTESIAN_POINT('Ctrl Pts',(14.1432949797111,40.3599676160584,62.9999999999988));
#126410=CARTESIAN_POINT('Ctrl Pts',(14.1511293052103,40.3839513999301,63.));
#126411=CARTESIAN_POINT('',(13.0860063053446,39.1656916769042,63.2585130660466));
#126412=CARTESIAN_POINT('Origin',(14.3042605619825,40.383945933542,66.));
#126413=CARTESIAN_POINT('',(11.6717927429715,38.5799052392773,63.6031065691757));
#126414=CARTESIAN_POINT('Ctrl Pts',(11.6717927429715,38.5799052392773,63.6031065691757));
#126415=CARTESIAN_POINT('Ctrl Pts',(11.9328135534399,38.5799052392773,63.6030995559188));
#126416=CARTESIAN_POINT('Ctrl Pts',(12.2039210685268,38.6336428861301,63.5604161086791));
#126417=CARTESIAN_POINT('Ctrl Pts',(12.6925492447761,38.8399015743528,63.4249648659377));
#126418=CARTESIAN_POINT('Ctrl Pts',(12.9115776150688,38.9912629866284,63.3360307308721));
#126419=CARTESIAN_POINT('Ctrl Pts',(13.0860063053446,39.1656916769042,63.2585130660466));
#126420=CARTESIAN_POINT('',(9.57079274297153,38.5799052392773,63.6031630218867));
#126421=CARTESIAN_POINT('',(10.6212927429715,38.5799052392773,63.6031347955312));
#126422=CARTESIAN_POINT('',(6.03525883703878,40.0443713333445,63.0193140827946));
#126423=CARTESIAN_POINT('Ctrl Pts',(6.03525883703881,40.0443713333445,63.0193140827946));
#126424=CARTESIAN_POINT('Ctrl Pts',(6.4652044862175,39.6144256841659,63.0683364616148));
#126425=CARTESIAN_POINT('Ctrl Pts',(6.98374971135328,39.2566553618154,63.2057305544297));
#126426=CARTESIAN_POINT('Ctrl Pts',(8.1875100639932,38.724779883745,63.480679103599));
#126427=CARTESIAN_POINT('Ctrl Pts',(8.88909486927775,38.5799295702497,63.6031630242847));
#126428=CARTESIAN_POINT('Ctrl Pts',(9.570614260986,38.5799052424629,63.6031630242847));
#126429=CARTESIAN_POINT('Ctrl Pts',(9.5706737548282,38.5799052403392,63.6031630242847));
#126430=CARTESIAN_POINT('Ctrl Pts',(9.5707332488234,38.5799052392773,63.6031630234854));
#126431=CARTESIAN_POINT('Ctrl Pts',(9.57079274297153,38.5799052392773,63.6031630218867));
#126432=CARTESIAN_POINT('Origin',(5.69537693071237,40.3842532396709,66.));
#126433=CARTESIAN_POINT('',(-6.03491922226453,40.0445867642791,63.019338654981));
#126434=CARTESIAN_POINT('Origin',(-5.69482187817972,40.3846598287309,66.));
#126435=CARTESIAN_POINT('',(-9.57050540210797,38.5802468769672,63.6034202264699));
#126436=CARTESIAN_POINT('Ctrl Pts',(-9.57050540210795,38.5802468769672,
63.60342022647));
#126437=CARTESIAN_POINT('Ctrl Pts',(-8.88897256914252,38.5802225487005,
63.60342022647));
#126438=CARTESIAN_POINT('Ctrl Pts',(-8.18737580567769,38.7250267702563,
63.480898503507));
#126439=CARTESIAN_POINT('Ctrl Pts',(-6.98352950944327,39.2568425175939,
63.2058517696258));
#126440=CARTESIAN_POINT('Ctrl Pts',(-6.46491979272285,39.6146168916673,
63.0683987779396));
#126441=CARTESIAN_POINT('Ctrl Pts',(-6.03491922226453,40.0445867642791,
63.019338654981));
#126442=CARTESIAN_POINT('',(-11.6715054007694,38.5803218750975,63.6034202264699));
#126443=CARTESIAN_POINT('',(-25.9994931547856,38.5808333326384,63.6034202264699));
#126444=CARTESIAN_POINT('',(-13.0856980517762,39.1661587946801,63.2587206975987));
#126445=CARTESIAN_POINT('Ctrl Pts',(-13.0856980517762,39.1661587946801,
63.2587206975987));
#126446=CARTESIAN_POINT('Ctrl Pts',(-12.9106059326522,38.9910541747943,
63.3365689270392));
#126447=CARTESIAN_POINT('Ctrl Pts',(-12.6901619533851,38.8388876989633,
63.4261076675721));
#126448=CARTESIAN_POINT('Ctrl Pts',(-12.2008654839661,38.6335041042048,
63.5611995838646));
#126449=CARTESIAN_POINT('Ctrl Pts',(-11.9310804859103,38.5803311409929,
63.6034202264699));
#126450=CARTESIAN_POINT('Ctrl Pts',(-11.6715054007694,38.5803218750975,
63.6034202264699));
#126451=CARTESIAN_POINT('',(-13.9073268007583,39.9878462041285,63.0263984455991));
#126452=CARTESIAN_POINT('Origin',(-14.3044194064105,40.3849671603434,66.));
#126453=CARTESIAN_POINT('Ctrl Pts',(-13.9073268007584,39.9878462041285,
63.0263984455991));
#126454=CARTESIAN_POINT('Ctrl Pts',(-13.9960100566734,40.076535791615,63.0145549020595));
#126455=CARTESIAN_POINT('Ctrl Pts',(-14.0730534099154,40.1890412751135,
63.0038655192316));
#126456=CARTESIAN_POINT('Ctrl Pts',(-14.1339891648514,40.3361862550399,
63.0003015081353));
#126457=CARTESIAN_POINT('Ctrl Pts',(-14.1429487704599,40.3604431105938,
62.9999999999987));
#126458=CARTESIAN_POINT('Ctrl Pts',(-14.1509424007594,40.384961681931,63.));
#126459=CARTESIAN_POINT('Origin',(16.0005712344353,40.3838853813626,86.));
#126460=CARTESIAN_POINT('',(16.0005576038968,40.0020390449739,83.0244003328805));
#126461=CARTESIAN_POINT('',(16.0005576038968,40.0020390449739,88.9755996671195));
#126462=CARTESIAN_POINT('',(16.0005576038968,40.0020390450537,56.));
#126463=CARTESIAN_POINT('Origin',(16.0005712344353,40.3838853813626,86.));
#126464=CARTESIAN_POINT('Origin',(-25.9994287388058,40.3853846300409,86.));
#126465=CARTESIAN_POINT('',(-16.000205842957,40.3850276938095,83.));
#126466=CARTESIAN_POINT('Origin',(-16.000205842957,40.3850276938095,86.));
#126467=CARTESIAN_POINT('',(-14.1509424007594,40.3849616818491,83.));
#126468=CARTESIAN_POINT('',(-25.9994287388058,40.3853846300409,83.));
#126469=CARTESIAN_POINT('',(-14.2001947782207,40.6949634400972,83.0160596520708));
#126470=CARTESIAN_POINT('Ctrl Pts',(-14.1509424007594,40.384961681931,83.));
#126471=CARTESIAN_POINT('Ctrl Pts',(-14.1842343067511,40.4870767337193,
83.0000000000055));
#126472=CARTESIAN_POINT('Ctrl Pts',(-14.2001983851187,40.5939196884095,
83.0055622696198));
#126473=CARTESIAN_POINT('Ctrl Pts',(-14.2001947782208,40.6949634400972,
83.0160596520708));
#126474=CARTESIAN_POINT('',(-14.200125669996,42.6309634388637,84.0111601371654));
#126475=CARTESIAN_POINT('Origin',(-14.2002058441038,40.3849634402947,86.));
#126476=CARTESIAN_POINT('',(-13.700107822116,43.1309455903466,84.7919089438291));
#126477=CARTESIAN_POINT('Ctrl Pts',(-13.700107822116,43.1309455903466,84.7919089438292));
#126478=CARTESIAN_POINT('Ctrl Pts',(-13.7344681318913,43.1309468168859,
84.7919089438292));
#126479=CARTESIAN_POINT('Ctrl Pts',(-13.76624790509,43.1274886274743,84.7839956698363));
#126480=CARTESIAN_POINT('Ctrl Pts',(-13.8258360433629,43.1158302297232,
84.7580245352879));
#126481=CARTESIAN_POINT('Ctrl Pts',(-13.8536394068926,43.1076076153794,
84.739965262305));
#126482=CARTESIAN_POINT('Ctrl Pts',(-13.9314960885267,43.0776671514126,
84.6765650238703));
#126483=CARTESIAN_POINT('Ctrl Pts',(-13.9757656431352,43.0505415815266,
84.6222760175062));
#126484=CARTESIAN_POINT('Ctrl Pts',(-14.0695955559554,42.9760100922221,
84.4847585375541));
#126485=CARTESIAN_POINT('Ctrl Pts',(-14.1169980465718,42.9170084867485,
84.3867107678662));
#126486=CARTESIAN_POINT('Ctrl Pts',(-14.1825405634598,42.7822411369273,
84.1925083525136));
#126487=CARTESIAN_POINT('Ctrl Pts',(-14.2001229797765,42.7063273319006,
84.0962687007213));
#126488=CARTESIAN_POINT('Ctrl Pts',(-14.2001256699959,42.6309634388638,
84.0111601371654));
#126489=CARTESIAN_POINT('',(-12.8001078226894,43.1309134635892,84.7919089438291));
#126490=CARTESIAN_POINT('',(-25.9993307164994,43.1313846282914,84.7919089438291));
#126491=CARTESIAN_POINT('',(-12.8001078226894,43.1309134635892,87.2080910561709));
#126492=CARTESIAN_POINT('Ctrl Pts',(-12.8001078226893,43.1309134635892,
87.2080910561709));
#126493=CARTESIAN_POINT('Ctrl Pts',(-12.7874290218161,43.1309130110017,
87.2080910561709));
#126494=CARTESIAN_POINT('Ctrl Pts',(-12.7747450872089,43.1317310514822,
87.2062354373186));
#126495=CARTESIAN_POINT('Ctrl Pts',(-12.7501661862404,43.1348375455173,
87.199133868969));
#126496=CARTESIAN_POINT('Ctrl Pts',(-12.7382804382214,43.1371385398321,
87.193861533145));
#126497=CARTESIAN_POINT('Ctrl Pts',(-12.7046747516163,43.1455281504129,
87.1743800110828));
#126498=CARTESIAN_POINT('Ctrl Pts',(-12.6851453672407,43.1532658613644,
87.1561143770981));
#126499=CARTESIAN_POINT('Ctrl Pts',(-12.6471649980075,43.1716314784724,
87.1112980566841));
#126500=CARTESIAN_POINT('Ctrl Pts',(-12.6264424973877,43.1855881094717,
87.0757741121274));
#126501=CARTESIAN_POINT('Ctrl Pts',(-12.5778499600881,43.224674918756,86.9705448594992));
#126502=CARTESIAN_POINT('Ctrl Pts',(-12.5550921166024,43.2558293923731,
86.8746617707269));
#126503=CARTESIAN_POINT('Ctrl Pts',(-12.5029059493652,43.3441575831397,
86.5522053662921));
#126504=CARTESIAN_POINT('Ctrl Pts',(-12.5036463989442,43.3849028811464,
86.2522550206409));
#126505=CARTESIAN_POINT('Ctrl Pts',(-12.5036463989442,43.3849028811464,
85.7477449793591));
#126506=CARTESIAN_POINT('Ctrl Pts',(-12.5029059493652,43.3441575831397,
85.4477946337079));
#126507=CARTESIAN_POINT('Ctrl Pts',(-12.5550921166024,43.2558293923731,
85.1253382292731));
#126508=CARTESIAN_POINT('Ctrl Pts',(-12.5778499600881,43.224674918756,85.0294551405008));
#126509=CARTESIAN_POINT('Ctrl Pts',(-12.6264424973877,43.1855881094717,
84.9242258878726));
#126510=CARTESIAN_POINT('Ctrl Pts',(-12.6471649980075,43.1716314784724,
84.8887019433159));
#126511=CARTESIAN_POINT('Ctrl Pts',(-12.6851453672407,43.1532658613644,
84.8438856229019));
#126512=CARTESIAN_POINT('Ctrl Pts',(-12.7046747516163,43.1455281504129,
84.8256199889172));
#126513=CARTESIAN_POINT('Ctrl Pts',(-12.7382804382214,43.1371385398321,
84.806138466855));
#126514=CARTESIAN_POINT('Ctrl Pts',(-12.7501661862404,43.1348375455173,
84.800866131031));
#126515=CARTESIAN_POINT('Ctrl Pts',(-12.7747450872088,43.1317310514822,
84.7937645626813));
#126516=CARTESIAN_POINT('Ctrl Pts',(-12.7874290218161,43.1309130110017,
84.7919089438291));
#126517=CARTESIAN_POINT('Ctrl Pts',(-12.8001078226893,43.1309134635892,
84.7919089438291));
#126518=CARTESIAN_POINT('',(-13.700107822116,43.1309455903466,87.2080910561709));
#126519=CARTESIAN_POINT('',(-25.9993307164994,43.1313846282914,87.2080910561709));
#126520=CARTESIAN_POINT('',(-14.200125669996,42.6309634388637,87.9888398628346));
#126521=CARTESIAN_POINT('Ctrl Pts',(-14.2001256699959,42.6309634388638,
87.9888398628346));
#126522=CARTESIAN_POINT('Ctrl Pts',(-14.2001229797765,42.7063273319006,
87.9037312992787));
#126523=CARTESIAN_POINT('Ctrl Pts',(-14.1825405634598,42.7822411369273,
87.8074916474864));
#126524=CARTESIAN_POINT('Ctrl Pts',(-14.1169980465718,42.9170084867485,
87.6132892321338));
#126525=CARTESIAN_POINT('Ctrl Pts',(-14.0695955559553,42.9760100922221,
87.5152414624458));
#126526=CARTESIAN_POINT('Ctrl Pts',(-13.9757656431352,43.0505415815266,
87.3777239824938));
#126527=CARTESIAN_POINT('Ctrl Pts',(-13.9314960885267,43.0776671514126,
87.3234349761297));
#126528=CARTESIAN_POINT('Ctrl Pts',(-13.8536394068926,43.1076076153794,
87.260034737695));
#126529=CARTESIAN_POINT('Ctrl Pts',(-13.8258360433629,43.1158302297232,
87.2419754647121));
#126530=CARTESIAN_POINT('Ctrl Pts',(-13.76624790509,43.1274886274743,87.2160043301637));
#126531=CARTESIAN_POINT('Ctrl Pts',(-13.7344681318912,43.1309468168859,
87.2080910561708));
#126532=CARTESIAN_POINT('Ctrl Pts',(-13.700107822116,43.1309455903466,87.2080910561708));
#126533=CARTESIAN_POINT('',(-14.2001947782207,40.6949634400972,88.9839403479292));
#126534=CARTESIAN_POINT('Origin',(-14.2002058441038,40.3849634402947,86.));
#126535=CARTESIAN_POINT('',(-13.9073268007584,39.9878462041285,88.9736015544009));
#126536=CARTESIAN_POINT('Ctrl Pts',(-13.9073268007584,39.9878462041285,
88.9736015544009));
#126537=CARTESIAN_POINT('Ctrl Pts',(-13.9960100566734,40.076535791615,88.9854450979405));
#126538=CARTESIAN_POINT('Ctrl Pts',(-14.0730534099154,40.1890412751135,
88.9961344807684));
#126539=CARTESIAN_POINT('Ctrl Pts',(-14.1751560019799,40.435594122051,89.0021062582817));
#126540=CARTESIAN_POINT('Ctrl Pts',(-14.2001992511613,40.5696583440676,
88.9969582287394));
#126541=CARTESIAN_POINT('Ctrl Pts',(-14.2001947782208,40.6949634400972,
88.9839403479292));
#126542=CARTESIAN_POINT('',(-13.0856980517762,39.1661587946801,88.7412793024013));
#126543=CARTESIAN_POINT('Origin',(-14.3044194064105,40.3849671603434,86.));
#126544=CARTESIAN_POINT('',(-11.6715054007694,38.5803218750975,88.3965797735301));
#126545=CARTESIAN_POINT('Ctrl Pts',(-11.6715054007694,38.5803218750975,
88.3965797735301));
#126546=CARTESIAN_POINT('Ctrl Pts',(-11.9310804859103,38.5803311409929,
88.3965797735301));
#126547=CARTESIAN_POINT('Ctrl Pts',(-12.2008654839661,38.6335041042048,
88.4388004161354));
#126548=CARTESIAN_POINT('Ctrl Pts',(-12.6901619533851,38.8388876989633,
88.5738923324279));
#126549=CARTESIAN_POINT('Ctrl Pts',(-12.9106059326522,38.9910541747943,
88.6634310729608));
#126550=CARTESIAN_POINT('Ctrl Pts',(-13.0856980517762,39.1661587946801,
88.7412793024013));
#126551=CARTESIAN_POINT('',(-9.57050540210797,38.5802468769672,88.3965797735301));
#126552=CARTESIAN_POINT('',(-25.9994931547856,38.5808333326384,88.3965797735301));
#126553=CARTESIAN_POINT('',(-6.03491922226453,40.0445867642791,88.980661345019));
#126554=CARTESIAN_POINT('Ctrl Pts',(-6.03491922226454,40.0445867642791,
88.980661345019));
#126555=CARTESIAN_POINT('Ctrl Pts',(-6.46491979272286,39.6146168916673,
88.9316012220604));
#126556=CARTESIAN_POINT('Ctrl Pts',(-6.98352950944328,39.2568425175939,
88.7941482303742));
#126557=CARTESIAN_POINT('Ctrl Pts',(-8.18737580567769,38.7250267702563,
88.519101496493));
#126558=CARTESIAN_POINT('Ctrl Pts',(-8.88897256914252,38.5802225487005,
88.3965797735301));
#126559=CARTESIAN_POINT('Ctrl Pts',(-9.57050540210795,38.5802468769672,
88.3965797735301));
#126560=CARTESIAN_POINT('',(-4.31517414500253,41.7642090685172,88.6639647170472));
#126561=CARTESIAN_POINT('Origin',(-5.69482187817972,40.3846598287309,86.));
#126562=CARTESIAN_POINT('',(-4.88081081954212,43.1299146855279,87.2097174218851));
#126563=CARTESIAN_POINT('Ctrl Pts',(-4.88081081954212,43.1299146855279,
87.2097174218852));
#126564=CARTESIAN_POINT('Ctrl Pts',(-4.82482221472671,43.1299126869364,
87.2097174218852));
#126565=CARTESIAN_POINT('Ctrl Pts',(-4.77320031795729,43.1241916785181,
87.2228273668612));
#126566=CARTESIAN_POINT('Ctrl Pts',(-4.67621148812538,43.104869821818,87.2652368623582));
#126567=CARTESIAN_POINT('Ctrl Pts',(-4.63083615831867,43.0912259898174,
87.2944976062003));
#126568=CARTESIAN_POINT('Ctrl Pts',(-4.50299531310251,43.0409837535405,
87.3962229005734));
#126569=CARTESIAN_POINT('Ctrl Pts',(-4.42918588082232,42.9947395232464,
87.4819738279894));
#126570=CARTESIAN_POINT('Ctrl Pts',(-4.28473708613121,42.8747600616692,
87.6785381778342));
#126571=CARTESIAN_POINT('Ctrl Pts',(-4.21173521992967,42.7838888359609,
87.808410822416));
#126572=CARTESIAN_POINT('Ctrl Pts',(-4.10948896604543,42.5724250222423,
88.0592085197964));
#126573=CARTESIAN_POINT('Ctrl Pts',(-4.08083503287426,42.4515873535033,
88.1801672395615));
#126574=CARTESIAN_POINT('Ctrl Pts',(-4.08084269258333,42.2370080209205,
88.3629383226615));
#126575=CARTESIAN_POINT('Ctrl Pts',(-4.09805029004739,42.1312231898084,
88.4421976606013));
#126576=CARTESIAN_POINT('Ctrl Pts',(-4.17859647402362,41.9330114055893,
88.5720688356092));
#126577=CARTESIAN_POINT('Ctrl Pts',(-4.23902256544591,41.8403552115938,
88.6245291895113));
#126578=CARTESIAN_POINT('Ctrl Pts',(-4.31517414500254,41.7642090685172,
88.6639647170472));
#126579=CARTESIAN_POINT('',(-7.19981081806464,43.1299974654728,87.209717421885));
#126580=CARTESIAN_POINT('',(-25.9993307420611,43.1306685406019,87.2097174218847));
#126581=CARTESIAN_POINT('',(-7.19981081806464,43.1299974654728,84.790282578115));
#126582=CARTESIAN_POINT('Ctrl Pts',(-7.19981081806464,43.1299974654728,
84.7902825781149));
#126583=CARTESIAN_POINT('Ctrl Pts',(-7.21250680486427,43.1299979186738,
84.7902825781149));
#126584=CARTESIAN_POINT('Ctrl Pts',(-7.22520787530932,43.1308190809083,
84.7921402324463));
#126585=CARTESIAN_POINT('Ctrl Pts',(-7.24981968793656,43.1339357989149,
84.7992497365214));
#126586=CARTESIAN_POINT('Ctrl Pts',(-7.26172119707253,43.13624393064,84.8045280031556));
#126587=CARTESIAN_POINT('Ctrl Pts',(-7.29537069273696,43.1446590481209,
84.8240319462817));
#126588=CARTESIAN_POINT('Ctrl Pts',(-7.31492435500479,43.1524197100444,
84.8423192550511));
#126589=CARTESIAN_POINT('Ctrl Pts',(-7.35294574461562,43.1708382902919,
84.8871870557474));
#126590=CARTESIAN_POINT('Ctrl Pts',(-7.37368596111585,43.1848338692446,
84.922750254659));
#126591=CARTESIAN_POINT('Ctrl Pts',(-7.42230928437433,43.2240280671579,
85.0280938938583));
#126592=CARTESIAN_POINT('Ctrl Pts',(-7.44506219926236,43.2552667477377,
85.1240810706962));
#126593=CARTESIAN_POINT('Ctrl Pts',(-7.49721225591252,43.34385822923,85.4469741746507));
#126594=CARTESIAN_POINT('Ctrl Pts',(-7.49636431121142,43.3847241392164,
85.7473663615792));
#126595=CARTESIAN_POINT('Ctrl Pts',(-7.49636431121142,43.3847241392164,
86.2526336384208));
#126596=CARTESIAN_POINT('Ctrl Pts',(-7.49721225591251,43.34385822923,86.5530258253493));
#126597=CARTESIAN_POINT('Ctrl Pts',(-7.44506219926236,43.2552667477377,
86.8759189293038));
#126598=CARTESIAN_POINT('Ctrl Pts',(-7.42230928437433,43.2240280671579,
86.9719061061417));
#126599=CARTESIAN_POINT('Ctrl Pts',(-7.37368596111585,43.1848338692446,
87.0772497453409));
#126600=CARTESIAN_POINT('Ctrl Pts',(-7.35294574461562,43.1708382902919,
87.1128129442526));
#126601=CARTESIAN_POINT('Ctrl Pts',(-7.31492435500479,43.1524197100444,
87.1576807449489));
#126602=CARTESIAN_POINT('Ctrl Pts',(-7.29537069273696,43.1446590481209,
87.1759680537183));
#126603=CARTESIAN_POINT('Ctrl Pts',(-7.26172119707253,43.13624393064,87.1954719968443));
#126604=CARTESIAN_POINT('Ctrl Pts',(-7.24981968793656,43.1339357989149,
87.2007502634786));
#126605=CARTESIAN_POINT('Ctrl Pts',(-7.22520787530932,43.1308190809083,
87.2078597675537));
#126606=CARTESIAN_POINT('Ctrl Pts',(-7.21250680486427,43.1299979186738,
87.209717421885));
#126607=CARTESIAN_POINT('Ctrl Pts',(-7.19981081806464,43.1299974654728,
87.2097174218851));
#126608=CARTESIAN_POINT('',(-4.88081081954212,43.1299146855279,84.7902825781149));
#126609=CARTESIAN_POINT('',(-25.9993307420611,43.1306685406019,84.7902825781153));
#126610=CARTESIAN_POINT('',(-4.31517414500253,41.7642090685172,83.3360352829528));
#126611=CARTESIAN_POINT('Ctrl Pts',(-4.31517414500253,41.7642090685172,
83.3360352829528));
#126612=CARTESIAN_POINT('Ctrl Pts',(-4.23902256544589,41.8403552115938,
83.3754708104887));
#126613=CARTESIAN_POINT('Ctrl Pts',(-4.17859647402362,41.9330114055893,
83.4279311643908));
#126614=CARTESIAN_POINT('Ctrl Pts',(-4.09805029004739,42.1312231898084,
83.5578023393987));
#126615=CARTESIAN_POINT('Ctrl Pts',(-4.08084269258333,42.2370080209205,
83.6370616773385));
#126616=CARTESIAN_POINT('Ctrl Pts',(-4.08083503287426,42.4515873535033,
83.8198327604385));
#126617=CARTESIAN_POINT('Ctrl Pts',(-4.10948896604541,42.5724250222423,
83.9407914802035));
#126618=CARTESIAN_POINT('Ctrl Pts',(-4.21173521992965,42.7838888359608,
84.191589177584));
#126619=CARTESIAN_POINT('Ctrl Pts',(-4.28473708613121,42.8747600616692,
84.3214618221658));
#126620=CARTESIAN_POINT('Ctrl Pts',(-4.42918588082232,42.9947395232464,
84.5180261720106));
#126621=CARTESIAN_POINT('Ctrl Pts',(-4.50299531310251,43.0409837535405,
84.6037770994266));
#126622=CARTESIAN_POINT('Ctrl Pts',(-4.63083615831867,43.0912259898174,
84.7055023937997));
#126623=CARTESIAN_POINT('Ctrl Pts',(-4.67621148812538,43.104869821818,84.7347631376418));
#126624=CARTESIAN_POINT('Ctrl Pts',(-4.77320031795728,43.1241916785181,
84.7771726331388));
#126625=CARTESIAN_POINT('Ctrl Pts',(-4.82482221472671,43.1299126869364,
84.7902825781148));
#126626=CARTESIAN_POINT('Ctrl Pts',(-4.88081081954212,43.1299146855279,
84.7902825781148));
#126627=CARTESIAN_POINT('',(-5.69482187817968,40.384659828731,83.));
#126628=CARTESIAN_POINT('Origin',(-5.69482187817972,40.3846598287309,86.));
#126629=CARTESIAN_POINT('',(5.69537693071232,40.384253239671,83.));
#126630=CARTESIAN_POINT('',(-25.9994287388058,40.3853846300409,83.));
#126631=CARTESIAN_POINT('',(4.3155751451931,41.7640550251902,83.3361150636597));
#126632=CARTESIAN_POINT('Origin',(5.69537693071237,40.3842532396709,86.));
#126633=CARTESIAN_POINT('',(4.88126057014233,43.1297404501394,84.7906780580687));
#126634=CARTESIAN_POINT('Ctrl Pts',(4.88126057014233,43.1297404501394,84.7906780580686));
#126635=CARTESIAN_POINT('Ctrl Pts',(4.82527855129633,43.1297404501394,84.7906735213082));
#126636=CARTESIAN_POINT('Ctrl Pts',(4.77366641546815,43.1240229215084,84.7775580917314));
#126637=CARTESIAN_POINT('Ctrl Pts',(4.6766881693441,43.1047100794269,84.7351374178226));
#126638=CARTESIAN_POINT('Ctrl Pts',(4.63131473335929,43.0910704365374,84.7058682945448));
#126639=CARTESIAN_POINT('Ctrl Pts',(4.50347730469683,43.040841140764,84.6041166977585));
#126640=CARTESIAN_POINT('Ctrl Pts',(4.42966809762419,42.9946063244288,84.5183478507339));
#126641=CARTESIAN_POINT('Ctrl Pts',(4.28521059479939,42.8746430433406,84.3217402796909));
#126642=CARTESIAN_POINT('Ctrl Pts',(4.21219885970608,42.7837779689826,84.1918390912012));
#126643=CARTESIAN_POINT('Ctrl Pts',(4.10993073305515,42.5723177386494,83.9409875062198));
#126644=CARTESIAN_POINT('Ctrl Pts',(4.08126491520575,42.4514774729932,83.8200033709791));
#126645=CARTESIAN_POINT('Ctrl Pts',(4.08125725528774,42.2368922872938,83.6371990515189));
#126646=CARTESIAN_POINT('Ctrl Pts',(4.09845674449903,42.1311064778841,83.5579277928478));
#126647=CARTESIAN_POINT('Ctrl Pts',(4.17899207419104,41.9328803074183,83.4280312090116));
#126648=CARTESIAN_POINT('Ctrl Pts',(4.23941854432905,41.8402116260542,83.375558776258));
#126649=CARTESIAN_POINT('Ctrl Pts',(4.31557514519306,41.7640550251902,83.3361150636597));
#126650=CARTESIAN_POINT('',(7.20026057014233,43.1297404501395,84.7908660063353));
#126651=CARTESIAN_POINT('',(6.04076057014233,43.1297404501395,84.790772032202));
#126652=CARTESIAN_POINT('',(7.20026057014233,43.1297404501395,87.2091339936647));
#126653=CARTESIAN_POINT('Ctrl Pts',(7.20026057014233,43.1297404501395,87.2091339936647));
#126654=CARTESIAN_POINT('Ctrl Pts',(7.21294682501949,43.1297404501395,87.2091329653849));
#126655=CARTESIAN_POINT('Ctrl Pts',(7.22563810372133,43.1305598955788,87.2072760701667));
#126656=CARTESIAN_POINT('Ctrl Pts',(7.25023479260245,43.1336713801016,87.2001704115751));
#126657=CARTESIAN_POINT('Ctrl Pts',(7.2621307534533,43.1359764055222,87.1948942718855));
#126658=CARTESIAN_POINT('Ctrl Pts',(7.29576491915057,43.144380828481,87.1753983698309));
#126659=CARTESIAN_POINT('Ctrl Pts',(7.31531022822448,43.152132358212,87.1571188348341));
#126660=CARTESIAN_POINT('Ctrl Pts',(7.35331775020091,43.1705301900497,87.1122694969576));
#126661=CARTESIAN_POINT('Ctrl Pts',(7.3740522567382,43.1845108420159,87.0767203752738));
#126662=CARTESIAN_POINT('Ctrl Pts',(7.4226663467744,43.2236642757062,86.9714177547316));
#126663=CARTESIAN_POINT('Ctrl Pts',(7.44542247694709,43.2548716957552,86.8754679026737));
#126664=CARTESIAN_POINT('Ctrl Pts',(7.49758960390303,43.3433662832606,86.5527314566462));
#126665=CARTESIAN_POINT('Ctrl Pts',(7.49678217092917,43.3841889379055,86.2524977920887));
#126666=CARTESIAN_POINT('Ctrl Pts',(7.49678217092917,43.3841889379055,85.7475022079113));
#126667=CARTESIAN_POINT('Ctrl Pts',(7.49758960390304,43.3433662832606,85.4472685433538));
#126668=CARTESIAN_POINT('Ctrl Pts',(7.4454224769471,43.2548716957552,85.1245320973263));
#126669=CARTESIAN_POINT('Ctrl Pts',(7.4226663467744,43.2236642757062,85.0285822452685));
#126670=CARTESIAN_POINT('Ctrl Pts',(7.3740522567382,43.1845108420159,84.9232796247263));
#126671=CARTESIAN_POINT('Ctrl Pts',(7.35331775020092,43.1705301900497,84.8877305030424));
#126672=CARTESIAN_POINT('Ctrl Pts',(7.31531022822448,43.152132358212,84.8428811651659));
#126673=CARTESIAN_POINT('Ctrl Pts',(7.29576491915058,43.144380828481,84.8246016301691));
#126674=CARTESIAN_POINT('Ctrl Pts',(7.2621307534533,43.1359764055222,84.8051057281145));
#126675=CARTESIAN_POINT('Ctrl Pts',(7.25023479260245,43.1336713801016,84.7998295884249));
#126676=CARTESIAN_POINT('Ctrl Pts',(7.22563810372133,43.1305598955788,84.7927239298333));
#126677=CARTESIAN_POINT('Ctrl Pts',(7.21294682501949,43.1297404501395,84.7908670346151));
#126678=CARTESIAN_POINT('Ctrl Pts',(7.20026057014233,43.1297404501395,84.7908660063353));
#126679=CARTESIAN_POINT('',(4.88126057014233,43.1297404501394,87.2093219419313));
#126680=CARTESIAN_POINT('',(6.04076057014233,43.1297404501395,87.209227967798));
#126681=CARTESIAN_POINT('',(4.3155751451931,41.7640550251902,88.6638849363403));
#126682=CARTESIAN_POINT('Ctrl Pts',(4.31557514519306,41.7640550251902,88.6638849363403));
#126683=CARTESIAN_POINT('Ctrl Pts',(4.23941854432905,41.8402116260542,88.624441223742));
#126684=CARTESIAN_POINT('Ctrl Pts',(4.17899207419104,41.9328803074183,88.5719687909884));
#126685=CARTESIAN_POINT('Ctrl Pts',(4.09845674449903,42.1311064778841,88.4420722071522));
#126686=CARTESIAN_POINT('Ctrl Pts',(4.08125725528774,42.2368922872938,88.3628009484811));
#126687=CARTESIAN_POINT('Ctrl Pts',(4.08126491520575,42.4514774729932,88.1799966290208));
#126688=CARTESIAN_POINT('Ctrl Pts',(4.10993073305515,42.5723177386494,88.0590124937802));
#126689=CARTESIAN_POINT('Ctrl Pts',(4.21219885970609,42.7837779689826,87.8081609087987));
#126690=CARTESIAN_POINT('Ctrl Pts',(4.28521059479939,42.8746430433406,87.6782597203091));
#126691=CARTESIAN_POINT('Ctrl Pts',(4.42966809762419,42.9946063244288,87.4816521492661));
#126692=CARTESIAN_POINT('Ctrl Pts',(4.50347730469683,43.040841140764,87.3958833022415));
#126693=CARTESIAN_POINT('Ctrl Pts',(4.63131473335929,43.0910704365374,87.2941317054552));
#126694=CARTESIAN_POINT('Ctrl Pts',(4.6766881693441,43.1047100794269,87.2648625821774));
#126695=CARTESIAN_POINT('Ctrl Pts',(4.77366641546814,43.1240229215084,87.2224419082686));
#126696=CARTESIAN_POINT('Ctrl Pts',(4.82527855129633,43.1297404501394,87.2093264786918));
#126697=CARTESIAN_POINT('Ctrl Pts',(4.88126057014233,43.1297404501394,87.2093219419314));
#126698=CARTESIAN_POINT('',(6.03525883703878,40.0443713333445,88.9806859172054));
#126699=CARTESIAN_POINT('Origin',(5.69537693071237,40.3842532396709,86.));
#126700=CARTESIAN_POINT('',(9.57079274297153,38.5799052392773,88.3968369781133));
#126701=CARTESIAN_POINT('Ctrl Pts',(9.57079274297153,38.5799052392773,88.3968369781133));
#126702=CARTESIAN_POINT('Ctrl Pts',(9.5707332488234,38.5799052392773,88.3968369765146));
#126703=CARTESIAN_POINT('Ctrl Pts',(9.57067375482821,38.5799052403392,88.3968369757153));
#126704=CARTESIAN_POINT('Ctrl Pts',(8.88909486927776,38.5799295702497,88.3968369757153));
#126705=CARTESIAN_POINT('Ctrl Pts',(8.1875100639932,38.724779883745,88.519320896401));
#126706=CARTESIAN_POINT('Ctrl Pts',(6.98374971135328,39.2566553618154,88.7942694455703));
#126707=CARTESIAN_POINT('Ctrl Pts',(6.46520448621751,39.6144256841658,88.9316635383852));
#126708=CARTESIAN_POINT('Ctrl Pts',(6.03525883703882,40.0443713333445,88.9806859172054));
#126709=CARTESIAN_POINT('',(11.6717927429715,38.5799052392773,88.3968934308243));
#126710=CARTESIAN_POINT('',(10.6212927429715,38.5799052392773,88.3968652044688));
#126711=CARTESIAN_POINT('',(13.0860063053446,39.1656916769042,88.7414869339534));
#126712=CARTESIAN_POINT('Ctrl Pts',(13.0860063053446,39.1656916769042,88.7414869339534));
#126713=CARTESIAN_POINT('Ctrl Pts',(12.9115776150688,38.9912629866284,88.663969269128));
#126714=CARTESIAN_POINT('Ctrl Pts',(12.6925492447761,38.8399015743528,88.5750351340623));
#126715=CARTESIAN_POINT('Ctrl Pts',(12.2039210685268,38.6336428861301,88.4395838913209));
#126716=CARTESIAN_POINT('Ctrl Pts',(11.9328135534399,38.5799052392773,88.3969004440812));
#126717=CARTESIAN_POINT('Ctrl Pts',(11.6717927429715,38.5799052392773,88.3968934308243));
#126718=CARTESIAN_POINT('',(13.9076643850834,39.987349756643,88.973667809827));
#126719=CARTESIAN_POINT('Origin',(14.3042605619825,40.383945933542,86.));
#126720=CARTESIAN_POINT('',(14.2005576038968,40.6944565378947,88.9838876432241));
#126721=CARTESIAN_POINT('Ctrl Pts',(14.2005576038968,40.6944565378295,88.9838876425972));
#126722=CARTESIAN_POINT('Ctrl Pts',(14.2005576038968,40.69444463897,88.9838888808067));
#126723=CARTESIAN_POINT('Ctrl Pts',(14.2005576036844,40.6944327401709,88.9838901189379));
#126724=CARTESIAN_POINT('Ctrl Pts',(14.2005531444961,40.5695128967916,88.996887916041));
#126725=CARTESIAN_POINT('Ctrl Pts',(14.1756575752172,40.4358460629751,89.0020722846323));
#126726=CARTESIAN_POINT('Ctrl Pts',(14.0741268986634,40.1899012740497,88.9962434199587));
#126727=CARTESIAN_POINT('Ctrl Pts',(13.9975074091711,40.0776069665203,88.9856559212044));
#126728=CARTESIAN_POINT('Ctrl Pts',(13.9087580506029,39.988444692808,88.9738136974119));
#126729=CARTESIAN_POINT('Ctrl Pts',(13.9082116449317,39.9878970164913,88.9737408027343));
#126730=CARTESIAN_POINT('Ctrl Pts',(13.9076643850834,39.987349756643,88.973667809827));
#126731=CARTESIAN_POINT('',(14.2005576038968,42.6304565378295,87.9882672716729));
#126732=CARTESIAN_POINT('Origin',(14.2005576038968,40.383949635364,86.));
#126733=CARTESIAN_POINT('',(13.7005576038968,43.1304565378295,87.206978825168));
#126734=CARTESIAN_POINT('Ctrl Pts',(13.7005576038968,43.1304565378295,87.206978825168));
#126735=CARTESIAN_POINT('Ctrl Pts',(13.7005635533611,43.1304565378295,87.2069788246847));
#126736=CARTESIAN_POINT('Ctrl Pts',(13.7005695027606,43.1304565377233,87.2069788244431));
#126737=CARTESIAN_POINT('Ctrl Pts',(13.7349434333177,43.1304553106978,87.2069788244431));
#126738=CARTESIAN_POINT('Ctrl Pts',(13.7667215268191,43.1269938687308,87.2149030662356));
#126739=CARTESIAN_POINT('Ctrl Pts',(13.8263020113281,43.1153320791706,87.240899990775));
#126740=CARTESIAN_POINT('Ctrl Pts',(13.8540993385831,43.1071092325231,87.2589741809338));
#126741=CARTESIAN_POINT('Ctrl Pts',(13.9319395673727,43.0771707831725,87.3224216534088));
#126742=CARTESIAN_POINT('Ctrl Pts',(13.9761986813102,43.0500508066361,87.3767434803275));
#126743=CARTESIAN_POINT('Ctrl Pts',(14.070024541769,42.9755247782782,87.5143570677025));
#126744=CARTESIAN_POINT('Ctrl Pts',(14.1174300227276,42.916521123884,87.6124763023577));
#126745=CARTESIAN_POINT('Ctrl Pts',(14.1829744042219,42.7817463851036,87.8068079086529));
#126746=CARTESIAN_POINT('Ctrl Pts',(14.2005576038968,42.7058286960662,87.9031056458045));
#126747=CARTESIAN_POINT('Ctrl Pts',(14.2005576038968,42.6304565378295,87.9882672716729));
#126748=CARTESIAN_POINT('',(12.8005576038968,43.1304565378295,87.2070519271956));
#126749=CARTESIAN_POINT('',(13.2505576038968,43.1304565378295,87.2070153761818));
#126750=CARTESIAN_POINT('',(12.8005576038968,43.1304565378295,84.7929480728044));
#126751=CARTESIAN_POINT('Ctrl Pts',(12.8005576038968,43.1304565378295,84.7929480728043));
#126752=CARTESIAN_POINT('Ctrl Pts',(12.8005540342567,43.1304565378295,84.7929480725144));
#126753=CARTESIAN_POINT('Ctrl Pts',(12.800550464617,43.1304565378932,84.7929480723695));
#126754=CARTESIAN_POINT('Ctrl Pts',(12.8005468949777,43.1304565380206,84.7929480723695));
#126755=CARTESIAN_POINT('Ctrl Pts',(12.7878790745653,43.1304569902162,84.7929480723695));
#126756=CARTESIAN_POINT('Ctrl Pts',(12.775206184161,43.1312745218071,84.7948023896051));
#126757=CARTESIAN_POINT('Ctrl Pts',(12.7506486750991,43.1343773655443,84.8018988837129));
#126758=CARTESIAN_POINT('Ctrl Pts',(12.738773266856,43.1366751949132,84.8071674273606));
#126759=CARTESIAN_POINT('Ctrl Pts',(12.7051965550664,43.1450524580709,84.826634614644));
#126760=CARTESIAN_POINT('Ctrl Pts',(12.6856835914487,43.1527778071505,84.8448863925531));
#126761=CARTESIAN_POINT('Ctrl Pts',(12.6477316006356,43.1711140657731,84.8896697992273));
#126762=CARTESIAN_POINT('Ctrl Pts',(12.6270220730305,43.1850482619964,84.9251686425469));
#126763=CARTESIAN_POINT('Ctrl Pts',(12.5784538537086,43.2240722091775,85.0303247407441));
#126764=CARTESIAN_POINT('Ctrl Pts',(12.5556965844494,43.2551755942419,85.126141257432));
#126765=CARTESIAN_POINT('Ctrl Pts',(12.5034979555493,43.3433419209884,85.4483186441275));
#126766=CARTESIAN_POINT('Ctrl Pts',(12.5041748497398,43.3840101920279,85.7479867774995));
#126767=CARTESIAN_POINT('Ctrl Pts',(12.5041748497398,43.3840101920279,86.2520132225005));
#126768=CARTESIAN_POINT('Ctrl Pts',(12.5034979555493,43.3433419209884,86.5516813558725));
#126769=CARTESIAN_POINT('Ctrl Pts',(12.5556965844494,43.2551755942419,86.8738587425681));
#126770=CARTESIAN_POINT('Ctrl Pts',(12.5784538537086,43.2240722091775,86.9696752592559));
#126771=CARTESIAN_POINT('Ctrl Pts',(12.6270220730305,43.1850482619964,87.0748313574531));
#126772=CARTESIAN_POINT('Ctrl Pts',(12.6477316006356,43.1711140657731,87.1103302007727));
#126773=CARTESIAN_POINT('Ctrl Pts',(12.6856835914487,43.1527778071505,87.1551136074469));
#126774=CARTESIAN_POINT('Ctrl Pts',(12.7051965550664,43.1450524580709,87.173365385356));
#126775=CARTESIAN_POINT('Ctrl Pts',(12.738773266856,43.1366751949132,87.1928325726394));
#126776=CARTESIAN_POINT('Ctrl Pts',(12.7506486750991,43.1343773655443,87.198101116287));
#126777=CARTESIAN_POINT('Ctrl Pts',(12.775206184161,43.1312745218071,87.2051976103948));
#126778=CARTESIAN_POINT('Ctrl Pts',(12.7878790745653,43.1304569902162,87.2070519276305));
#126779=CARTESIAN_POINT('Ctrl Pts',(12.800550464617,43.1304565378932,87.2070519276305));
#126780=CARTESIAN_POINT('Ctrl Pts',(12.8005540342567,43.1304565378295,87.2070519274856));
#126781=CARTESIAN_POINT('Ctrl Pts',(12.8005576038968,43.1304565378295,87.2070519271956));
#126782=CARTESIAN_POINT('',(13.7005576038968,43.1304565378295,84.793021174832));
#126783=CARTESIAN_POINT('',(13.2505576038968,43.1304565378295,84.7929846238182));
#126784=CARTESIAN_POINT('',(14.2005576038968,42.6304565378295,84.0117327283271));
#126785=CARTESIAN_POINT('Ctrl Pts',(14.2005576038968,42.6304565378295,84.0117327283271));
#126786=CARTESIAN_POINT('Ctrl Pts',(14.2005576038968,42.7058286960663,84.0968943541956));
#126787=CARTESIAN_POINT('Ctrl Pts',(14.1829744042219,42.7817463851036,84.1931920913471));
#126788=CARTESIAN_POINT('Ctrl Pts',(14.1174300227276,42.916521123884,84.3875236976423));
#126789=CARTESIAN_POINT('Ctrl Pts',(14.070024541769,42.9755247782782,84.4856429322975));
#126790=CARTESIAN_POINT('Ctrl Pts',(13.9761986813102,43.0500508066361,84.6232565196725));
#126791=CARTESIAN_POINT('Ctrl Pts',(13.9319395673727,43.0771707831725,84.6775783465912));
#126792=CARTESIAN_POINT('Ctrl Pts',(13.8540993385831,43.1071092325231,84.7410258190662));
#126793=CARTESIAN_POINT('Ctrl Pts',(13.8263020113281,43.1153320791706,84.759100009225));
#126794=CARTESIAN_POINT('Ctrl Pts',(13.7667215268191,43.1269938687308,84.7850969337644));
#126795=CARTESIAN_POINT('Ctrl Pts',(13.7349434333177,43.1304553106978,84.7930211755569));
#126796=CARTESIAN_POINT('Ctrl Pts',(13.7005695027606,43.1304565377233,84.7930211755569));
#126797=CARTESIAN_POINT('Ctrl Pts',(13.7005635533611,43.1304565378295,84.7930211753153));
#126798=CARTESIAN_POINT('Ctrl Pts',(13.7005576038968,43.1304565378295,84.793021174832));
#126799=CARTESIAN_POINT('',(14.2005576038968,40.6944565378948,83.0161123567759));
#126800=CARTESIAN_POINT('Origin',(14.2005576038968,40.383949635364,86.));
#126801=CARTESIAN_POINT('',(14.1511293052103,40.3839513998532,83.));
#126802=CARTESIAN_POINT('Ctrl Pts',(14.1511293052103,40.3839513999301,83.));
#126803=CARTESIAN_POINT('Ctrl Pts',(14.184533612433,40.4862144071147,83.0000000000052));
#126804=CARTESIAN_POINT('Ctrl Pts',(14.2005539915515,40.5932423327881,83.0055811103851));
#126805=CARTESIAN_POINT('Ctrl Pts',(14.2005576036844,40.6944327401709,83.0161098810621));
#126806=CARTESIAN_POINT('Ctrl Pts',(14.2005576038968,40.69444463897,83.0161111191933));
#126807=CARTESIAN_POINT('Ctrl Pts',(14.2005576038968,40.6944565378295,83.0161123574028));
#126808=CARTESIAN_POINT('',(16.0005576038968,40.3838853818492,82.9999999980886));
#126809=CARTESIAN_POINT('',(-25.9994287388058,40.3853846300409,83.));
#126810=CARTESIAN_POINT('Origin',(16.0005576038968,40.3838853818492,86.));
#126811=CARTESIAN_POINT('Origin',(16.0005576038968,40.3838853818492,86.));
#126812=CARTESIAN_POINT('',(13.9076643850834,39.987349756643,83.026332190173));
#126813=CARTESIAN_POINT('Ctrl Pts',(13.9076643850834,39.987349756643,83.0263321901729));
#126814=CARTESIAN_POINT('Ctrl Pts',(13.9082116449317,39.9878970164913,83.0262591972656));
#126815=CARTESIAN_POINT('Ctrl Pts',(13.9087580506029,39.988444692808,83.0261863025881));
#126816=CARTESIAN_POINT('Ctrl Pts',(13.9975074091711,40.0776069665203,83.0143440787956));
#126817=CARTESIAN_POINT('Ctrl Pts',(14.0741268986634,40.1899012740497,83.0037565800413));
#126818=CARTESIAN_POINT('Ctrl Pts',(14.1345364020809,40.3362353976012,83.000288477273));
#126819=CARTESIAN_POINT('Ctrl Pts',(14.1432949797111,40.3599676160584,82.9999999999988));
#126820=CARTESIAN_POINT('Ctrl Pts',(14.1511293052103,40.3839513999301,83.));
#126821=CARTESIAN_POINT('',(13.0860063053446,39.1656916769042,83.2585130660466));
#126822=CARTESIAN_POINT('Origin',(14.3042605619825,40.383945933542,86.));
#126823=CARTESIAN_POINT('',(11.6717927429715,38.5799052392773,83.6031065691756));
#126824=CARTESIAN_POINT('Ctrl Pts',(11.6717927429715,38.5799052392773,83.6031065691756));
#126825=CARTESIAN_POINT('Ctrl Pts',(11.9328135534399,38.5799052392773,83.6030995559188));
#126826=CARTESIAN_POINT('Ctrl Pts',(12.2039210685268,38.6336428861301,83.5604161086791));
#126827=CARTESIAN_POINT('Ctrl Pts',(12.6925492447761,38.8399015743528,83.4249648659377));
#126828=CARTESIAN_POINT('Ctrl Pts',(12.9115776150688,38.9912629866284,83.336030730872));
#126829=CARTESIAN_POINT('Ctrl Pts',(13.0860063053446,39.1656916769042,83.2585130660466));
#126830=CARTESIAN_POINT('',(9.57079274297153,38.5799052392773,83.6031630218867));
#126831=CARTESIAN_POINT('',(10.6212927429715,38.5799052392773,83.6031347955312));
#126832=CARTESIAN_POINT('',(6.03525883703878,40.0443713333445,83.0193140827946));
#126833=CARTESIAN_POINT('Ctrl Pts',(6.0352588370388,40.0443713333445,83.0193140827946));
#126834=CARTESIAN_POINT('Ctrl Pts',(6.4652044862175,39.6144256841658,83.0683364616148));
#126835=CARTESIAN_POINT('Ctrl Pts',(6.98374971135328,39.2566553618154,83.2057305544296));
#126836=CARTESIAN_POINT('Ctrl Pts',(8.1875100639932,38.724779883745,83.4806791035989));
#126837=CARTESIAN_POINT('Ctrl Pts',(8.88909486927776,38.5799295702497,83.6031630242847));
#126838=CARTESIAN_POINT('Ctrl Pts',(9.57061426098601,38.5799052424629,83.6031630242847));
#126839=CARTESIAN_POINT('Ctrl Pts',(9.57067375482821,38.5799052403392,83.6031630242847));
#126840=CARTESIAN_POINT('Ctrl Pts',(9.5707332488234,38.5799052392773,83.6031630234854));
#126841=CARTESIAN_POINT('Ctrl Pts',(9.57079274297153,38.5799052392773,83.6031630218867));
#126842=CARTESIAN_POINT('Origin',(5.69537693071237,40.3842532396709,86.));
#126843=CARTESIAN_POINT('',(-6.03491922226453,40.0445867642791,83.019338654981));
#126844=CARTESIAN_POINT('Origin',(-5.69482187817972,40.3846598287309,86.));
#126845=CARTESIAN_POINT('',(-9.57050540210797,38.5802468769672,83.6034202264699));
#126846=CARTESIAN_POINT('Ctrl Pts',(-9.57050540210795,38.5802468769672,
83.6034202264699));
#126847=CARTESIAN_POINT('Ctrl Pts',(-8.88897256914252,38.5802225487005,
83.6034202264699));
#126848=CARTESIAN_POINT('Ctrl Pts',(-8.18737580567768,38.7250267702563,
83.480898503507));
#126849=CARTESIAN_POINT('Ctrl Pts',(-6.98352950944328,39.2568425175939,
83.2058517696258));
#126850=CARTESIAN_POINT('Ctrl Pts',(-6.46491979272285,39.6146168916673,
83.0683987779395));
#126851=CARTESIAN_POINT('Ctrl Pts',(-6.03491922226454,40.0445867642791,
83.019338654981));
#126852=CARTESIAN_POINT('',(-11.6715054007694,38.5803218750975,83.6034202264699));
#126853=CARTESIAN_POINT('',(-25.9994931547856,38.5808333326384,83.6034202264699));
#126854=CARTESIAN_POINT('',(-13.0856980517762,39.1661587946801,83.2587206975987));
#126855=CARTESIAN_POINT('Ctrl Pts',(-13.0856980517762,39.1661587946801,
83.2587206975987));
#126856=CARTESIAN_POINT('Ctrl Pts',(-12.9106059326522,38.9910541747942,
83.3365689270392));
#126857=CARTESIAN_POINT('Ctrl Pts',(-12.6901619533851,38.8388876989633,
83.4261076675721));
#126858=CARTESIAN_POINT('Ctrl Pts',(-12.2008654839661,38.6335041042048,
83.5611995838646));
#126859=CARTESIAN_POINT('Ctrl Pts',(-11.9310804859103,38.5803311409929,
83.6034202264699));
#126860=CARTESIAN_POINT('Ctrl Pts',(-11.6715054007694,38.5803218750975,
83.6034202264699));
#126861=CARTESIAN_POINT('',(-13.9073268007584,39.9878462041285,83.0263984455991));
#126862=CARTESIAN_POINT('Origin',(-14.3044194064105,40.3849671603434,86.));
#126863=CARTESIAN_POINT('Ctrl Pts',(-13.9073268007584,39.9878462041285,
83.0263984455991));
#126864=CARTESIAN_POINT('Ctrl Pts',(-13.9960100566734,40.076535791615,83.0145549020595));
#126865=CARTESIAN_POINT('Ctrl Pts',(-14.0730534099154,40.1890412751135,
83.0038655192316));
#126866=CARTESIAN_POINT('Ctrl Pts',(-14.1339891648514,40.3361862550399,
83.0003015081353));
#126867=CARTESIAN_POINT('Ctrl Pts',(-14.1429487704599,40.3604431105938,
82.9999999999987));
#126868=CARTESIAN_POINT('Ctrl Pts',(-14.1509424007594,40.384961681931,83.));
#126869=CARTESIAN_POINT('Origin',(-12.8000971137702,43.4309134633981,26.));
#126870=CARTESIAN_POINT('',(-12.8001078226894,43.1309134635892,26.));
#126871=CARTESIAN_POINT('',(-12.8001078226894,43.1309134635892,26.));
#126872=CARTESIAN_POINT('',(-12.5000971139614,43.4309027544789,26.));
#126873=CARTESIAN_POINT('Origin',(-12.8000971137702,43.4309134633981,26.));
#126874=CARTESIAN_POINT('',(-12.5000971139614,43.4309027544789,106.));
#126875=CARTESIAN_POINT('',(-12.5000971139614,43.4309027544789,26.));
#126876=CARTESIAN_POINT('',(-12.8001078226894,43.1309134635892,106.));
#126877=CARTESIAN_POINT('Origin',(-12.8000971137702,43.4309134633981,106.));
#126878=CARTESIAN_POINT('',(-12.8001078226894,43.1309134635892,26.));
#126879=CARTESIAN_POINT('',(-12.8001078226894,43.1309134635892,26.));
#126880=CARTESIAN_POINT('',(-12.8001078226894,43.1309134635892,26.));
#126881=CARTESIAN_POINT('Origin',(-12.8001078226894,43.1309134635892,26.));
#126882=CARTESIAN_POINT('',(-13.700107822116,43.1309455903466,26.));
#126883=CARTESIAN_POINT('',(-13.700107822116,43.1309455903466,26.));
#126884=CARTESIAN_POINT('',(-12.8001078226894,43.1309134635892,26.));
#126885=CARTESIAN_POINT('Origin',(-12.8001078226894,43.1309134635892,26.));
#126886=CARTESIAN_POINT('',(-13.700107822116,43.1309455903466,106.));
#126887=CARTESIAN_POINT('',(-12.8001078226894,43.1309134635892,106.));
#126888=CARTESIAN_POINT('',(-13.700107822116,43.1309455903466,26.));
#126889=CARTESIAN_POINT('Origin',(-12.8001078226894,43.1309134635892,26.));
#126890=CARTESIAN_POINT('',(-13.700107822116,43.1309455903466,26.));
#126891=CARTESIAN_POINT('Origin',(-13.7001256703145,42.6309455906652,26.));
#126892=CARTESIAN_POINT('',(-14.200125669996,42.6309634388637,26.));
#126893=CARTESIAN_POINT('',(-14.200125669996,42.6309634388637,26.));
#126894=CARTESIAN_POINT('Origin',(-13.7001256703145,42.6309455906652,26.));
#126895=CARTESIAN_POINT('Origin',(-13.7001256703145,42.6309455906652,26.));
#126896=CARTESIAN_POINT('',(-14.200125669996,42.6309634388637,106.));
#126897=CARTESIAN_POINT('Origin',(-13.7001256703145,42.6309455906652,106.));
#126898=CARTESIAN_POINT('',(-14.200125669996,42.6309634388637,26.));
#126899=CARTESIAN_POINT('Origin',(-13.7001256703145,42.6309455906652,26.));
#126900=CARTESIAN_POINT('',(-14.200125669996,42.6309634388637,26.));
#126901=CARTESIAN_POINT('Origin',(-14.200125669996,42.6309634388637,26.));
#126902=CARTESIAN_POINT('',(-14.2001947782207,40.6949634400972,26.));
#126903=CARTESIAN_POINT('',(-14.2001947782207,40.6949634400972,26.));
#126904=CARTESIAN_POINT('',(-14.200125669996,42.6309634388637,26.));
#126905=CARTESIAN_POINT('Origin',(-14.200125669996,42.6309634388637,26.));
#126906=CARTESIAN_POINT('',(-14.2001947782207,40.6949634400972,106.));
#126907=CARTESIAN_POINT('',(-14.200125669996,42.6309634388637,106.));
#126908=CARTESIAN_POINT('',(-14.2001947782207,40.6949634400972,26.));
#126909=CARTESIAN_POINT('Origin',(-14.200125669996,42.6309634388637,26.));
#126910=CARTESIAN_POINT('',(-14.2001947782207,40.6949634400972,26.));
#126911=CARTESIAN_POINT('Origin',(-13.2001947788579,40.6949277437001,26.));
#126912=CARTESIAN_POINT('',(-13.9073268007584,39.9878462041285,26.));
#126913=CARTESIAN_POINT('',(-13.9073268007584,39.9878462041285,26.));
#126914=CARTESIAN_POINT('Origin',(-13.2001947788579,40.6949277437001,26.));
#126915=CARTESIAN_POINT('Origin',(-13.2001947788579,40.6949277437001,26.));
#126916=CARTESIAN_POINT('',(-13.9073268007584,39.9878462041285,106.));
#126917=CARTESIAN_POINT('Origin',(-13.2001947788579,40.6949277437001,106.));
#126918=CARTESIAN_POINT('',(-13.9073268007584,39.9878462041285,26.));
#126919=CARTESIAN_POINT('Origin',(-13.2001947788579,40.6949277437001,26.));
#126920=CARTESIAN_POINT('',(-13.9073268007584,39.9878462041285,26.));
#126921=CARTESIAN_POINT('Origin',(-13.9073268007584,39.9878462041285,26.));
#126922=CARTESIAN_POINT('',(-13.0856980517762,39.1661587946801,26.));
#126923=CARTESIAN_POINT('',(-13.0856980517762,39.1661587946801,26.));
#126924=CARTESIAN_POINT('',(-13.9073268007584,39.9878462041285,26.));
#126925=CARTESIAN_POINT('Origin',(-13.9073268007584,39.9878462041285,26.));
#126926=CARTESIAN_POINT('',(-13.0856980517762,39.1661587946801,106.));
#126927=CARTESIAN_POINT('',(-13.9073268007584,39.9878462041285,106.));
#126928=CARTESIAN_POINT('',(-13.0856980517762,39.1661587946801,26.));
#126929=CARTESIAN_POINT('Origin',(-13.9073268007584,39.9878462041285,26.));
#126930=CARTESIAN_POINT('',(-13.0856980517762,39.1661587946801,26.));
#126931=CARTESIAN_POINT('Origin',(-11.6714340079752,40.5803218738233,26.));
#126932=CARTESIAN_POINT('',(-11.6715054007694,38.5803218750975,26.));
#126933=CARTESIAN_POINT('',(-11.6715054007694,38.5803218750975,26.));
#126934=CARTESIAN_POINT('Origin',(-11.6714340079752,40.5803218738233,26.));
#126935=CARTESIAN_POINT('Origin',(-11.6714340079752,40.5803218738233,26.));
#126936=CARTESIAN_POINT('',(-11.6715054007694,38.5803218750975,106.));
#126937=CARTESIAN_POINT('Origin',(-11.6714340079752,40.5803218738233,106.));
#126938=CARTESIAN_POINT('',(-11.6715054007694,38.5803218750975,26.));
#126939=CARTESIAN_POINT('Origin',(-11.6714340079752,40.5803218738233,26.));
#126940=CARTESIAN_POINT('',(-11.6715054007694,38.5803218750975,26.));
#126941=CARTESIAN_POINT('Origin',(-11.6715054007694,38.5803218750975,26.));
#126942=CARTESIAN_POINT('',(-9.57050540210797,38.5802468769672,26.));
#126943=CARTESIAN_POINT('',(-9.57050540210797,38.5802468769672,26.));
#126944=CARTESIAN_POINT('',(-11.6715054007694,38.5803218750975,26.));
#126945=CARTESIAN_POINT('Origin',(-11.6715054007694,38.5803218750975,26.));
#126946=CARTESIAN_POINT('',(-9.57050540210797,38.5802468769672,106.));
#126947=CARTESIAN_POINT('',(-11.6715054007694,38.5803218750975,106.));
#126948=CARTESIAN_POINT('',(-9.57050540210797,38.5802468769672,26.));
#126949=CARTESIAN_POINT('Origin',(-11.6715054007694,38.5803218750975,26.));
#126950=CARTESIAN_POINT('',(-9.57050540210797,38.5802468769672,26.));
#126951=CARTESIAN_POINT('Origin',(-9.57032692012244,43.5802468737816,26.));
#126952=CARTESIAN_POINT('',(-6.03491922226454,40.0445867642791,26.));
#126953=CARTESIAN_POINT('',(-6.03491922226454,40.0445867642791,26.));
#126954=CARTESIAN_POINT('Origin',(-9.57032692012244,43.5802468737816,26.));
#126955=CARTESIAN_POINT('Origin',(-9.57032692012244,43.5802468737816,26.));
#126956=CARTESIAN_POINT('',(-6.03491922226454,40.0445867642791,106.));
#126957=CARTESIAN_POINT('Origin',(-9.57032692012244,43.5802468737816,106.));
#126958=CARTESIAN_POINT('',(-6.03491922226454,40.0445867642791,26.));
#126959=CARTESIAN_POINT('Origin',(-9.57032692012244,43.5802468737816,26.));
#126960=CARTESIAN_POINT('',(-6.03491922226454,40.0445867642791,26.));
#126961=CARTESIAN_POINT('Origin',(-6.03491922226454,40.0445867642791,26.));
#126962=CARTESIAN_POINT('',(-4.31517414500253,41.7642090685172,26.));
#126963=CARTESIAN_POINT('',(-4.31517414500253,41.7642090685172,26.));
#126964=CARTESIAN_POINT('',(-6.03491922226454,40.0445867642791,26.));
#126965=CARTESIAN_POINT('Origin',(-6.03491922226454,40.0445867642791,26.));
#126966=CARTESIAN_POINT('',(-4.31517414500253,41.7642090685172,106.));
#126967=CARTESIAN_POINT('',(-6.03491922226454,40.0445867642791,106.));
#126968=CARTESIAN_POINT('',(-4.31517414500253,41.7642090685172,26.));
#126969=CARTESIAN_POINT('Origin',(-6.03491922226454,40.0445867642791,26.));
#126970=CARTESIAN_POINT('',(-4.31517414500253,41.7642090685172,26.));
#126971=CARTESIAN_POINT('Origin',(-4.8808393766598,42.3299146860376,26.));
#126972=CARTESIAN_POINT('',(-4.88081081954211,43.1299146855279,26.));
#126973=CARTESIAN_POINT('',(-4.88081081954211,43.1299146855279,26.));
#126974=CARTESIAN_POINT('Origin',(-4.8808393766598,42.3299146860376,26.));
#126975=CARTESIAN_POINT('Origin',(-4.8808393766598,42.3299146860376,26.));
#126976=CARTESIAN_POINT('',(-4.88081081954212,43.1299146855279,106.));
#126977=CARTESIAN_POINT('Origin',(-4.8808393766598,42.3299146860376,106.));
#126978=CARTESIAN_POINT('',(-4.88081081954211,43.1299146855279,26.));
#126979=CARTESIAN_POINT('Origin',(-4.8808393766598,42.3299146860376,26.));
#126980=CARTESIAN_POINT('',(-4.88081081954211,43.1299146855279,26.));
#126981=CARTESIAN_POINT('Origin',(-4.88081081954211,43.1299146855279,26.));
#126982=CARTESIAN_POINT('',(-7.19981081806464,43.1299974654728,26.));
#126983=CARTESIAN_POINT('',(-7.19981081806464,43.1299974654728,26.));
#126984=CARTESIAN_POINT('',(-4.88081081954211,43.1299146855279,26.));
#126985=CARTESIAN_POINT('Origin',(-4.88081081954211,43.1299146855279,26.));
#126986=CARTESIAN_POINT('',(-7.19981081806464,43.1299974654728,106.));
#126987=CARTESIAN_POINT('',(-4.88081081954211,43.1299146855279,106.));
#126988=CARTESIAN_POINT('',(-7.19981081806464,43.1299974654728,26.));
#126989=CARTESIAN_POINT('Origin',(-4.88081081954211,43.1299146855279,26.));
#126990=CARTESIAN_POINT('',(-7.19981081806464,43.1299974654728,26.));
#126991=CARTESIAN_POINT('Origin',(12.8005576038968,43.4304565378295,26.));
#126992=CARTESIAN_POINT('',(12.8005576038968,43.1304565378295,26.));
#126993=CARTESIAN_POINT('',(12.8005576038968,43.1304565378295,26.));
#126994=CARTESIAN_POINT('',(12.8005576038968,43.1304565378295,106.));
#126995=CARTESIAN_POINT('',(12.8005576038968,43.1304565378295,26.));
#126996=CARTESIAN_POINT('',(12.5005576038968,43.4304565378295,106.));
#126997=CARTESIAN_POINT('Origin',(12.8005576038968,43.4304565378295,106.));
#126998=CARTESIAN_POINT('',(12.5005576038968,43.4304565378295,26.));
#126999=CARTESIAN_POINT('',(12.5005576038968,43.4304565378295,26.));
#127000=CARTESIAN_POINT('',(12.8005576038968,43.1304565378295,26.));
#127001=CARTESIAN_POINT('Origin',(12.8005576038968,43.4304565378295,26.));
#127002=CARTESIAN_POINT('',(12.8005576038968,43.1304565378295,26.));
#127003=CARTESIAN_POINT('Origin',(12.8005576038968,43.1304565378295,26.));
#127004=CARTESIAN_POINT('',(13.7005576038968,43.1304565378295,106.));
#127005=CARTESIAN_POINT('',(13.7005576038968,43.1304565378295,26.));
#127006=CARTESIAN_POINT('',(12.8005576038968,43.1304565378295,106.));
#127007=CARTESIAN_POINT('Origin',(12.8005576038968,43.1304565378295,26.));
#127008=CARTESIAN_POINT('',(13.7005576038968,43.1304565378295,26.));
#127009=CARTESIAN_POINT('Origin',(12.8005576038968,43.1304565378295,26.));
#127010=CARTESIAN_POINT('',(13.7005576038968,43.1304565378295,26.));
#127011=CARTESIAN_POINT('Origin',(13.7005576038968,42.6304565378295,26.));
#127012=CARTESIAN_POINT('',(14.2005576038968,42.6304565378295,106.));
#127013=CARTESIAN_POINT('',(14.2005576038968,42.6304565378295,26.));
#127014=CARTESIAN_POINT('Origin',(13.7005576038968,42.6304565378295,106.));
#127015=CARTESIAN_POINT('Origin',(13.7005576038968,42.6304565378295,26.));
#127016=CARTESIAN_POINT('',(14.2005576038968,42.6304565378295,26.));
#127017=CARTESIAN_POINT('Origin',(13.7005576038968,42.6304565378295,26.));
#127018=CARTESIAN_POINT('',(14.2005576038968,42.6304565378295,26.));
#127019=CARTESIAN_POINT('Origin',(14.2005576038968,42.6304565378295,26.));
#127020=CARTESIAN_POINT('',(14.2005576038968,40.6944565378295,106.));
#127021=CARTESIAN_POINT('',(14.2005576038968,40.6944565378295,26.));
#127022=CARTESIAN_POINT('',(14.2005576038968,42.6304565378295,106.));
#127023=CARTESIAN_POINT('Origin',(14.2005576038968,42.6304565378295,26.));
#127024=CARTESIAN_POINT('',(14.2005576038968,40.6944565378295,26.));
#127025=CARTESIAN_POINT('Origin',(14.2005576038968,42.6304565378295,26.));
#127026=CARTESIAN_POINT('',(14.2005576038968,40.6944565378295,26.));
#127027=CARTESIAN_POINT('Origin',(13.2005576038968,40.6944565378295,26.));
#127028=CARTESIAN_POINT('',(13.9076643850834,39.987349756643,106.));
#127029=CARTESIAN_POINT('',(13.9076643850834,39.987349756643,26.));
#127030=CARTESIAN_POINT('Origin',(13.2005576038968,40.6944565378295,106.));
#127031=CARTESIAN_POINT('Origin',(13.2005576038968,40.6944565378295,26.));
#127032=CARTESIAN_POINT('',(13.9076643850834,39.987349756643,26.));
#127033=CARTESIAN_POINT('Origin',(13.2005576038968,40.6944565378295,26.));
#127034=CARTESIAN_POINT('',(13.9076643850834,39.987349756643,26.));
#127035=CARTESIAN_POINT('Origin',(13.9076643850834,39.987349756643,26.));
#127036=CARTESIAN_POINT('',(13.0860063053446,39.1656916769042,106.));
#127037=CARTESIAN_POINT('',(13.0860063053446,39.1656916769042,26.));
#127038=CARTESIAN_POINT('',(13.9076643850834,39.987349756643,106.));
#127039=CARTESIAN_POINT('Origin',(13.9076643850834,39.987349756643,26.));
#127040=CARTESIAN_POINT('',(13.0860063053446,39.1656916769042,26.));
#127041=CARTESIAN_POINT('Origin',(13.9076643850834,39.987349756643,26.));
#127042=CARTESIAN_POINT('',(13.0860063053446,39.1656916769042,26.));
#127043=CARTESIAN_POINT('Origin',(11.6717927429715,40.5799052392773,26.));
#127044=CARTESIAN_POINT('',(11.6717927429715,38.5799052392773,106.));
#127045=CARTESIAN_POINT('',(11.6717927429715,38.5799052392773,26.));
#127046=CARTESIAN_POINT('Origin',(11.6717927429715,40.5799052392773,106.));
#127047=CARTESIAN_POINT('Origin',(11.6717927429715,40.5799052392773,26.));
#127048=CARTESIAN_POINT('',(11.6717927429715,38.5799052392773,26.));
#127049=CARTESIAN_POINT('Origin',(11.6717927429715,40.5799052392773,26.));
#127050=CARTESIAN_POINT('',(11.6717927429715,38.5799052392773,26.));
#127051=CARTESIAN_POINT('Origin',(11.6717927429715,38.5799052392773,26.));
#127052=CARTESIAN_POINT('',(9.57079274297153,38.5799052392773,106.));
#127053=CARTESIAN_POINT('',(9.57079274297153,38.5799052392773,26.));
#127054=CARTESIAN_POINT('',(11.6717927429715,38.5799052392773,106.));
#127055=CARTESIAN_POINT('Origin',(11.6717927429715,38.5799052392773,26.));
#127056=CARTESIAN_POINT('',(9.57079274297153,38.5799052392773,26.));
#127057=CARTESIAN_POINT('Origin',(11.6717927429715,38.5799052392773,26.));
#127058=CARTESIAN_POINT('',(9.57079274297153,38.5799052392773,26.));
#127059=CARTESIAN_POINT('Origin',(9.57079274297151,43.5799052392773,26.));
#127060=CARTESIAN_POINT('',(6.03525883703878,40.0443713333445,106.));
#127061=CARTESIAN_POINT('',(6.03525883703878,40.0443713333445,26.));
#127062=CARTESIAN_POINT('Origin',(9.57079274297151,43.5799052392773,106.));
#127063=CARTESIAN_POINT('Origin',(9.57079274297151,43.5799052392773,26.));
#127064=CARTESIAN_POINT('',(6.03525883703878,40.0443713333445,26.));
#127065=CARTESIAN_POINT('Origin',(9.57079274297151,43.5799052392773,26.));
#127066=CARTESIAN_POINT('',(6.03525883703878,40.0443713333445,26.));
#127067=CARTESIAN_POINT('Origin',(6.03525883703878,40.0443713333445,26.));
#127068=CARTESIAN_POINT('',(4.31557514519309,41.7640550251902,106.));
#127069=CARTESIAN_POINT('',(4.31557514519309,41.7640550251902,26.));
#127070=CARTESIAN_POINT('',(6.03525883703878,40.0443713333445,106.));
#127071=CARTESIAN_POINT('Origin',(6.03525883703878,40.0443713333445,26.));
#127072=CARTESIAN_POINT('',(4.31557514519309,41.7640550251902,26.));
#127073=CARTESIAN_POINT('Origin',(6.03525883703878,40.0443713333445,26.));
#127074=CARTESIAN_POINT('',(4.31557514519309,41.7640550251902,26.));
#127075=CARTESIAN_POINT('Origin',(4.88126057014233,42.3297404501394,26.));
#127076=CARTESIAN_POINT('',(4.88126057014233,43.1297404501394,106.));
#127077=CARTESIAN_POINT('',(4.88126057014233,43.1297404501394,26.));
#127078=CARTESIAN_POINT('Origin',(4.88126057014233,42.3297404501394,106.));
#127079=CARTESIAN_POINT('Origin',(4.88126057014233,42.3297404501394,26.));
#127080=CARTESIAN_POINT('',(4.88126057014233,43.1297404501394,26.));
#127081=CARTESIAN_POINT('Origin',(4.88126057014233,42.3297404501394,26.));
#127082=CARTESIAN_POINT('',(4.88126057014233,43.1297404501394,26.));
#127083=CARTESIAN_POINT('Origin',(4.88126057014233,43.1297404501394,26.));
#127084=CARTESIAN_POINT('',(7.20026057014233,43.1297404501395,106.));
#127085=CARTESIAN_POINT('',(7.20026057014233,43.1297404501395,26.));
#127086=CARTESIAN_POINT('',(4.88126057014233,43.1297404501394,106.));
#127087=CARTESIAN_POINT('Origin',(4.88126057014233,43.1297404501394,26.));
#127088=CARTESIAN_POINT('',(7.20026057014233,43.1297404501395,26.));
#127089=CARTESIAN_POINT('Origin',(4.88126057014233,43.1297404501394,26.));
#127090=CARTESIAN_POINT('',(7.20026057014233,43.1297404501395,26.));
#127091=CARTESIAN_POINT('Origin',(-26.0001963416363,18.8817346167756,46.));
#127092=CARTESIAN_POINT('',(-26.0001963416363,18.8817346167756,43.5));
#127093=CARTESIAN_POINT('Origin',(-26.0001963416363,18.8817346167756,46.));
#127094=CARTESIAN_POINT('',(-19.0004228631993,18.8814847500817,43.5));
#127095=CARTESIAN_POINT('',(-26.0001963416363,18.8817346167756,43.5));
#127096=CARTESIAN_POINT('Origin',(-19.0004228631993,18.8814847500817,46.));
#127097=CARTESIAN_POINT('Origin',(-26.0001963416363,18.8817346167756,66.));
#127098=CARTESIAN_POINT('',(-26.0001963416363,18.8817346167756,63.5));
#127099=CARTESIAN_POINT('Origin',(-26.0001963416363,18.8817346167756,66.));
#127100=CARTESIAN_POINT('',(-19.0004228631993,18.8814847500817,63.5));
#127101=CARTESIAN_POINT('',(-26.0001963416363,18.8817346167756,63.5));
#127102=CARTESIAN_POINT('Origin',(-19.0004228631993,18.8814847500817,66.));
#127103=CARTESIAN_POINT('Origin',(-26.0001963416363,18.8817346167756,86.));
#127104=CARTESIAN_POINT('',(-26.0001963416363,18.8817346167756,83.5));
#127105=CARTESIAN_POINT('Origin',(-26.0001963416363,18.8817346167756,86.));
#127106=CARTESIAN_POINT('',(-19.0004228631993,18.8814847500817,83.5));
#127107=CARTESIAN_POINT('',(-26.0001963416363,18.8817346167756,83.5));
#127108=CARTESIAN_POINT('Origin',(-19.0004228631993,18.8814847500817,86.));
#127109=CARTESIAN_POINT('Origin',(0.,30.5305,26.));
#127110=CARTESIAN_POINT('',(-11.9999999923546,30.5309283567652,26.));
#127111=CARTESIAN_POINT('',(0.,30.5305,26.));
#127112=CARTESIAN_POINT('',(-11.9999999923546,30.5309283567652,26.));
#127113=CARTESIAN_POINT('',(0.,30.5305,106.));
#127114=CARTESIAN_POINT('',(0.,30.5305,26.));
#127115=CARTESIAN_POINT('',(-11.9999999923546,30.5309283567652,106.));
#127116=CARTESIAN_POINT('',(-11.9999999923546,30.5309283567652,106.));
#127117=CARTESIAN_POINT('',(-11.9999999923546,30.5309283567652,26.));
#127118=CARTESIAN_POINT('Origin',(-7.19973942527044,45.1299974641986,26.));
#127119=CARTESIAN_POINT('',(-7.19973942527044,45.1299974641986,26.));
#127120=CARTESIAN_POINT('',(-7.19973942527044,45.1299974641986,26.));
#127121=CARTESIAN_POINT('',(-7.19973942527044,45.1299974641986,106.));
#127122=CARTESIAN_POINT('',(-7.19973942527044,45.1299974641986,26.));
#127123=CARTESIAN_POINT('',(-7.19973942527044,45.1299974641986,106.));
#127124=CARTESIAN_POINT('Origin',(-7.19975013418957,44.8299974643897,26.));
#127125=CARTESIAN_POINT('',(-7.49975013399844,44.8300081733089,26.));
#127126=CARTESIAN_POINT('Origin',(-7.19975013418957,44.8299974643897,26.));
#127127=CARTESIAN_POINT('',(-7.49975013399844,44.8300081733089,106.));
#127128=CARTESIAN_POINT('',(-7.49975013399844,44.8300081733089,26.));
#127129=CARTESIAN_POINT('Origin',(-7.19975013418957,44.8299974643897,106.));
#127130=CARTESIAN_POINT('Origin',(-7.49980010895438,43.4300081742008,26.));
#127131=CARTESIAN_POINT('',(-7.49980010895438,43.4300081742008,26.));
#127132=CARTESIAN_POINT('',(-7.49980010895438,43.4300081742008,26.));
#127133=CARTESIAN_POINT('',(-7.49980010895438,43.4300081742008,106.));
#127134=CARTESIAN_POINT('',(-7.49980010895438,43.4300081742008,26.));
#127135=CARTESIAN_POINT('',(-7.49980010895438,43.4300081742008,106.));
#127136=CARTESIAN_POINT('Origin',(-7.19980010914551,43.4299974652817,26.));
#127137=CARTESIAN_POINT('',(-7.19981081806464,43.1299974654728,26.));
#127138=CARTESIAN_POINT('Origin',(-7.19980010914551,43.4299974652817,106.));
#127139=CARTESIAN_POINT('Origin',(-7.19980010914551,43.4299974652817,26.));
#127140=CARTESIAN_POINT('Origin',(-4.88081081954211,43.1299146855279,26.));
#127141=CARTESIAN_POINT('',(-4.88081081954211,43.1299146855279,26.));
#127142=CARTESIAN_POINT('Origin',(-4.8808393766598,42.3299146860376,26.));
#127143=CARTESIAN_POINT('',(-4.31517414500253,41.7642090685172,26.));
#127144=CARTESIAN_POINT('Origin',(-6.03491922226454,40.0445867642791,26.));
#127145=CARTESIAN_POINT('',(-6.03491922226454,40.0445867642791,26.));
#127146=CARTESIAN_POINT('Origin',(-9.57032692012244,43.5802468737816,26.));
#127147=CARTESIAN_POINT('',(-9.57050540210797,38.5802468769672,26.));
#127148=CARTESIAN_POINT('Origin',(-11.6715054007694,38.5803218750975,26.));
#127149=CARTESIAN_POINT('',(-11.6715054007694,38.5803218750975,26.));
#127150=CARTESIAN_POINT('Origin',(-11.6714340079752,40.5803218738233,26.));
#127151=CARTESIAN_POINT('',(-13.0856980517762,39.1661587946801,26.));
#127152=CARTESIAN_POINT('Origin',(-13.9073268007584,39.9878462041285,26.));
#127153=CARTESIAN_POINT('',(-13.9073268007584,39.9878462041285,26.));
#127154=CARTESIAN_POINT('Origin',(-13.2001947788579,40.6949277437001,26.));
#127155=CARTESIAN_POINT('',(-14.2001947782207,40.6949634400972,26.));
#127156=CARTESIAN_POINT('Origin',(-14.200125669996,42.6309634388637,26.));
#127157=CARTESIAN_POINT('',(-14.200125669996,42.6309634388637,26.));
#127158=CARTESIAN_POINT('Origin',(-13.7001256703145,42.6309455906652,26.));
#127159=CARTESIAN_POINT('',(-13.700107822116,43.1309455903466,26.));
#127160=CARTESIAN_POINT('Origin',(-12.8001078226894,43.1309134635892,26.));
#127161=CARTESIAN_POINT('Origin',(-12.5000471390054,44.830902753587,26.));
#127162=CARTESIAN_POINT('',(-12.5000471390054,44.830902753587,26.));
#127163=CARTESIAN_POINT('',(-12.5000471390054,44.830902753587,26.));
#127164=CARTESIAN_POINT('',(-12.5000471390054,44.830902753587,106.));
#127165=CARTESIAN_POINT('',(-12.5000471390054,44.830902753587,26.));
#127166=CARTESIAN_POINT('',(-12.5000471390054,44.830902753587,106.));
#127167=CARTESIAN_POINT('Origin',(-12.8000471388143,44.8309134625061,26.));
#127168=CARTESIAN_POINT('',(-12.8000364298952,45.130913462315,26.));
#127169=CARTESIAN_POINT('Origin',(-12.8000471388143,44.8309134625061,26.));
#127170=CARTESIAN_POINT('',(-12.8000364298952,45.130913462315,106.));
#127171=CARTESIAN_POINT('',(-12.8000364298952,45.130913462315,26.));
#127172=CARTESIAN_POINT('Origin',(-12.8000471388143,44.8309134625061,106.));
#127173=CARTESIAN_POINT('Origin',(-15.500036428175,45.1310098425871,26.));
#127174=CARTESIAN_POINT('',(-15.500036428175,45.1310098425871,26.));
#127175=CARTESIAN_POINT('',(-15.500036428175,45.1310098425871,26.));
#127176=CARTESIAN_POINT('',(-15.500036428175,45.1310098425871,106.));
#127177=CARTESIAN_POINT('',(-15.500036428175,45.1310098425871,26.));
#127178=CARTESIAN_POINT('',(-15.500036428175,45.1310098425871,106.));
#127179=CARTESIAN_POINT('Origin',(-15.5000542763735,44.6310098429057,26.));
#127180=CARTESIAN_POINT('',(-16.0000542760549,44.6310276911043,26.));
#127181=CARTESIAN_POINT('Origin',(-15.5000542763735,44.6310098429057,26.));
#127182=CARTESIAN_POINT('',(-16.0000542760549,44.6310276911043,106.));
#127183=CARTESIAN_POINT('',(-16.0000542760549,44.6310276911043,26.));
#127184=CARTESIAN_POINT('Origin',(-15.5000542763735,44.6310098429057,106.));
#127185=CARTESIAN_POINT('Origin',(-16.0003574098591,36.1390276965147,26.));
#127186=CARTESIAN_POINT('',(-16.0003574098591,36.1390276965147,26.));
#127187=CARTESIAN_POINT('',(-16.0003574098591,36.1390276965147,26.));
#127188=CARTESIAN_POINT('',(-16.0003574098591,36.1390276965147,106.));
#127189=CARTESIAN_POINT('',(-16.0003574098591,36.1390276965147,26.));
#127190=CARTESIAN_POINT('',(-16.0003574098591,36.1390276965147,106.));
#127191=CARTESIAN_POINT('Origin',(-16.5083574095355,36.1390458302844,26.));
#127192=CARTESIAN_POINT('',(-16.5083755433052,35.631045830608,26.));
#127193=CARTESIAN_POINT('Origin',(-16.5083574095355,36.1390458302844,26.));
#127194=CARTESIAN_POINT('',(-16.5083755433052,35.631045830608,106.));
#127195=CARTESIAN_POINT('',(-16.5083755433052,35.631045830608,26.));
#127196=CARTESIAN_POINT('Origin',(-16.5083574095355,36.1390458302844,106.));
#127197=CARTESIAN_POINT('Origin',(-16.8283755431013,35.6310572534551,26.));
#127198=CARTESIAN_POINT('',(-16.8283755431013,35.6310572534551,26.));
#127199=CARTESIAN_POINT('',(-16.8283755431013,35.6310572534551,26.));
#127200=CARTESIAN_POINT('',(-16.8283755431013,35.6310572534551,106.));
#127201=CARTESIAN_POINT('',(-16.8283755431013,35.6310572534551,26.));
#127202=CARTESIAN_POINT('',(-16.8283755431013,35.6310572534551,106.));
#127203=CARTESIAN_POINT('Origin',(-16.8284826322926,32.6310572553665,26.));
#127204=CARTESIAN_POINT('',(-18.9497272510074,34.7524533210679,26.));
#127205=CARTESIAN_POINT('Origin',(-16.8284826322926,32.6310572553665,26.));
#127206=CARTESIAN_POINT('',(-18.9497272510074,34.7524533210679,106.));
#127207=CARTESIAN_POINT('',(-18.9497272510074,34.7524533210679,26.));
#127208=CARTESIAN_POINT('Origin',(-16.8284826322926,32.6310572553665,106.));
#127209=CARTESIAN_POINT('Origin',(-24.5353630919994,29.167216239992,26.));
#127210=CARTESIAN_POINT('',(-24.5353630919994,29.167216239992,26.));
#127211=CARTESIAN_POINT('',(-24.5353630919994,29.167216239992,26.));
#127212=CARTESIAN_POINT('',(-24.5353630919994,29.167216239992,106.));
#127213=CARTESIAN_POINT('',(-24.5353630919994,29.167216239992,26.));
#127214=CARTESIAN_POINT('',(-24.5353630919994,29.167216239992,106.));
#127215=CARTESIAN_POINT('Origin',(-20.9999553941414,25.6315561304895,26.));
#127216=CARTESIAN_POINT('',(-25.9999553909559,25.631734612475,26.));
#127217=CARTESIAN_POINT('Origin',(-20.9999553941414,25.6315561304895,26.));
#127218=CARTESIAN_POINT('',(-25.9999553909559,25.631734612475,106.));
#127219=CARTESIAN_POINT('',(-25.9999553909559,25.631734612475,26.));
#127220=CARTESIAN_POINT('Origin',(-20.9999553941414,25.6315561304895,106.));
#127221=CARTESIAN_POINT('Origin',(-26.0004372923167,12.1317346210761,26.));
#127222=CARTESIAN_POINT('',(-26.0004372923167,12.1317346210761,26.));
#127223=CARTESIAN_POINT('',(-26.0004372923167,12.1317346210761,26.));
#127224=CARTESIAN_POINT('',(-26.0004372923167,12.1317346210761,106.));
#127225=CARTESIAN_POINT('',(-26.0004372923167,12.1317346210761,26.));
#127226=CARTESIAN_POINT('',(-26.0004372923167,12.1317346210761,106.));
#127227=CARTESIAN_POINT('Origin',(-25.0004372929538,12.131698924679,26.));
#127228=CARTESIAN_POINT('',(-25.0004729893509,11.1316989253161,26.));
#127229=CARTESIAN_POINT('Origin',(-25.0004372929538,12.131698924679,26.));
#127230=CARTESIAN_POINT('',(-25.0004729893509,11.1316989253161,106.));
#127231=CARTESIAN_POINT('',(-25.0004729893509,11.1316989253161,26.));
#127232=CARTESIAN_POINT('Origin',(-25.0004372929538,12.131698924679,106.));
#127233=CARTESIAN_POINT('Origin',(-20.500472992218,11.1315382915292,26.));
#127234=CARTESIAN_POINT('',(-20.500472992218,11.1315382915292,26.));
#127235=CARTESIAN_POINT('',(-20.500472992218,11.1315382915292,26.));
#127236=CARTESIAN_POINT('',(-20.500472992218,11.1315382915292,106.));
#127237=CARTESIAN_POINT('',(-20.500472992218,11.1315382915292,26.));
#127238=CARTESIAN_POINT('',(-20.500472992218,11.1315382915292,106.));
#127239=CARTESIAN_POINT('Origin',(-19.000645973767,12.6312582369605,26.));
#127240=CARTESIAN_POINT('',(-19.000645973767,12.6312582369605,26.));
#127241=CARTESIAN_POINT('',(-19.000645973767,12.6312582369605,26.));
#127242=CARTESIAN_POINT('',(-19.000645973767,12.6312582369605,106.));
#127243=CARTESIAN_POINT('',(-19.000645973767,12.6312582369605,26.));
#127244=CARTESIAN_POINT('',(-19.000645973767,12.6312582369605,106.));
#127245=CARTESIAN_POINT('Origin',(-19.0003186021092,21.8022582311175,26.));
#127246=CARTESIAN_POINT('',(-19.0003186021092,21.8022582311175,26.));
#127247=CARTESIAN_POINT('',(-19.0003186021092,21.8022582311175,26.));
#127248=CARTESIAN_POINT('',(-19.0003186021092,21.8022582311175,106.));
#127249=CARTESIAN_POINT('',(-19.0003186021092,21.8022582311175,26.));
#127250=CARTESIAN_POINT('',(-19.0003186021092,21.8022582311175,106.));
#127251=CARTESIAN_POINT('Origin',(-18.0003186027463,21.8022225347204,26.));
#127252=CARTESIAN_POINT('',(-18.4697586471852,22.6851868854601,26.));
#127253=CARTESIAN_POINT('Origin',(-18.0003186027463,21.8022225347204,26.));
#127254=CARTESIAN_POINT('',(-18.4697586471852,22.6851868854601,106.));
#127255=CARTESIAN_POINT('',(-18.4697586471852,22.6851868854601,26.));
#127256=CARTESIAN_POINT('Origin',(-18.0003186027463,21.8022225347204,106.));
#127257=CARTESIAN_POINT('Origin',(-15.7502284469069,24.1310622223319,26.));
#127258=CARTESIAN_POINT('',(-15.7502284469069,24.1310622223319,26.));
#127259=CARTESIAN_POINT('',(-15.7502284469069,24.1310622223319,26.));
#127260=CARTESIAN_POINT('',(-15.7502284469069,24.1310622223319,106.));
#127261=CARTESIAN_POINT('',(-15.7502284469069,24.1310622223319,26.));
#127262=CARTESIAN_POINT('',(-15.7502284469069,24.1310622223319,106.));
#127263=CARTESIAN_POINT('Origin',(-12.0002284492961,24.1309283608428,26.));
#127264=CARTESIAN_POINT('',(-12.0002284492961,24.1309283608428,26.));
#127265=CARTESIAN_POINT('',(-12.0002284492961,24.1309283608428,26.));
#127266=CARTESIAN_POINT('',(-12.0002284492961,24.1309283608428,106.));
#127267=CARTESIAN_POINT('',(-12.0002284492961,24.1309283608428,26.));
#127268=CARTESIAN_POINT('',(-12.0002284492961,24.1309283608428,106.));
#127269=CARTESIAN_POINT('Origin',(-11.9999999923546,30.5309283567652,26.));
#127270=CARTESIAN_POINT('',(-11.9999999923546,30.5309283567652,26.));
#127271=CARTESIAN_POINT('',(-11.9999999923546,30.5309283567652,106.));
#127272=CARTESIAN_POINT('Origin',(0.,30.5305,26.));
#127273=CARTESIAN_POINT('',(12.,30.5305,26.));
#127274=CARTESIAN_POINT('',(12.,30.5305,26.));
#127275=CARTESIAN_POINT('',(12.,30.5305,106.));
#127276=CARTESIAN_POINT('',(12.,30.5305,26.));
#127277=CARTESIAN_POINT('',(12.,30.5305,106.));
#127278=CARTESIAN_POINT('Origin',(7.20026057014233,44.8297404501395,26.));
#127279=CARTESIAN_POINT('',(7.50026057014233,44.8297404501395,26.));
#127280=CARTESIAN_POINT('Origin',(7.20026057014233,44.8297404501395,26.));
#127281=CARTESIAN_POINT('',(7.50026057014233,44.8297404501395,106.));
#127282=CARTESIAN_POINT('Origin',(7.20026057014233,44.8297404501395,106.));
#127283=CARTESIAN_POINT('',(7.50026057014233,44.8297404501395,26.));
#127284=CARTESIAN_POINT('Origin',(7.50026057014233,43.4297404501395,26.));
#127285=CARTESIAN_POINT('',(7.50026057014233,43.4297404501395,26.));
#127286=CARTESIAN_POINT('',(7.50026057014233,43.4297404501395,26.));
#127287=CARTESIAN_POINT('',(7.50026057014233,43.4297404501395,106.));
#127288=CARTESIAN_POINT('',(7.50026057014233,43.4297404501395,106.));
#127289=CARTESIAN_POINT('',(7.50026057014233,43.4297404501395,26.));
#127290=CARTESIAN_POINT('Origin',(7.20026057014232,43.4297404501395,26.));
#127291=CARTESIAN_POINT('',(7.20026057014233,43.1297404501395,26.));
#127292=CARTESIAN_POINT('',(7.20026057014233,43.1297404501395,26.));
#127293=CARTESIAN_POINT('Origin',(7.20026057014232,43.4297404501395,26.));
#127294=CARTESIAN_POINT('Origin',(7.20026057014232,43.4297404501395,106.));
#127295=CARTESIAN_POINT('Origin',(4.88126057014233,43.1297404501394,26.));
#127296=CARTESIAN_POINT('',(4.88126057014233,43.1297404501394,26.));
#127297=CARTESIAN_POINT('',(4.88126057014233,43.1297404501394,26.));
#127298=CARTESIAN_POINT('',(4.88126057014233,43.1297404501394,26.));
#127299=CARTESIAN_POINT('Origin',(4.88126057014233,42.3297404501394,26.));
#127300=CARTESIAN_POINT('',(4.31557514519309,41.7640550251902,26.));
#127301=CARTESIAN_POINT('',(4.31557514519309,41.7640550251902,26.));
#127302=CARTESIAN_POINT('Origin',(4.88126057014233,42.3297404501394,26.));
#127303=CARTESIAN_POINT('Origin',(6.03525883703878,40.0443713333445,26.));
#127304=CARTESIAN_POINT('',(6.03525883703878,40.0443713333445,26.));
#127305=CARTESIAN_POINT('',(6.03525883703878,40.0443713333445,26.));
#127306=CARTESIAN_POINT('',(6.03525883703878,40.0443713333445,26.));
#127307=CARTESIAN_POINT('Origin',(9.57079274297151,43.5799052392773,26.));
#127308=CARTESIAN_POINT('',(9.57079274297153,38.5799052392773,26.));
#127309=CARTESIAN_POINT('',(9.57079274297153,38.5799052392773,26.));
#127310=CARTESIAN_POINT('Origin',(9.57079274297151,43.5799052392773,26.));
#127311=CARTESIAN_POINT('Origin',(11.6717927429715,38.5799052392773,26.));
#127312=CARTESIAN_POINT('',(11.6717927429715,38.5799052392773,26.));
#127313=CARTESIAN_POINT('',(11.6717927429715,38.5799052392773,26.));
#127314=CARTESIAN_POINT('',(11.6717927429715,38.5799052392773,26.));
#127315=CARTESIAN_POINT('Origin',(11.6717927429715,40.5799052392773,26.));
#127316=CARTESIAN_POINT('',(13.0860063053446,39.1656916769042,26.));
#127317=CARTESIAN_POINT('',(13.0860063053446,39.1656916769042,26.));
#127318=CARTESIAN_POINT('Origin',(11.6717927429715,40.5799052392773,26.));
#127319=CARTESIAN_POINT('Origin',(13.9076643850834,39.987349756643,26.));
#127320=CARTESIAN_POINT('',(13.9076643850834,39.987349756643,26.));
#127321=CARTESIAN_POINT('',(13.9076643850834,39.987349756643,26.));
#127322=CARTESIAN_POINT('',(13.9076643850834,39.987349756643,26.));
#127323=CARTESIAN_POINT('Origin',(13.2005576038968,40.6944565378295,26.));
#127324=CARTESIAN_POINT('',(14.2005576038968,40.6944565378295,26.));
#127325=CARTESIAN_POINT('',(14.2005576038968,40.6944565378295,26.));
#127326=CARTESIAN_POINT('Origin',(13.2005576038968,40.6944565378295,26.));
#127327=CARTESIAN_POINT('Origin',(14.2005576038968,42.6304565378295,26.));
#127328=CARTESIAN_POINT('',(14.2005576038968,42.6304565378295,26.));
#127329=CARTESIAN_POINT('',(14.2005576038968,42.6304565378295,26.));
#127330=CARTESIAN_POINT('',(14.2005576038968,42.6304565378295,26.));
#127331=CARTESIAN_POINT('Origin',(13.7005576038968,42.6304565378295,26.));
#127332=CARTESIAN_POINT('',(13.7005576038968,43.1304565378295,26.));
#127333=CARTESIAN_POINT('',(13.7005576038968,43.1304565378295,26.));
#127334=CARTESIAN_POINT('Origin',(13.7005576038968,42.6304565378295,26.));
#127335=CARTESIAN_POINT('Origin',(12.8005576038968,43.1304565378295,26.));
#127336=CARTESIAN_POINT('',(12.8005576038968,43.1304565378295,26.));
#127337=CARTESIAN_POINT('Origin',(12.5005576038968,44.8304565378295,26.));
#127338=CARTESIAN_POINT('',(12.5005576038968,44.8304565378295,26.));
#127339=CARTESIAN_POINT('',(12.5005576038968,44.8304565378295,26.));
#127340=CARTESIAN_POINT('',(12.5005576038968,44.8304565378295,106.));
#127341=CARTESIAN_POINT('',(12.5005576038968,44.8304565378295,106.));
#127342=CARTESIAN_POINT('',(12.5005576038968,44.8304565378295,26.));
#127343=CARTESIAN_POINT('Origin',(12.8005576038968,44.8304565378295,26.));
#127344=CARTESIAN_POINT('',(12.8005576038968,45.1304565378295,26.));
#127345=CARTESIAN_POINT('Origin',(12.8005576038968,44.8304565378295,26.));
#127346=CARTESIAN_POINT('',(12.8005576038968,45.1304565378295,106.));
#127347=CARTESIAN_POINT('Origin',(12.8005576038968,44.8304565378295,106.));
#127348=CARTESIAN_POINT('',(12.8005576038968,45.1304565378295,26.));
#127349=CARTESIAN_POINT('Origin',(15.5005576038968,45.1304565378295,26.));
#127350=CARTESIAN_POINT('',(15.5005576038968,45.1304565378295,26.));
#127351=CARTESIAN_POINT('',(15.5005576038968,45.1304565378295,26.));
#127352=CARTESIAN_POINT('',(15.5005576038968,45.1304565378295,106.));
#127353=CARTESIAN_POINT('',(15.5005576038968,45.1304565378295,106.));
#127354=CARTESIAN_POINT('',(15.5005576038968,45.1304565378295,26.));
#127355=CARTESIAN_POINT('Origin',(15.5005576038968,44.6304565378295,26.));
#127356=CARTESIAN_POINT('',(16.0005576038968,44.6304565378295,26.));
#127357=CARTESIAN_POINT('Origin',(15.5005576038968,44.6304565378295,26.));
#127358=CARTESIAN_POINT('',(16.0005576038968,44.6304565378295,106.));
#127359=CARTESIAN_POINT('Origin',(15.5005576038968,44.6304565378295,106.));
#127360=CARTESIAN_POINT('',(16.0005576038968,44.6304565378295,26.));
#127361=CARTESIAN_POINT('Origin',(16.0005576038968,36.1384565378295,26.));
#127362=CARTESIAN_POINT('',(16.0005576038968,36.1384565378295,26.));
#127363=CARTESIAN_POINT('',(16.0005576038968,36.1384565378295,26.));
#127364=CARTESIAN_POINT('',(16.0005576038968,36.1384565378295,106.));
#127365=CARTESIAN_POINT('',(16.0005576038968,36.1384565378295,106.));
#127366=CARTESIAN_POINT('',(16.0005576038968,36.1384565378295,26.));
#127367=CARTESIAN_POINT('Origin',(16.5085576038968,36.1384565378295,26.));
#127368=CARTESIAN_POINT('',(16.5085576038968,35.6304565378295,26.));
#127369=CARTESIAN_POINT('Origin',(16.5085576038968,36.1384565378295,26.));
#127370=CARTESIAN_POINT('',(16.5085576038968,35.6304565378295,106.));
#127371=CARTESIAN_POINT('Origin',(16.5085576038968,36.1384565378295,106.));
#127372=CARTESIAN_POINT('',(16.5085576038968,35.6304565378295,26.));
#127373=CARTESIAN_POINT('Origin',(16.8285576038968,35.6304565378295,26.));
#127374=CARTESIAN_POINT('',(16.8285576038968,35.6304565378295,26.));
#127375=CARTESIAN_POINT('',(16.8285576038968,35.6304565378295,26.));
#127376=CARTESIAN_POINT('',(16.8285576038968,35.6304565378295,106.));
#127377=CARTESIAN_POINT('',(16.8285576038968,35.6304565378295,106.));
#127378=CARTESIAN_POINT('',(16.8285576038968,35.6304565378295,26.));
#127379=CARTESIAN_POINT('Origin',(16.8285576038968,32.6304565378295,26.));
#127380=CARTESIAN_POINT('',(18.9498779474565,34.7517768813891,26.));
#127381=CARTESIAN_POINT('Origin',(16.8285576038968,32.6304565378295,26.));
#127382=CARTESIAN_POINT('',(18.9498779474565,34.7517768813891,106.));
#127383=CARTESIAN_POINT('Origin',(16.8285576038968,32.6304565378295,106.));
#127384=CARTESIAN_POINT('',(18.9498779474565,34.7517768813891,26.));
#127385=CARTESIAN_POINT('Origin',(24.535314412049,29.1663404167966,26.));
#127386=CARTESIAN_POINT('',(24.535314412049,29.1663404167966,26.));
#127387=CARTESIAN_POINT('',(24.535314412049,29.1663404167966,26.));
#127388=CARTESIAN_POINT('',(24.535314412049,29.1663404167966,106.));
#127389=CARTESIAN_POINT('',(24.535314412049,29.1663404167966,106.));
#127390=CARTESIAN_POINT('',(24.535314412049,29.1663404167966,26.));
#127391=CARTESIAN_POINT('Origin',(20.9997805061163,25.6308065108639,26.));
#127392=CARTESIAN_POINT('',(25.9997805061163,25.6308065108639,26.));
#127393=CARTESIAN_POINT('Origin',(20.9997805061163,25.6308065108639,26.));
#127394=CARTESIAN_POINT('',(25.9997805061163,25.6308065108639,106.));
#127395=CARTESIAN_POINT('Origin',(20.9997805061163,25.6308065108639,106.));
#127396=CARTESIAN_POINT('',(25.9997805061163,25.6308065108639,26.));
#127397=CARTESIAN_POINT('Origin',(25.9997805061163,12.1308065108639,26.));
#127398=CARTESIAN_POINT('',(25.9997805061163,12.1308065108639,26.));
#127399=CARTESIAN_POINT('',(25.9997805061163,12.1308065108639,26.));
#127400=CARTESIAN_POINT('',(25.9997805061163,12.1308065108639,106.));
#127401=CARTESIAN_POINT('',(25.9997805061163,12.1308065108639,106.));
#127402=CARTESIAN_POINT('',(25.9997805061163,12.1308065108639,26.));
#127403=CARTESIAN_POINT('Origin',(24.9997805061163,12.1308065108639,26.));
#127404=CARTESIAN_POINT('',(24.9997805061163,11.1308065108639,26.));
#127405=CARTESIAN_POINT('Origin',(24.9997805061163,12.1308065108639,26.));
#127406=CARTESIAN_POINT('',(24.9997805061163,11.1308065108639,106.));
#127407=CARTESIAN_POINT('Origin',(24.9997805061163,12.1308065108639,106.));
#127408=CARTESIAN_POINT('',(24.9997805061163,11.1308065108639,26.));
#127409=CARTESIAN_POINT('Origin',(20.4997805061163,11.1308065108639,26.));
#127410=CARTESIAN_POINT('',(20.4997805061163,11.1308065108639,26.));
#127411=CARTESIAN_POINT('',(20.4997805061163,11.1308065108639,26.));
#127412=CARTESIAN_POINT('',(20.4997805061163,11.1308065108639,106.));
#127413=CARTESIAN_POINT('',(20.4997805061163,11.1308065108639,106.));
#127414=CARTESIAN_POINT('',(20.4997805061163,11.1308065108639,26.));
#127415=CARTESIAN_POINT('Origin',(19.0000070232196,12.6305799937605,26.));
#127416=CARTESIAN_POINT('',(19.0000070232196,12.6305799937605,26.));
#127417=CARTESIAN_POINT('',(19.0000070232196,12.6305799937605,26.));
#127418=CARTESIAN_POINT('',(19.0000070232196,12.6305799937605,106.));
#127419=CARTESIAN_POINT('',(19.0000070232196,12.6305799937605,106.));
#127420=CARTESIAN_POINT('',(19.0000070232196,12.6305799937605,26.));
#127421=CARTESIAN_POINT('Origin',(19.0000070232196,21.8015799937605,26.));
#127422=CARTESIAN_POINT('',(19.0000070232196,21.8015799937605,26.));
#127423=CARTESIAN_POINT('',(19.0000070232196,21.8015799937605,26.));
#127424=CARTESIAN_POINT('',(19.0000070232196,21.8015799937605,106.));
#127425=CARTESIAN_POINT('',(19.0000070232196,21.8015799937605,106.));
#127426=CARTESIAN_POINT('',(19.0000070232196,21.8015799937605,26.));
#127427=CARTESIAN_POINT('Origin',(18.0000070232196,21.8015799937605,26.));
#127428=CARTESIAN_POINT('',(18.4694785860055,22.6845275866195,26.));
#127429=CARTESIAN_POINT('Origin',(18.0000070232196,21.8015799937605,26.));
#127430=CARTESIAN_POINT('',(18.4694785860055,22.6845275866195,106.));
#127431=CARTESIAN_POINT('Origin',(18.0000070232196,21.8015799937605,106.));
#127432=CARTESIAN_POINT('',(18.4694785860055,22.6845275866195,26.));
#127433=CARTESIAN_POINT('Origin',(15.75,24.1305,26.));
#127434=CARTESIAN_POINT('',(15.75,24.1305,26.));
#127435=CARTESIAN_POINT('',(15.75,24.1305,26.));
#127436=CARTESIAN_POINT('',(15.75,24.1305,106.));
#127437=CARTESIAN_POINT('',(15.75,24.1305,106.));
#127438=CARTESIAN_POINT('',(15.75,24.1305,26.));
#127439=CARTESIAN_POINT('Origin',(12.,24.1305,26.));
#127440=CARTESIAN_POINT('',(12.,24.1305,26.));
#127441=CARTESIAN_POINT('',(12.,24.1305,26.));
#127442=CARTESIAN_POINT('',(12.,24.1305,106.));
#127443=CARTESIAN_POINT('',(12.,24.1305,106.));
#127444=CARTESIAN_POINT('',(12.,24.1305,26.));
#127445=CARTESIAN_POINT('Origin',(12.,30.5305,26.));
#127446=CARTESIAN_POINT('',(12.,30.5305,26.));
#127447=CARTESIAN_POINT('',(12.,30.5305,106.));
#127448=CARTESIAN_POINT('Origin',(12.9998902530581,28.1306315243467,106.));
#127449=CARTESIAN_POINT('Origin',(12.9998902530581,28.1306315243467,26.));
#127450=CARTESIAN_POINT('',(0.,0.,0.));
#127451=CARTESIAN_POINT('',(0.,0.,132.));
#127452=CARTESIAN_POINT('',(0.,0.,0.));
#127453=CARTESIAN_POINT('Origin',(0.,17.2745,396.));
#127454=CARTESIAN_POINT('',(-6.81246236636335,15.2682931400241,396.));
#127455=CARTESIAN_POINT('',(-6.80496662630522,14.858,396.));
#127456=CARTESIAN_POINT('',(-6.87343118006261,18.6055334688258,396.));
#127457=CARTESIAN_POINT('',(-6.89783581472438,14.858,396.));
#127458=CARTESIAN_POINT('',(-2.477,14.858,396.));
#127459=CARTESIAN_POINT('Origin',(-10.752,15.874,396.));
#127460=CARTESIAN_POINT('Origin',(0.,17.2745,396.));
#127461=CARTESIAN_POINT('',(6.9,14.858,396.));
#127462=CARTESIAN_POINT('',(6.9000000000081,16.898174578473,396.));
#127463=CARTESIAN_POINT('',(6.9,16.06625,396.));
#127464=CARTESIAN_POINT('',(6.89783581472438,14.858,396.));
#127465=CARTESIAN_POINT('Origin',(10.752,15.874,396.));
#127466=CARTESIAN_POINT('',(-2.477,14.858,396.));
#127467=CARTESIAN_POINT('Origin',(0.,17.2745,396.));
#127468=CARTESIAN_POINT('',(-6.83721545938402,16.6231992843132,396.));
#127469=CARTESIAN_POINT('Origin',(-10.752,15.874,396.));
#127470=CARTESIAN_POINT('',(-6.87343118006261,18.6055334688258,396.));
#127471=CARTESIAN_POINT('Origin',(-8.847,15.049,400.));
#127472=CARTESIAN_POINT('',(-8.847,19.4868506020415,400.));
#127473=CARTESIAN_POINT('',(-8.847,19.4868506020415,422.));
#127474=CARTESIAN_POINT('',(-8.847,19.4868506020415,416.));
#127475=CARTESIAN_POINT('',(-8.847,22.145,422.));
#127476=CARTESIAN_POINT('',(-8.847,17.27175,422.));
#127477=CARTESIAN_POINT('',(-8.847,22.145,400.));
#127478=CARTESIAN_POINT('',(-8.847,22.145,400.));
#127479=CARTESIAN_POINT('',(-8.847,17.27175,400.));
#127480=CARTESIAN_POINT('Origin',(0.,19.4945,400.));
#127481=CARTESIAN_POINT('',(6.9000000000081,16.898174578473,400.));
#127482=CARTESIAN_POINT('',(8.751846859637,19.321640494912,400.));
#127483=CARTESIAN_POINT('Origin',(10.752,15.874,400.));
#127484=CARTESIAN_POINT('',(6.9,20.058,400.));
#127485=CARTESIAN_POINT('',(6.9,17.17625,400.));
#127486=CARTESIAN_POINT('',(-6.89996662630522,20.058,400.));
#127487=CARTESIAN_POINT('',(3.55,20.058,400.));
#127488=CARTESIAN_POINT('',(-6.83721545938402,16.6231992843132,400.));
#127489=CARTESIAN_POINT('',(-6.89370326010986,19.7151631135172,400.));
#127490=CARTESIAN_POINT('',(-8.751846859637,19.321640494912,400.));
#127491=CARTESIAN_POINT('Origin',(-10.752,15.874,400.));
#127492=CARTESIAN_POINT('Origin',(-8.656,19.4868506020415,400.));
#127493=CARTESIAN_POINT('',(-7.291,22.145,400.));
#127494=CARTESIAN_POINT('',(-4.528,22.145,400.));
#127495=CARTESIAN_POINT('',(-6.7,22.736,400.));
#127496=CARTESIAN_POINT('Origin',(-7.291,22.736,400.));
#127497=CARTESIAN_POINT('',(-6.7,23.731,400.));
#127498=CARTESIAN_POINT('',(-6.7,21.11525,400.));
#127499=CARTESIAN_POINT('',(6.7,23.731,400.));
#127500=CARTESIAN_POINT('',(-3.4545,23.731,400.));
#127501=CARTESIAN_POINT('',(6.7,22.736,400.));
#127502=CARTESIAN_POINT('',(6.7,21.71725,400.));
#127503=CARTESIAN_POINT('',(7.291,22.145,400.));
#127504=CARTESIAN_POINT('Origin',(7.291,22.736,400.));
#127505=CARTESIAN_POINT('',(8.847,22.145,400.));
#127506=CARTESIAN_POINT('',(3.6455,22.145,400.));
#127507=CARTESIAN_POINT('',(8.847,19.4868506020415,400.));
#127508=CARTESIAN_POINT('',(8.847,20.92425,400.));
#127509=CARTESIAN_POINT('Origin',(8.656,19.4868506020415,400.));
#127510=CARTESIAN_POINT('Origin',(8.656,19.4868506020415,422.));
#127511=CARTESIAN_POINT('',(8.751846859637,19.321640494912,422.));
#127512=CARTESIAN_POINT('',(8.847,19.4868506020415,422.));
#127513=CARTESIAN_POINT('Origin',(8.656,19.4868506020415,422.));
#127514=CARTESIAN_POINT('',(8.751846859637,19.321640494912,416.));
#127515=CARTESIAN_POINT('',(8.847,19.4868506020415,416.));
#127516=CARTESIAN_POINT('Origin',(8.847,22.354,400.));
#127517=CARTESIAN_POINT('',(8.847,22.145,422.));
#127518=CARTESIAN_POINT('',(8.847,22.145,400.));
#127519=CARTESIAN_POINT('',(8.847,20.92425,422.));
#127520=CARTESIAN_POINT('Origin',(0.,19.4945,422.));
#127521=CARTESIAN_POINT('',(7.291,22.145,422.));
#127522=CARTESIAN_POINT('',(3.6455,22.145,422.));
#127523=CARTESIAN_POINT('',(6.7,22.736,422.));
#127524=CARTESIAN_POINT('Origin',(7.291,22.736,422.));
#127525=CARTESIAN_POINT('',(6.7,23.731,422.));
#127526=CARTESIAN_POINT('',(6.7,21.71725,422.));
#127527=CARTESIAN_POINT('',(-6.7,23.731,422.));
#127528=CARTESIAN_POINT('',(-3.4545,23.731,422.));
#127529=CARTESIAN_POINT('',(-6.7,22.736,422.));
#127530=CARTESIAN_POINT('',(-6.7,21.11525,422.));
#127531=CARTESIAN_POINT('',(-7.291,22.145,422.));
#127532=CARTESIAN_POINT('Origin',(-7.291,22.736,422.));
#127533=CARTESIAN_POINT('',(-4.528,22.145,422.));
#127534=CARTESIAN_POINT('',(-8.751846859637,19.321640494912,422.));
#127535=CARTESIAN_POINT('Origin',(-8.656,19.4868506020415,422.));
#127536=CARTESIAN_POINT('',(-6.89783581472438,14.858,422.));
#127537=CARTESIAN_POINT('Origin',(-10.752,15.874,422.));
#127538=CARTESIAN_POINT('',(-4.954,14.858,422.));
#127539=CARTESIAN_POINT('',(-6.898,14.858,422.));
#127540=CARTESIAN_POINT('',(-4.763,15.049,422.));
#127541=CARTESIAN_POINT('Origin',(-4.954,15.049,422.));
#127542=CARTESIAN_POINT('',(-4.763,19.748,422.));
#127543=CARTESIAN_POINT('',(-4.763,19.748,422.));
#127544=CARTESIAN_POINT('',(-4.572,19.939,422.));
#127545=CARTESIAN_POINT('Origin',(-4.572,19.748,422.));
#127546=CARTESIAN_POINT('',(4.572,19.939,422.));
#127547=CARTESIAN_POINT('',(-4.572,19.939,422.));
#127548=CARTESIAN_POINT('',(4.763,19.748,422.));
#127549=CARTESIAN_POINT('Origin',(4.572,19.748,422.));
#127550=CARTESIAN_POINT('',(4.763,15.049,422.));
#127551=CARTESIAN_POINT('',(4.763,19.748,422.));
#127552=CARTESIAN_POINT('',(4.954,14.858,422.));
#127553=CARTESIAN_POINT('Origin',(4.954,15.049,422.));
#127554=CARTESIAN_POINT('',(6.89783581472438,14.858,422.));
#127555=CARTESIAN_POINT('',(4.954,14.858,422.));
#127556=CARTESIAN_POINT('Origin',(10.752,15.874,422.));
#127557=CARTESIAN_POINT('Origin',(-8.656,19.4868506020415,422.));
#127558=CARTESIAN_POINT('',(-8.751846859637,19.321640494912,422.));
#127559=CARTESIAN_POINT('Origin',(7.291,22.145,400.));
#127560=CARTESIAN_POINT('',(7.291,22.145,400.));
#127561=CARTESIAN_POINT('Origin',(-6.909,23.731,400.));
#127562=CARTESIAN_POINT('',(6.7,23.731,400.));
#127563=CARTESIAN_POINT('',(-6.7,23.731,400.));
#127564=CARTESIAN_POINT('',(6.109,23.731,400.8));
#127565=CARTESIAN_POINT('',(-6.109,23.731,400.8));
#127566=CARTESIAN_POINT('',(-0.399999999999999,23.731,400.8));
#127567=CARTESIAN_POINT('',(6.109,23.731,421.2));
#127568=CARTESIAN_POINT('',(6.109,23.731,410.6));
#127569=CARTESIAN_POINT('',(-6.109,23.731,421.2));
#127570=CARTESIAN_POINT('',(-6.509,23.731,421.2));
#127571=CARTESIAN_POINT('',(-6.109,23.731,400.4));
#127572=CARTESIAN_POINT('Origin',(6.7,23.94,400.));
#127573=CARTESIAN_POINT('',(6.7,22.736,400.));
#127574=CARTESIAN_POINT('Origin',(-6.7,22.736,400.));
#127575=CARTESIAN_POINT('',(-6.7,22.736,400.));
#127576=CARTESIAN_POINT('Origin',(-9.056,22.145,400.));
#127577=CARTESIAN_POINT('',(-7.291,22.145,400.));
#127578=CARTESIAN_POINT('Origin',(10.752,15.874,422.));
#127579=CARTESIAN_POINT('',(6.89783581472438,14.858,422.));
#127580=CARTESIAN_POINT('',(6.9,16.89817457841,422.));
#127581=CARTESIAN_POINT('Origin',(-10.752,15.874,422.));
#127582=CARTESIAN_POINT('',(-6.83721545938402,16.6231992843132,422.));
#127583=CARTESIAN_POINT('',(-6.89783581472438,14.858,422.));
#127584=CARTESIAN_POINT('Origin',(6.109,24.131,400.8));
#127585=CARTESIAN_POINT('',(-6.109,23.931,400.8));
#127586=CARTESIAN_POINT('',(-6.109,24.131,400.8));
#127587=CARTESIAN_POINT('',(6.109,23.931,400.8));
#127588=CARTESIAN_POINT('',(-6.109,23.931,400.8));
#127589=CARTESIAN_POINT('',(6.109,24.131,400.8));
#127590=CARTESIAN_POINT('Origin',(6.109,24.131,421.2));
#127591=CARTESIAN_POINT('',(6.109,23.931,421.2));
#127592=CARTESIAN_POINT('',(6.109,23.931,400.8));
#127593=CARTESIAN_POINT('',(6.109,24.131,421.2));
#127594=CARTESIAN_POINT('Origin',(-6.109,24.131,421.2));
#127595=CARTESIAN_POINT('',(-6.109,23.931,421.2));
#127596=CARTESIAN_POINT('',(6.109,23.931,421.2));
#127597=CARTESIAN_POINT('',(-6.109,24.131,421.2));
#127598=CARTESIAN_POINT('Origin',(-6.109,24.131,400.8));
#127599=CARTESIAN_POINT('',(-6.109,23.931,421.2));
#127600=CARTESIAN_POINT('Origin',(1.11022302462516E-15,23.931,411.));
#127601=CARTESIAN_POINT('Origin',(0.,19.4945,400.));
#127602=CARTESIAN_POINT('',(4.954,14.858,400.));
#127603=CARTESIAN_POINT('',(4.954,19.939,400.));
#127604=CARTESIAN_POINT('',(4.954,18.67625,400.));
#127605=CARTESIAN_POINT('',(4.763,15.049,400.));
#127606=CARTESIAN_POINT('Origin',(4.954,15.049,400.));
#127607=CARTESIAN_POINT('',(4.763,19.748,400.));
#127608=CARTESIAN_POINT('',(4.763,19.748,400.));
#127609=CARTESIAN_POINT('',(4.572,19.939,400.));
#127610=CARTESIAN_POINT('Origin',(4.572,19.748,400.));
#127611=CARTESIAN_POINT('',(-2.477,19.939,400.));
#127612=CARTESIAN_POINT('Origin',(0.,19.4945,400.));
#127613=CARTESIAN_POINT('',(-4.954,19.939,400.));
#127614=CARTESIAN_POINT('',(-4.954,14.858,400.));
#127615=CARTESIAN_POINT('',(-4.954,17.17625,400.));
#127616=CARTESIAN_POINT('',(-4.572,19.939,400.));
#127617=CARTESIAN_POINT('',(-2.477,19.939,400.));
#127618=CARTESIAN_POINT('',(-4.763,19.748,400.));
#127619=CARTESIAN_POINT('Origin',(-4.572,19.748,400.));
#127620=CARTESIAN_POINT('',(-4.763,15.049,400.));
#127621=CARTESIAN_POINT('',(-4.763,19.748,400.));
#127622=CARTESIAN_POINT('Origin',(-4.954,15.049,400.));
#127623=CARTESIAN_POINT('Origin',(4.572,19.748,400.));
#127624=CARTESIAN_POINT('',(4.763,19.748,400.));
#127625=CARTESIAN_POINT('',(4.572,19.939,400.));
#127626=CARTESIAN_POINT('Origin',(4.763,15.049,400.));
#127627=CARTESIAN_POINT('',(4.763,15.049,400.));
#127628=CARTESIAN_POINT('Origin',(4.954,15.049,400.));
#127629=CARTESIAN_POINT('',(4.954,14.858,400.));
#127630=CARTESIAN_POINT('Origin',(7.291,22.736,400.));
#127631=CARTESIAN_POINT('Origin',(-7.291,22.736,400.));
#127632=CARTESIAN_POINT('Origin',(-4.954,15.049,400.));
#127633=CARTESIAN_POINT('',(-4.763,15.049,400.));
#127634=CARTESIAN_POINT('',(-4.954,14.858,400.));
#127635=CARTESIAN_POINT('Origin',(-4.763,19.748,400.));
#127636=CARTESIAN_POINT('',(-4.763,19.748,400.));
#127637=CARTESIAN_POINT('Origin',(-4.572,19.748,400.));
#127638=CARTESIAN_POINT('',(-4.572,19.939,400.));
#127639=CARTESIAN_POINT('Origin',(0.,17.2745,4.));
#127640=CARTESIAN_POINT('',(-6.81246236636335,15.2682931400241,4.));
#127641=CARTESIAN_POINT('',(-6.80496662630522,14.858,4.));
#127642=CARTESIAN_POINT('',(-6.87343118006261,18.6055334688258,4.));
#127643=CARTESIAN_POINT('',(-6.89783581472438,14.858,4.));
#127644=CARTESIAN_POINT('Origin',(-10.752,15.874,4.));
#127645=CARTESIAN_POINT('',(-2.477,14.858,4.));
#127646=CARTESIAN_POINT('Origin',(0.,17.2745,4.));
#127647=CARTESIAN_POINT('',(6.9,14.858,4.));
#127648=CARTESIAN_POINT('',(6.9000000000081,16.898174578473,4.));
#127649=CARTESIAN_POINT('',(6.9,16.06625,4.));
#127650=CARTESIAN_POINT('',(6.89783581472438,14.858,4.));
#127651=CARTESIAN_POINT('',(-2.477,14.858,4.));
#127652=CARTESIAN_POINT('Origin',(10.752,15.874,4.));
#127653=CARTESIAN_POINT('Origin',(0.,17.2745,4.));
#127654=CARTESIAN_POINT('',(-6.83721545938402,16.6231992843132,4.));
#127655=CARTESIAN_POINT('Origin',(-10.752,15.874,4.));
#127656=CARTESIAN_POINT('',(-6.87343118006261,18.6055334688258,4.));
#127657=CARTESIAN_POINT('Origin',(6.9,14.858,0.));
#127658=CARTESIAN_POINT('',(6.9000000000081,16.898174578473,0.));
#127659=CARTESIAN_POINT('',(6.9,16.89817457841,-22.));
#127660=CARTESIAN_POINT('',(6.9,20.058,0.));
#127661=CARTESIAN_POINT('',(6.9,17.17625,0.));
#127662=CARTESIAN_POINT('',(6.9,20.058,0.));
#127663=CARTESIAN_POINT('',(6.9,14.858,0.));
#127664=CARTESIAN_POINT('Origin',(-8.847,15.049,0.));
#127665=CARTESIAN_POINT('',(-8.847,19.4868506020415,0.));
#127666=CARTESIAN_POINT('',(-8.847,19.4868506020415,-22.));
#127667=CARTESIAN_POINT('',(-8.847,19.4868506020415,-16.));
#127668=CARTESIAN_POINT('',(-8.847,22.145,0.));
#127669=CARTESIAN_POINT('',(-8.847,17.27175,0.));
#127670=CARTESIAN_POINT('',(-8.847,22.145,-22.));
#127671=CARTESIAN_POINT('',(-8.847,22.145,0.));
#127672=CARTESIAN_POINT('',(-8.847,17.27175,-22.));
#127673=CARTESIAN_POINT('Origin',(0.,19.4945,0.));
#127674=CARTESIAN_POINT('',(8.751846859637,19.321640494912,0.));
#127675=CARTESIAN_POINT('Origin',(10.752,15.874,0.));
#127676=CARTESIAN_POINT('',(8.847,19.4868506020415,0.));
#127677=CARTESIAN_POINT('Origin',(8.656,19.4868506020415,0.));
#127678=CARTESIAN_POINT('',(8.847,22.145,0.));
#127679=CARTESIAN_POINT('',(8.847,20.92425,0.));
#127680=CARTESIAN_POINT('',(7.291,22.145,0.));
#127681=CARTESIAN_POINT('',(3.6455,22.145,0.));
#127682=CARTESIAN_POINT('',(6.7,22.736,0.));
#127683=CARTESIAN_POINT('Origin',(7.291,22.736,0.));
#127684=CARTESIAN_POINT('',(6.7,23.731,0.));
#127685=CARTESIAN_POINT('',(6.7,21.71725,0.));
#127686=CARTESIAN_POINT('',(-6.7,23.731,0.));
#127687=CARTESIAN_POINT('',(-3.4545,23.731,0.));
#127688=CARTESIAN_POINT('',(-6.7,22.736,0.));
#127689=CARTESIAN_POINT('',(-6.7,21.11525,0.));
#127690=CARTESIAN_POINT('',(-7.291,22.145,0.));
#127691=CARTESIAN_POINT('Origin',(-7.291,22.736,0.));
#127692=CARTESIAN_POINT('',(-4.528,22.145,0.));
#127693=CARTESIAN_POINT('',(-8.751846859637,19.321640494912,0.));
#127694=CARTESIAN_POINT('Origin',(-8.656,19.4868506020415,0.));
#127695=CARTESIAN_POINT('',(-6.83721545938402,16.6231992843132,0.));
#127696=CARTESIAN_POINT('Origin',(-10.752,15.874,0.));
#127697=CARTESIAN_POINT('',(-6.89996662630522,20.058,0.));
#127698=CARTESIAN_POINT('',(-6.89370326010986,19.7151631135172,0.));
#127699=CARTESIAN_POINT('',(3.55,20.058,0.));
#127700=CARTESIAN_POINT('Origin',(-6.90003336812669,20.0616532365438,0.));
#127701=CARTESIAN_POINT('',(-6.83721545938402,16.6231992843132,-22.));
#127702=CARTESIAN_POINT('',(-6.80496662630522,14.858,0.));
#127703=CARTESIAN_POINT('',(-6.89996662630522,20.058,0.));
#127704=CARTESIAN_POINT('Origin',(8.656,19.4868506020415,-22.));
#127705=CARTESIAN_POINT('',(8.751846859637,19.321640494912,-22.));
#127706=CARTESIAN_POINT('',(8.847,19.4868506020415,-22.));
#127707=CARTESIAN_POINT('Origin',(8.656,19.4868506020415,-22.));
#127708=CARTESIAN_POINT('',(8.847,19.4868506020415,-16.));
#127709=CARTESIAN_POINT('',(8.751846859637,19.321640494912,-16.));
#127710=CARTESIAN_POINT('Origin',(8.847,22.354,0.));
#127711=CARTESIAN_POINT('',(8.847,22.145,-22.));
#127712=CARTESIAN_POINT('',(8.847,20.92425,-22.));
#127713=CARTESIAN_POINT('',(8.847,22.145,0.));
#127714=CARTESIAN_POINT('Origin',(0.,19.4945,-22.));
#127715=CARTESIAN_POINT('',(6.89783581472438,14.858,-22.));
#127716=CARTESIAN_POINT('Origin',(10.752,15.874,-22.));
#127717=CARTESIAN_POINT('',(4.954,14.858,-22.));
#127718=CARTESIAN_POINT('',(4.954,14.858,-22.));
#127719=CARTESIAN_POINT('',(4.763,15.049,-22.));
#127720=CARTESIAN_POINT('Origin',(4.954,15.049,-22.));
#127721=CARTESIAN_POINT('',(4.763,19.748,-22.));
#127722=CARTESIAN_POINT('',(4.763,19.748,-22.));
#127723=CARTESIAN_POINT('',(4.572,19.939,-22.));
#127724=CARTESIAN_POINT('Origin',(4.572,19.748,-22.));
#127725=CARTESIAN_POINT('',(-4.572,19.939,-22.));
#127726=CARTESIAN_POINT('',(-4.572,19.939,-22.));
#127727=CARTESIAN_POINT('',(-4.763,19.748,-22.));
#127728=CARTESIAN_POINT('Origin',(-4.572,19.748,-22.));
#127729=CARTESIAN_POINT('',(-4.763,15.049,-22.));
#127730=CARTESIAN_POINT('',(-4.763,19.748,-22.));
#127731=CARTESIAN_POINT('',(-4.954,14.858,-22.));
#127732=CARTESIAN_POINT('Origin',(-4.954,15.049,-22.));
#127733=CARTESIAN_POINT('',(-6.89783581472438,14.858,-22.));
#127734=CARTESIAN_POINT('',(-6.898,14.858,-22.));
#127735=CARTESIAN_POINT('',(-8.751846859637,19.321640494912,-22.));
#127736=CARTESIAN_POINT('Origin',(-10.752,15.874,-22.));
#127737=CARTESIAN_POINT('Origin',(-8.656,19.4868506020415,-22.));
#127738=CARTESIAN_POINT('',(-7.291,22.145,-22.));
#127739=CARTESIAN_POINT('',(-4.528,22.145,-22.));
#127740=CARTESIAN_POINT('',(-6.7,22.736,-22.));
#127741=CARTESIAN_POINT('Origin',(-7.291,22.736,-22.));
#127742=CARTESIAN_POINT('',(-6.7,23.731,-22.));
#127743=CARTESIAN_POINT('',(-6.7,21.11525,-22.));
#127744=CARTESIAN_POINT('',(6.7,23.731,-22.));
#127745=CARTESIAN_POINT('',(-3.4545,23.731,-22.));
#127746=CARTESIAN_POINT('',(6.7,22.736,-22.));
#127747=CARTESIAN_POINT('',(6.7,21.71725,-22.));
#127748=CARTESIAN_POINT('',(7.291,22.145,-22.));
#127749=CARTESIAN_POINT('Origin',(7.291,22.736,-22.));
#127750=CARTESIAN_POINT('',(3.6455,22.145,-22.));
#127751=CARTESIAN_POINT('Origin',(-4.954,14.858,0.));
#127752=CARTESIAN_POINT('',(4.954,14.858,0.));
#127753=CARTESIAN_POINT('',(4.954,14.858,0.));
#127754=CARTESIAN_POINT('',(4.954,14.858,0.));
#127755=CARTESIAN_POINT('',(6.89783581472438,14.858,-22.));
#127756=CARTESIAN_POINT('Origin',(-8.656,19.4868506020415,-22.));
#127757=CARTESIAN_POINT('',(-8.751846859637,19.321640494912,-22.));
#127758=CARTESIAN_POINT('Origin',(7.291,22.145,0.));
#127759=CARTESIAN_POINT('',(7.291,22.145,0.));
#127760=CARTESIAN_POINT('Origin',(-6.909,23.731,0.));
#127761=CARTESIAN_POINT('',(-6.7,23.731,0.));
#127762=CARTESIAN_POINT('',(6.7,23.731,0.));
#127763=CARTESIAN_POINT('',(6.109,23.731,-0.8));
#127764=CARTESIAN_POINT('',(-6.109,23.731,-0.800000000000001));
#127765=CARTESIAN_POINT('',(-0.399999999999999,23.731,-0.8));
#127766=CARTESIAN_POINT('',(-6.109,23.731,-21.2));
#127767=CARTESIAN_POINT('',(-6.109,23.731,-0.4));
#127768=CARTESIAN_POINT('',(6.109,23.731,-21.2));
#127769=CARTESIAN_POINT('',(-6.509,23.731,-21.2));
#127770=CARTESIAN_POINT('',(6.109,23.731,-10.6));
#127771=CARTESIAN_POINT('Origin',(6.7,23.94,0.));
#127772=CARTESIAN_POINT('',(6.7,22.736,0.));
#127773=CARTESIAN_POINT('Origin',(-6.7,22.736,0.));
#127774=CARTESIAN_POINT('',(-6.7,22.736,0.));
#127775=CARTESIAN_POINT('Origin',(-9.056,22.145,0.));
#127776=CARTESIAN_POINT('',(-7.291,22.145,0.));
#127777=CARTESIAN_POINT('Origin',(10.752,15.874,-22.));
#127778=CARTESIAN_POINT('Origin',(-10.752,15.874,-22.));
#127779=CARTESIAN_POINT('',(-6.89783581472438,14.858,-22.));
#127780=CARTESIAN_POINT('Origin',(6.109,24.131,-0.8));
#127781=CARTESIAN_POINT('',(6.109,23.931,-0.800000000000001));
#127782=CARTESIAN_POINT('',(6.109,24.131,-0.8));
#127783=CARTESIAN_POINT('',(-6.109,23.931,-0.800000000000001));
#127784=CARTESIAN_POINT('',(-6.109,23.931,-0.8));
#127785=CARTESIAN_POINT('',(-6.109,24.131,-0.800000000000001));
#127786=CARTESIAN_POINT('Origin',(6.109,24.131,-21.2));
#127787=CARTESIAN_POINT('',(6.109,23.931,-21.2));
#127788=CARTESIAN_POINT('',(6.109,24.131,-21.2));
#127789=CARTESIAN_POINT('',(6.109,23.931,-0.8));
#127790=CARTESIAN_POINT('Origin',(-6.109,24.131,-21.2));
#127791=CARTESIAN_POINT('',(-6.109,23.931,-21.2));
#127792=CARTESIAN_POINT('',(-6.109,24.131,-21.2));
#127793=CARTESIAN_POINT('',(6.109,23.931,-21.2));
#127794=CARTESIAN_POINT('Origin',(-6.109,24.131,-0.800000000000001));
#127795=CARTESIAN_POINT('',(-6.109,23.931,-21.2));
#127796=CARTESIAN_POINT('Origin',(1.11022302462516E-15,23.931,-11.));
#127797=CARTESIAN_POINT('Origin',(7.1,20.058,0.));
#127798=CARTESIAN_POINT('Origin',(4.954,17.858,0.));
#127799=CARTESIAN_POINT('',(4.954,19.939,0.));
#127800=CARTESIAN_POINT('',(4.954,18.67625,0.));
#127801=CARTESIAN_POINT('',(4.954,19.939,0.));
#127802=CARTESIAN_POINT('Origin',(-4.954,14.858,0.));
#127803=CARTESIAN_POINT('',(-4.954,19.939,0.));
#127804=CARTESIAN_POINT('',(-4.954,14.858,0.));
#127805=CARTESIAN_POINT('',(-4.954,17.17625,0.));
#127806=CARTESIAN_POINT('',(-4.954,19.939,400.));
#127807=CARTESIAN_POINT('',(-4.954,14.858,0.));
#127808=CARTESIAN_POINT('Origin',(0.,19.4945,0.));
#127809=CARTESIAN_POINT('',(4.572,19.939,0.));
#127810=CARTESIAN_POINT('',(-2.477,19.939,0.));
#127811=CARTESIAN_POINT('',(4.763,19.748,0.));
#127812=CARTESIAN_POINT('Origin',(4.572,19.748,0.));
#127813=CARTESIAN_POINT('',(4.763,15.049,0.));
#127814=CARTESIAN_POINT('',(4.763,19.748,0.));
#127815=CARTESIAN_POINT('Origin',(4.954,15.049,0.));
#127816=CARTESIAN_POINT('Origin',(0.,19.4945,0.));
#127817=CARTESIAN_POINT('',(-4.763,15.049,0.));
#127818=CARTESIAN_POINT('Origin',(-4.954,15.049,0.));
#127819=CARTESIAN_POINT('',(-4.763,19.748,0.));
#127820=CARTESIAN_POINT('',(-4.763,19.748,0.));
#127821=CARTESIAN_POINT('',(-4.572,19.939,0.));
#127822=CARTESIAN_POINT('Origin',(-4.572,19.748,0.));
#127823=CARTESIAN_POINT('',(-2.477,19.939,0.));
#127824=CARTESIAN_POINT('Origin',(-4.954,14.858,0.));
#127825=CARTESIAN_POINT('',(-4.954,14.858,0.));
#127826=CARTESIAN_POINT('Origin',(4.572,19.939,0.));
#127827=CARTESIAN_POINT('',(-4.572,19.939,0.));
#127828=CARTESIAN_POINT('',(4.572,19.939,0.));
#127829=CARTESIAN_POINT('Origin',(4.572,19.748,0.));
#127830=CARTESIAN_POINT('',(4.763,19.748,0.));
#127831=CARTESIAN_POINT('Origin',(4.763,15.049,0.));
#127832=CARTESIAN_POINT('',(4.763,15.049,0.));
#127833=CARTESIAN_POINT('Origin',(4.954,15.049,0.));
#127834=CARTESIAN_POINT('Origin',(7.291,22.736,0.));
#127835=CARTESIAN_POINT('Origin',(-7.291,22.736,0.));
#127836=CARTESIAN_POINT('Origin',(-4.954,15.049,0.));
#127837=CARTESIAN_POINT('',(-4.763,15.049,0.));
#127838=CARTESIAN_POINT('Origin',(-4.763,19.748,0.));
#127839=CARTESIAN_POINT('',(-4.763,19.748,0.));
#127840=CARTESIAN_POINT('Origin',(-4.572,19.748,0.));
#127841=CARTESIAN_POINT('',(0.,0.,0.));
#127842=CARTESIAN_POINT('Origin',(0.,0.,0.));
#127843=CARTESIAN_POINT('',(-12.5,-1.53080849893419E-15,0.));
#127844=CARTESIAN_POINT('Origin',(0.,0.,0.));
#127845=CARTESIAN_POINT('',(-12.5,-1.53080849893419E-15,400.));
#127846=CARTESIAN_POINT('',(-12.5,-1.53080849893419E-15,0.));
#127847=CARTESIAN_POINT('Origin',(0.,0.,400.));
#127848=CARTESIAN_POINT('Origin',(17.4998349855931,-17.0532626526482,0.));
#127849=CARTESIAN_POINT('',(17.4998526169879,-18.0532626524928,0.));
#127850=CARTESIAN_POINT('',(18.4998349854377,-17.0532450212534,0.));
#127851=CARTESIAN_POINT('Origin',(17.4998349855931,-17.0532626526482,0.));
#127852=CARTESIAN_POINT('',(18.4998349854377,-17.0532450212534,400.));
#127853=CARTESIAN_POINT('',(18.4998349854377,-17.0532450212534,0.));
#127854=CARTESIAN_POINT('',(17.4998526169879,-18.0532626524928,400.));
#127855=CARTESIAN_POINT('Origin',(17.4998349855931,-17.0532626526482,400.));
#127856=CARTESIAN_POINT('',(17.4998526169879,-18.0532626524928,0.));
#127857=CARTESIAN_POINT('Origin',(12.5,-18.0545,0.));
#127858=CARTESIAN_POINT('',(12.5,-18.0545,0.));
#127859=CARTESIAN_POINT('',(17.4998526169879,-18.0532626524928,0.));
#127860=CARTESIAN_POINT('',(12.5,-18.0545,400.));
#127861=CARTESIAN_POINT('',(17.4998526169879,-18.0532626524928,400.));
#127862=CARTESIAN_POINT('',(12.5,-18.0545,0.));
#127863=CARTESIAN_POINT('Origin',(12.165,-16.8045,0.));
#127864=CARTESIAN_POINT('',(12.165,-16.8045,0.));
#127865=CARTESIAN_POINT('',(12.165,-16.8045,0.));
#127866=CARTESIAN_POINT('',(12.165,-16.8045,400.));
#127867=CARTESIAN_POINT('',(12.165,-16.8045,400.));
#127868=CARTESIAN_POINT('',(12.165,-16.8045,0.));
#127869=CARTESIAN_POINT('Origin',(-12.165,-16.8045,0.));
#127870=CARTESIAN_POINT('',(-12.165,-16.8045,0.));
#127871=CARTESIAN_POINT('',(-12.165,-16.8045,0.));
#127872=CARTESIAN_POINT('',(-12.165,-16.8045,400.));
#127873=CARTESIAN_POINT('',(-12.165,-16.8045,400.));
#127874=CARTESIAN_POINT('',(-12.165,-16.8045,0.));
#127875=CARTESIAN_POINT('Origin',(-12.5,-18.0545,0.));
#127876=CARTESIAN_POINT('',(-12.5,-18.0545,0.));
#127877=CARTESIAN_POINT('',(-12.165,-16.8045,0.));
#127878=CARTESIAN_POINT('',(-12.5,-18.0545,400.));
#127879=CARTESIAN_POINT('',(-12.165,-16.8045,400.));
#127880=CARTESIAN_POINT('',(-12.5,-18.0545,0.));
#127881=CARTESIAN_POINT('Origin',(-17.4998526949542,-18.0532626524735,0.));
#127882=CARTESIAN_POINT('',(-17.4998526949542,-18.0532626524735,0.));
#127883=CARTESIAN_POINT('',(-17.4998526949542,-18.0532626524735,0.));
#127884=CARTESIAN_POINT('',(-17.4998526949542,-18.0532626524735,400.));
#127885=CARTESIAN_POINT('',(-17.4998526949542,-18.0532626524735,400.));
#127886=CARTESIAN_POINT('',(-17.4998526949542,-18.0532626524735,0.));
#127887=CARTESIAN_POINT('Origin',(-17.4998349855931,-17.0532626526482,0.));
#127888=CARTESIAN_POINT('',(-18.4998349854377,-17.0532450212534,0.));
#127889=CARTESIAN_POINT('Origin',(-17.4998349855931,-17.0532626526482,0.));
#127890=CARTESIAN_POINT('',(-18.4998349854377,-17.0532450212534,400.));
#127891=CARTESIAN_POINT('Origin',(-17.4998349855931,-17.0532626526482,400.));
#127892=CARTESIAN_POINT('',(-18.4998349854377,-17.0532450212534,0.));
#127893=CARTESIAN_POINT('Origin',(-18.4998261697403,-16.5532450213311,0.));
#127894=CARTESIAN_POINT('',(-18.4998261697403,-16.5532450213311,0.));
#127895=CARTESIAN_POINT('',(-18.4998349854377,-17.0532450212534,0.));
#127896=CARTESIAN_POINT('',(-18.4998261697403,-16.5532450213311,400.));
#127897=CARTESIAN_POINT('',(-18.4998349854377,-17.0532450212534,400.));
#127898=CARTESIAN_POINT('',(-18.4998261697403,-16.5532450213311,0.));
#127899=CARTESIAN_POINT('Origin',(-15.6381145716457,-13.6916343333914,0.));
#127900=CARTESIAN_POINT('',(-15.6381145716457,-13.6916343333914,0.));
#127901=CARTESIAN_POINT('',(-18.4998261697403,-16.5532450213311,0.));
#127902=CARTESIAN_POINT('',(-15.6381145716457,-13.6916343333914,400.));
#127903=CARTESIAN_POINT('',(-18.4998261697403,-16.5532450213311,400.));
#127904=CARTESIAN_POINT('',(-15.6381145716457,-13.6916343333914,0.));
#127905=CARTESIAN_POINT('Origin',(-15.4259862775064,-13.903770107898,0.));
#127906=CARTESIAN_POINT('',(-15.2500702858638,-13.6607607173708,0.));
#127907=CARTESIAN_POINT('Origin',(-15.4259862775064,-13.903770107898,0.));
#127908=CARTESIAN_POINT('',(-15.2500702858638,-13.6607607173708,400.));
#127909=CARTESIAN_POINT('Origin',(-15.4259862775064,-13.903770107898,400.));
#127910=CARTESIAN_POINT('',(-15.2500702858638,-13.6607607173708,0.));
#127911=CARTESIAN_POINT('Origin',(-14.8102803067574,-13.0532372410527,0.));
#127912=CARTESIAN_POINT('',(-15.2545491221624,-12.4489809326903,0.));
#127913=CARTESIAN_POINT('Origin',(-14.8102803067574,-13.0532372410527,0.));
#127914=CARTESIAN_POINT('',(-15.2545491221624,-12.4489809326903,400.));
#127915=CARTESIAN_POINT('Origin',(-14.8102803067574,-13.0532372410527,400.));
#127916=CARTESIAN_POINT('',(-15.2545493158391,-12.4489806895913,0.));
#127917=CARTESIAN_POINT('Origin',(-15.4259562865038,-12.2027701081624,0.));
#127918=CARTESIAN_POINT('',(-15.6380920610105,-12.4148984023017,0.));
#127919=CARTESIAN_POINT('Origin',(-15.4259562865038,-12.2027701081624,0.));
#127920=CARTESIAN_POINT('',(-15.6380920610105,-12.4148984023017,400.));
#127921=CARTESIAN_POINT('Origin',(-15.4259562865038,-12.2027701081624,400.));
#127922=CARTESIAN_POINT('',(-15.6380920610105,-12.4148984023017,0.));
#127923=CARTESIAN_POINT('Origin',(-18.4997027489502,-9.55318680420717,0.));
#127924=CARTESIAN_POINT('',(-18.4997027489502,-9.55318680420717,0.));
#127925=CARTESIAN_POINT('',(-18.4997027489502,-9.55318680420717,0.));
#127926=CARTESIAN_POINT('',(-18.4997027489502,-9.55318680420717,400.));
#127927=CARTESIAN_POINT('',(-18.4997027489502,-9.55318680420717,400.));
#127928=CARTESIAN_POINT('',(-18.4997027489502,-9.55318680420717,0.));
#127929=CARTESIAN_POINT('Origin',(-18.4996895254041,-8.80318680432375,0.));
#127930=CARTESIAN_POINT('',(-18.4996895254041,-8.80318680432375,0.));
#127931=CARTESIAN_POINT('',(-18.4997027489502,-9.55318680420717,0.));
#127932=CARTESIAN_POINT('',(-18.4996895254041,-8.80318680432375,400.));
#127933=CARTESIAN_POINT('',(-18.4997027489502,-9.55318680420717,400.));
#127934=CARTESIAN_POINT('',(-18.4996895254041,-8.80318680432375,0.));
#127935=CARTESIAN_POINT('Origin',(-21.4567579457066,-5.84601410770119,0.));
#127936=CARTESIAN_POINT('',(-21.4567579457066,-5.84601410770119,0.));
#127937=CARTESIAN_POINT('',(-18.4996895254041,-8.80318680432375,0.));
#127938=CARTESIAN_POINT('',(-21.4567579457066,-5.84601410770119,400.));
#127939=CARTESIAN_POINT('',(-18.4996895254041,-8.80318680432375,400.));
#127940=CARTESIAN_POINT('',(-21.4567579457066,-5.84601410770119,0.));
#127941=CARTESIAN_POINT('Origin',(-22.1638771940621,-6.55310842149901,0.));
#127942=CARTESIAN_POINT('',(-22.1638595626673,-5.55310842165444,0.));
#127943=CARTESIAN_POINT('Origin',(-22.1638771940621,-6.55310842149901,0.));
#127944=CARTESIAN_POINT('',(-22.1638595626673,-5.55310842165444,400.));
#127945=CARTESIAN_POINT('Origin',(-22.1638771940621,-6.55310842149901,400.));
#127946=CARTESIAN_POINT('',(-22.1638595626673,-5.55310842165444,0.));
#127947=CARTESIAN_POINT('Origin',(-22.499859562615,-5.55310249750579,0.));
#127948=CARTESIAN_POINT('',(-22.4998595626151,-5.55310249750579,0.));
#127949=CARTESIAN_POINT('',(-22.1638595626673,-5.55310842165444,0.));
#127950=CARTESIAN_POINT('',(-22.4998595626151,-5.55310249750579,400.));
#127951=CARTESIAN_POINT('',(-22.1638595626673,-5.55310842165444,400.));
#127952=CARTESIAN_POINT('',(-22.4998595626151,-5.55310249750579,0.));
#127953=CARTESIAN_POINT('Origin',(-22.4998507469176,-5.0531024975835,0.));
#127954=CARTESIAN_POINT('',(-22.9998507468399,-5.0530936818861,0.));
#127955=CARTESIAN_POINT('Origin',(-22.4998507469176,-5.0531024975835,0.));
#127956=CARTESIAN_POINT('',(-22.9998507468399,-5.0530936818861,400.));
#127957=CARTESIAN_POINT('Origin',(-22.4998507469176,-5.0531024975835,400.));
#127958=CARTESIAN_POINT('',(-22.9998507468399,-5.0530936818861,0.));
#127959=CARTESIAN_POINT('Origin',(-22.999779339691,-1.00309368251561,0.));
#127960=CARTESIAN_POINT('',(-22.999779339691,-1.00309368251561,0.));
#127961=CARTESIAN_POINT('',(-22.9998507468399,-5.0530936818861,0.));
#127962=CARTESIAN_POINT('',(-22.999779339691,-1.00309368251561,400.));
#127963=CARTESIAN_POINT('',(-22.9998507468399,-5.0530936818861,400.));
#127964=CARTESIAN_POINT('',(-22.999779339691,-1.00309368251561,0.));
#127965=CARTESIAN_POINT('Origin',(-22.6997793397376,-1.00309897193405,0.));
#127966=CARTESIAN_POINT('',(-22.6997740503192,-0.703098971980677,0.));
#127967=CARTESIAN_POINT('Origin',(-22.6997793397376,-1.00309897193405,0.));
#127968=CARTESIAN_POINT('',(-22.6997740503192,-0.703098971980677,400.));
#127969=CARTESIAN_POINT('Origin',(-22.6997793397376,-1.00309897193405,400.));
#127970=CARTESIAN_POINT('',(-22.6997740503192,-0.703098971980677,0.));
#127971=CARTESIAN_POINT('Origin',(-21.6997740504746,-0.703116603375476,
0.));
#127972=CARTESIAN_POINT('',(-21.6997740504746,-0.703116603375476,0.));
#127973=CARTESIAN_POINT('',(-22.6997740503192,-0.703098971980677,0.));
#127974=CARTESIAN_POINT('',(-21.6997740504746,-0.703116603375476,400.));
#127975=CARTESIAN_POINT('',(-22.6997740503192,-0.703098971980677,400.));
#127976=CARTESIAN_POINT('',(-21.6997740504746,-0.703116603375476,0.));
#127977=CARTESIAN_POINT('Origin',(-20.999603173455,-1.07541989771172,0.));
#127978=CARTESIAN_POINT('',(-20.999603173455,-1.07541989771172,0.));
#127979=CARTESIAN_POINT('',(-21.6997740504746,-0.703116603375476,0.));
#127980=CARTESIAN_POINT('',(-20.999603173455,-1.07541989771172,400.));
#127981=CARTESIAN_POINT('',(-21.6997740504746,-0.703116603375476,400.));
#127982=CARTESIAN_POINT('',(-20.999603173455,-1.07541989771172,0.));
#127983=CARTESIAN_POINT('Origin',(-20.9996316305262,-2.68941989746085,0.));
#127984=CARTESIAN_POINT('',(-20.9996316305262,-2.68941989746085,0.));
#127985=CARTESIAN_POINT('',(-20.999603173455,-1.07541989771172,0.));
#127986=CARTESIAN_POINT('',(-20.9996316305262,-2.68941989746085,400.));
#127987=CARTESIAN_POINT('',(-20.999603173455,-1.07541989771172,400.));
#127988=CARTESIAN_POINT('',(-20.9996316305262,-2.68941989746085,0.));
#127989=CARTESIAN_POINT('Origin',(-19.9996316306817,-2.68943752885565,0.));
#127990=CARTESIAN_POINT('',(-19.292531083162,-3.39655054365413,0.));
#127991=CARTESIAN_POINT('Origin',(-19.9996316306817,-2.68943752885565,0.));
#127992=CARTESIAN_POINT('',(-19.292531083162,-3.39655054365413,400.));
#127993=CARTESIAN_POINT('Origin',(-19.9996316306817,-2.68943752885565,400.));
#127994=CARTESIAN_POINT('',(-19.292531083162,-3.39655054365413,0.));
#127995=CARTESIAN_POINT('Origin',(-17.9143678173198,-2.01841157653832,0.));
#127996=CARTESIAN_POINT('',(-17.9143678173198,-2.01841157653832,0.));
#127997=CARTESIAN_POINT('',(-19.292531083162,-3.39655054365413,0.));
#127998=CARTESIAN_POINT('',(-17.9143678173198,-2.01841157653832,400.));
#127999=CARTESIAN_POINT('',(-19.292531083162,-3.39655054365413,400.));
#128000=CARTESIAN_POINT('',(-17.9143678173198,-2.01841157653832,0.));
#128001=CARTESIAN_POINT('Origin',(-21.4498705549181,1.5171534974541,0.));
#128002=CARTESIAN_POINT('',(-16.4498705551123,1.5171094189671,0.));
#128003=CARTESIAN_POINT('Origin',(-21.4498705549181,1.5171534974541,0.));
#128004=CARTESIAN_POINT('',(-16.4498705551123,1.5171094189671,400.));
#128005=CARTESIAN_POINT('Origin',(-21.4498705549181,1.5171534974541,400.));
#128006=CARTESIAN_POINT('',(-16.4498705551123,1.5171094189671,0.));
#128007=CARTESIAN_POINT('Origin',(-16.449862991244,2.37510941893376,0.));
#128008=CARTESIAN_POINT('',(-16.449862991244,2.37510941893376,0.));
#128009=CARTESIAN_POINT('',(-16.449862991244,2.37510941893376,0.));
#128010=CARTESIAN_POINT('',(-16.449862991244,2.37510941893376,400.));
#128011=CARTESIAN_POINT('',(-16.449862991244,2.37510941893376,400.));
#128012=CARTESIAN_POINT('',(-16.449862991244,2.37510941893376,0.));
#128013=CARTESIAN_POINT('Origin',(-21.4498629910497,2.37515349742076,0.));
#128014=CARTESIAN_POINT('',(-17.9142979170573,5.91065623501905,0.));
#128015=CARTESIAN_POINT('Origin',(-21.4498629910497,2.37515349742076,0.));
#128016=CARTESIAN_POINT('',(-17.9142979170573,5.91065623501905,400.));
#128017=CARTESIAN_POINT('Origin',(-21.4498629910497,2.37515349742076,400.));
#128018=CARTESIAN_POINT('',(-17.9142979170573,5.91065623501905,0.));
#128019=CARTESIAN_POINT('Origin',(-19.2924368841731,7.28881950086129,0.));
#128020=CARTESIAN_POINT('',(-19.2924368841731,7.28881950086129,0.));
#128021=CARTESIAN_POINT('',(-19.2924368841731,7.28881950086129,0.));
#128022=CARTESIAN_POINT('',(-19.2924368841731,7.28881950086129,400.));
#128023=CARTESIAN_POINT('',(-19.2924368841731,7.28881950086129,400.));
#128024=CARTESIAN_POINT('',(-19.2924368841731,7.28881950086129,0.));
#128025=CARTESIAN_POINT('Origin',(-19.9995498989716,6.58171895334164,0.));
#128026=CARTESIAN_POINT('',(-20.9995498989716,6.58171895334164,0.));
#128027=CARTESIAN_POINT('Origin',(-19.9995498989716,6.58171895334164,0.));
#128028=CARTESIAN_POINT('',(-20.9995498989716,6.58171895334164,400.));
#128029=CARTESIAN_POINT('Origin',(-19.9995498989716,6.58171895334164,400.));
#128030=CARTESIAN_POINT('',(-20.9995498989716,6.58171895334164,0.));
#128031=CARTESIAN_POINT('Origin',(-20.9995498989716,4.96771895334164,0.));
#128032=CARTESIAN_POINT('',(-20.9995498989716,4.96771895334164,0.));
#128033=CARTESIAN_POINT('',(-20.9995498989716,4.96771895334164,0.));
#128034=CARTESIAN_POINT('',(-20.9995498989716,4.96771895334164,400.));
#128035=CARTESIAN_POINT('',(-20.9995498989716,4.96771895334164,400.));
#128036=CARTESIAN_POINT('',(-20.9995498989716,4.96771895334164,0.));
#128037=CARTESIAN_POINT('Origin',(-21.6997273401087,4.59542800405243,0.));
#128038=CARTESIAN_POINT('',(-21.6997273401087,4.59542800405243,0.));
#128039=CARTESIAN_POINT('',(-21.6997273401087,4.59542800405243,0.));
#128040=CARTESIAN_POINT('',(-21.6997273401087,4.59542800405243,400.));
#128041=CARTESIAN_POINT('',(-21.6997273401087,4.59542800405243,400.));
#128042=CARTESIAN_POINT('',(-21.6997273401087,4.59542800405243,0.));
#128043=CARTESIAN_POINT('Origin',(-22.6997273401087,4.59542800405243,0.));
#128044=CARTESIAN_POINT('',(-22.6997273401087,4.59542800405243,0.));
#128045=CARTESIAN_POINT('',(-22.6997273401087,4.59542800405243,0.));
#128046=CARTESIAN_POINT('',(-22.6997273401087,4.59542800405243,400.));
#128047=CARTESIAN_POINT('',(-22.6997273401087,4.59542800405243,400.));
#128048=CARTESIAN_POINT('',(-22.6997273401087,4.59542800405243,0.));
#128049=CARTESIAN_POINT('Origin',(-22.6997273401087,4.89542800405243,0.));
#128050=CARTESIAN_POINT('',(-22.9997273401087,4.89542800405243,0.));
#128051=CARTESIAN_POINT('Origin',(-22.6997273401087,4.89542800405243,0.));
#128052=CARTESIAN_POINT('',(-22.9997273401087,4.89542800405243,400.));
#128053=CARTESIAN_POINT('Origin',(-22.6997273401087,4.89542800405243,400.));
#128054=CARTESIAN_POINT('',(-22.9997273401087,4.89542800405243,0.));
#128055=CARTESIAN_POINT('Origin',(-22.9997273401087,8.94542800405243,0.));
#128056=CARTESIAN_POINT('',(-22.9997273401087,8.94542800405243,0.));
#128057=CARTESIAN_POINT('',(-22.9997273401087,8.94542800405243,0.));
#128058=CARTESIAN_POINT('',(-22.9997273401087,8.94542800405243,400.));
#128059=CARTESIAN_POINT('',(-22.9997273401087,8.94542800405243,400.));
#128060=CARTESIAN_POINT('',(-22.9997273401087,8.94542800405243,0.));
#128061=CARTESIAN_POINT('Origin',(-22.4997273401087,8.94542800405243,0.));
#128062=CARTESIAN_POINT('',(-22.4997273401087,9.44542800405243,0.));
#128063=CARTESIAN_POINT('Origin',(-22.4997273401087,8.94542800405243,0.));
#128064=CARTESIAN_POINT('',(-22.4997273401087,9.44542800405243,400.));
#128065=CARTESIAN_POINT('Origin',(-22.4997273401087,8.94542800405243,400.));
#128066=CARTESIAN_POINT('',(-22.4997273401087,9.44542800405243,0.));
#128067=CARTESIAN_POINT('Origin',(-22.1637273401087,9.44542800405243,0.));
#128068=CARTESIAN_POINT('',(-22.1637273401087,9.44542800405243,0.));
#128069=CARTESIAN_POINT('',(-22.1637273401087,9.44542800405243,0.));
#128070=CARTESIAN_POINT('',(-22.1637273401087,9.44542800405243,400.));
#128071=CARTESIAN_POINT('',(-22.1637273401087,9.44542800405243,400.));
#128072=CARTESIAN_POINT('',(-22.1637273401087,9.44542800405243,0.));
#128073=CARTESIAN_POINT('Origin',(-22.1637273401087,10.4454280040524,0.));
#128074=CARTESIAN_POINT('',(-21.4566205589221,9.73832122286588,0.));
#128075=CARTESIAN_POINT('Origin',(-22.1637273401087,10.4454280040524,0.));
#128076=CARTESIAN_POINT('',(-21.4566205589221,9.73832122286588,400.));
#128077=CARTESIAN_POINT('Origin',(-22.1637273401087,10.4454280040524,400.));
#128078=CARTESIAN_POINT('',(-21.4566205589221,9.73832122286588,0.));
#128079=CARTESIAN_POINT('Origin',(-18.4995,12.695441781788,0.));
#128080=CARTESIAN_POINT('',(-18.4995,12.695441781788,0.));
#128081=CARTESIAN_POINT('',(-18.4995,12.695441781788,0.));
#128082=CARTESIAN_POINT('',(-18.4995,12.695441781788,400.));
#128083=CARTESIAN_POINT('',(-18.4995,12.695441781788,400.));
#128084=CARTESIAN_POINT('',(-18.4995,12.695441781788,0.));
#128085=CARTESIAN_POINT('Origin',(-18.4995,13.445441781788,0.));
#128086=CARTESIAN_POINT('',(-18.4995,13.445441781788,0.));
#128087=CARTESIAN_POINT('',(-18.4995,13.445441781788,0.));
#128088=CARTESIAN_POINT('',(-18.4995,13.445441781788,400.));
#128089=CARTESIAN_POINT('',(-18.4995,13.445441781788,400.));
#128090=CARTESIAN_POINT('',(-18.4995,13.445441781788,0.));
#128091=CARTESIAN_POINT('Origin',(-15.637838856538,16.30710292525,0.));
#128092=CARTESIAN_POINT('',(-15.637838856538,16.30710292525,0.));
#128093=CARTESIAN_POINT('',(-18.4995,13.445441781788,0.));
#128094=CARTESIAN_POINT('',(-15.637838856538,16.30710292525,400.));
#128095=CARTESIAN_POINT('',(-18.4995,13.445441781788,400.));
#128096=CARTESIAN_POINT('',(-15.637838856538,16.30710292525,0.));
#128097=CARTESIAN_POINT('Origin',(-15.4257068221821,16.094970890894,0.));
#128098=CARTESIAN_POINT('',(-15.2542955236899,16.341178459318,0.));
#128099=CARTESIAN_POINT('Origin',(-15.4257068221821,16.094970890894,0.));
#128100=CARTESIAN_POINT('',(-15.2542955236899,16.341178459318,400.));
#128101=CARTESIAN_POINT('Origin',(-15.4257068221821,16.094970890894,400.));
#128102=CARTESIAN_POINT('',(-15.2542955236899,16.341178459318,0.));
#128103=CARTESIAN_POINT('Origin',(-14.8100158476095,16.9454271684259,0.));
#128104=CARTESIAN_POINT('',(-15.2497952977804,17.5529586510386,0.));
#128105=CARTESIAN_POINT('Origin',(-14.8100158476095,16.9454271684259,0.));
#128106=CARTESIAN_POINT('',(-15.2497952977804,17.5529586510386,400.));
#128107=CARTESIAN_POINT('Origin',(-14.8100158476095,16.9454271684259,400.));
#128108=CARTESIAN_POINT('',(-15.2497954798992,17.5529589026258,0.));
#128109=CARTESIAN_POINT('Origin',(-15.4257068221821,17.795970890894,0.));
#128110=CARTESIAN_POINT('',(-15.637838856538,17.583838856538,0.));
#128111=CARTESIAN_POINT('Origin',(-15.4257068221821,17.795970890894,0.));
#128112=CARTESIAN_POINT('',(-15.637838856538,17.583838856538,400.));
#128113=CARTESIAN_POINT('Origin',(-15.4257068221821,17.795970890894,400.));
#128114=CARTESIAN_POINT('',(-15.637838856538,17.583838856538,0.));
#128115=CARTESIAN_POINT('Origin',(-18.4995,20.4455,0.));
#128116=CARTESIAN_POINT('',(-18.4995,20.4455,0.));
#128117=CARTESIAN_POINT('',(-18.4995,20.4455,0.));
#128118=CARTESIAN_POINT('',(-18.4995,20.4455,400.));
#128119=CARTESIAN_POINT('',(-18.4995,20.4455,400.));
#128120=CARTESIAN_POINT('',(-18.4995,20.4455,0.));
#128121=CARTESIAN_POINT('Origin',(-18.4995,20.9455,0.));
#128122=CARTESIAN_POINT('',(-18.4995,20.9455,0.));
#128123=CARTESIAN_POINT('',(-18.4995,20.9455,0.));
#128124=CARTESIAN_POINT('',(-18.4995,20.9455,400.));
#128125=CARTESIAN_POINT('',(-18.4995,20.9455,400.));
#128126=CARTESIAN_POINT('',(-18.4995,20.9455,0.));
#128127=CARTESIAN_POINT('Origin',(-17.4995,20.9455,0.));
#128128=CARTESIAN_POINT('',(-17.4995,21.9455,0.));
#128129=CARTESIAN_POINT('Origin',(-17.4995,20.9455,0.));
#128130=CARTESIAN_POINT('',(-17.4995,21.9455,400.));
#128131=CARTESIAN_POINT('Origin',(-17.4995,20.9455,400.));
#128132=CARTESIAN_POINT('',(-17.4995,21.9455,0.));
#128133=CARTESIAN_POINT('Origin',(-7.0995,21.9455,0.));
#128134=CARTESIAN_POINT('',(-7.0995,21.9455,0.));
#128135=CARTESIAN_POINT('',(-7.0995,21.9455,0.));
#128136=CARTESIAN_POINT('',(-7.0995,21.9455,400.));
#128137=CARTESIAN_POINT('',(-7.0995,21.9455,400.));
#128138=CARTESIAN_POINT('',(-7.0995,21.9455,0.));
#128139=CARTESIAN_POINT('Origin',(-7.0995,16.8045,0.));
#128140=CARTESIAN_POINT('',(-7.0995,16.8045,0.));
#128141=CARTESIAN_POINT('',(-7.0995,16.8045,0.));
#128142=CARTESIAN_POINT('',(-7.0995,16.8045,400.));
#128143=CARTESIAN_POINT('',(-7.0995,16.8045,400.));
#128144=CARTESIAN_POINT('',(-7.0995,16.8045,0.));
#128145=CARTESIAN_POINT('Origin',(7.0995,16.8045,0.));
#128146=CARTESIAN_POINT('',(7.0995,16.8045,0.));
#128147=CARTESIAN_POINT('',(-7.0995,16.8045,0.));
#128148=CARTESIAN_POINT('',(7.0995,16.8045,400.));
#128149=CARTESIAN_POINT('',(-7.0995,16.8045,400.));
#128150=CARTESIAN_POINT('',(7.0995,16.8045,0.));
#128151=CARTESIAN_POINT('Origin',(7.0995,21.9455,0.));
#128152=CARTESIAN_POINT('',(7.0995,21.9455,0.));
#128153=CARTESIAN_POINT('',(7.0995,16.8045,0.));
#128154=CARTESIAN_POINT('',(7.0995,21.9455,400.));
#128155=CARTESIAN_POINT('',(7.0995,16.8045,400.));
#128156=CARTESIAN_POINT('',(7.0995,21.9455,0.));
#128157=CARTESIAN_POINT('Origin',(17.4995,21.9455,0.));
#128158=CARTESIAN_POINT('',(17.4995,21.9455,0.));
#128159=CARTESIAN_POINT('',(7.0995,21.9455,0.));
#128160=CARTESIAN_POINT('',(17.4995,21.9455,400.));
#128161=CARTESIAN_POINT('',(7.0995,21.9455,400.));
#128162=CARTESIAN_POINT('',(17.4995,21.9455,0.));
#128163=CARTESIAN_POINT('Origin',(17.4995,20.9455,0.));
#128164=CARTESIAN_POINT('',(18.4995,20.9455,0.));
#128165=CARTESIAN_POINT('Origin',(17.4995,20.9455,0.));
#128166=CARTESIAN_POINT('',(18.4995,20.9455,400.));
#128167=CARTESIAN_POINT('Origin',(17.4995,20.9455,400.));
#128168=CARTESIAN_POINT('',(18.4995,20.9455,0.));
#128169=CARTESIAN_POINT('Origin',(18.4995,20.4455,0.));
#128170=CARTESIAN_POINT('',(18.4995,20.4455,0.));
#128171=CARTESIAN_POINT('',(18.4995,20.9455,0.));
#128172=CARTESIAN_POINT('',(18.4995,20.4455,400.));
#128173=CARTESIAN_POINT('',(18.4995,20.9455,400.));
#128174=CARTESIAN_POINT('',(18.4995,20.4455,0.));
#128175=CARTESIAN_POINT('Origin',(15.637838856538,17.583838856538,0.));
#128176=CARTESIAN_POINT('',(15.637838856538,17.583838856538,0.));
#128177=CARTESIAN_POINT('',(18.4995,20.4455,0.));
#128178=CARTESIAN_POINT('',(15.637838856538,17.583838856538,400.));
#128179=CARTESIAN_POINT('',(18.4995,20.4455,400.));
#128180=CARTESIAN_POINT('',(15.637838856538,17.583838856538,0.));
#128181=CARTESIAN_POINT('Origin',(15.4257068221821,17.795970890894,0.));
#128182=CARTESIAN_POINT('',(15.2497951151613,17.5529583987603,0.));
#128183=CARTESIAN_POINT('Origin',(15.4257068221821,17.795970890894,0.));
#128184=CARTESIAN_POINT('',(15.2497951151613,17.5529583987603,400.));
#128185=CARTESIAN_POINT('Origin',(15.4257068221821,17.795970890894,400.));
#128186=CARTESIAN_POINT('',(15.2497951151613,17.5529583987603,0.));
#128187=CARTESIAN_POINT('Origin',(14.8100158476095,16.9454271684259,0.));
#128188=CARTESIAN_POINT('',(15.254295316827,16.3411786932362,0.));
#128189=CARTESIAN_POINT('Origin',(14.8100158476095,16.9454271684259,0.));
#128190=CARTESIAN_POINT('',(15.254295316827,16.3411786932362,400.));
#128191=CARTESIAN_POINT('Origin',(14.8100158476095,16.9454271684259,400.));
#128192=CARTESIAN_POINT('',(15.254295510508,16.3411784501406,0.));
#128193=CARTESIAN_POINT('Origin',(15.4257068221821,16.094970890894,0.));
#128194=CARTESIAN_POINT('',(15.637838856538,16.30710292525,0.));
#128195=CARTESIAN_POINT('Origin',(15.4257068221821,16.094970890894,0.));
#128196=CARTESIAN_POINT('',(15.637838856538,16.30710292525,400.));
#128197=CARTESIAN_POINT('Origin',(15.4257068221821,16.094970890894,400.));
#128198=CARTESIAN_POINT('',(15.637838856538,16.30710292525,0.));
#128199=CARTESIAN_POINT('Origin',(18.4995,13.445441781788,0.));
#128200=CARTESIAN_POINT('',(18.4995,13.445441781788,0.));
#128201=CARTESIAN_POINT('',(18.4995,13.445441781788,0.));
#128202=CARTESIAN_POINT('',(18.4995,13.445441781788,400.));
#128203=CARTESIAN_POINT('',(18.4995,13.445441781788,400.));
#128204=CARTESIAN_POINT('',(18.4995,13.445441781788,0.));
#128205=CARTESIAN_POINT('Origin',(18.4995,12.695441781788,0.));
#128206=CARTESIAN_POINT('',(18.4995,12.695441781788,0.));
#128207=CARTESIAN_POINT('',(18.4995,13.445441781788,0.));
#128208=CARTESIAN_POINT('',(18.4995,12.695441781788,400.));
#128209=CARTESIAN_POINT('',(18.4995,13.445441781788,400.));
#128210=CARTESIAN_POINT('',(18.4995,12.695441781788,0.));
#128211=CARTESIAN_POINT('Origin',(21.4566205589221,9.73832122286588,0.));
#128212=CARTESIAN_POINT('',(21.4566205589221,9.73832122286588,0.));
#128213=CARTESIAN_POINT('',(18.4995,12.695441781788,0.));
#128214=CARTESIAN_POINT('',(21.4566205589221,9.73832122286588,400.));
#128215=CARTESIAN_POINT('',(18.4995,12.695441781788,400.));
#128216=CARTESIAN_POINT('',(21.4566205589221,9.73832122286588,0.));
#128217=CARTESIAN_POINT('Origin',(22.1637273401087,10.4454280040524,0.));
#128218=CARTESIAN_POINT('',(22.1637273401087,9.44542800405243,0.));
#128219=CARTESIAN_POINT('Origin',(22.1637273401087,10.4454280040524,0.));
#128220=CARTESIAN_POINT('',(22.1637273401087,9.44542800405243,400.));
#128221=CARTESIAN_POINT('Origin',(22.1637273401087,10.4454280040524,400.));
#128222=CARTESIAN_POINT('',(22.1637273401087,9.44542800405243,0.));
#128223=CARTESIAN_POINT('Origin',(22.4997273401087,9.44542800405243,0.));
#128224=CARTESIAN_POINT('',(22.4997273401087,9.44542800405243,0.));
#128225=CARTESIAN_POINT('',(22.1637273401087,9.44542800405243,0.));
#128226=CARTESIAN_POINT('',(22.4997273401087,9.44542800405243,400.));
#128227=CARTESIAN_POINT('',(22.1637273401087,9.44542800405243,400.));
#128228=CARTESIAN_POINT('',(22.4997273401087,9.44542800405243,0.));
#128229=CARTESIAN_POINT('Origin',(22.4997273401087,8.94542800405243,0.));
#128230=CARTESIAN_POINT('',(22.9997273401087,8.94542800405243,0.));
#128231=CARTESIAN_POINT('Origin',(22.4997273401087,8.94542800405243,0.));
#128232=CARTESIAN_POINT('',(22.9997273401087,8.94542800405243,400.));
#128233=CARTESIAN_POINT('Origin',(22.4997273401087,8.94542800405243,400.));
#128234=CARTESIAN_POINT('',(22.9997273401087,8.94542800405243,0.));
#128235=CARTESIAN_POINT('Origin',(22.9997273401087,4.89542800405242,0.));
#128236=CARTESIAN_POINT('',(22.9997273401087,4.89542800405242,0.));
#128237=CARTESIAN_POINT('',(22.9997273401087,8.94542800405243,0.));
#128238=CARTESIAN_POINT('',(22.9997273401087,4.89542800405242,400.));
#128239=CARTESIAN_POINT('',(22.9997273401087,8.94542800405243,400.));
#128240=CARTESIAN_POINT('',(22.9997273401087,4.89542800405242,0.));
#128241=CARTESIAN_POINT('Origin',(22.6997273401087,4.89542800405242,0.));
#128242=CARTESIAN_POINT('',(22.6997273401087,4.59542800405243,0.));
#128243=CARTESIAN_POINT('Origin',(22.6997273401087,4.89542800405242,0.));
#128244=CARTESIAN_POINT('',(22.6997273401087,4.59542800405243,400.));
#128245=CARTESIAN_POINT('Origin',(22.6997273401087,4.89542800405242,400.));
#128246=CARTESIAN_POINT('',(22.6997273401087,4.59542800405243,0.));
#128247=CARTESIAN_POINT('Origin',(21.6997273401087,4.59542800405243,0.));
#128248=CARTESIAN_POINT('',(21.6997273401087,4.59542800405243,0.));
#128249=CARTESIAN_POINT('',(22.6997273401087,4.59542800405243,0.));
#128250=CARTESIAN_POINT('',(21.6997273401087,4.59542800405243,400.));
#128251=CARTESIAN_POINT('',(22.6997273401087,4.59542800405243,400.));
#128252=CARTESIAN_POINT('',(21.6997273401087,4.59542800405243,0.));
#128253=CARTESIAN_POINT('Origin',(20.9995498989716,4.96771895334164,0.));
#128254=CARTESIAN_POINT('',(20.9995498989716,4.96771895334164,0.));
#128255=CARTESIAN_POINT('',(21.6997273401087,4.59542800405243,0.));
#128256=CARTESIAN_POINT('',(20.9995498989716,4.96771895334164,400.));
#128257=CARTESIAN_POINT('',(21.6997273401087,4.59542800405243,400.));
#128258=CARTESIAN_POINT('',(20.9995498989716,4.96771895334164,0.));
#128259=CARTESIAN_POINT('Origin',(20.9995498989716,6.58171895334164,0.));
#128260=CARTESIAN_POINT('',(20.9995498989716,6.58171895334164,0.));
#128261=CARTESIAN_POINT('',(20.9995498989716,4.96771895334164,0.));
#128262=CARTESIAN_POINT('',(20.9995498989716,6.58171895334164,400.));
#128263=CARTESIAN_POINT('',(20.9995498989716,4.96771895334164,400.));
#128264=CARTESIAN_POINT('',(20.9995498989716,6.58171895334164,0.));
#128265=CARTESIAN_POINT('Origin',(19.9995498989716,6.58171895334164,0.));
#128266=CARTESIAN_POINT('',(19.2924368841731,7.28881950086129,0.));
#128267=CARTESIAN_POINT('Origin',(19.9995498989716,6.58171895334164,0.));
#128268=CARTESIAN_POINT('',(19.2924368841731,7.28881950086129,400.));
#128269=CARTESIAN_POINT('Origin',(19.9995498989716,6.58171895334164,400.));
#128270=CARTESIAN_POINT('',(19.2924368841731,7.28881950086129,0.));
#128271=CARTESIAN_POINT('Origin',(17.9142979170573,5.91065623501905,0.));
#128272=CARTESIAN_POINT('',(17.9142979170573,5.91065623501905,0.));
#128273=CARTESIAN_POINT('',(19.2924368841731,7.28881950086129,0.));
#128274=CARTESIAN_POINT('',(17.9142979170573,5.91065623501905,400.));
#128275=CARTESIAN_POINT('',(19.2924368841731,7.28881950086129,400.));
#128276=CARTESIAN_POINT('',(17.9142979170573,5.91065623501905,0.));
#128277=CARTESIAN_POINT('Origin',(21.4498629910497,2.37515349742076,0.));
#128278=CARTESIAN_POINT('',(16.449862991244,2.37510941893376,0.));
#128279=CARTESIAN_POINT('Origin',(21.4498629910497,2.37515349742076,0.));
#128280=CARTESIAN_POINT('',(16.449862991244,2.37510941893376,400.));
#128281=CARTESIAN_POINT('Origin',(21.4498629910497,2.37515349742076,400.));
#128282=CARTESIAN_POINT('',(16.449862991244,2.37510941893376,0.));
#128283=CARTESIAN_POINT('Origin',(16.4498705551123,1.5171094189671,0.));
#128284=CARTESIAN_POINT('',(16.4498705551123,1.5171094189671,0.));
#128285=CARTESIAN_POINT('',(16.449862991244,2.37510941893376,0.));
#128286=CARTESIAN_POINT('',(16.4498705551124,1.5171094189671,400.));
#128287=CARTESIAN_POINT('',(16.449862991244,2.37510941893376,400.));
#128288=CARTESIAN_POINT('',(16.4498705551123,1.5171094189671,0.));
#128289=CARTESIAN_POINT('Origin',(21.4498705549181,1.5171534974541,0.));
#128290=CARTESIAN_POINT('',(17.9143678173198,-2.01841157653832,0.));
#128291=CARTESIAN_POINT('Origin',(21.4498705549181,1.5171534974541,0.));
#128292=CARTESIAN_POINT('',(17.9143678173198,-2.01841157653832,400.));
#128293=CARTESIAN_POINT('Origin',(21.4498705549181,1.5171534974541,400.));
#128294=CARTESIAN_POINT('',(17.9143678173198,-2.01841157653832,0.));
#128295=CARTESIAN_POINT('Origin',(19.292531083162,-3.39655054365413,0.));
#128296=CARTESIAN_POINT('',(19.292531083162,-3.39655054365413,0.));
#128297=CARTESIAN_POINT('',(19.292531083162,-3.39655054365413,0.));
#128298=CARTESIAN_POINT('',(19.292531083162,-3.39655054365413,400.));
#128299=CARTESIAN_POINT('',(19.292531083162,-3.39655054365413,400.));
#128300=CARTESIAN_POINT('',(19.292531083162,-3.39655054365413,0.));
#128301=CARTESIAN_POINT('Origin',(19.9996316306817,-2.68943752885565,0.));
#128302=CARTESIAN_POINT('',(20.9996316305262,-2.68941989746085,0.));
#128303=CARTESIAN_POINT('Origin',(19.9996316306817,-2.68943752885565,0.));
#128304=CARTESIAN_POINT('',(20.9996316305262,-2.68941989746085,400.));
#128305=CARTESIAN_POINT('Origin',(19.9996316306817,-2.68943752885565,400.));
#128306=CARTESIAN_POINT('',(20.9996316305262,-2.68941989746085,0.));
#128307=CARTESIAN_POINT('Origin',(20.999603173455,-1.07541989771172,0.));
#128308=CARTESIAN_POINT('',(20.999603173455,-1.07541989771172,0.));
#128309=CARTESIAN_POINT('',(20.999603173455,-1.07541989771172,0.));
#128310=CARTESIAN_POINT('',(20.999603173455,-1.07541989771172,400.));
#128311=CARTESIAN_POINT('',(20.999603173455,-1.07541989771172,400.));
#128312=CARTESIAN_POINT('',(20.999603173455,-1.07541989771172,0.));
#128313=CARTESIAN_POINT('Origin',(21.6997740504746,-0.703116603375476,0.));
#128314=CARTESIAN_POINT('',(21.6997740504746,-0.703116603375476,0.));
#128315=CARTESIAN_POINT('',(21.6997740504746,-0.703116603375476,0.));
#128316=CARTESIAN_POINT('',(21.6997740504746,-0.703116603375476,400.));
#128317=CARTESIAN_POINT('',(21.6997740504746,-0.703116603375476,400.));
#128318=CARTESIAN_POINT('',(21.6997740504746,-0.703116603375476,0.));
#128319=CARTESIAN_POINT('Origin',(22.6997740503192,-0.703098971980677,0.));
#128320=CARTESIAN_POINT('',(22.6997740503192,-0.703098971980672,0.));
#128321=CARTESIAN_POINT('',(22.6997740503192,-0.703098971980677,0.));
#128322=CARTESIAN_POINT('',(22.6997740503192,-0.703098971980672,400.));
#128323=CARTESIAN_POINT('',(22.6997740503192,-0.703098971980677,400.));
#128324=CARTESIAN_POINT('',(22.6997740503192,-0.703098971980672,0.));
#128325=CARTESIAN_POINT('Origin',(22.6997793397376,-1.00309897193405,0.));
#128326=CARTESIAN_POINT('',(22.999779339691,-1.00309368251561,0.));
#128327=CARTESIAN_POINT('Origin',(22.6997793397376,-1.00309897193405,0.));
#128328=CARTESIAN_POINT('',(22.999779339691,-1.00309368251561,400.));
#128329=CARTESIAN_POINT('Origin',(22.6997793397376,-1.00309897193405,400.));
#128330=CARTESIAN_POINT('',(22.999779339691,-1.00309368251561,0.));
#128331=CARTESIAN_POINT('Origin',(22.9998507468399,-5.0530936818861,0.));
#128332=CARTESIAN_POINT('',(22.9998507468399,-5.0530936818861,0.));
#128333=CARTESIAN_POINT('',(22.9998507468399,-5.0530936818861,0.));
#128334=CARTESIAN_POINT('',(22.9998507468399,-5.0530936818861,400.));
#128335=CARTESIAN_POINT('',(22.9998507468399,-5.0530936818861,400.));
#128336=CARTESIAN_POINT('',(22.9998507468399,-5.0530936818861,0.));
#128337=CARTESIAN_POINT('Origin',(22.4998507469176,-5.0531024975835,0.));
#128338=CARTESIAN_POINT('',(22.499859562615,-5.55310249750579,0.));
#128339=CARTESIAN_POINT('Origin',(22.4998507469176,-5.0531024975835,0.));
#128340=CARTESIAN_POINT('',(22.499859562615,-5.55310249750579,400.));
#128341=CARTESIAN_POINT('Origin',(22.4998507469176,-5.0531024975835,400.));
#128342=CARTESIAN_POINT('',(22.499859562615,-5.55310249750579,0.));
#128343=CARTESIAN_POINT('Origin',(22.1638595626673,-5.55310842165444,0.));
#128344=CARTESIAN_POINT('',(22.1638595626673,-5.55310842165444,0.));
#128345=CARTESIAN_POINT('',(22.1638595626673,-5.55310842165444,0.));
#128346=CARTESIAN_POINT('',(22.1638595626673,-5.55310842165444,400.));
#128347=CARTESIAN_POINT('',(22.1638595626673,-5.55310842165444,400.));
#128348=CARTESIAN_POINT('',(22.1638595626673,-5.55310842165444,0.));
#128349=CARTESIAN_POINT('Origin',(22.1638771940621,-6.55310842149901,0.));
#128350=CARTESIAN_POINT('',(21.4567579457066,-5.84601410770119,0.));
#128351=CARTESIAN_POINT('Origin',(22.1638771940621,-6.55310842149901,0.));
#128352=CARTESIAN_POINT('',(21.4567579457066,-5.84601410770119,400.));
#128353=CARTESIAN_POINT('Origin',(22.1638771940621,-6.55310842149901,400.));
#128354=CARTESIAN_POINT('',(21.4567579457066,-5.84601410770119,0.));
#128355=CARTESIAN_POINT('Origin',(18.4996895254041,-8.80318680432375,0.));
#128356=CARTESIAN_POINT('',(18.4996895254041,-8.80318680432375,0.));
#128357=CARTESIAN_POINT('',(18.4996895254041,-8.80318680432375,0.));
#128358=CARTESIAN_POINT('',(18.4996895254041,-8.80318680432375,400.));
#128359=CARTESIAN_POINT('',(18.4996895254041,-8.80318680432375,400.));
#128360=CARTESIAN_POINT('',(18.4996895254041,-8.80318680432375,0.));
#128361=CARTESIAN_POINT('Origin',(18.4997027489502,-9.55318680420717,0.));
#128362=CARTESIAN_POINT('',(18.4997027489502,-9.55318680420717,0.));
#128363=CARTESIAN_POINT('',(18.4997027489502,-9.55318680420717,0.));
#128364=CARTESIAN_POINT('',(18.4997027489502,-9.55318680420717,400.));
#128365=CARTESIAN_POINT('',(18.4997027489502,-9.55318680420717,400.));
#128366=CARTESIAN_POINT('',(18.4997027489502,-9.55318680420717,0.));
#128367=CARTESIAN_POINT('Origin',(15.6380920610105,-12.4148984023017,0.));
#128368=CARTESIAN_POINT('',(15.6380920610105,-12.4148984023017,0.));
#128369=CARTESIAN_POINT('',(18.4997027489502,-9.55318680420717,0.));
#128370=CARTESIAN_POINT('',(15.6380920610105,-12.4148984023017,400.));
#128371=CARTESIAN_POINT('',(18.4997027489502,-9.55318680420717,400.));
#128372=CARTESIAN_POINT('',(15.6380920610105,-12.4148984023017,0.));
#128373=CARTESIAN_POINT('Origin',(15.4259562865038,-12.2027701081624,0.));
#128374=CARTESIAN_POINT('',(15.2545493290212,-12.4489806987683,0.));
#128375=CARTESIAN_POINT('Origin',(15.4259562865038,-12.2027701081624,0.));
#128376=CARTESIAN_POINT('',(15.2545493290212,-12.4489806987683,400.));
#128377=CARTESIAN_POINT('Origin',(15.4259562865038,-12.2027701081624,400.));
#128378=CARTESIAN_POINT('',(15.2545493290212,-12.4489806987683,0.));
#128379=CARTESIAN_POINT('Origin',(14.8102803067574,-13.0532372410527,0.));
#128380=CARTESIAN_POINT('',(15.250070467987,-13.6607609689548,0.));
#128381=CARTESIAN_POINT('Origin',(14.8102803067574,-13.0532372410527,0.));
#128382=CARTESIAN_POINT('',(15.250070467987,-13.6607609689548,400.));
#128383=CARTESIAN_POINT('Origin',(14.8102803067574,-13.0532372410527,400.));
#128384=CARTESIAN_POINT('',(15.2500702858638,-13.6607607173708,0.));
#128385=CARTESIAN_POINT('Origin',(15.4259862775064,-13.903770107898,0.));
#128386=CARTESIAN_POINT('',(15.6381145716457,-13.6916343333914,0.));
#128387=CARTESIAN_POINT('Origin',(15.4259862775064,-13.903770107898,0.));
#128388=CARTESIAN_POINT('',(15.6381145716457,-13.6916343333914,400.));
#128389=CARTESIAN_POINT('Origin',(15.4259862775064,-13.903770107898,400.));
#128390=CARTESIAN_POINT('',(15.6381145716457,-13.6916343333914,0.));
#128391=CARTESIAN_POINT('Origin',(18.4998261697403,-16.5532450213311,0.));
#128392=CARTESIAN_POINT('',(18.4998261697403,-16.5532450213311,0.));
#128393=CARTESIAN_POINT('',(18.4998261697403,-16.5532450213311,0.));
#128394=CARTESIAN_POINT('',(18.4998261697403,-16.5532450213311,400.));
#128395=CARTESIAN_POINT('',(18.4998261697403,-16.5532450213311,400.));
#128396=CARTESIAN_POINT('',(18.4998261697403,-16.5532450213311,0.));
#128397=CARTESIAN_POINT('Origin',(18.4998349854377,-17.0532450212534,0.));
#128398=CARTESIAN_POINT('',(18.4998349854377,-17.0532450212534,0.));
#128399=CARTESIAN_POINT('',(18.4998349854377,-17.0532450212534,400.));
#128400=CARTESIAN_POINT('Origin',(0.,1.9455,400.));
#128401=CARTESIAN_POINT('Origin',(0.,1.9455,0.));
#128402=CARTESIAN_POINT('',(0.,0.,0.));
#128403=CARTESIAN_POINT('Origin',(-26.8463464956315,10.1295,7.));
#128404=CARTESIAN_POINT('',(-23.3525227612526,5.6491961756188,9.4344770775744));
#128405=CARTESIAN_POINT('',(-23.4778327537502,5.64975127298007,9.43417554508985));
#128406=CARTESIAN_POINT('',(-26.8463464956315,5.6491961756188,9.4344770775744));
#128407=CARTESIAN_POINT('',(-23.534,5.20511879703991,5.67702200776683));
#128408=CARTESIAN_POINT('Ctrl Pts',(-23.534,5.20511879703991,5.67702200776683));
#128409=CARTESIAN_POINT('Ctrl Pts',(-23.5270930683901,5.16684928138222,
5.81946858258322));
#128410=CARTESIAN_POINT('Ctrl Pts',(-23.5201861367802,5.13475838719278,
5.96360047114363));
#128411=CARTESIAN_POINT('Ctrl Pts',(-23.5132792051702,5.10897409853572,
6.10886551367019));
#128412=CARTESIAN_POINT('Ctrl Pts',(-23.5063724191029,5.08319035320424,
6.25412749517716));
#128413=CARTESIAN_POINT('Ctrl Pts',(-23.4994656330356,5.06371301191541,
6.40052225348957));
#128414=CARTESIAN_POINT('Ctrl Pts',(-23.4925588469683,5.05061883811789,
6.54748796316664));
#128415=CARTESIAN_POINT('Ctrl Pts',(-23.4856526672931,5.03752581394379,
6.69444076975994));
#128416=CARTESIAN_POINT('Ctrl Pts',(-23.4787464876178,5.03081486640317,
6.84196409317217));
#128417=CARTESIAN_POINT('Ctrl Pts',(-23.4718403079426,5.03051082838708,
6.98949153797162));
#128418=CARTESIAN_POINT('Ctrl Pts',(-23.4649324605092,5.03020671694952,
7.13705460884823));
#128419=CARTESIAN_POINT('Ctrl Pts',(-23.4580246130759,5.03631260848016,
7.28462146729368));
#128420=CARTESIAN_POINT('Ctrl Pts',(-23.4511167656425,5.04880119697881,
7.43162561668542));
#128421=CARTESIAN_POINT('Ctrl Pts',(-23.4457233772622,5.05855181882527,
7.54640094703871));
#128422=CARTESIAN_POINT('Ctrl Pts',(-23.4403299888818,5.07219222530018,
7.66083321109948));
#128423=CARTESIAN_POINT('Ctrl Pts',(-23.4349366005015,5.08968742686135,
7.77465490873909));
#128424=CARTESIAN_POINT('Ctrl Pts',(-23.4280025544932,5.11218025029517,
7.92099053905438));
#128425=CARTESIAN_POINT('Ctrl Pts',(-23.421068508485,5.14105472641507,8.06637105423135));
#128426=CARTESIAN_POINT('Ctrl Pts',(-23.4141344624767,5.17620499254735,
8.2102353362651));
#128427=CARTESIAN_POINT('Ctrl Pts',(-23.4072019044794,5.21134771561133,
8.35406874575578));
#128428=CARTESIAN_POINT('Ctrl Pts',(-23.4002693464821,5.25276346236797,
8.49638625049076));
#128429=CARTESIAN_POINT('Ctrl Pts',(-23.3933367884849,5.3002956501243,8.63663873446207));
#128430=CARTESIAN_POINT('Ctrl Pts',(-23.386403940659,5.34782982505307,8.77689708195206));
#128431=CARTESIAN_POINT('Ctrl Pts',(-23.3794710928331,5.40148084971533,
8.91508992173121));
#128432=CARTESIAN_POINT('Ctrl Pts',(-23.3725382450072,5.46104263992793,
9.05068448991768));
#128433=CARTESIAN_POINT('Ctrl Pts',(-23.365866417089,5.51836194431456,9.1811739580702));
#128434=CARTESIAN_POINT('Ctrl Pts',(-23.3591945891708,5.58115492638012,
9.30925697507771));
#128435=CARTESIAN_POINT('Ctrl Pts',(-23.3525227612526,5.6491961756188,9.4344770775744));
#128436=CARTESIAN_POINT('',(-23.534,5.20509380555675,8.32288496556916));
#128437=CARTESIAN_POINT('Origin',(-23.534,10.1295,7.));
#128438=CARTESIAN_POINT('Ctrl Pts',(-23.534,5.20509380555674,8.3228849655691));
#128439=CARTESIAN_POINT('Ctrl Pts',(-23.5152775845834,5.30884009368174,
8.7090779280641));
#128440=CARTESIAN_POINT('Ctrl Pts',(-23.4965551691667,5.45884546440214,
9.08275280579124));
#128441=CARTESIAN_POINT('Ctrl Pts',(-23.4778327537501,5.6497512729813,9.43417554509213));
#128442=CARTESIAN_POINT('Origin',(-26.8463464956315,10.1295,7.));
#128443=CARTESIAN_POINT('',(-21.8525208770954,5.64940737302611,9.43436256508443));
#128444=CARTESIAN_POINT('',(-21.9778242975584,5.64919617561881,9.43447707757441));
#128445=CARTESIAN_POINT('',(-26.8463464956315,5.6491961756188,9.4344770775744));
#128446=CARTESIAN_POINT('',(-23.0963464956316,10.1295667748524,12.0990157389949));
#128447=CARTESIAN_POINT('Ctrl Pts',(-23.0963464956316,10.129566778808,12.099317792417));
#128448=CARTESIAN_POINT('Ctrl Pts',(-23.0928642190133,10.2039288711016,
12.0993673408814));
#128449=CARTESIAN_POINT('Ctrl Pts',(-23.0506000607591,11.1064308613037,
12.0800148219986));
#128450=CARTESIAN_POINT('Ctrl Pts',(-22.9695540208687,12.8165649252773,
11.5744658007328));
#128451=CARTESIAN_POINT('Ctrl Pts',(-22.8532083759605,14.6458800384554,
9.78358876962574));
#128452=CARTESIAN_POINT('Ctrl Pts',(-22.7368627310523,15.4235830862095,
7.34457044966851));
#128453=CARTESIAN_POINT('Ctrl Pts',(-22.6205170861442,14.9685952857722,
4.82532064892663));
#128454=CARTESIAN_POINT('Ctrl Pts',(-22.504171441236,13.3868454525908,2.8124323194202));
#128455=CARTESIAN_POINT('Ctrl Pts',(-22.3878257963277,11.0466612589386,
1.77459151989547));
#128456=CARTESIAN_POINT('Ctrl Pts',(-22.2714801514196,8.49288304070303,
1.95345842253097));
#128457=CARTESIAN_POINT('Ctrl Pts',(-22.1551345065114,6.32026199879215,
3.30737376532056));
#128458=CARTESIAN_POINT('Ctrl Pts',(-22.0387888616032,5.03442895202576,
5.52111017618096));
#128459=CARTESIAN_POINT('Ctrl Pts',(-21.9379176517979,4.94849006028041,
7.73893242254741));
#128460=CARTESIAN_POINT('Ctrl Pts',(-21.8758283236286,5.41193861852495,
8.99675599064833));
#128461=CARTESIAN_POINT('Ctrl Pts',(-21.8525208770954,5.64940737302611,
9.43436256508443));
#128462=CARTESIAN_POINT('Ctrl Pts',(-23.3525227612526,5.6491961756188,9.4344770775744));
#128463=CARTESIAN_POINT('Ctrl Pts',(-23.3455889849682,5.7199088507827,9.56461355406351));
#128464=CARTESIAN_POINT('Ctrl Pts',(-23.3386552086839,5.79629012476817,
9.69165746727976));
#128465=CARTESIAN_POINT('Ctrl Pts',(-23.3317214323995,5.87804227441008,
9.81512134863167));
#128466=CARTESIAN_POINT('Ctrl Pts',(-23.3273446067974,5.92964689603369,
9.89305577493429));
#128467=CARTESIAN_POINT('Ctrl Pts',(-23.3229677811954,5.98339066303623,
9.96956424290311));
#128468=CARTESIAN_POINT('Ctrl Pts',(-23.3185909555933,6.03918981564711,
10.0445301108347));
#128469=CARTESIAN_POINT('Ctrl Pts',(-23.3116576154912,6.12758138927417,
10.1632837249084));
#128470=CARTESIAN_POINT('Ctrl Pts',(-23.3047242753892,6.22116338578777,
10.2782058956994));
#128471=CARTESIAN_POINT('Ctrl Pts',(-23.2977909352871,6.31957962315755,
10.3888505015891));
#128472=CARTESIAN_POINT('Ctrl Pts',(-23.2908589155155,6.41797711891765,
10.4994740371953));
#128473=CARTESIAN_POINT('Ctrl Pts',(-23.2839268957439,6.52120679919789,
10.6058213862123));
#128474=CARTESIAN_POINT('Ctrl Pts',(-23.2769948759722,6.6288732637029,10.7074807421107));
#128475=CARTESIAN_POINT('Ctrl Pts',(-23.2700626150757,6.73654347330225,
10.8091436341509));
#128476=CARTESIAN_POINT('Ctrl Pts',(-23.2631303541791,6.84865053786314,
10.9061179773461));
#128477=CARTESIAN_POINT('Ctrl Pts',(-23.2561980932826,6.96476298683125,
10.9980295943727));
#128478=CARTESIAN_POINT('Ctrl Pts',(-23.2492662087238,7.0808691323009,11.0899362217126));
#128479=CARTESIAN_POINT('Ctrl Pts',(-23.242334324165,7.20097996725737,11.1767804683626));
#128480=CARTESIAN_POINT('Ctrl Pts',(-23.2354024396062,7.32463180495121,
11.2582291399599));
#128481=CARTESIAN_POINT('Ctrl Pts',(-23.228469013263,7.44831114519013,11.3396959273071));
#128482=CARTESIAN_POINT('Ctrl Pts',(-23.2215355869198,7.57553278566342,
11.4157645597462));
#128483=CARTESIAN_POINT('Ctrl Pts',(-23.2146021605767,7.70580446372732,
11.4861454443043));
#128484=CARTESIAN_POINT('Ctrl Pts',(-23.2104832106128,7.78319513568308,
11.5279567115708));
#128485=CARTESIAN_POINT('Ctrl Pts',(-23.206364260649,7.86166171055421,11.5677615028386));
#128486=CARTESIAN_POINT('Ctrl Pts',(-23.2022453106851,7.94109688570871,
11.6055067918048));
#128487=CARTESIAN_POINT('Ctrl Pts',(-23.1953326013538,8.0744105412136,11.6688535703621));
#128488=CARTESIAN_POINT('Ctrl Pts',(-23.1884198920225,8.21050236448007,
11.7264202219746));
#128489=CARTESIAN_POINT('Ctrl Pts',(-23.1815071826912,8.34885199561309,
11.7779800841436));
#128490=CARTESIAN_POINT('Ctrl Pts',(-23.1744104587696,8.49088445926188,
11.8309124569247));
#128491=CARTESIAN_POINT('Ctrl Pts',(-23.1673137348479,8.63529628394864,
11.8775136191942));
#128492=CARTESIAN_POINT('Ctrl Pts',(-23.1602170109263,8.78150369622116,
11.9175915817602));
#128493=CARTESIAN_POINT('Ctrl Pts',(-23.1533056463726,8.92389231635461,
11.9566227478196));
#128494=CARTESIAN_POINT('Ctrl Pts',(-23.1463942818189,9.06798355227891,
11.9894671549689));
#128495=CARTESIAN_POINT('Ctrl Pts',(-23.1394829172652,9.21322389390579,
12.0159983151314));
#128496=CARTESIAN_POINT('Ctrl Pts',(-23.1322935136596,9.36430714637444,
12.0435968041202));
#128497=CARTESIAN_POINT('Ctrl Pts',(-23.125104110054,9.51663350849815,12.0643634281151));
#128498=CARTESIAN_POINT('Ctrl Pts',(-23.1179147064484,9.66956947446774,
12.0782147366652));
#128499=CARTESIAN_POINT('Ctrl Pts',(-23.1107253028428,9.82250544043734,
12.0920660452153));
#128500=CARTESIAN_POINT('Ctrl Pts',(-23.1035358992372,9.97605060390634,
12.0990020099546));
#128501=CARTESIAN_POINT('Ctrl Pts',(-23.0963464956316,10.1295667746463,
12.0989999995628));
#128502=CARTESIAN_POINT('',(-23.2216535038385,10.1296134643043,12.0989502562419));
#128503=CARTESIAN_POINT('Ctrl Pts',(-23.4778327537501,5.6497512729813,9.43417554509213));
#128504=CARTESIAN_POINT('Ctrl Pts',(-23.4577732875307,5.85429051287487,
9.81069494234303));
#128505=CARTESIAN_POINT('Ctrl Pts',(-23.3989319396752,6.59199771031906,
10.8402274681031));
#128506=CARTESIAN_POINT('Ctrl Pts',(-23.3135388565479,8.1665770620453,11.8658594947153));
#128507=CARTESIAN_POINT('Ctrl Pts',(-23.2482052396401,9.56246707210738,
12.0983697268913));
#128508=CARTESIAN_POINT('Ctrl Pts',(-23.2216535043684,10.1296134499674,
12.0988145792455));
#128509=CARTESIAN_POINT('Ctrl Pts',(-23.2216535036443,10.1296134695606,
12.0989999987375));
#128510=CARTESIAN_POINT('Ctrl Pts',(-23.2144616176573,10.2832380933687,
12.0989965800831));
#128511=CARTESIAN_POINT('Ctrl Pts',(-23.2072697316703,10.4368320308009,
12.092046129591));
#128512=CARTESIAN_POINT('Ctrl Pts',(-23.2000778456833,10.589781612833,12.0781829266863));
#128513=CARTESIAN_POINT('Ctrl Pts',(-23.1950395855473,10.6969301109268,
12.0684710899472));
#128514=CARTESIAN_POINT('Ctrl Pts',(-23.1900013254114,10.80376240697,12.0553677903385));
#128515=CARTESIAN_POINT('Ctrl Pts',(-23.1849630652754,10.9100690396704,
12.0388999766128));
#128516=CARTESIAN_POINT('Ctrl Pts',(-23.1780322210911,11.0563089493057,
12.016246154081));
#128517=CARTESIAN_POINT('Ctrl Pts',(-23.1711013769068,11.2015880256627,
11.9872177039362));
#128518=CARTESIAN_POINT('Ctrl Pts',(-23.1641705327225,11.3453457830432,
11.9519208426484));
#128519=CARTESIAN_POINT('Ctrl Pts',(-23.1572410393046,11.4890755231802,
11.9166308604382));
#128520=CARTESIAN_POINT('Ctrl Pts',(-23.1503115458867,11.6312842144825,
11.875074983332));
#128521=CARTESIAN_POINT('Ctrl Pts',(-23.1433820524688,11.7714233688928,
11.8274101390584));
#128522=CARTESIAN_POINT('Ctrl Pts',(-23.1364523390414,11.9115669726828,
11.779743781439));
#128523=CARTESIAN_POINT('Ctrl Pts',(-23.129522625614,12.0496405935019,11.725968171853));
#128524=CARTESIAN_POINT('Ctrl Pts',(-23.1225929121865,12.1851121473728,
11.666289714492));
#128525=CARTESIAN_POINT('Ctrl Pts',(-23.1156635809782,12.3205762291,11.6066145487888));
#128526=CARTESIAN_POINT('Ctrl Pts',(-23.1087342497699,12.453438228391,11.5410373210932));
#128527=CARTESIAN_POINT('Ctrl Pts',(-23.1018049185616,12.5831872350453,
11.4698120712817));
#128528=CARTESIAN_POINT('Ctrl Pts',(-23.0948740323597,12.7129653583441,
11.3985708379931));
#128529=CARTESIAN_POINT('Ctrl Pts',(-23.0879431461578,12.8396288027836,
11.3216792094331));
#128530=CARTESIAN_POINT('Ctrl Pts',(-23.0810122599559,12.9626918508012,
11.2394368654992));
#128531=CARTESIAN_POINT('Ctrl Pts',(-23.0768806467596,13.0360517211474,
11.1904108760966));
#128532=CARTESIAN_POINT('Ctrl Pts',(-23.0727490335634,13.1081326835169,
11.1394843440002));
#128533=CARTESIAN_POINT('Ctrl Pts',(-23.0686174203672,13.1788367906057,
11.0867280478958));
#128534=CARTESIAN_POINT('Ctrl Pts',(-23.0616832477982,13.2975009676742,
10.9981860562044));
#128535=CARTESIAN_POINT('Ctrl Pts',(-23.0547490752291,13.4123264715572,
10.9044570184215));
#128536=CARTESIAN_POINT('Ctrl Pts',(-23.0478149026601,13.5228675281008,
10.8058977678376));
#128537=CARTESIAN_POINT('Ctrl Pts',(-23.0408820410097,13.6333876866445,
10.7073571500701));
#128538=CARTESIAN_POINT('Ctrl Pts',(-23.0339491793593,13.7396247673742,
10.6039883612046));
#128539=CARTESIAN_POINT('Ctrl Pts',(-23.027016317709,13.8411673613832,10.4961874089417));
#128540=CARTESIAN_POINT('Ctrl Pts',(-23.0200832090312,13.9427135734955,
10.3883826155816));
#128541=CARTESIAN_POINT('Ctrl Pts',(-23.0131501003533,14.0395647351762,
10.2761455810761));
#128542=CARTESIAN_POINT('Ctrl Pts',(-23.0062169916755,14.131347111674,10.1599083364532));
#128543=CARTESIAN_POINT('Ctrl Pts',(-22.9992842580324,14.2231245233599,
10.0436773794868));
#128544=CARTESIAN_POINT('Ctrl Pts',(-22.9923515243894,14.3098334944501,
9.9234469053268));
#128545=CARTESIAN_POINT('Ctrl Pts',(-22.9854187907463,14.3911413124602,
9.79968111111478));
#128546=CARTESIAN_POINT('Ctrl Pts',(-22.9784845207415,14.4724671490789,
9.67588788919075));
#128547=CARTESIAN_POINT('Ctrl Pts',(-22.9715502507368,14.5483892594452,
9.54855805804282));
#128548=CARTESIAN_POINT('Ctrl Pts',(-22.9646159807321,14.6186185668019,
9.41818433813362));
#128549=CARTESIAN_POINT('Ctrl Pts',(-22.960501245641,14.6602920227245,9.34082171454237));
#128550=CARTESIAN_POINT('Ctrl Pts',(-22.95638651055,14.6999618159018,9.26238781469777));
#128551=CARTESIAN_POINT('Ctrl Pts',(-22.952271775459,14.7375752110852,9.18298965846895));
#128552=CARTESIAN_POINT('Ctrl Pts',(-22.9453381247487,14.800956726167,9.04919755031274));
#128553=CARTESIAN_POINT('Ctrl Pts',(-22.9384044740384,14.8585183931822,
8.91262019456305));
#128554=CARTESIAN_POINT('Ctrl Pts',(-22.9314708233281,14.9100334467114,
8.77378154372893));
#128555=CARTESIAN_POINT('Ctrl Pts',(-22.92453848664,14.9615387374293,8.63496920472942));
#128556=CARTESIAN_POINT('Ctrl Pts',(-22.917606149952,15.0069995860105,8.49389673540899));
#128557=CARTESIAN_POINT('Ctrl Pts',(-22.9106738132639,15.0462379353463,
8.35110661131037));
#128558=CARTESIAN_POINT('Ctrl Pts',(-22.9037412290525,15.085477685711,8.20831138880432));
#128559=CARTESIAN_POINT('Ctrl Pts',(-22.8968086448412,15.1184944014449,
8.06379870665251));
#128560=CARTESIAN_POINT('Ctrl Pts',(-22.8898760606299,15.1451601822359,
7.91812522911281));
#128561=CARTESIAN_POINT('Ctrl Pts',(-22.8829438499011,15.1718245264478,
7.77245959951431));
#128562=CARTESIAN_POINT('Ctrl Pts',(-22.8760116391724,15.1921385617596,
7.62563362499968));
#128563=CARTESIAN_POINT('Ctrl Pts',(-22.8690794284437,15.2060256970908,
7.47821318130803));
#128564=CARTESIAN_POINT('Ctrl Pts',(-22.8621456743553,15.2199159241982,
7.33075991651844));
#128565=CARTESIAN_POINT('Ctrl Pts',(-22.855211920267,15.2273763612686,7.18271224732234));
#128566=CARTESIAN_POINT('Ctrl Pts',(-22.8482781661786,15.2283823298558,
7.03464081817565));
#128567=CARTESIAN_POINT('Ctrl Pts',(-22.8441608209693,15.2289796859043,
6.9467142517509));
#128568=CARTESIAN_POINT('Ctrl Pts',(-22.8400434757601,15.2273021079282,
6.85877936703632));
#128569=CARTESIAN_POINT('Ctrl Pts',(-22.8359261305508,15.223353127859,6.77095565538246));
#128570=CARTESIAN_POINT('Ctrl Pts',(-22.8289927904143,15.2167033036104,
6.62306626695431));
#128571=CARTESIAN_POINT('Ctrl Pts',(-22.8220594502778,15.2036075003542,
6.47544108085083));
#128572=CARTESIAN_POINT('Ctrl Pts',(-22.8151261101414,15.1841106766401,
6.32864919185574));
#128573=CARTESIAN_POINT('Ctrl Pts',(-22.8081940903344,15.1646175657443,
6.18188525672731));
#128574=CARTESIAN_POINT('Ctrl Pts',(-22.8012620705275,15.1387259098974,
6.03595462967193));
#128575=CARTESIAN_POINT('Ctrl Pts',(-22.7943300507205,15.1065323796292,
5.8914199658471));
#128576=CARTESIAN_POINT('Ctrl Pts',(-22.7873977897876,15.0743377295293,
5.74688027447465));
#128577=CARTESIAN_POINT('Ctrl Pts',(-22.7804655288547,15.0358408349672,
5.60373696693589));
#128578=CARTESIAN_POINT('Ctrl Pts',(-22.7735332679218,14.9911893286948,
5.46254174975221));
#128579=CARTESIAN_POINT('Ctrl Pts',(-22.7666013833261,14.9465402464547,
5.32135419774698));
#128580=CARTESIAN_POINT('Ctrl Pts',(-22.7596694987304,14.8957373216521,
5.18211483944176));
#128581=CARTESIAN_POINT('Ctrl Pts',(-22.7527376141347,14.8389778369684,
5.04535949517476));
#128582=CARTESIAN_POINT('Ctrl Pts',(-22.7458041877542,14.7822057278808,
4.9085737338822));
#128583=CARTESIAN_POINT('Ctrl Pts',(-22.7388707613737,14.7194745384637,
4.77427339605927));
#128584=CARTESIAN_POINT('Ctrl Pts',(-22.7319373349933,14.6510296539597,
4.64297420710704));
#128585=CARTESIAN_POINT('Ctrl Pts',(-22.7278183852097,14.6103685108622,
4.56497312420261));
#128586=CARTESIAN_POINT('Ctrl Pts',(-22.7236994354262,14.5676917913382,
4.48803079706271));
#128587=CARTESIAN_POINT('Ctrl Pts',(-22.7195804856426,14.5230586438665,
4.4122512790253));
#128588=CARTESIAN_POINT('Ctrl Pts',(-22.7126467716635,14.4479245696929,
4.28468635807346));
#128589=CARTESIAN_POINT('Ctrl Pts',(-22.7057130576844,14.3672181376313,
4.16037390646582));
#128590=CARTESIAN_POINT('Ctrl Pts',(-22.6987793437054,14.2812456294001,
4.03979574543294));
#128591=CARTESIAN_POINT('Ctrl Pts',(-22.6918469440267,14.1952894174433,
3.91924044025052));
#128592=CARTESIAN_POINT('Ctrl Pts',(-22.6849145443481,14.1040693126661,
3.8024182823838));
#128593=CARTESIAN_POINT('Ctrl Pts',(-22.6779821446695,14.0079342710063,
3.68978118465205));
#128594=CARTESIAN_POINT('Ctrl Pts',(-22.6710494985103,13.9117958112779,
3.57714008212316));
#128595=CARTESIAN_POINT('Ctrl Pts',(-22.6641168523511,13.810742277035,3.4686845910636));
#128596=CARTESIAN_POINT('Ctrl Pts',(-22.6571842061919,13.7051625248584,
3.36483308384289));
#128597=CARTESIAN_POINT('Ctrl Pts',(-22.6502519342582,13.5995884718967,
3.26098718254614));
#128598=CARTESIAN_POINT('Ctrl Pts',(-22.6433196623246,13.4894889262164,
3.16174499892527));
#128599=CARTESIAN_POINT('Ctrl Pts',(-22.6363873903909,13.375289173411,3.06748761708652));
#128600=CARTESIAN_POINT('Ctrl Pts',(-22.6294535767895,13.2610640237249,
2.97320927335051));
#128601=CARTESIAN_POINT('Ctrl Pts',(-22.622519763188,13.1427370999496,2.88391815695374));
#128602=CARTESIAN_POINT('Ctrl Pts',(-22.6155859495865,13.0207667789116,
2.79995507010194));
#128603=CARTESIAN_POINT('Ctrl Pts',(-22.6114689133025,12.9483454151206,
2.7501009645609));
#128604=CARTESIAN_POINT('Ctrl Pts',(-22.6073518770184,12.8746401652181,
2.70212448718511));
#128605=CARTESIAN_POINT('Ctrl Pts',(-22.6032348407344,12.7997518707891,
2.65608978608592));
#128606=CARTESIAN_POINT('Ctrl Pts',(-22.5963013561296,12.6736327888376,
2.57856292711801));
#128607=CARTESIAN_POINT('Ctrl Pts',(-22.5893678715248,12.5441133362429,
2.50651890621843));
#128608=CARTESIAN_POINT('Ctrl Pts',(-22.5824343869199,12.4116897238054,
2.4402400211681));
#128609=CARTESIAN_POINT('Ctrl Pts',(-22.5755022202333,12.2792912824762,
2.37397373442229));
#128610=CARTESIAN_POINT('Ctrl Pts',(-22.5685700535467,12.1439900781449,
2.31347054505179));
#128611=CARTESIAN_POINT('Ctrl Pts',(-22.5616378868601,12.0063060236781,
2.25896634166285));
#128612=CARTESIAN_POINT('Ctrl Pts',(-22.5547054768533,11.8686171364781,
2.20446022516737));
#128613=CARTESIAN_POINT('Ctrl Pts',(-22.5477730668465,11.7285455379248,
2.15595364079637));
#128614=CARTESIAN_POINT('Ctrl Pts',(-22.5408406568397,11.5866306909856,
2.11363415723017));
#128615=CARTESIAN_POINT('Ctrl Pts',(-22.5339086222827,11.4447235299589,
2.07131696562882));
#128616=CARTESIAN_POINT('Ctrl Pts',(-22.5269765877257,11.3009736373841,
2.03518629791229));
#128617=CARTESIAN_POINT('Ctrl Pts',(-22.5200445531686,11.1559352036829,
2.00537971687132));
#128618=CARTESIAN_POINT('Ctrl Pts',(-22.5131109767612,11.0108645099632,
1.97556650613344));
#128619=CARTESIAN_POINT('Ctrl Pts',(-22.5061774003538,10.864505026392,1.95208025927438));
#128620=CARTESIAN_POINT('Ctrl Pts',(-22.4992438239464,10.7174213194625,
1.9350074509313));
#128621=CARTESIAN_POINT('Ctrl Pts',(-22.495125614573,10.6300607042531,1.92486702768973));
#128622=CARTESIAN_POINT('Ctrl Pts',(-22.4910074051996,10.5424447657293,
1.91698814828052));
#128623=CARTESIAN_POINT('Ctrl Pts',(-22.4868891958262,10.4546927511912,
1.9113802780545));
#128624=CARTESIAN_POINT('Ctrl Pts',(-22.4799556232166,10.3069501501543,
1.90193865625436));
#128625=CARTESIAN_POINT('Ctrl Pts',(-22.4730220506069,10.158770604134,1.89893406224141));
#128626=CARTESIAN_POINT('Ctrl Pts',(-22.4660884779973,10.0107247644674,
1.90238355273524));
#128627=CARTESIAN_POINT('Ctrl Pts',(-22.4591562216396,9.86270702945001,
1.90583238838649));
#128628=CARTESIAN_POINT('Ctrl Pts',(-22.4522239652819,9.71482328045241,
1.91573285633567));
#128629=CARTESIAN_POINT('Ctrl Pts',(-22.4452917089242,9.56764337792384,
1.93204990787901));
#128630=CARTESIAN_POINT('Ctrl Pts',(-22.4383592076211,9.420458274917,1.94836753597166));
#128631=CARTESIAN_POINT('Ctrl Pts',(-22.4314267063179,9.27397739706878,
1.97110216823797));
#128632=CARTESIAN_POINT('Ctrl Pts',(-22.4244942050148,9.12876525084503,
2.00016690660241));
#128633=CARTESIAN_POINT('Ctrl Pts',(-22.41756207846,8.98356095431581,2.02923007382199));
#128634=CARTESIAN_POINT('Ctrl Pts',(-22.4106299519053,8.83962557614821,
2.06462259662998));
#128635=CARTESIAN_POINT('Ctrl Pts',(-22.4036978253505,8.69751321817358,
2.10620649631859));
#128636=CARTESIAN_POINT('Ctrl Pts',(-22.3967641566674,8.55536924572963,
2.14779964680663));
#128637=CARTESIAN_POINT('Ctrl Pts',(-22.3898304879842,8.41504942121115,
2.19558683341147));
#128638=CARTESIAN_POINT('Ctrl Pts',(-22.3828968193011,8.27709309039585,
2.24938007821602));
#128639=CARTESIAN_POINT('Ctrl Pts',(-22.3787790631734,8.19516380410787,
2.28132672486794));
#128640=CARTESIAN_POINT('Ctrl Pts',(-22.3746613070457,8.11406779091711,
2.31539071346896));
#128641=CARTESIAN_POINT('Ctrl Pts',(-22.370543550918,8.03391480971792,2.35152458215918));
#128642=CARTESIAN_POINT('Ctrl Pts',(-22.3636099925257,7.89895165060084,
2.41236749775123));
#128643=CARTESIAN_POINT('Ctrl Pts',(-22.3566764341333,7.76661674914673,
2.47910262080128));
#128644=CARTESIAN_POINT('Ctrl Pts',(-22.3497428757409,7.63742230671767,
2.55147779924112));
#128645=CARTESIAN_POINT('Ctrl Pts',(-22.3428106342854,7.5082524030468,2.62383923098281));
#128646=CARTESIAN_POINT('Ctrl Pts',(-22.3358783928298,7.3822220565691,2.70183841932422));
#128647=CARTESIAN_POINT('Ctrl Pts',(-22.3289461513742,7.25981836998035,
2.78517754320212));
#128648=CARTESIAN_POINT('Ctrl Pts',(-22.322013665852,7.13741037386829,2.86851960123916));
#128649=CARTESIAN_POINT('Ctrl Pts',(-22.3150811803298,7.01862956828097,
2.95720178773977));
#128650=CARTESIAN_POINT('Ctrl Pts',(-22.3081486948075,6.90393404520842,
3.05088297574135));
#128651=CARTESIAN_POINT('Ctrl Pts',(-22.3012165844928,6.78924472981139,
3.14455909342806));
#128652=CARTESIAN_POINT('Ctrl Pts',(-22.2942844741781,6.67864050993959,
3.24323346137456));
#128653=CARTESIAN_POINT('Ctrl Pts',(-22.2873523638634,6.5725463642529,3.34652469104477));
#128654=CARTESIAN_POINT('Ctrl Pts',(-22.2804187119845,6.4664286253275,3.44983889064064));
#128655=CARTESIAN_POINT('Ctrl Pts',(-22.2734850601056,6.36482320156598,
3.55777177275135));
#128656=CARTESIAN_POINT('Ctrl Pts',(-22.2665514082267,6.2681186198229,3.66990468052016));
#128657=CARTESIAN_POINT('Ctrl Pts',(-22.2624335741544,6.21068663035953,
3.73649941534445));
#128658=CARTESIAN_POINT('Ctrl Pts',(-22.2583157400821,6.15498248326484,
3.80457483855878));
#128659=CARTESIAN_POINT('Ctrl Pts',(-22.2541979060098,6.10108093818732,
3.87403761020318));
#128660=CARTESIAN_POINT('Ctrl Pts',(-22.247264295271,6.01032149396891,3.99099905424433));
#128661=CARTESIAN_POINT('Ctrl Pts',(-22.2403306845322,5.92464363472474,
4.11193600283431));
#128662=CARTESIAN_POINT('Ctrl Pts',(-22.2333970737934,5.84438185374589,
4.23638579525945));
#128663=CARTESIAN_POINT('Ctrl Pts',(-22.2264647793601,5.76413530999738,
4.36081196161838));
#128664=CARTESIAN_POINT('Ctrl Pts',(-22.2195324849268,5.68930297214713,
4.48874936360589));
#128665=CARTESIAN_POINT('Ctrl Pts',(-22.2126001904935,5.62017577060433,
4.61970674197797));
#128666=CARTESIAN_POINT('Ctrl Pts',(-22.2056676515668,5.55104613103073,
4.75066873905461));
#128667=CARTESIAN_POINT('Ctrl Pts',(-22.1987351126401,5.48762218766616,
4.88465063487431));
#128668=CARTESIAN_POINT('Ctrl Pts',(-22.1918025737133,5.43014895812622,
5.02113649150837));
#128669=CARTESIAN_POINT('Ctrl Pts',(-22.1848704098817,5.37267883825905,
5.15761496337642));
#128670=CARTESIAN_POINT('Ctrl Pts',(-22.1779382460501,5.3211589153847,5.2965968199325));
#128671=CARTESIAN_POINT('Ctrl Pts',(-22.1710060822185,5.27578609499789,
5.43754605559421));
#128672=CARTESIAN_POINT('Ctrl Pts',(-22.1640723771204,5.23040318662025,
5.57852662928132));
#128673=CARTESIAN_POINT('Ctrl Pts',(-22.1571386720224,5.19117021294783,
5.72147514131237));
#128674=CARTESIAN_POINT('Ctrl Pts',(-22.1502049669243,5.15823441927751,
5.8658397265272));
#128675=CARTESIAN_POINT('Ctrl Pts',(-22.1460873983168,5.13867555599091,
5.95157038217522));
#128676=CARTESIAN_POINT('Ctrl Pts',(-22.1419698297092,5.12133647341795,
6.03780015164788));
#128677=CARTESIAN_POINT('Ctrl Pts',(-22.1378522611016,5.10623951371014,
6.12441157677879));
#128678=CARTESIAN_POINT('Ctrl Pts',(-22.1309189485113,5.08081870089726,
6.27025106157069));
#128679=CARTESIAN_POINT('Ctrl Pts',(-22.123985635921,5.06174897458694,6.41722355017293));
#128680=CARTESIAN_POINT('Ctrl Pts',(-22.1170523233307,5.04910923496427,
6.56476365668796));
#128681=CARTESIAN_POINT('Ctrl Pts',(-22.1101203285711,5.03647189780609,
6.71227571991428));
#128682=CARTESIAN_POINT('Ctrl Pts',(-22.1031883338116,5.03026213714831,
6.86035485655778));
#128683=CARTESIAN_POINT('Ctrl Pts',(-22.096256339052,5.03050696985794,7.00843081032557));
#128684=CARTESIAN_POINT('Ctrl Pts',(-22.0893240991684,5.03075181122517,
7.1565120002449));
#128685=CARTESIAN_POINT('Ctrl Pts',(-22.0823918592848,5.03745170547962,
7.3045896764382));
#128686=CARTESIAN_POINT('Ctrl Pts',(-22.0754596194012,5.05058154531324,
7.45209327648424));
#128687=CARTESIAN_POINT('Ctrl Pts',(-22.0685277535374,5.06371067674367,
7.59958891816818));
#128688=CARTESIAN_POINT('Ctrl Pts',(-22.0615958876737,5.08326902931617,
7.74651021643174));
#128689=CARTESIAN_POINT('Ctrl Pts',(-22.0546640218099,5.1091795875243,7.89229140760168));
#128690=CARTESIAN_POINT('Ctrl Pts',(-22.0477306104145,5.13509592276123,
8.03810510220653));
#128691=CARTESIAN_POINT('Ctrl Pts',(-22.0407971990191,5.16736723568734,
8.18277785615113));
#128692=CARTESIAN_POINT('Ctrl Pts',(-22.0338637876236,5.20586520532838,
8.32575314772358));
#128693=CARTESIAN_POINT('Ctrl Pts',(-22.0297447304802,5.22873639063855,
8.41069306582364));
#128694=CARTESIAN_POINT('Ctrl Pts',(-22.0256256733368,5.2538042436447,8.49503408736315));
#128695=CARTESIAN_POINT('Ctrl Pts',(-22.0215066161934,5.28103345893842,
8.57866183845887));
#128696=CARTESIAN_POINT('Ctrl Pts',(-22.0142262297542,5.32916078586583,
8.72647293304141));
#128697=CARTESIAN_POINT('Ctrl Pts',(-22.0069458433151,5.3840610914241,8.87210820405202));
#128698=CARTESIAN_POINT('Ctrl Pts',(-21.9996654568759,5.44550712798327,
9.01494708985037));
#128699=CARTESIAN_POINT('Ctrl Pts',(-21.9923850704367,5.50695316454245,
9.15778597564872));
#128700=CARTESIAN_POINT('Ctrl Pts',(-21.9851046839976,5.57494477387249,
9.29782808536408));
#128701=CARTESIAN_POINT('Ctrl Pts',(-21.9778242975584,5.64919617561881,
9.43447707757441));
#128702=CARTESIAN_POINT('Origin',(-26.8463464956315,10.1295,7.));
#128703=CARTESIAN_POINT('',(-20.35256332674,5.6491961756188,9.4344770775744));
#128704=CARTESIAN_POINT('',(-20.4776000298804,5.6491961756188,9.4344770775744));
#128705=CARTESIAN_POINT('',(-26.8463464956315,5.6491961756188,9.4344770775744));
#128706=CARTESIAN_POINT('',(-21.5963464956315,10.1291161856969,12.0989999855547));
#128707=CARTESIAN_POINT('Ctrl Pts',(-21.5963464956315,10.1291161856969,
12.0989999855547));
#128708=CARTESIAN_POINT('Ctrl Pts',(-21.5886997577445,10.2924291785527,
12.0990122785264));
#128709=CARTESIAN_POINT('Ctrl Pts',(-21.5810530198574,10.4557419617455,
12.0911739196201));
#128710=CARTESIAN_POINT('Ctrl Pts',(-21.5734062819704,10.6183440341081,
12.0755130292727));
#128711=CARTESIAN_POINT('Ctrl Pts',(-21.5666848517297,10.761270142277,12.0617472138972));
#128712=CARTESIAN_POINT('Ctrl Pts',(-21.5599634214889,10.9036700321504,
12.0419345290273));
#128713=CARTESIAN_POINT('Ctrl Pts',(-21.5532419912482,11.0450086188271,
12.0161384519223));
#128714=CARTESIAN_POINT('Ctrl Pts',(-21.5465222109883,11.1863125096208,
11.9903487072541));
#128715=CARTESIAN_POINT('Ctrl Pts',(-21.5398024307283,11.3265552547391,
11.9585785632498));
#128716=CARTESIAN_POINT('Ctrl Pts',(-21.5330826504684,11.4652102525116,
11.9209429097822));
#128717=CARTESIAN_POINT('Ctrl Pts',(-21.5263615518046,11.6038924540449,
11.8832998722942));
#128718=CARTESIAN_POINT('Ctrl Pts',(-21.5196404531407,11.7409859290593,
11.8397891166586));
#128719=CARTESIAN_POINT('Ctrl Pts',(-21.5129193544769,11.8759772620419,
11.7905759750964));
#128720=CARTESIAN_POINT('Ctrl Pts',(-21.5061977698631,12.0109783551886,
11.7413592753181));
#128721=CARTESIAN_POINT('Ctrl Pts',(-21.4994761852493,12.1438766594992,
11.6864394991817));
#128722=CARTESIAN_POINT('Ctrl Pts',(-21.4927546006356,12.2741773917404,
11.6260306835729));
#128723=CARTESIAN_POINT('Ctrl Pts',(-21.4860285543178,12.4045646159827,
11.5655817693456));
#128724=CARTESIAN_POINT('Ctrl Pts',(-21.479302508,12.5323504905475,11.4996366941743));
#128725=CARTESIAN_POINT('Ctrl Pts',(-21.4725764616822,12.6570630553875,
11.4284563903284));
#128726=CARTESIAN_POINT('Ctrl Pts',(-21.4674045201422,12.7529598221028,
11.3737228436212));
#128727=CARTESIAN_POINT('Ctrl Pts',(-21.4622325786022,12.8470398696579,
11.3158948186789));
#128728=CARTESIAN_POINT('Ctrl Pts',(-21.4570606370622,12.9390999696984,
11.255108577965));
#128729=CARTESIAN_POINT('Ctrl Pts',(-21.4497817937609,13.0686627339555,
11.1695597530969));
#128730=CARTESIAN_POINT('Ctrl Pts',(-21.4425029504596,13.1943036068353,
11.0780978347688));
#128731=CARTESIAN_POINT('Ctrl Pts',(-21.4352241071583,13.3155153827349,
10.9810936915597));
#128732=CARTESIAN_POINT('Ctrl Pts',(-21.427946142148,13.4367125327922,10.8841012532143));
#128733=CARTESIAN_POINT('Ctrl Pts',(-21.4206681771377,13.553481456089,10.7815680846603));
#128734=CARTESIAN_POINT('Ctrl Pts',(-21.4133902121274,13.6653475008962,
10.6739057487102));
#128735=CARTESIAN_POINT('Ctrl Pts',(-21.4061165971437,13.7771466835695,
10.5663077623448));
#128736=CARTESIAN_POINT('Ctrl Pts',(-21.39884298216,13.884048659969,10.4535869088841));
#128737=CARTESIAN_POINT('Ctrl Pts',(-21.3915693671764,13.9856148483401,
10.3361923320473));
#128738=CARTESIAN_POINT('Ctrl Pts',(-21.3843006041387,14.0871132858521,
10.2188760645726));
#128739=CARTESIAN_POINT('Ctrl Pts',(-21.377031841101,14.1832828744343,10.0968924881681));
#128740=CARTESIAN_POINT('Ctrl Pts',(-21.3697630780634,14.2737238199281,
9.97072548889001));
#128741=CARTESIAN_POINT('Ctrl Pts',(-21.362503319337,14.3640527300697,9.8447147812575));
#128742=CARTESIAN_POINT('Ctrl Pts',(-21.3552435606107,14.4486670178919,
9.714531202894));
#128743=CARTESIAN_POINT('Ctrl Pts',(-21.3479838018843,14.5272087473904,
9.58068959255577));
#128744=CARTESIAN_POINT('Ctrl Pts',(-21.3455608653075,14.5534219641621,
9.53602010071664));
#128745=CARTESIAN_POINT('Ctrl Pts',(-21.3431379287308,14.5789591128104,
9.49094340429971));
#128746=CARTESIAN_POINT('Ctrl Pts',(-21.340714992154,14.6038079371955,9.44547939740844));
#128747=CARTESIAN_POINT('Ctrl Pts',(-21.3339843753385,14.6728348844358,
9.31918603413387));
#128748=CARTESIAN_POINT('Ctrl Pts',(-21.3272537585231,14.7365235713096,
9.18994468860563));
#128749=CARTESIAN_POINT('Ctrl Pts',(-21.3205231417076,14.7946316255851,
9.05823903275727));
#128750=CARTESIAN_POINT('Ctrl Pts',(-21.3137927443259,14.8527377854031,
8.92653767081916));
#128751=CARTESIAN_POINT('Ctrl Pts',(-21.3070623469442,14.9052635284588,
8.79237249361529));
#128752=CARTESIAN_POINT('Ctrl Pts',(-21.3003319495625,14.9520141566814,
8.65624823278624));
#128753=CARTESIAN_POINT('Ctrl Pts',(-21.2935981100412,14.9987886946641,
8.5200543536752));
#128754=CARTESIAN_POINT('Ctrl Pts',(-21.2868642705199,15.0397820953061,
8.38189973457288));
#128755=CARTESIAN_POINT('Ctrl Pts',(-21.2801304309986,15.0748490349448,
8.24230588929219));
#128756=CARTESIAN_POINT('Ctrl Pts',(-21.2733949256714,15.1099246493845,
8.10267751151975));
#128757=CARTESIAN_POINT('Ctrl Pts',(-21.2666594203442,15.1390707988719,
7.96160955465822));
#128758=CARTESIAN_POINT('Ctrl Pts',(-21.259923915017,15.1621931252001,7.81963461832902));
#128759=CARTESIAN_POINT('Ctrl Pts',(-21.253182158197,15.185336912287,7.67752790936546));
#128760=CARTESIAN_POINT('Ctrl Pts',(-21.2464404013771,15.2024456529539,
7.53451290148192));
#128761=CARTESIAN_POINT('Ctrl Pts',(-21.2396986445571,15.2134767052048,
7.39112895691197));
#128762=CARTESIAN_POINT('Ctrl Pts',(-21.2345888787867,15.2218374477693,
7.28245426104793));
#128763=CARTESIAN_POINT('Ctrl Pts',(-21.2294791130162,15.2267078994303,
7.17356777436155));
#128764=CARTESIAN_POINT('Ctrl Pts',(-21.2243693472458,15.2280894461353,
7.06470440292566));
#128765=CARTESIAN_POINT('Ctrl Pts',(-21.2176534076632,15.229905260131,6.92162155761189));
#128766=CARTESIAN_POINT('Ctrl Pts',(-21.2109374680805,15.2256953339438,
6.77833302577364));
#128767=CARTESIAN_POINT('Ctrl Pts',(-21.2042215284979,15.2154462623456,
6.63537469021888));
#128768=CARTESIAN_POINT('Ctrl Pts',(-21.19751094786,15.2052053689341,6.49253042743137));
#128769=CARTESIAN_POINT('Ctrl Pts',(-21.1908003672221,15.1889349545926,
6.35001620351518));
#128770=CARTESIAN_POINT('Ctrl Pts',(-21.1840897865841,15.1666736682128,
6.20836723396308));
#128771=CARTESIAN_POINT('Ctrl Pts',(-21.1773831930339,15.1444256083638,
6.06680242506643));
#128772=CARTESIAN_POINT('Ctrl Pts',(-21.1706765994837,15.1161938245229,
5.9261022107914));
#128773=CARTESIAN_POINT('Ctrl Pts',(-21.1639700059334,15.0820687172022,
5.7867959358006));
#128774=CARTESIAN_POINT('Ctrl Pts',(-21.1572660310837,15.0479569345949,
5.64754405525195));
#128775=CARTESIAN_POINT('Ctrl Pts',(-21.150562056234,15.0079565014168,5.50968538809937));
#128776=CARTESIAN_POINT('Ctrl Pts',(-21.1438580813843,14.9622087395493,
5.37373826255313));
#128777=CARTESIAN_POINT('Ctrl Pts',(-21.1371540388033,14.9164605154848,
5.23778976351097));
#128778=CARTESIAN_POINT('Ctrl Pts',(-21.1304499962222,14.8649649559917,
5.10375319788511));
#128779=CARTESIAN_POINT('Ctrl Pts',(-21.1237459536412,14.8079130727842,
4.97213113826322));
#128780=CARTESIAN_POINT('Ctrl Pts',(-21.1170415605953,14.7508582070962,
4.84050219788285));
#128781=CARTESIAN_POINT('Ctrl Pts',(-21.1103371675495,14.6882465856708,
4.71128835456374));
#128782=CARTESIAN_POINT('Ctrl Pts',(-21.1036327745036,14.6203170020036,
4.58497129323161));
#128783=CARTESIAN_POINT('Ctrl Pts',(-21.0969267918465,14.5523713122353,
4.45862428213015));
#128784=CARTESIAN_POINT('Ctrl Pts',(-21.0902208091894,14.479105323588,4.33517574698731));
#128785=CARTESIAN_POINT('Ctrl Pts',(-21.0835148265322,14.4008032643884,
4.21508179229178));
#128786=CARTESIAN_POINT('Ctrl Pts',(-21.0768060142702,14.322468165454,4.09493716367445));
#128787=CARTESIAN_POINT('Ctrl Pts',(-21.0700972020082,14.2390929647963,
3.97815024480523));
#128788=CARTESIAN_POINT('Ctrl Pts',(-21.0633883897462,14.1510045080489,
3.86514713395636));
#128789=CARTESIAN_POINT('Ctrl Pts',(-21.0566716293294,14.0628116899532,
3.75201014453292));
#128790=CARTESIAN_POINT('Ctrl Pts',(-21.0499548689125,13.9698946892751,
3.6426662096424));
#128791=CARTESIAN_POINT('Ctrl Pts',(-21.0432381084957,13.8726203565898,
3.53750797891421));
#128792=CARTESIAN_POINT('Ctrl Pts',(-21.0365169651504,13.7752825488948,
3.43228112864843));
#128793=CARTESIAN_POINT('Ctrl Pts',(-21.0297958218052,13.6735820019257,
3.33124568889817));
#128794=CARTESIAN_POINT('Ctrl Pts',(-21.02307467846,13.5679211722343,3.23475620413089));
#128795=CARTESIAN_POINT('Ctrl Pts',(-21.0163436137068,13.4621043714322,
3.13812428652298));
#128796=CARTESIAN_POINT('Ctrl Pts',(-21.0096125489537,13.3523158907957,
3.04605196896882));
#128797=CARTESIAN_POINT('Ctrl Pts',(-21.0028814842005,13.238990562671,2.95885295483325));
#128798=CARTESIAN_POINT('Ctrl Pts',(-20.9991470086101,13.1761163091654,
2.91047389420382));
#128799=CARTESIAN_POINT('Ctrl Pts',(-20.9954125330198,13.112153873401,2.86359414379601));
#128800=CARTESIAN_POINT('Ctrl Pts',(-20.9916780574294,13.0471810287064,
2.81826131678142));
#128801=CARTESIAN_POINT('Ctrl Pts',(-20.9851848243432,12.9342109972609,
2.73943991197113));
#128802=CARTESIAN_POINT('Ctrl Pts',(-20.978691591257,12.8178257484995,2.66504726072126));
#128803=CARTESIAN_POINT('Ctrl Pts',(-20.9721983581708,12.6984140612852,
2.59540222656695));
#128804=CARTESIAN_POINT('Ctrl Pts',(-20.9657135848688,12.5791579509766,
2.52584793025557));
#128805=CARTESIAN_POINT('Ctrl Pts',(-20.9592288115668,12.4568835846724,
2.46102915145827));
#128806=CARTESIAN_POINT('Ctrl Pts',(-20.9527440382649,12.3320115771825,
2.40122366793327));
#128807=CARTESIAN_POINT('Ctrl Pts',(-20.9462660723299,12.2072706536237,
2.34148096499489));
#128808=CARTESIAN_POINT('Ctrl Pts',(-20.9397881063949,12.0799378707497,
2.2867412629917));
#128809=CARTESIAN_POINT('Ctrl Pts',(-20.9333101404599,11.9504610849393,
2.23723801485559));
#128810=CARTESIAN_POINT('Ctrl Pts',(-20.9268373376134,11.8210874951179,
2.1877742219517));
#128811=CARTESIAN_POINT('Ctrl Pts',(-20.9203645347668,11.6895736743514,
2.14353872349908));
#128812=CARTESIAN_POINT('Ctrl Pts',(-20.9138917319203,11.5563897947106,
2.10471793317782));
#128813=CARTESIAN_POINT('Ctrl Pts',(-20.9074218424765,11.4232658610135,
2.06591461605917));
#128814=CARTESIAN_POINT('Ctrl Pts',(-20.9009519530327,11.2884737466312,
2.03252127528892));
#128815=CARTESIAN_POINT('Ctrl Pts',(-20.8944820635889,11.1525008815456,
2.00467516608211));
#128816=CARTESIAN_POINT('Ctrl Pts',(-20.8880136068027,11.0165581255621,
1.97683522296837));
#128817=CARTESIAN_POINT('Ctrl Pts',(-20.8815451500165,10.8794355313552,
1.95454015043084));
#128818=CARTESIAN_POINT('Ctrl Pts',(-20.8750766932303,10.7416323549925,
1.93787643572666));
#128819=CARTESIAN_POINT('Ctrl Pts',(-20.868608190712,10.6038282043591,1.92121260320976));
#128820=CARTESIAN_POINT('Ctrl Pts',(-20.8621396881937,10.4653438603421,
1.91018025615929));
#128821=CARTESIAN_POINT('Ctrl Pts',(-20.8556711856754,10.3266848256182,
1.90481412070709));
#128822=CARTESIAN_POINT('Ctrl Pts',(-20.8492011591068,10.1879931213016,
1.89944672093439));
#128823=CARTESIAN_POINT('Ctrl Pts',(-20.8427311325382,10.0491270452858,
1.89974820296182));
#128824=CARTESIAN_POINT('Ctrl Pts',(-20.8362611059696,9.91059269124868,
1.90570116795498));
#128825=CARTESIAN_POINT('Ctrl Pts',(-20.8297838192034,9.77190288394011,
1.91166081293658));
#128826=CARTESIAN_POINT('Ctrl Pts',(-20.8233065324371,9.6335459434392,1.92328458861965));
#128827=CARTESIAN_POINT('Ctrl Pts',(-20.8168292456708,9.49602388099488,
1.94050308759357));
#128828=CARTESIAN_POINT('Ctrl Pts',(-20.8103483111699,9.35842437192744,
1.95773128329961));
#128829=CARTESIAN_POINT('Ctrl Pts',(-20.803867376669,9.22166107196966,1.98056040833072));
#128830=CARTESIAN_POINT('Ctrl Pts',(-20.7973864421682,9.08622511032575,
2.00887001726311));
#128831=CARTESIAN_POINT('Ctrl Pts',(-20.7908944963577,8.95055903876371,
2.03722772510301));
#128832=CARTESIAN_POINT('Ctrl Pts',(-20.7844025505471,8.81622519909787,
2.07108441947432));
#128833=CARTESIAN_POINT('Ctrl Pts',(-20.7779106047366,8.68369966808103,
2.1102697006662));
#128834=CARTESIAN_POINT('Ctrl Pts',(-20.7716026590288,8.55493028537777,
2.14834436017835));
#128835=CARTESIAN_POINT('Ctrl Pts',(-20.7652947133209,8.42786837597987,
2.19144945063097));
#128836=CARTESIAN_POINT('Ctrl Pts',(-20.758986767613,8.30292988577589,2.23938631919967));
#128837=CARTESIAN_POINT('Ctrl Pts',(-20.7522553481606,8.16960385187237,
2.29054135199688));
#128838=CARTESIAN_POINT('Ctrl Pts',(-20.7455239287083,8.0382566326181,2.34736719785055));
#128839=CARTESIAN_POINT('Ctrl Pts',(-20.7387925092559,7.90939433831116,
2.4096915298711));
#128840=CARTESIAN_POINT('Ctrl Pts',(-20.7320693374223,7.7806899315173,2.47193949949378));
#128841=CARTESIAN_POINT('Ctrl Pts',(-20.7253461655886,7.65446471705759,
2.53967237964706));
#128842=CARTESIAN_POINT('Ctrl Pts',(-20.718622993755,7.53120645650351,2.6126691870997));
#128843=CARTESIAN_POINT('Ctrl Pts',(-20.7119066869372,7.40807405468524,
2.68559145767453));
#128844=CARTESIAN_POINT('Ctrl Pts',(-20.7051903801194,7.28790288938902,
2.76376676295887));
#128845=CARTESIAN_POINT('Ctrl Pts',(-20.6984740733016,7.17115757741741,
2.8469275095722));
#128846=CARTESIAN_POINT('Ctrl Pts',(-20.691763254633,7.05450766246991,2.93002030238408));
#128847=CARTESIAN_POINT('Ctrl Pts',(-20.6850524359643,6.94127832456694,
3.0180902078119));
#128848=CARTESIAN_POINT('Ctrl Pts',(-20.6783416172957,6.83190647329252,
3.11082554613232));
#128849=CARTESIAN_POINT('Ctrl Pts',(-20.6716350376826,6.72260370946926,
3.20350230586892));
#128850=CARTESIAN_POINT('Ctrl Pts',(-20.6649284580695,6.6171538582951,3.30083838763056));
#128851=CARTESIAN_POINT('Ctrl Pts',(-20.6582218784564,6.51596181868043,
3.40248101990474));
#128852=CARTESIAN_POINT('Ctrl Pts',(-20.651517616954,6.41480475581314,3.50408851968543));
#128853=CARTESIAN_POINT('Ctrl Pts',(-20.6448133554515,6.31790283410827,
3.60999934380801));
#128854=CARTESIAN_POINT('Ctrl Pts',(-20.638109093949,6.22562508005278,3.7198229301748));
#128855=CARTESIAN_POINT('Ctrl Pts',(-20.6314059106226,6.13336216605965,
3.82962885476722));
#128856=CARTESIAN_POINT('Ctrl Pts',(-20.6247027272961,6.04572217583957,
3.94334600500746));
#128857=CARTESIAN_POINT('Ctrl Pts',(-20.6179995439696,5.96303463779049,
4.06054981578045));
#128858=CARTESIAN_POINT('Ctrl Pts',(-20.6112961998865,5.88034511671715,
4.17775643735183));
#128859=CARTESIAN_POINT('Ctrl Pts',(-20.6045928558033,5.80260849649827,
4.29844958329638));
#128860=CARTESIAN_POINT('Ctrl Pts',(-20.5978895117201,5.73011159094298,
4.4221748262819));
#128861=CARTESIAN_POINT('Ctrl Pts',(-20.5911822561601,5.65757238262621,
4.54597226434116));
#128862=CARTESIAN_POINT('Ctrl Pts',(-20.5844750006002,5.5902791850645,4.67280501527352));
#128863=CARTESIAN_POINT('Ctrl Pts',(-20.5777677450402,5.52847358717437,
4.80219269532544));
#128864=CARTESIAN_POINT('Ctrl Pts',(-20.5710584023763,5.46664875716989,
4.93162063708084));
#128865=CARTESIAN_POINT('Ctrl Pts',(-20.5643490597123,5.41031508149065,
5.06360475507181));
#128866=CARTESIAN_POINT('Ctrl Pts',(-20.5576397170484,5.35966624389706,
5.19764405869958));
#128867=CARTESIAN_POINT('Ctrl Pts',(-20.550923952482,5.3089689273521,5.33181165914898));
#128868=CARTESIAN_POINT('Ctrl Pts',(-20.5442081879156,5.26396744082792,
5.4680380257195));
#128869=CARTESIAN_POINT('Ctrl Pts',(-20.5374924233492,5.22480597472622,
5.60580578166324));
#128870=CARTESIAN_POINT('Ctrl Pts',(-20.533760108165,5.20304182067926,5.68237080747907));
#128871=CARTESIAN_POINT('Ctrl Pts',(-20.5300277929808,5.18308053177186,
5.75941167581817));
#128872=CARTESIAN_POINT('Ctrl Pts',(-20.5262954777966,5.16494003467883,
5.83683820956401));
#128873=CARTESIAN_POINT('Ctrl Pts',(-20.5195533162237,5.13217051860648,
5.97670372862885));
#128874=CARTESIAN_POINT('Ctrl Pts',(-20.5128111546507,5.10528904643071,
6.11806934857141));
#128875=CARTESIAN_POINT('Ctrl Pts',(-20.5060689930777,5.08442238336994,
6.26041035554957));
#128876=CARTESIAN_POINT('Ctrl Pts',(-20.4993317332857,5.06357089108352,
6.40264787577027));
#128877=CARTESIAN_POINT('Ctrl Pts',(-20.4925944734937,5.04872555025024,
6.54585900974906));
#128878=CARTESIAN_POINT('Ctrl Pts',(-20.4858572137017,5.03996208500972,
6.68950875716634));
#128879=CARTESIAN_POINT('Ctrl Pts',(-20.4791236997967,5.03120349221757,
6.83307863595198));
#128880=CARTESIAN_POINT('Ctrl Pts',(-20.4723901858916,5.02852005962299,
6.9770862778926));
#128881=CARTESIAN_POINT('Ctrl Pts',(-20.4656566719866,5.03193567501757,
7.12099153964812));
#128882=CARTESIAN_POINT('Ctrl Pts',(-20.4589254983211,5.0353501033116,7.26484678698583));
#128883=CARTESIAN_POINT('Ctrl Pts',(-20.4521943246556,5.04485934699362,
7.40859935977437));
#128884=CARTESIAN_POINT('Ctrl Pts',(-20.4454631509901,5.06043518884772,
7.55170910844189));
#128885=CARTESIAN_POINT('Ctrl Pts',(-20.4387320860167,5.07601077918977,
7.69481654623414));
#128886=CARTESIAN_POINT('Ctrl Pts',(-20.4320010210433,5.09765273928883,
7.83728081633733));
#128887=CARTESIAN_POINT('Ctrl Pts',(-20.4252699560699,5.12528095940224,
7.97856670376571));
#128888=CARTESIAN_POINT('Ctrl Pts',(-20.4201632483428,5.14624186910957,
8.08575713142076));
#128889=CARTESIAN_POINT('Ctrl Pts',(-20.4150565406156,5.17064735025746,
8.19226935385378));
#128890=CARTESIAN_POINT('Ctrl Pts',(-20.4099498328884,5.19844276440152,
8.29787346812079));
#128891=CARTESIAN_POINT('Ctrl Pts',(-20.4026901610334,5.23795659533554,
8.44799978375887));
#128892=CARTESIAN_POINT('Ctrl Pts',(-20.3954304891783,5.28430814356502,
8.59623550876125));
#128893=CARTESIAN_POINT('Ctrl Pts',(-20.3881708173233,5.33728986957224,
8.74198825077139));
#128894=CARTESIAN_POINT('Ctrl Pts',(-20.3809013580099,5.39034302531422,
8.88793749600039));
#128895=CARTESIAN_POINT('Ctrl Pts',(-20.3736318986965,5.45004414095369,
9.03139682741447));
#128896=CARTESIAN_POINT('Ctrl Pts',(-20.3663624393832,5.51613698008329,
9.17179249618029));
#128897=CARTESIAN_POINT('Ctrl Pts',(-20.3617627351688,5.55795680430693,
9.26062696398146));
#128898=CARTESIAN_POINT('Ctrl Pts',(-20.3571630309544,5.60233469474515,
9.34823528301885));
#128899=CARTESIAN_POINT('Ctrl Pts',(-20.35256332674,5.6491961756188,9.4344770775744));
#128900=CARTESIAN_POINT('Ctrl Pts',(-21.8525208770954,5.64940737302611,
9.43436256508443));
#128901=CARTESIAN_POINT('Ctrl Pts',(-21.8370464419925,5.80706920978094,
9.7249012359362));
#128902=CARTESIAN_POINT('Ctrl Pts',(-21.7827901252536,6.45799744036311,
10.6901681088921));
#128903=CARTESIAN_POINT('Ctrl Pts',(-21.6973986661372,7.9715431412064,11.8045112188381));
#128904=CARTESIAN_POINT('Ctrl Pts',(-21.6274816421238,9.46413915462446,
12.0984964029847));
#128905=CARTESIAN_POINT('Ctrl Pts',(-21.5963464997463,10.1291160878984,
12.0991317151048));
#128906=CARTESIAN_POINT('',(-21.7216535043236,10.1295436686122,12.098999999813));
#128907=CARTESIAN_POINT('Ctrl Pts',(-21.9778242975584,5.64919617561881,
9.43447707757441));
#128908=CARTESIAN_POINT('Ctrl Pts',(-21.9708911970379,5.71990566836338,
9.56460769727989));
#128909=CARTESIAN_POINT('Ctrl Pts',(-21.9639580965173,5.79629143323561,
9.69166108851864));
#128910=CARTESIAN_POINT('Ctrl Pts',(-21.9570249959968,5.87805954066539,
9.81514742433371));
#128911=CARTESIAN_POINT('Ctrl Pts',(-21.9500922126906,5.95982390690941,
9.93862811020363));
#128912=CARTESIAN_POINT('Ctrl Pts',(-21.9431594293844,6.04696993941788,
10.0585417924252));
#128913=CARTESIAN_POINT('Ctrl Pts',(-21.9362266460782,6.13916035711196,
10.1744275916134));
#128914=CARTESIAN_POINT('Ctrl Pts',(-21.9292923813661,6.2313704741715,10.2903381534262));
#128915=CARTESIAN_POINT('Ctrl Pts',(-21.922358116654,6.32862692396764,10.4022188541319));
#128916=CARTESIAN_POINT('Ctrl Pts',(-21.9154238519419,6.43055173913713,
10.5096414009781));
#128917=CARTESIAN_POINT('Ctrl Pts',(-21.912002891723,6.48083547540742,10.5626373961743));
#128918=CARTESIAN_POINT('Ctrl Pts',(-21.9085819315041,6.53225482388749,
10.6145488689097));
#128919=CARTESIAN_POINT('Ctrl Pts',(-21.9051609712852,6.58476102287579,
10.6653276230177));
#128920=CARTESIAN_POINT('Ctrl Pts',(-21.8982288574645,6.69115774320861,
10.7682239096234));
#128921=CARTESIAN_POINT('Ctrl Pts',(-21.8912967436438,6.80205628720019,
10.8665022681371));
#128922=CARTESIAN_POINT('Ctrl Pts',(-21.8843646298231,6.91703324183498,
10.959780085773));
#128923=CARTESIAN_POINT('Ctrl Pts',(-21.8774338365917,7.03198829300128,
11.0530401336938));
#128924=CARTESIAN_POINT('Ctrl Pts',(-21.8705030433603,7.15101994789284,
11.1413013330035));
#128925=CARTESIAN_POINT('Ctrl Pts',(-21.8635722501289,7.27367163221511,
11.224221269507));
#128926=CARTESIAN_POINT('Ctrl Pts',(-21.8566412042781,7.39632778705101,
11.3071442283473));
#128927=CARTESIAN_POINT('Ctrl Pts',(-21.8497101584272,7.5226039631228,11.3847253467467));
#128928=CARTESIAN_POINT('Ctrl Pts',(-21.8427791125763,7.65201406730425,
11.456665171773));
#128929=CARTESIAN_POINT('Ctrl Pts',(-21.8358484336565,7.78141732048731,
11.5286011882897));
#128930=CARTESIAN_POINT('Ctrl Pts',(-21.8289177547366,7.91395388012152,
11.5948963491392));
#128931=CARTESIAN_POINT('Ctrl Pts',(-21.8219870758168,8.04911248293117,
11.6552968518478));
#128932=CARTESIAN_POINT('Ctrl Pts',(-21.815054830091,8.18430164079941,11.7157110091879));
#128933=CARTESIAN_POINT('Ctrl Pts',(-21.8081225843652,8.32211372406546,
11.7702277106697));
#128934=CARTESIAN_POINT('Ctrl Pts',(-21.8011903386395,8.46201631468178,
11.8186407999764));
#128935=CARTESIAN_POINT('Ctrl Pts',(-21.797065334552,8.54526477138265,11.8474488081138));
#128936=CARTESIAN_POINT('Ctrl Pts',(-21.7929403304645,8.62925305861431,
11.8740965742915));
#128937=CARTESIAN_POINT('Ctrl Pts',(-21.788815326377,8.71386618713863,11.898548959425));
#128938=CARTESIAN_POINT('Ctrl Pts',(-21.7818417513357,8.85690992448683,
11.939887231837));
#128939=CARTESIAN_POINT('Ctrl Pts',(-21.7748681762943,9.00178738562049,
11.9749620552806));
#128940=CARTESIAN_POINT('Ctrl Pts',(-21.7678946012529,9.14793866626696,
12.0036325152953));
#128941=CARTESIAN_POINT('Ctrl Pts',(-21.7609225553009,9.29405790045778,
12.0322966887649));
#128942=CARTESIAN_POINT('Ctrl Pts',(-21.7539505093488,9.44145008039454,
12.0545592393556));
#128943=CARTESIAN_POINT('Ctrl Pts',(-21.7469784633968,9.58954487878361,
12.0703303114365));
#128944=CARTESIAN_POINT('Ctrl Pts',(-21.740007262077,9.73762173614916,12.0860994729225));
#128945=CARTESIAN_POINT('Ctrl Pts',(-21.7330360607571,9.88640072158192,
12.0953786905622));
#128946=CARTESIAN_POINT('Ctrl Pts',(-21.7260648594373,10.0353056921974,
12.0981298955968));
#128947=CARTESIAN_POINT('Ctrl Pts',(-21.7245944077477,10.0667145635801,
12.0987102136662));
#128948=CARTESIAN_POINT('Ctrl Pts',(-21.723123956058,10.0981290288572,12.0990002688469));
#128949=CARTESIAN_POINT('Ctrl Pts',(-21.7216535043684,10.1295436676547,
12.098999999813));
#128950=CARTESIAN_POINT('Ctrl Pts',(-21.7216535043236,10.1295436686122,
12.098999999813));
#128951=CARTESIAN_POINT('Ctrl Pts',(-21.7145780772905,10.2807026533976,
12.0989987052645));
#128952=CARTESIAN_POINT('Ctrl Pts',(-21.7075026502575,10.4318398568485,
12.0922714484638));
#128953=CARTESIAN_POINT('Ctrl Pts',(-21.7004272232244,10.582361479932,12.0788500155049));
#128954=CARTESIAN_POINT('Ctrl Pts',(-21.693349719895,10.7329272738466,12.0654246440032));
#128955=CARTESIAN_POINT('Ctrl Pts',(-21.6862722165656,10.8828768275428,
12.0453011997449));
#128956=CARTESIAN_POINT('Ctrl Pts',(-21.6791947132363,11.0316213327613,
12.0185633503003));
#128957=CARTESIAN_POINT('Ctrl Pts',(-21.6769530359805,11.0787335923755,
12.0100945971002));
#128958=CARTESIAN_POINT('Ctrl Pts',(-21.6747113587247,11.1257250216099,
12.0009626767532));
#128959=CARTESIAN_POINT('Ctrl Pts',(-21.6724696814689,11.1725771008058,
11.9911713216213));
#128960=CARTESIAN_POINT('Ctrl Pts',(-21.665538500834,11.3174419439415,11.9608968247447));
#128961=CARTESIAN_POINT('Ctrl Pts',(-21.6586073201992,11.4610130681156,
11.9243059246399));
#128962=CARTESIAN_POINT('Ctrl Pts',(-21.6516761395644,11.6027362745548,
11.88153417271));
#128963=CARTESIAN_POINT('Ctrl Pts',(-21.6447462728878,11.7444326142333,
11.8387705291094));
#128964=CARTESIAN_POINT('Ctrl Pts',(-21.6378164062113,11.884281418354,11.7898284670043));
#128965=CARTESIAN_POINT('Ctrl Pts',(-21.6308865395347,12.0217431373186,
11.7348935478288));
#128966=CARTESIAN_POINT('Ctrl Pts',(-21.6239564014542,12.1592102398846,
11.6799564771618));
#128967=CARTESIAN_POINT('Ctrl Pts',(-21.6170262633738,12.2942897616118,
11.6190261995686));
#128968=CARTESIAN_POINT('Ctrl Pts',(-21.6100961252933,12.426461132908,11.5523368234249));
#128969=CARTESIAN_POINT('Ctrl Pts',(-21.6031663413856,12.5586257494336,
11.4856508555187));
#128970=CARTESIAN_POINT('Ctrl Pts',(-21.5962365574778,12.6878822178597,
11.4132065281025));
#128971=CARTESIAN_POINT('Ctrl Pts',(-21.5893067735701,12.8137336190688,
11.3352844056949));
#128972=CARTESIAN_POINT('Ctrl Pts',(-21.5823753954677,12.9396139723548,
11.2573443573264));
#128973=CARTESIAN_POINT('Ctrl Pts',(-21.5754440173652,13.0620874116896,
11.1739241703709));
#128974=CARTESIAN_POINT('Ctrl Pts',(-21.5685126392628,13.1806845732687,
11.0853486631923));
#128975=CARTESIAN_POINT('Ctrl Pts',(-21.5643831050287,13.2513416679423,
11.0325776869467));
#128976=CARTESIAN_POINT('Ctrl Pts',(-21.5602535707947,13.3206234444385,
10.9779776769825));
#128977=CARTESIAN_POINT('Ctrl Pts',(-21.5561240365606,13.3884359580966,
10.9216243345105));
#128978=CARTESIAN_POINT('Ctrl Pts',(-21.5491919873467,13.5022695420679,
10.8270267064872));
#128979=CARTESIAN_POINT('Ctrl Pts',(-21.5422599381329,13.6120015769791,
10.7274526569437));
#128980=CARTESIAN_POINT('Ctrl Pts',(-21.535327888919,13.7172057131023,10.6232814845348));
#128981=CARTESIAN_POINT('Ctrl Pts',(-21.5283971834842,13.8223894553827,
10.5191305057286));
#128982=CARTESIAN_POINT('Ctrl Pts',(-21.5214664780495,13.9230468150587,
10.4103844146959));
#128983=CARTESIAN_POINT('Ctrl Pts',(-21.5145357726147,14.0187877971565,
10.2974598452277));
#128984=CARTESIAN_POINT('Ctrl Pts',(-21.5076048482097,14.1145318041177,
10.1845317079939));
#128985=CARTESIAN_POINT('Ctrl Pts',(-21.5006739238046,14.2053589060595,
10.06742507829));
#128986=CARTESIAN_POINT('Ctrl Pts',(-21.4937429993995,14.2909186070078,
9.94659060224677));
#128987=CARTESIAN_POINT('Ctrl Pts',(-21.4868124606186,14.3764735475678,
9.82576284921712));
#128988=CARTESIAN_POINT('Ctrl Pts',(-21.4798819218377,14.4567614830456,
9.70120793542299));
#128989=CARTESIAN_POINT('Ctrl Pts',(-21.4729513830568,14.5314745604009,
9.57340649132294));
#128990=CARTESIAN_POINT('Ctrl Pts',(-21.4660193048808,14.6062042328509,
9.44557666026405));
#128991=CARTESIAN_POINT('Ctrl Pts',(-21.4590872267048,14.6753564058714,
9.31449914377409));
#128992=CARTESIAN_POINT('Ctrl Pts',(-21.4521551485288,14.7386682911608,
9.18068077988451));
#128993=CARTESIAN_POINT('Ctrl Pts',(-21.4480295629033,14.7763479879615,
9.10103956631653));
#128994=CARTESIAN_POINT('Ctrl Pts',(-21.4439039772779,14.8119599512988,
9.020428027734));
#128995=CARTESIAN_POINT('Ctrl Pts',(-21.4397783916524,14.8454567318764,
8.93895670479501));
#128996=CARTESIAN_POINT('Ctrl Pts',(-21.4328287564197,14.9018827590196,
8.80171655812195));
#128997=CARTESIAN_POINT('Ctrl Pts',(-21.425879121187,14.9523225305843,8.661990870534));
#128998=CARTESIAN_POINT('Ctrl Pts',(-21.4189294859543,14.9965767489365,
8.52031737474841));
#128999=CARTESIAN_POINT('Ctrl Pts',(-21.4119810766083,15.0408231610291,
8.37866886957668));
#129000=CARTESIAN_POINT('Ctrl Pts',(-21.4050326672623,15.0788860995113,
8.23507355414718));
#129001=CARTESIAN_POINT('Ctrl Pts',(-21.3980842579163,15.110615897284,8.09008505072978));
#129002=CARTESIAN_POINT('Ctrl Pts',(-21.3911356289697,15.1423466978592,
7.94509196503175));
#129003=CARTESIAN_POINT('Ctrl Pts',(-21.3841870000231,15.1677438841323,
7.79870592238976));
#129004=CARTESIAN_POINT('Ctrl Pts',(-21.3772383710765,15.1867086284737,
7.65149204760402));
#129005=CARTESIAN_POINT('Ctrl Pts',(-21.3702901717336,15.2056722003069,
7.50428727441542));
#129006=CARTESIAN_POINT('Ctrl Pts',(-21.3633419723906,15.2182040846995,
7.35625509628934));
#129007=CARTESIAN_POINT('Ctrl Pts',(-21.3563937730477,15.2242571742947,
7.20796714878315));
#129008=CARTESIAN_POINT('Ctrl Pts',(-21.349444258653,15.2303114095286,7.05965113554095));
#129009=CARTESIAN_POINT('Ctrl Pts',(-21.3424947442583,15.2298843862783,
6.91107958341258));
#129010=CARTESIAN_POINT('Ctrl Pts',(-21.3355452298636,15.2229810863828,
6.76282617627361));
#129011=CARTESIAN_POINT('Ctrl Pts',(-21.3315077354905,15.2189704414799,
6.67669464777756));
#129012=CARTESIAN_POINT('Ctrl Pts',(-21.3274702411173,15.2127748193448,
6.59067051003166));
#129013=CARTESIAN_POINT('Ctrl Pts',(-21.3234327467442,15.204403268655,6.50486586282613));
#129014=CARTESIAN_POINT('Ctrl Pts',(-21.3165507415352,15.190133761349,6.35860980041301));
#129015=CARTESIAN_POINT('Ctrl Pts',(-21.3096687363261,15.1695340759322,
6.21293699097909));
#129016=CARTESIAN_POINT('Ctrl Pts',(-21.3027867311171,15.1426759370888,
6.06840565491517));
#129017=CARTESIAN_POINT('Ctrl Pts',(-21.2959062311046,15.1158236725187,
5.92390592999826));
#129018=CARTESIAN_POINT('Ctrl Pts',(-21.2890257310922,15.0827157467963,
5.78054751496051));
#129019=CARTESIAN_POINT('Ctrl Pts',(-21.2821452310798,15.0434752182249,
5.6388796692902));
#129020=CARTESIAN_POINT('Ctrl Pts',(-21.2752642995611,15.0042322287083,
5.49720293900931));
#129021=CARTESIAN_POINT('Ctrl Pts',(-21.2683833680424,14.9588559542225,
5.35721731924814));
#129022=CARTESIAN_POINT('Ctrl Pts',(-21.2615024365237,14.9075198065232,
5.21945858557805));
#129023=CARTESIAN_POINT('Ctrl Pts',(-21.2546216674167,14.8561848705187,
5.0817031034479));
#129024=CARTESIAN_POINT('Ctrl Pts',(-21.2477408983096,14.7988904640696,
4.94617472034536));
#129025=CARTESIAN_POINT('Ctrl Pts',(-21.2408601292026,14.7358587467216,
4.81339073071985));
#129026=CARTESIAN_POINT('Ctrl Pts',(-21.2339770585297,14.6728059457358,
4.68056232584361));
#129027=CARTESIAN_POINT('Ctrl Pts',(-21.2270939878569,14.6040121460501,
4.5504804560362));
#129028=CARTESIAN_POINT('Ctrl Pts',(-21.2202109171841,14.5297464825698,
4.42363979757638));
#129029=CARTESIAN_POINT('Ctrl Pts',(-21.2158363120681,14.4825461897283,
4.3430249354323));
#129030=CARTESIAN_POINT('Ctrl Pts',(-21.2114617069521,14.4331365440049,
4.26371883720866));
#129031=CARTESIAN_POINT('Ctrl Pts',(-21.2070871018361,14.3815959889042,
4.1858428080249));
#129032=CARTESIAN_POINT('Ctrl Pts',(-21.2000237327386,14.2983770572496,
4.0601018272089));
#129033=CARTESIAN_POINT('Ctrl Pts',(-21.1929603636411,14.2095738290717,
3.93804985679066));
#129034=CARTESIAN_POINT('Ctrl Pts',(-21.1858969945437,14.1155331325974,
3.82016653488964));
#129035=CARTESIAN_POINT('Ctrl Pts',(-21.178834458356,14.0215035253657,3.70229711374445));
#129036=CARTESIAN_POINT('Ctrl Pts',(-21.1717719221683,13.9222378725607,
3.58859559695674));
#129037=CARTESIAN_POINT('Ctrl Pts',(-21.1647093859805,13.8181238245223,
3.47950922722885));
#129038=CARTESIAN_POINT('Ctrl Pts',(-21.1576473847886,13.7140176632508,
3.37043112092746));
#129039=CARTESIAN_POINT('Ctrl Pts',(-21.1505853835967,13.6050640485619,
3.26596768458527));
#129040=CARTESIAN_POINT('Ctrl Pts',(-21.1435233824048,13.4916885213516,
3.16653037746596));
#129041=CARTESIAN_POINT('Ctrl Pts',(-21.1364626336035,13.3783331004038,
3.06711070477482));
#129042=CARTESIAN_POINT('Ctrl Pts',(-21.1294018848022,13.2605575614681,
2.97271558142976));
#129043=CARTESIAN_POINT('Ctrl Pts',(-21.1223411360009,13.1388219318202,
2.88371739178833));
#129044=CARTESIAN_POINT('Ctrl Pts',(-21.1152814326218,13.0171043264813,
2.79473237931509));
#129045=CARTESIAN_POINT('Ctrl Pts',(-21.1082217292426,12.8914280458127,
2.71114288504483));
#129046=CARTESIAN_POINT('Ctrl Pts',(-21.1011620258634,12.7622840994283,
2.63327939000014));
#129047=CARTESIAN_POINT('Ctrl Pts',(-21.0976885028849,12.6987425536711,
2.59496890800147));
#129048=CARTESIAN_POINT('Ctrl Pts',(-21.0942149799064,12.6343619930903,
2.55804394760152));
#129049=CARTESIAN_POINT('Ctrl Pts',(-21.0907414569279,12.5692033929549,
2.52253996618568));
#129050=CARTESIAN_POINT('Ctrl Pts',(-21.0840199577374,12.4431171454252,
2.4538373884787));
#129051=CARTESIAN_POINT('Ctrl Pts',(-21.0772984585468,12.3140777046371,
2.39043779766263));
#129052=CARTESIAN_POINT('Ctrl Pts',(-21.0705769593563,12.1825638082227,
2.33258851188734));
#129053=CARTESIAN_POINT('Ctrl Pts',(-21.0638571099993,12.0510821927081,
2.27475342557727));
#129054=CARTESIAN_POINT('Ctrl Pts',(-21.0571372606424,11.917127668362,2.2224660775447));
#129055=CARTESIAN_POINT('Ctrl Pts',(-21.0504174112854,11.7812007609424,
2.17592645202188));
#129056=CARTESIAN_POINT('Ctrl Pts',(-21.0436962436786,11.6452471883979,
2.12937769670309));
#129057=CARTESIAN_POINT('Ctrl Pts',(-21.0369750760718,11.5073208059466,
2.08857904163403));
#129058=CARTESIAN_POINT('Ctrl Pts',(-21.030253908465,11.3679394888552,2.05368130500632));
#129059=CARTESIAN_POINT('Ctrl Pts',(-21.0235322550113,11.2285480964327,
2.01878104575749));
#129060=CARTESIAN_POINT('Ctrl Pts',(-21.0168106015575,11.0877019181293,
1.98978263908414));
#129061=CARTESIAN_POINT('Ctrl Pts',(-21.0100889481037,10.9459306945815,
1.96678612406097));
#129062=CARTESIAN_POINT('Ctrl Pts',(-21.00336283355,10.8040653787673,1.94377434646079));
#129063=CARTESIAN_POINT('Ctrl Pts',(-20.9966367189962,10.6612741552295,
1.92677247459323));
#129064=CARTESIAN_POINT('Ctrl Pts',(-20.9899106044424,10.5180941451528,
1.91582891806806));
#129065=CARTESIAN_POINT('Ctrl Pts',(-20.9847390069682,10.4080054197001,
1.90741459969269));
#129066=CARTESIAN_POINT('Ctrl Pts',(-20.9795674094939,10.2976870254571,
1.90258079609333));
#129067=CARTESIAN_POINT('Ctrl Pts',(-20.9743958120197,10.1873835904047,
1.90132855638237));
#129068=CARTESIAN_POINT('Ctrl Pts',(-20.9671170684873,10.0321374757399,
1.89956609676666));
#129069=CARTESIAN_POINT('Ctrl Pts',(-20.959838324955,9.87682543926592,1.90489862489669));
#129070=CARTESIAN_POINT('Ctrl Pts',(-20.9525595814226,9.7220753784726,1.91730325734721));
#129071=CARTESIAN_POINT('Ctrl Pts',(-20.9452817167969,9.56734400371569,
1.92970639194104));
#129072=CARTESIAN_POINT('Ctrl Pts',(-20.9380038521713,9.41317472155407,
1.94917990409636));
#129073=CARTESIAN_POINT('Ctrl Pts',(-20.9307259875456,9.26019127590926,
1.97564896307795));
#129074=CARTESIAN_POINT('Ctrl Pts',(-20.9234524716548,9.10729924230271,
2.00210220603041));
#129075=CARTESIAN_POINT('Ctrl Pts',(-20.9161789557639,8.95559187901386,
2.03554260156708));
#129076=CARTESIAN_POINT('Ctrl Pts',(-20.9089054398731,8.80568411965762,
2.07584397942619));
#129077=CARTESIAN_POINT('Ctrl Pts',(-20.9016367742746,8.65587632522299,
2.11611848259851));
#129078=CARTESIAN_POINT('Ctrl Pts',(-20.894368108676,8.50786598368629,2.16324476993341));
#129079=CARTESIAN_POINT('Ctrl Pts',(-20.8870994430774,8.36225537649466,
2.21704615946469));
#129080=CARTESIAN_POINT('Ctrl Pts',(-20.8798397779555,8.21682507266881,
2.27078092904428));
#129081=CARTESIAN_POINT('Ctrl Pts',(-20.8725801128336,8.07378880792323,
2.33117421095855));
#129082=CARTESIAN_POINT('Ctrl Pts',(-20.8653204477117,7.93373154482647,
2.39800022911074));
#129083=CARTESIAN_POINT('Ctrl Pts',(-20.862897020845,7.88697752400415,2.42030814071116));
#129084=CARTESIAN_POINT('Ctrl Pts',(-20.8604735939782,7.84055533141693,
2.44333248635513));
#129085=CARTESIAN_POINT('Ctrl Pts',(-20.8580501671115,7.79448628016983,
2.46706365275169));
#129086=CARTESIAN_POINT('Ctrl Pts',(-20.8513195102469,7.6665373082926,2.53297294021673));
#129087=CARTESIAN_POINT('Ctrl Pts',(-20.8445888533824,7.54135727855362,
2.6043155917558));
#129088=CARTESIAN_POINT('Ctrl Pts',(-20.8378581965178,7.41941799831926,
2.68082686800284));
#129089=CARTESIAN_POINT('Ctrl Pts',(-20.8311277589209,7.29748269055658,
2.75733565170707));
#129090=CARTESIAN_POINT('Ctrl Pts',(-20.824397321324,7.17878823114962,2.83901252941112));
#129091=CARTESIAN_POINT('Ctrl Pts',(-20.8176668837272,7.06377874695439,
2.92554860151401));
#129092=CARTESIAN_POINT('Ctrl Pts',(-20.8109330039709,6.94871044325873,
3.01212893091069));
#129093=CARTESIAN_POINT('Ctrl Pts',(-20.8041991242146,6.83733117429048,
3.10357320184736));
#129094=CARTESIAN_POINT('Ctrl Pts',(-20.7974652444583,6.73005358099377,
3.19953094417206));
#129095=CARTESIAN_POINT('Ctrl Pts',(-20.7907296988947,6.62274944968287,
3.29551242423964));
#129096=CARTESIAN_POINT('Ctrl Pts',(-20.7839941533312,6.51954928410615,
3.3960093515451));
#129097=CARTESIAN_POINT('Ctrl Pts',(-20.7772586077676,6.42082972916417,
3.50063351130258));
#129098=CARTESIAN_POINT('Ctrl Pts',(-20.7705168109826,6.32201855316575,
3.60535477214659));
#129099=CARTESIAN_POINT('Ctrl Pts',(-20.7637750141976,6.22769654299804,
3.7142106479578));
#129100=CARTESIAN_POINT('Ctrl Pts',(-20.7570332174125,6.13820130284807,
3.82677833895687));
#129101=CARTESIAN_POINT('Ctrl Pts',(-20.7519236523428,6.07037342734832,
3.91209267877634));
#129102=CARTESIAN_POINT('Ctrl Pts',(-20.746814087273,6.00531726134624,3.99953837678175));
#129103=CARTESIAN_POINT('Ctrl Pts',(-20.7417045222033,5.9431632940884,4.08892013425649));
#129104=CARTESIAN_POINT('Ctrl Pts',(-20.7349885840485,5.86146902178138,
4.20640221877302));
#129105=CARTESIAN_POINT('Ctrl Pts',(-20.7282726458937,5.7846499298272,4.32743176090146));
#129106=CARTESIAN_POINT('Ctrl Pts',(-20.7215567077389,5.7130174542218,4.45157246074438));
#129107=CARTESIAN_POINT('Ctrl Pts',(-20.7148461284493,5.64144213649507,
4.5756141046912));
#129108=CARTESIAN_POINT('Ctrl Pts',(-20.7081355491596,5.57504537611946,
4.70276164277715));
#129109=CARTESIAN_POINT('Ctrl Pts',(-20.70142496987,5.51409512437855,4.83255015419278));
#129110=CARTESIAN_POINT('Ctrl Pts',(-20.6947183775871,5.45318108546702,
4.96226155338845));
#129111=CARTESIAN_POINT('Ctrl Pts',(-20.6880117853042,5.39770726562995,
5.09461046626503));
#129112=CARTESIAN_POINT('Ctrl Pts',(-20.6813051930213,5.34789546567042,
5.22910783013794));
#129113=CARTESIAN_POINT('Ctrl Pts',(-20.6746012193564,5.2981031149441,5.36355267893212));
#129114=CARTESIAN_POINT('Ctrl Pts',(-20.6678972456915,5.25396850735589,
5.50014396102872));
#129115=CARTESIAN_POINT('Ctrl Pts',(-20.6611932720266,5.2156650969859,5.63837319873601));
#129116=CARTESIAN_POINT('Ctrl Pts',(-20.6544892305015,5.17736129889393,
5.77660383565325));
#129117=CARTESIAN_POINT('Ctrl Pts',(-20.6477851889764,5.14488892341421,
5.91647210752774));
#129118=CARTESIAN_POINT('Ctrl Pts',(-20.6410811474513,5.11837144179926,
6.05745473679778));
#129119=CARTESIAN_POINT('Ctrl Pts',(-20.6343767553807,5.0918525736203,6.1984447378628));
#129120=CARTESIAN_POINT('Ctrl Pts',(-20.6276723633102,5.07128928850254,
6.34054884896834));
#129121=CARTESIAN_POINT('Ctrl Pts',(-20.6209679712396,5.05675377886092,
6.48323431236274));
#129122=CARTESIAN_POINT('Ctrl Pts',(-20.6142619894755,5.04221482267187,
6.62595360822882));
#129123=CARTESIAN_POINT('Ctrl Pts',(-20.6075560077115,5.03370652666762,
6.76925416302977));
#129124=CARTESIAN_POINT('Ctrl Pts',(-20.6008500259474,5.03124911809654,
6.91259894067805));
#129125=CARTESIAN_POINT('Ctrl Pts',(-20.5941412144946,5.02879067258536,
7.05600420478712));
#129126=CARTESIAN_POINT('Ctrl Pts',(-20.5874324030418,5.03238820704158,
7.19945335934839));
#129127=CARTESIAN_POINT('Ctrl Pts',(-20.580723591589,5.04200983657999,7.34241033440097));
#129128=CARTESIAN_POINT('Ctrl Pts',(-20.5740068318481,5.05164286537795,
7.48553667823434));
#129129=CARTESIAN_POINT('Ctrl Pts',(-20.5672900721073,5.06731422089046,
7.62816930839523));
#129130=CARTESIAN_POINT('Ctrl Pts',(-20.5605733123664,5.088940140337,7.76977743611652));
#129131=CARTESIAN_POINT('Ctrl Pts',(-20.5538521696223,5.11058017171842,
7.91147796983615));
#129132=CARTESIAN_POINT('Ctrl Pts',(-20.5471310268781,5.1381824435197,8.05215230563782));
#129133=CARTESIAN_POINT('Ctrl Pts',(-20.540409884134,5.17161234851655,8.19128125783457));
#129134=CARTESIAN_POINT('Ctrl Pts',(-20.5336788198585,5.20509160164702,
8.33061558764527));
#129135=CARTESIAN_POINT('Ctrl Pts',(-20.526947755583,5.24441557450116,8.46839962056655));
#129136=CARTESIAN_POINT('Ctrl Pts',(-20.5202166913075,5.28939995726619,
8.60412985020796));
#129137=CARTESIAN_POINT('Ctrl Pts',(-20.5164822050006,5.31435790664587,
8.67943483368136));
#129138=CARTESIAN_POINT('Ctrl Pts',(-20.5127477186938,5.34105737182238,
8.7541079689008));
#129139=CARTESIAN_POINT('Ctrl Pts',(-20.5090132323869,5.36946062600318,
8.82806623457683));
#129140=CARTESIAN_POINT('Ctrl Pts',(-20.502520363616,5.41884321490794,8.95665187503696));
#129141=CARTESIAN_POINT('Ctrl Pts',(-20.4960274948451,5.47353574030531,
9.08348391875456));
#129142=CARTESIAN_POINT('Ctrl Pts',(-20.4895346260742,5.53339495200478,
9.20808047584159));
#129143=CARTESIAN_POINT('Ctrl Pts',(-20.4855564273429,5.57007085728481,
9.28442113246241));
#129144=CARTESIAN_POINT('Ctrl Pts',(-20.4815782286116,5.60868536043436,
9.35992276697046));
#129145=CARTESIAN_POINT('Ctrl Pts',(-20.4776000298804,5.6491961756188,9.4344770775744));
#129146=CARTESIAN_POINT('Origin',(-26.8463464956315,10.1295,7.));
#129147=CARTESIAN_POINT('',(-18.8525174996886,5.6491961756188,9.4344770775744));
#129148=CARTESIAN_POINT('',(-18.977821433234,5.64904402747702,9.43455986027809));
#129149=CARTESIAN_POINT('',(-26.8463464956315,5.6491961756188,9.4344770775744));
#129150=CARTESIAN_POINT('',(-20.0963464956032,10.1297172757599,12.0989999953708));
#129151=CARTESIAN_POINT('Ctrl Pts',(-20.0963464956032,10.1297172757598,
12.0989999953708));
#129152=CARTESIAN_POINT('Ctrl Pts',(-20.089015871315,10.2862367018524,12.0989933258518));
#129153=CARTESIAN_POINT('Ctrl Pts',(-20.0816852470269,10.4427270477282,
12.0917755131971));
#129154=CARTESIAN_POINT('Ctrl Pts',(-20.0743546227387,10.5985501666255,
12.0773805196369));
#129155=CARTESIAN_POINT('Ctrl Pts',(-20.0698740478804,10.6937913250079,
12.06858210852));
#129156=CARTESIAN_POINT('Ctrl Pts',(-20.0653934730221,10.7887832630484,
12.0571034512937));
#129157=CARTESIAN_POINT('Ctrl Pts',(-20.0609128981638,10.883381113265,12.0429618546111));
#129158=CARTESIAN_POINT('Ctrl Pts',(-20.0540299000486,11.0287010432615,
12.0212377262588));
#129159=CARTESIAN_POINT('Ctrl Pts',(-20.0471469019333,11.1731216585732,
11.9932218786075));
#129160=CARTESIAN_POINT('Ctrl Pts',(-20.040263903818,11.3160889030018,11.959012782326));
#129161=CARTESIAN_POINT('Ctrl Pts',(-20.0333828335523,11.4590161039285,
11.924813267624));
#129162=CARTESIAN_POINT('Ctrl Pts',(-20.0265017632867,11.6004904149984,
11.8844240428383));
#129163=CARTESIAN_POINT('Ctrl Pts',(-20.019620693021,11.7399691658932,11.837994425969));
#129164=CARTESIAN_POINT('Ctrl Pts',(-20.0127398324751,11.8794436657853,
11.7915662241714));
#129165=CARTESIAN_POINT('Ctrl Pts',(-20.0058589719292,12.0169224023365,
11.7390981002918));
#129166=CARTESIAN_POINT('Ctrl Pts',(-19.9989781113832,12.1518786132926,
11.6807890087566));
#129167=CARTESIAN_POINT('Ctrl Pts',(-19.9920977747547,12.2868245485124,
11.6224843569492));
#129168=CARTESIAN_POINT('Ctrl Pts',(-19.9852174381262,12.419248029891,11.5583397622004));
#129169=CARTESIAN_POINT('Ctrl Pts',(-19.9783371014977,12.5486430535138,
11.4886019969068));
#129170=CARTESIAN_POINT('Ctrl Pts',(-19.9714550222469,12.6780708497566,
11.4188465687294));
#129171=CARTESIAN_POINT('Ctrl Pts',(-19.964572942996,12.8044683557619,11.3434953008952));
#129172=CARTESIAN_POINT('Ctrl Pts',(-19.9576908637452,12.9273544175526,
11.2628407967201));
#129173=CARTESIAN_POINT('Ctrl Pts',(-19.9533163269153,13.0054659276911,
11.2115734273474));
#129174=CARTESIAN_POINT('Ctrl Pts',(-19.9489417900855,13.0821591944104,
11.1581642466885));
#129175=CARTESIAN_POINT('Ctrl Pts',(-19.9445672532557,13.1573167585015,
11.1026974878654));
#129176=CARTESIAN_POINT('Ctrl Pts',(-19.9376178346047,13.2767125706703,
11.014582621476));
#129177=CARTESIAN_POINT('Ctrl Pts',(-19.9306684159537,13.392276360347,10.9212397631479));
#129178=CARTESIAN_POINT('Ctrl Pts',(-19.9237189973027,13.5035591632226,
10.8230257340323));
#129179=CARTESIAN_POINT('Ctrl Pts',(-19.9167707096019,13.6148238559054,
10.724827688294));
#129180=CARTESIAN_POINT('Ctrl Pts',(-19.9098224219011,13.7218087066573,
10.6217602701984));
#129181=CARTESIAN_POINT('Ctrl Pts',(-19.9028741342004,13.8240989854157,
10.5142195914549));
#129182=CARTESIAN_POINT('Ctrl Pts',(-19.8959254836163,13.9263946064161,
10.4066732962605));
#129183=CARTESIAN_POINT('Ctrl Pts',(-19.8889768330322,14.0239949372702,
10.2946535083665));
#129184=CARTESIAN_POINT('Ctrl Pts',(-19.8820281824482,14.116522779692,10.1785925115084));
#129185=CARTESIAN_POINT('Ctrl Pts',(-19.8750798802786,14.209045982645,10.0625373341027));
#129186=CARTESIAN_POINT('Ctrl Pts',(-19.8681315781091,14.2964970028861,
9.9424416099158));
#129187=CARTESIAN_POINT('Ctrl Pts',(-19.8611832759396,14.3785395224088,
9.81876996879985));
#129188=CARTESIAN_POINT('Ctrl Pts',(-19.8542335347365,14.4605990334123,
9.69507271457101));
#129189=CARTESIAN_POINT('Ctrl Pts',(-19.8472837935334,14.5372476244609,
9.56779833651679));
#129190=CARTESIAN_POINT('Ctrl Pts',(-19.8403340523302,14.6081924776181,
9.43744019227688));
#129191=CARTESIAN_POINT('Ctrl Pts',(-19.8362965710027,14.6494081878925,
9.36170808112577));
#129192=CARTESIAN_POINT('Ctrl Pts',(-19.8322590896751,14.6886996717564,
9.28493568412992));
#129193=CARTESIAN_POINT('Ctrl Pts',(-19.8282216083475,14.7260166271649,
9.20722357186493));
#129194=CARTESIAN_POINT('Ctrl Pts',(-19.8212896270348,14.7900863816857,
9.07379907617413));
#129195=CARTESIAN_POINT('Ctrl Pts',(-19.8143576457221,14.8483539160099,
8.93755987242083));
#129196=CARTESIAN_POINT('Ctrl Pts',(-19.8074256644093,14.9005897744139,
8.79902845015939));
#129197=CARTESIAN_POINT('Ctrl Pts',(-19.800494999141,14.9528157157817,8.66052332824371));
#129198=CARTESIAN_POINT('Ctrl Pts',(-19.7935643338727,14.9990121492195,
8.51972716550497));
#129199=CARTESIAN_POINT('Ctrl Pts',(-19.7866336686044,15.0389982277045,
8.37718123432116));
#129200=CARTESIAN_POINT('Ctrl Pts',(-19.7797027424108,15.0789858115835,
8.23462993657493));
#129201=CARTESIAN_POINT('Ctrl Pts',(-19.7727718162171,15.1127624801018,
8.09032905625727));
#129202=CARTESIAN_POINT('Ctrl Pts',(-19.7658408900234,15.1401974670158,
7.94483432094795));
#129203=CARTESIAN_POINT('Ctrl Pts',(-19.7589103257021,15.1676310215149,
7.79934718210023));
#129204=CARTESIAN_POINT('Ctrl Pts',(-19.7519797613807,15.1887234966507,
7.65266663834769));
#129205=CARTESIAN_POINT('Ctrl Pts',(-19.7450491970594,15.2033953868547,
7.50535789620315));
#129206=CARTESIAN_POINT('Ctrl Pts',(-19.7381170569175,15.2180706130446,
7.35801566008556));
#129207=CARTESIAN_POINT('Ctrl Pts',(-19.7311849167757,15.2263223045308,
7.21004526955849));
#129208=CARTESIAN_POINT('Ctrl Pts',(-19.7242527766338,15.228122843019,7.06201697061806));
#129209=CARTESIAN_POINT('Ctrl Pts',(-19.7201271722356,15.2291944182259,
6.97391918426839));
#129210=CARTESIAN_POINT('Ctrl Pts',(-19.7160015678375,15.2279820313568,
6.88580095229293));
#129211=CARTESIAN_POINT('Ctrl Pts',(-19.7118759634393,15.2244886255794,
6.79778252989406));
#129212=CARTESIAN_POINT('Ctrl Pts',(-19.7049446779354,15.2186194751504,
6.64990581745022));
#129213=CARTESIAN_POINT('Ctrl Pts',(-19.6980133924316,15.2063069875029,
6.50225841772228));
#129214=CARTESIAN_POINT('Ctrl Pts',(-19.6910821069277,15.1875929083198,
6.35540933081153));
#129215=CARTESIAN_POINT('Ctrl Pts',(-19.6841521797915,15.1688824966527,
6.20858902284121));
#129216=CARTESIAN_POINT('Ctrl Pts',(-19.6772222526554,15.1437730382402,
6.06256704375078));
#129217=CARTESIAN_POINT('Ctrl Pts',(-19.6702923255192,15.1123580259662,
5.91790624571419));
#129218=CARTESIAN_POINT('Ctrl Pts',(-19.6633621941248,15.0809420877409,
5.77324118382936));
#129219=CARTESIAN_POINT('Ctrl Pts',(-19.6564320627304,15.0432202905388,
5.62993770751524));
#129220=CARTESIAN_POINT('Ctrl Pts',(-19.649501931336,14.9993371489926,5.4885480019888));
#129221=CARTESIAN_POINT('Ctrl Pts',(-19.6425721921158,14.9554564907814,
5.34716629766733));
#129222=CARTESIAN_POINT('Ctrl Pts',(-19.6356424528956,14.9054152848104,
5.20769846335047));
#129223=CARTESIAN_POINT('Ctrl Pts',(-19.6287127136755,14.8494077822416,
5.07068107169002));
#129224=CARTESIAN_POINT('Ctrl Pts',(-19.6217814385137,14.7933878658937,
4.93363331081897));
#129225=CARTESIAN_POINT('Ctrl Pts',(-19.614850163352,14.7313991358923,4.7990373843918));
#129226=CARTESIAN_POINT('Ctrl Pts',(-19.6079188881903,14.6636840544642,
4.66741003169391));
#129227=CARTESIAN_POINT('Ctrl Pts',(-19.6037893649705,14.6233406840804,
4.58898893360848));
#129228=CARTESIAN_POINT('Ctrl Pts',(-19.5996598417508,14.5809656252747,
4.51162113845325));
#129229=CARTESIAN_POINT('Ctrl Pts',(-19.5955303185311,14.5366179506424,
4.43541185194857));
#129230=CARTESIAN_POINT('Ctrl Pts',(-19.5885944784662,14.4621327468707,
4.30741271148285));
#129231=CARTESIAN_POINT('Ctrl Pts',(-19.5816586384013,14.3820549717155,
4.1826393380251));
#129232=CARTESIAN_POINT('Ctrl Pts',(-19.5747227983364,14.2966886979184,
4.06157536153454));
#129233=CARTESIAN_POINT('Ctrl Pts',(-19.5677882396657,14.2113381955128,
3.94053375157444));
#129234=CARTESIAN_POINT('Ctrl Pts',(-19.560853680995,14.1207013340158,3.82320044090237));
#129235=CARTESIAN_POINT('Ctrl Pts',(-19.5539191223243,14.0251250075616,
3.71002936176316));
#129236=CARTESIAN_POINT('Ctrl Pts',(-19.5469842888657,13.9295448938135,
3.59685379812276));
#129237=CARTESIAN_POINT('Ctrl Pts',(-19.5400494554072,13.829025134011,3.48784105031471));
#129238=CARTESIAN_POINT('Ctrl Pts',(-19.5331146219486,13.7239526913764,
3.38341171136981));
#129239=CARTESIAN_POINT('Ctrl Pts',(-19.5261801519479,13.6188857556362,
3.27898784561402));
#129240=CARTESIAN_POINT('Ctrl Pts',(-19.5192456819471,13.5092668493917,
3.17914714004377));
#129241=CARTESIAN_POINT('Ctrl Pts',(-19.5123112119463,13.3955195536049,
3.08427308466612));
#129242=CARTESIAN_POINT('Ctrl Pts',(-19.5053752028742,13.2817470121674,
2.98937797246017));
#129243=CARTESIAN_POINT('Ctrl Pts',(-19.498439193802,13.1638445039637,2.89945192455088));
#129244=CARTESIAN_POINT('Ctrl Pts',(-19.4915031847299,13.0422689075063,
2.81483831955505));
#129245=CARTESIAN_POINT('Ctrl Pts',(-19.4873970143609,12.9702952254405,
2.76474641886229));
#129246=CARTESIAN_POINT('Ctrl Pts',(-19.4832908439919,12.8970348335195,
2.7165156038769));
#129247=CARTESIAN_POINT('Ctrl Pts',(-19.4791846736229,12.8225874034969,
2.67021002390112));
#129248=CARTESIAN_POINT('Ctrl Pts',(-19.4722525221646,12.6969031736126,
2.59203565096661));
#129249=CARTESIAN_POINT('Ctrl Pts',(-19.4653203707063,12.5677907388499,
2.51932374374962));
#129250=CARTESIAN_POINT('Ctrl Pts',(-19.4583882192479,12.4357445771247,
2.45235918849313));
#129251=CARTESIAN_POINT('Ctrl Pts',(-19.4514574046156,12.3037238797516,
2.38540754697065));
#129252=CARTESIAN_POINT('Ctrl Pts',(-19.4445265899833,12.1687708790819,
2.32420119569282));
#129253=CARTESIAN_POINT('Ctrl Pts',(-19.437595775351,12.0314040081221,2.2689787419745));
#129254=CARTESIAN_POINT('Ctrl Pts',(-19.4306647326403,11.8940326167084,
2.21375447100176));
#129255=CARTESIAN_POINT('Ctrl Pts',(-19.4237336899295,11.7542475017451,
2.16451461821821));
#129256=CARTESIAN_POINT('Ctrl Pts',(-19.4168026472187,11.6125869069858,
2.12144957735116));
#129257=CARTESIAN_POINT('Ctrl Pts',(-19.4098719853274,11.4709340956326,
2.07838690265164));
#129258=CARTESIAN_POINT('Ctrl Pts',(-19.4029413234362,11.3274063275018,
2.04149845637549));
#129259=CARTESIAN_POINT('Ctrl Pts',(-19.3960106615449,11.1825568421866,
2.01092470620818));
#129260=CARTESIAN_POINT('Ctrl Pts',(-19.3890784541281,11.0376750556869,
1.98034413814747));
#129261=CARTESIAN_POINT('Ctrl Pts',(-19.3821462467112,10.8914712869162,
1.95608114825949));
#129262=CARTESIAN_POINT('Ctrl Pts',(-19.3752140392943,10.7445094240285,
1.93822517210058));
#129263=CARTESIAN_POINT('Ctrl Pts',(-19.3710890357678,10.6570599052499,
1.92759999022186));
#129264=CARTESIAN_POINT('Ctrl Pts',(-19.3669640322412,10.5693421308198,
1.91924244470383));
#129265=CARTESIAN_POINT('Ctrl Pts',(-19.3628390287147,10.481475913415,1.91316267643876));
#129266=CARTESIAN_POINT('Ctrl Pts',(-19.3559048049855,10.3337708252122,
1.90294244920731));
#129267=CARTESIAN_POINT('Ctrl Pts',(-19.3489705812563,10.1855950223114,
1.89915811409712));
#129268=CARTESIAN_POINT('Ctrl Pts',(-19.3420363575271,10.0375191660747,
1.90182968838914));
#129269=CARTESIAN_POINT('Ctrl Pts',(-19.3351034415158,9.8894712353064,1.9045007588518));
#129270=CARTESIAN_POINT('Ctrl Pts',(-19.3281705255045,9.74152354381111,
1.9136253036207));
#129271=CARTESIAN_POINT('Ctrl Pts',(-19.3212376094931,9.59424623169765,
1.9291712310986));
#129272=CARTESIAN_POINT('Ctrl Pts',(-19.3143044421616,9.44696358073864,
1.9447177221209));
#129273=CARTESIAN_POINT('Ctrl Pts',(-19.30737127483,9.30035168675085,1.96668603024645));
#129274=CARTESIAN_POINT('Ctrl Pts',(-19.3004381074985,9.15497560566773,
1.99499218733364));
#129275=CARTESIAN_POINT('Ctrl Pts',(-19.2935053129045,9.00960734022225,
2.02329682263908));
#129276=CARTESIAN_POINT('Ctrl Pts',(-19.2865725183105,8.86547507891971,
2.05793856101137));
#129277=CARTESIAN_POINT('Ctrl Pts',(-19.2796397237165,8.72313373977314,
2.09878230007118));
#129278=CARTESIAN_POINT('Ctrl Pts',(-19.2727053897295,8.58076079443217,
2.13963510828241));
#129279=CARTESIAN_POINT('Ctrl Pts',(-19.2657710557426,8.44017988357931,
2.18669257768057));
#129280=CARTESIAN_POINT('Ctrl Pts',(-19.2588367217556,8.30193143109621,
2.23976953016401));
#129281=CARTESIAN_POINT('Ctrl Pts',(-19.2547222757726,8.21990253098119,
2.27126242542232));
#129282=CARTESIAN_POINT('Ctrl Pts',(-19.2506078297895,8.13869448353687,
2.30487357806509));
#129283=CARTESIAN_POINT('Ctrl Pts',(-19.2464933838065,8.05841702068354,
2.34055622495714));
#129284=CARTESIAN_POINT('Ctrl Pts',(-19.2395600669797,7.92314022125396,
2.40068560741598));
#129285=CARTESIAN_POINT('Ctrl Pts',(-19.232626750153,7.79046037418254,2.4667205608979));
#129286=CARTESIAN_POINT('Ctrl Pts',(-19.2256934333262,7.66089097296183,
2.53841166493079));
#129287=CARTESIAN_POINT('Ctrl Pts',(-19.218761436208,7.53134623437504,2.61008912306088));
#129288=CARTESIAN_POINT('Ctrl Pts',(-19.2118294390899,7.40491104954959,
2.68742042376904));
#129289=CARTESIAN_POINT('Ctrl Pts',(-19.2048974419717,7.28207405548853,
2.77011034534907));
#129290=CARTESIAN_POINT('Ctrl Pts',(-19.1979652025665,7.1592327680301,2.8528031571064));
#129291=CARTESIAN_POINT('Ctrl Pts',(-19.1910329631612,7.03999019913484,
2.94085478267516));
#129292=CARTESIAN_POINT('Ctrl Pts',(-19.184100723756,6.92480620440643,3.03392654171861));
#129293=CARTESIAN_POINT('Ctrl Pts',(-19.177168859976,6.8096284509534,3.12699325764406));
#129294=CARTESIAN_POINT('Ctrl Pts',(-19.170236996196,6.69850908820766,3.22507935421226));
#129295=CARTESIAN_POINT('Ctrl Pts',(-19.163305132416,6.5918750714188,3.32780571528673));
#129296=CARTESIAN_POINT('Ctrl Pts',(-19.1563717255625,6.48521731727435,
3.43055494384976));
#129297=CARTESIAN_POINT('Ctrl Pts',(-19.1494383187091,6.38304714234844,
3.53794627142115));
#129298=CARTESIAN_POINT('Ctrl Pts',(-19.1425049118557,6.28575524711227,
3.64956312182307));
#129299=CARTESIAN_POINT('Ctrl Pts',(-19.1383858542032,6.22795524574662,
3.71587341509055));
#129300=CARTESIAN_POINT('Ctrl Pts',(-19.1342667965508,6.17187627667052,
3.7836743770029));
#129301=CARTESIAN_POINT('Ctrl Pts',(-19.1301477388983,6.11759365881622,
3.8528729753044));
#129302=CARTESIAN_POINT('Ctrl Pts',(-19.1232141282746,6.02621971662068,
3.96935499056361));
#129303=CARTESIAN_POINT('Ctrl Pts',(-19.1162805176509,5.93990636053414,
4.08983920703717));
#129304=CARTESIAN_POINT('Ctrl Pts',(-19.1093469070272,5.85899051470744,
4.21386473120448));
#129305=CARTESIAN_POINT('Ctrl Pts',(-19.1024146126326,5.77809002939035,
4.3378667112163));
#129306=CARTESIAN_POINT('Ctrl Pts',(-19.095482318238,5.70258519057678,4.46540838095846));
#129307=CARTESIAN_POINT('Ctrl Pts',(-19.0885500238434,5.63276951068097,
4.5960000194616));
#129308=CARTESIAN_POINT('Ctrl Pts',(-19.0816174848406,5.56295136731649,
4.72659626593262));
#129309=CARTESIAN_POINT('Ctrl Pts',(-19.0746849458378,5.49882294336051,
4.86024240657262));
#129310=CARTESIAN_POINT('Ctrl Pts',(-19.067752406835,5.44063196898206,4.99642380037644));
#129311=CARTESIAN_POINT('Ctrl Pts',(-19.0608202428625,5.38244414256678,
5.13259782716129));
#129312=CARTESIAN_POINT('Ctrl Pts',(-19.0538880788899,5.33019325204807,
5.27130652831807));
#129313=CARTESIAN_POINT('Ctrl Pts',(-19.0469559149174,5.28407902177485,
5.41201494220643));
#129314=CARTESIAN_POINT('Ctrl Pts',(-19.0400222095796,5.2379545380122,5.55275464258111));
#129315=CARTESIAN_POINT('Ctrl Pts',(-19.0330885042419,5.19796954390401,
5.69549462988479));
#129316=CARTESIAN_POINT('Ctrl Pts',(-19.0261547989042,5.1642741877754,5.83968382170268));
#129317=CARTESIAN_POINT('Ctrl Pts',(-19.0220372305995,5.1442642618192,5.92531031103094));
#129318=CARTESIAN_POINT('Ctrl Pts',(-19.0179196622948,5.12647145780716,
6.01144759299916));
#129319=CARTESIAN_POINT('Ctrl Pts',(-19.0138020939901,5.11091873588374,
6.09797832871864));
#129320=CARTESIAN_POINT('Ctrl Pts',(-19.0068685366575,5.08472956762835,
6.24368709970922));
#129321=CARTESIAN_POINT('Ctrl Pts',(-18.9999349793249,5.06488588872228,
6.39056232944993));
#129322=CARTESIAN_POINT('Ctrl Pts',(-18.9930014219922,5.05146956995229,
6.53803901516524));
#129323=CARTESIAN_POINT('Ctrl Pts',(-18.9860691811566,5.03805579858218,
6.68548769900486));
#129324=CARTESIAN_POINT('Ctrl Pts',(-18.9791369403209,5.03106698243318,
6.83353728193027));
#129325=CARTESIAN_POINT('Ctrl Pts',(-18.9722046994853,5.03053313522663,
6.981617618673));
#129326=CARTESIAN_POINT('Ctrl Pts',(-18.9652722139179,5.02999926917346,
7.12970318315559));
#129327=CARTESIAN_POINT('Ctrl Pts',(-18.9583397283506,5.03592083259744,
7.27781917307016));
#129328=CARTESIAN_POINT('Ctrl Pts',(-18.9514072427832,5.04827571738032,
7.425394863293));
#129329=CARTESIAN_POINT('Ctrl Pts',(-18.9444751320469,5.06062993414973,
7.5729625742793));
#129330=CARTESIAN_POINT('Ctrl Pts',(-18.9375430213105,5.07941674773547,
7.71998971467153));
#129331=CARTESIAN_POINT('Ctrl Pts',(-18.9306109105742,5.10456211729908,
7.86591008482244));
#129332=CARTESIAN_POINT('Ctrl Pts',(-18.9236772576965,5.1297130807884,8.01186291692259));
#129333=CARTESIAN_POINT('Ctrl Pts',(-18.9167436048189,5.16122537054665,
8.15670816091301));
#129334=CARTESIAN_POINT('Ctrl Pts',(-18.9098099519412,5.19897359234506,
8.29988858884801));
#129335=CARTESIAN_POINT('Ctrl Pts',(-18.9056921176548,5.22139192287256,
8.38492216144007));
#129336=CARTESIAN_POINT('Ctrl Pts',(-18.9015742833684,5.24600873413893,
8.46936874424738));
#129337=CARTESIAN_POINT('Ctrl Pts',(-18.8974564490819,5.27278935781425,
8.55311388445269));
#129338=CARTESIAN_POINT('Ctrl Pts',(-18.8905229466365,5.31788187655751,
8.69412177695536));
#129339=CARTESIAN_POINT('Ctrl Pts',(-18.883589444191,5.36912726528092,8.83318887245178));
#129340=CARTESIAN_POINT('Ctrl Pts',(-18.8766559417456,5.42633328808934,
8.96977762196028));
#129341=CARTESIAN_POINT('Ctrl Pts',(-18.8697236783249,5.48352908811637,
9.10634196290375));
#129342=CARTESIAN_POINT('Ctrl Pts',(-18.8627914149043,5.54668326980763,
9.24042853657159));
#129343=CARTESIAN_POINT('Ctrl Pts',(-18.8558591514836,5.61555536291239,
9.37151951569199));
#129344=CARTESIAN_POINT('Ctrl Pts',(-18.8547452675519,5.62662180877491,
9.39258336257253));
#129345=CARTESIAN_POINT('Ctrl Pts',(-18.8536313836203,5.63783578315601,
9.41356991427992));
#129346=CARTESIAN_POINT('Ctrl Pts',(-18.8525174996886,5.6491961756188,9.4344770775744));
#129347=CARTESIAN_POINT('Ctrl Pts',(-20.35256332674,5.6491961756188,9.4344770775744));
#129348=CARTESIAN_POINT('Ctrl Pts',(-20.3452864953739,5.72333205001175,
9.57091345835869));
#129349=CARTESIAN_POINT('Ctrl Pts',(-20.3380096640078,5.80368599783711,
9.70392825010587));
#129350=CARTESIAN_POINT('Ctrl Pts',(-20.3307328326417,5.88992663933501,
9.83298759607941));
#129351=CARTESIAN_POINT('Ctrl Pts',(-20.3234537917686,5.97619346658475,
9.96208612909918));
#129352=CARTESIAN_POINT('Ctrl Pts',(-20.3161747508955,6.06835041676543,
10.0872266066909));
#129353=CARTESIAN_POINT('Ctrl Pts',(-20.3088957100224,6.16602295733249,
10.20790441445));
#129354=CARTESIAN_POINT('Ctrl Pts',(-20.3037985360084,6.23441849794657,
10.2924094744585));
#129355=CARTESIAN_POINT('Ctrl Pts',(-20.2987013619943,6.30551773923257,
10.3747268589894));
#129356=CARTESIAN_POINT('Ctrl Pts',(-20.2936041879802,6.3791801760683,10.4546927820321));
#129357=CARTESIAN_POINT('Ctrl Pts',(-20.2868779809018,6.47638478448219,
10.5602154414733));
#129358=CARTESIAN_POINT('Ctrl Pts',(-20.2801517738235,6.57810999823997,
10.6617018342539));
#129359=CARTESIAN_POINT('Ctrl Pts',(-20.2734255667451,6.68398946099055,
10.7587575241793));
#129360=CARTESIAN_POINT('Ctrl Pts',(-20.2667029434128,6.7898125108012,10.8557615025012));
#129361=CARTESIAN_POINT('Ctrl Pts',(-20.2599803200806,6.89978512979311,
10.9483392324725));
#129362=CARTESIAN_POINT('Ctrl Pts',(-20.2532576967484,7.01350428426586,
11.0361332608731));
#129363=CARTESIAN_POINT('Ctrl Pts',(-20.2465367266287,7.12719547317678,
11.1239056991614));
#129364=CARTESIAN_POINT('Ctrl Pts',(-20.2398157565091,7.24463107375143,
11.2068965514905));
#129365=CARTESIAN_POINT('Ctrl Pts',(-20.2330947863894,7.36537511122738,
11.2847887461656));
#129366=CARTESIAN_POINT('Ctrl Pts',(-20.2263749847876,7.48609815596555,
11.3626673983881));
#129367=CARTESIAN_POINT('Ctrl Pts',(-20.2196551831858,7.61012818104768,
11.435448961937));
#129368=CARTESIAN_POINT('Ctrl Pts',(-20.212935381584,7.73700061751279,11.5028599472778));
#129369=CARTESIAN_POINT('Ctrl Pts',(-20.2062137509067,7.86390758762793,
11.570289281343));
#129370=CARTESIAN_POINT('Ctrl Pts',(-20.1994921202293,7.99365819072875,
11.6323449420533));
#129371=CARTESIAN_POINT('Ctrl Pts',(-20.1927704895519,8.12576338186563,
11.6887994801599));
#129372=CARTESIAN_POINT('Ctrl Pts',(-20.1875998407253,8.2273859767871,11.732227422757));
#129373=CARTESIAN_POINT('Ctrl Pts',(-20.1824291918987,8.33040137579851,
11.7723418012303));
#129374=CARTESIAN_POINT('Ctrl Pts',(-20.1772585430721,8.43457914043762,
11.809058564815));
#129375=CARTESIAN_POINT('Ctrl Pts',(-20.1702026804407,8.57674002221321,
11.8591622266207));
#129376=CARTESIAN_POINT('Ctrl Pts',(-20.1631468178092,8.72111220267323,
11.9029539856882));
#129377=CARTESIAN_POINT('Ctrl Pts',(-20.1560909551778,8.86712880719496,
11.9402651721923));
#129378=CARTESIAN_POINT('Ctrl Pts',(-20.1490348696706,9.01315002398955,
11.9775775372567));
#129379=CARTESIAN_POINT('Ctrl Pts',(-20.1419787841634,9.16081547203784,
12.0084088496475));
#129380=CARTESIAN_POINT('Ctrl Pts',(-20.1349226986562,9.30954582988,12.0326410719326));
#129381=CARTESIAN_POINT('Ctrl Pts',(-20.1278650246748,9.45830967007435,
12.0568787494039));
#129382=CARTESIAN_POINT('Ctrl Pts',(-20.1208073506934,9.60813859809027,
12.0745143189556));
#129383=CARTESIAN_POINT('Ctrl Pts',(-20.1137496767119,9.75844499148024,
12.085481214266));
#129384=CARTESIAN_POINT('Ctrl Pts',(-20.1079486163518,9.8819894429335,12.094495461995));
#129385=CARTESIAN_POINT('Ctrl Pts',(-20.1021475559916,10.0058562501456,
12.0990052732534));
#129386=CARTESIAN_POINT('Ctrl Pts',(-20.0963464956315,10.1297172751558,
12.0989999953708));
#129387=CARTESIAN_POINT('',(-20.2216535043684,10.1252586289357,12.098998236004));
#129388=CARTESIAN_POINT('Ctrl Pts',(-20.4776000298804,5.6491961756188,9.4344770775744));
#129389=CARTESIAN_POINT('Ctrl Pts',(-20.4711196343864,5.71518737462922,
9.55592435839926));
#129390=CARTESIAN_POINT('Ctrl Pts',(-20.4646392388925,5.78621302249013,
9.67485669317108));
#129391=CARTESIAN_POINT('Ctrl Pts',(-20.4581588433985,5.86205110746356,
9.7908208379596));
#129392=CARTESIAN_POINT('Ctrl Pts',(-20.4516842460785,5.93782133818231,
9.90668122669182));
#129393=CARTESIAN_POINT('Ctrl Pts',(-20.4452096487584,6.01839522353272,
10.0195783739772));
#129394=CARTESIAN_POINT('Ctrl Pts',(-20.4387350514384,6.10350485213512,
10.1290835829949));
#129395=CARTESIAN_POINT('Ctrl Pts',(-20.4319678385689,6.1924609594459,10.243537814372));
#129396=CARTESIAN_POINT('Ctrl Pts',(-20.4252006256994,6.28637217257196,
10.3542859469112));
#129397=CARTESIAN_POINT('Ctrl Pts',(-20.4184334128299,6.38488171041246,
10.4608719804822));
#129398=CARTESIAN_POINT('Ctrl Pts',(-20.4119646414821,6.47904686941601,
10.562757452882));
#129399=CARTESIAN_POINT('Ctrl Pts',(-20.4054958701343,6.5774131285831,10.6608397694563));
#129400=CARTESIAN_POINT('Ctrl Pts',(-20.3990270987865,6.67962808601849,
10.7547549556691));
#129401=CARTESIAN_POINT('Ctrl Pts',(-20.392558785631,6.7818358034224,10.8486634897351));
#129402=CARTESIAN_POINT('Ctrl Pts',(-20.3860904724756,6.88789138192054,
10.9384052085303));
#129403=CARTESIAN_POINT('Ctrl Pts',(-20.3796221593201,6.99740680186872,
11.0236542095737));
#129404=CARTESIAN_POINT('Ctrl Pts',(-20.3731528261516,7.10693949172239,
11.1089166538581));
#129405=CARTESIAN_POINT('Ctrl Pts',(-20.366683492983,7.21993279133841,11.189684725096));
#129406=CARTESIAN_POINT('Ctrl Pts',(-20.3602141598145,7.33596740778494,
11.2656742323145));
#129407=CARTESIAN_POINT('Ctrl Pts',(-20.3537423276633,7.45204684623852,
11.3416930928617));
#129408=CARTESIAN_POINT('Ctrl Pts',(-20.3472704955121,7.57116960235738,
11.4129294991824));
#129409=CARTESIAN_POINT('Ctrl Pts',(-20.3407986633609,7.69288983290592,
11.4791441027962));
#129410=CARTESIAN_POINT('Ctrl Pts',(-20.3343191314151,7.81475487882639,
11.5454374845424));
#129411=CARTESIAN_POINT('Ctrl Pts',(-20.3278395994692,7.9392232143583,11.60669694793));
#129412=CARTESIAN_POINT('Ctrl Pts',(-20.3213600675234,8.06582667605563,
11.6627302529784));
#129413=CARTESIAN_POINT('Ctrl Pts',(-20.3148760101054,8.19251856087417,
11.7188026931316));
#129414=CARTESIAN_POINT('Ctrl Pts',(-20.3083919526874,8.321348168011,11.7696415644407));
#129415=CARTESIAN_POINT('Ctrl Pts',(-20.3019078952694,8.45183129723872,
11.8151042277167));
#129416=CARTESIAN_POINT('Ctrl Pts',(-20.2954140890341,8.58251060859469,
11.860635244366));
#129417=CARTESIAN_POINT('Ctrl Pts',(-20.2889202827989,8.71484802107036,
11.9007738090514));
#129418=CARTESIAN_POINT('Ctrl Pts',(-20.2824264765636,8.84834794582099,
11.9354280882283));
#129419=CARTESIAN_POINT('Ctrl Pts',(-20.2803916318992,8.8901803627013,11.946287062538));
#129420=CARTESIAN_POINT('Ctrl Pts',(-20.2783567872349,8.93212688187923,
11.956607921674));
#129421=CARTESIAN_POINT('Ctrl Pts',(-20.2763219425705,8.97417216558045,
11.9663888888221));
#129422=CARTESIAN_POINT('Ctrl Pts',(-20.2664274954747,9.17861766576668,
12.0139489132734));
#129423=CARTESIAN_POINT('Ctrl Pts',(-20.2565330483789,9.38595698020578,
12.0488706803317));
#129424=CARTESIAN_POINT('Ctrl Pts',(-20.2466386012831,9.59491891455191,
12.0708997291488));
#129425=CARTESIAN_POINT('Ctrl Pts',(-20.2383102356448,9.77080659951878,
12.0894420460094));
#129426=CARTESIAN_POINT('Ctrl Pts',(-20.2299818700066,9.94784426009558,
12.0988506618854));
#129427=CARTESIAN_POINT('Ctrl Pts',(-20.2216535043684,10.1252586289357,
12.098998236004));
#129428=CARTESIAN_POINT('Ctrl Pts',(-20.2216531624029,10.1252652855325,
12.0997546424994));
#129429=CARTESIAN_POINT('Ctrl Pts',(-20.1623123258533,11.389567257658,12.087821313962));
#129430=CARTESIAN_POINT('Ctrl Pts',(-20.0641896076676,13.4904584433699,
11.2892797426427));
#129431=CARTESIAN_POINT('Ctrl Pts',(-19.9272850078459,15.1309521650029,
8.75245213992368));
#129432=CARTESIAN_POINT('Ctrl Pts',(-19.8109393629377,15.377488382025,6.21192549167328));
#129433=CARTESIAN_POINT('Ctrl Pts',(-19.6945937180295,14.3935630371621,
3.84345496751412));
#129434=CARTESIAN_POINT('Ctrl Pts',(-19.5782480731213,12.4208416194932,
2.21543165074234));
#129435=CARTESIAN_POINT('Ctrl Pts',(-19.4619024282132,9.91265035575874,
1.69885130841003));
#129436=CARTESIAN_POINT('Ctrl Pts',(-19.3455567833049,7.45588094355372,
2.41786028132917));
#129437=CARTESIAN_POINT('Ctrl Pts',(-19.2292111383967,5.62120273326431,
4.20319480177778));
#129438=CARTESIAN_POINT('Ctrl Pts',(-19.1128654934885,4.83646615949574,
6.64003369704514));
#129439=CARTESIAN_POINT('Ctrl Pts',(-19.029068925101,5.15885344613513,8.45540706951305));
#129440=CARTESIAN_POINT('Ctrl Pts',(-18.9840542383494,5.58538293497073,
9.31766121934795));
#129441=CARTESIAN_POINT('Ctrl Pts',(-18.977821433234,5.64904402747702,9.43455986027809));
#129442=CARTESIAN_POINT('Origin',(26.8463464956315,10.1295,7.));
#129443=CARTESIAN_POINT('',(23.3525227608221,14.6098038194187,9.43447708670711));
#129444=CARTESIAN_POINT('',(23.4778327564121,14.6092485246327,9.4341754467045));
#129445=CARTESIAN_POINT('',(26.8463464956315,14.6098038194187,9.43447708670711));
#129446=CARTESIAN_POINT('',(23.5339999999999,15.0538811994916,5.6770219948566));
#129447=CARTESIAN_POINT('Ctrl Pts',(23.5339999999999,15.0538811994916,5.6770219948566));
#129448=CARTESIAN_POINT('Ctrl Pts',(23.5270930717027,15.0921506970965,5.8194685009863));
#129449=CARTESIAN_POINT('Ctrl Pts',(23.5201861434054,15.1242415793792,5.96360031998381));
#129450=CARTESIAN_POINT('Ctrl Pts',(23.5132792151082,15.1500258622284,6.10886529262073));
#129451=CARTESIAN_POINT('Ctrl Pts',(23.5063724323829,15.1758096016423,6.25412720362094));
#129452=CARTESIAN_POINT('Ctrl Pts',(23.4994656496576,15.1952869431655,6.40052189108961));
#129453=CARTESIAN_POINT('Ctrl Pts',(23.4925588669324,15.2083811232991,6.54748753012045));
#129454=CARTESIAN_POINT('Ctrl Pts',(23.4856526906085,15.2214741537902,6.69444026586755));
#129455=CARTESIAN_POINT('Ctrl Pts',(23.4787465142847,15.2281851137662,6.84196351862882));
#129456=CARTESIAN_POINT('Ctrl Pts',(23.4718403379609,15.2284891702847,6.98949089349636));
#129457=CARTESIAN_POINT('Ctrl Pts',(23.4649324938645,15.2287933002297,7.13705389474971));
#129458=CARTESIAN_POINT('Ctrl Pts',(23.4580246497681,15.2226874332482,7.28462068429066));
#129459=CARTESIAN_POINT('Ctrl Pts',(23.4511168056718,15.2101988752891,7.43162476601365));
#129460=CARTESIAN_POINT('Ctrl Pts',(23.4457234039484,15.2004482484538,7.54640038292906));
#129461=CARTESIAN_POINT('Ctrl Pts',(23.4403300022249,15.186807817628,7.66083293227476));
#129462=CARTESIAN_POINT('Ctrl Pts',(23.4349366005015,15.1693125726679,7.77465491180164));
#129463=CARTESIAN_POINT('Ctrl Pts',(23.428002553564,15.1468197460705,7.92099056210697));
#129464=CARTESIAN_POINT('Ctrl Pts',(23.4210685066266,15.1179452650816,8.06637109676426));
#129465=CARTESIAN_POINT('Ctrl Pts',(23.4141344596891,15.0827949924592,8.21023539763084));
#129466=CARTESIAN_POINT('Ctrl Pts',(23.4072019007547,15.0476522628654,8.35406882611838));
#129467=CARTESIAN_POINT('Ctrl Pts',(23.4002693418204,15.0062365079439,8.49638634919968));
#129468=CARTESIAN_POINT('Ctrl Pts',(23.393336782886,14.9587043104703,8.63663885073485));
#129469=CARTESIAN_POINT('Ctrl Pts',(23.3864039341192,14.9111701257981,8.77689721586582));
#129470=CARTESIAN_POINT('Ctrl Pts',(23.3794710853524,14.8575190898333,8.91509007250136));
#129471=CARTESIAN_POINT('Ctrl Pts',(23.3725382365856,14.7979572868406,9.05068465663168));
#129472=CARTESIAN_POINT('Ctrl Pts',(23.3658664113311,14.7406380008189,9.18117407032051));
#129473=CARTESIAN_POINT('Ctrl Pts',(23.3591945860766,14.6778450416099,9.30925703459592));
#129474=CARTESIAN_POINT('Ctrl Pts',(23.3525227608221,14.6098038194187,9.43447708670711));
#129475=CARTESIAN_POINT('',(23.534,15.0539061944433,8.32288496556904));
#129476=CARTESIAN_POINT('Origin',(23.534,10.1295,7.));
#129477=CARTESIAN_POINT('Ctrl Pts',(23.534,15.0539061944433,8.32288496556903));
#129478=CARTESIAN_POINT('Ctrl Pts',(23.5152775854706,14.950159911235,8.70907790976189));
#129479=CARTESIAN_POINT('Ctrl Pts',(23.4965551709413,14.8001544393626,9.08275274683618));
#129480=CARTESIAN_POINT('Ctrl Pts',(23.4778327564119,14.6092485246315,9.43417544670676));
#129481=CARTESIAN_POINT('Origin',(26.8463464956315,10.1295,7.));
#129482=CARTESIAN_POINT('',(21.8525208814298,14.6095924811794,9.43436249769606));
#129483=CARTESIAN_POINT('',(21.9778242972865,14.6098038194187,9.43447708670711));
#129484=CARTESIAN_POINT('',(26.8463464956315,14.6098038194187,9.43447708670711));
#129485=CARTESIAN_POINT('',(23.0963464956316,10.1294332246189,12.0990156955494));
#129486=CARTESIAN_POINT('Ctrl Pts',(23.0963464956316,10.1294332206623,12.0993178216526));
#129487=CARTESIAN_POINT('Ctrl Pts',(23.0928642190134,10.0550711278111,12.0993673700521));
#129488=CARTESIAN_POINT('Ctrl Pts',(23.0506000607591,9.15256913101046,12.0800148503643));
#129489=CARTESIAN_POINT('Ctrl Pts',(22.9695540208687,7.44243506000627,11.5744658280441));
#129490=CARTESIAN_POINT('Ctrl Pts',(22.8532083759605,5.61311993670382,9.783588785421));
#129491=CARTESIAN_POINT('Ctrl Pts',(22.7368627310523,4.83541687908909,7.34457045164505));
#129492=CARTESIAN_POINT('Ctrl Pts',(22.6205170861442,5.29040469497751,4.82532063665908));
#129493=CARTESIAN_POINT('Ctrl Pts',(22.504171441236,6.87215451106252,2.81243229447991));
#129494=CARTESIAN_POINT('Ctrl Pts',(22.3878257963277,9.21233876997001,1.77459149097018));
#129495=CARTESIAN_POINT('Ctrl Pts',(22.2714801514196,11.7661169025298,1.95345839105347));
#129496=CARTESIAN_POINT('Ctrl Pts',(22.1551345065114,13.9387381504676,3.30737374765752));
#129497=CARTESIAN_POINT('Ctrl Pts',(22.0387888616032,15.2245708351663,5.52111016209781));
#129498=CARTESIAN_POINT('Ctrl Pts',(21.9379176532427,15.310510332437,7.7389324002892));
#129499=CARTESIAN_POINT('Ctrl Pts',(21.8758283265182,14.8470613098453,8.99675594530229));
#129500=CARTESIAN_POINT('Ctrl Pts',(21.8525208814298,14.6095924811794,9.43436249769606));
#129501=CARTESIAN_POINT('Ctrl Pts',(23.3525227608221,14.6098038194187,9.43447708670711));
#129502=CARTESIAN_POINT('Ctrl Pts',(23.3455889836027,14.5390911345967,9.56461358033825));
#129503=CARTESIAN_POINT('Ctrl Pts',(23.3386552063833,14.4627098494206,9.69165750992628));
#129504=CARTESIAN_POINT('Ctrl Pts',(23.3317214291639,14.3809576871128,9.8151214067407));
#129505=CARTESIAN_POINT('Ctrl Pts',(23.3273446046404,14.3293530771693,9.89305581308964));
#129506=CARTESIAN_POINT('Ctrl Pts',(23.3229677801168,14.2756093228907,9.9695642618301));
#129507=CARTESIAN_POINT('Ctrl Pts',(23.3185909555933,14.2198101839654,10.0445301113552));
#129508=CARTESIAN_POINT('Ctrl Pts',(23.3116576153536,14.1314186084821,10.1632837278912));
#129509=CARTESIAN_POINT('Ctrl Pts',(23.304724275114,14.0378366099381,10.2782059009288));
#129510=CARTESIAN_POINT('Ctrl Pts',(23.2977909348743,13.9394203703912,10.3888505088419));
#129511=CARTESIAN_POINT('Ctrl Pts',(23.2908589149614,13.8410228724023,10.4994740465299));
#129512=CARTESIAN_POINT('Ctrl Pts',(23.2839268950485,13.7377931897414,10.6058213974011));
#129513=CARTESIAN_POINT('Ctrl Pts',(23.2769948751356,13.6301267227303,10.7074807549206));
#129514=CARTESIAN_POINT('Ctrl Pts',(23.2700626140937,13.5224565105608,10.8091436486423));
#129515=CARTESIAN_POINT('Ctrl Pts',(23.2631303530518,13.410349443299,10.9061179932801));
#129516=CARTESIAN_POINT('Ctrl Pts',(23.2561980920098,13.2942369915247,10.9980296115055));
#129517=CARTESIAN_POINT('Ctrl Pts',(23.2492662073036,13.1781308432153,11.089936240071));
#129518=CARTESIAN_POINT('Ctrl Pts',(23.2423343225974,13.0580200053115,11.1767804876996));
#129519=CARTESIAN_POINT('Ctrl Pts',(23.2354024378912,12.9343681645872,11.2582291600247));
#129520=CARTESIAN_POINT('Ctrl Pts',(23.2284690113988,12.8106888212853,11.3396959481209));
#129521=CARTESIAN_POINT('Ctrl Pts',(23.2215355849065,12.6834671776639,11.4157645810553));
#129522=CARTESIAN_POINT('Ctrl Pts',(23.2146021584141,12.5531954963905,11.4861454658511));
#129523=CARTESIAN_POINT('Ctrl Pts',(23.2104832091711,12.4758048377378,11.5279567250416));
#129524=CARTESIAN_POINT('Ctrl Pts',(23.2063642599281,12.3973382765711,11.5677615089315));
#129525=CARTESIAN_POINT('Ctrl Pts',(23.2022453106851,12.3179031154636,11.6055067912478));
#129526=CARTESIAN_POINT('Ctrl Pts',(23.1953326016546,12.1845894660025,11.6688535669748));
#129527=CARTESIAN_POINT('Ctrl Pts',(23.1884198926241,12.0484976489229,11.7264202163307));
#129528=CARTESIAN_POINT('Ctrl Pts',(23.1815071835936,11.9101480240635,11.7779800768106));
#129529=CARTESIAN_POINT('Ctrl Pts',(23.1744104595967,11.7681155591704,11.8309124507215));
#129530=CARTESIAN_POINT('Ctrl Pts',(23.1673137355999,11.6237037330732,11.8775136140333));
#129531=CARTESIAN_POINT('Ctrl Pts',(23.1602170116031,11.4774963192628,11.9175915775158));
#129532=CARTESIAN_POINT('Ctrl Pts',(23.1533056473611,11.3351077055635,11.9566227422935));
#129533=CARTESIAN_POINT('Ctrl Pts',(23.1463942831192,11.1910164761425,11.9894671487316));
#129534=CARTESIAN_POINT('Ctrl Pts',(23.1394829188772,11.045776141037,12.0159983087484));
#129535=CARTESIAN_POINT('Ctrl Pts',(23.132293515003,10.8946928828906,12.0435967998619));
#129536=CARTESIAN_POINT('Ctrl Pts',(23.1251041111287,10.7423665149036,12.0643634254656));
#129537=CARTESIAN_POINT('Ctrl Pts',(23.1179147072544,10.5894305429874,12.0782147350843));
#129538=CARTESIAN_POINT('Ctrl Pts',(23.1107253033801,10.4364945710712,12.092066044703));
#129539=CARTESIAN_POINT('Ctrl Pts',(23.1035358995059,10.2829494015725,12.0990020099706));
#129540=CARTESIAN_POINT('Ctrl Pts',(23.0963464956316,10.1294332248244,12.0989999995628));
#129541=CARTESIAN_POINT('',(23.2216535038391,10.1293865181645,12.0989501584294));
#129542=CARTESIAN_POINT('Ctrl Pts',(23.4778327564119,14.6092485246315,9.43417544670676));
#129543=CARTESIAN_POINT('Ctrl Pts',(23.4577732893052,14.4047091522646,9.81069483620949));
#129544=CARTESIAN_POINT('Ctrl Pts',(23.3989319405624,13.6670015456634,10.8402272996134));
#129545=CARTESIAN_POINT('Ctrl Pts',(23.3135388565479,12.092423032665,11.8658595382605));
#129546=CARTESIAN_POINT('Ctrl Pts',(23.2482052396401,10.6965329474454,12.0983697707759));
#129547=CARTESIAN_POINT('Ctrl Pts',(23.2216535043684,10.1293865324873,12.0988146186003));
#129548=CARTESIAN_POINT('Ctrl Pts',(23.2216535036445,10.1293865128977,12.0989999987371));
#129549=CARTESIAN_POINT('Ctrl Pts',(23.2144616473686,9.97576251488196,12.0989965795681));
#129550=CARTESIAN_POINT('Ctrl Pts',(23.2072697910928,9.82216920243597,12.0920461851236));
#129551=CARTESIAN_POINT('Ctrl Pts',(23.2000779348169,9.66922023943467,12.0781830945737));
#129552=CARTESIAN_POINT('Ctrl Pts',(23.1950396449697,9.56207110048146,12.0684712391514));
#129553=CARTESIAN_POINT('Ctrl Pts',(23.1900013551225,9.45523816700231,12.0553678804514));
#129554=CARTESIAN_POINT('Ctrl Pts',(23.1849630652753,9.34893090479854,12.0388999680105));
#129555=CARTESIAN_POINT('Ctrl Pts',(23.1780322106042,9.20269077031505,12.0162461089975));
#129556=CARTESIAN_POINT('Ctrl Pts',(23.1711013559331,9.05741147522505,11.9872176032497));
#129557=CARTESIAN_POINT('Ctrl Pts',(23.1641705012619,8.91365350675345,11.9519206682721));
#129558=CARTESIAN_POINT('Ctrl Pts',(23.1572409972287,8.76992355285804,11.9166306117213));
#129559=CARTESIAN_POINT('Ctrl Pts',(23.1503114931954,8.6277146554914,11.8750746419589));
#129560=CARTESIAN_POINT('Ctrl Pts',(23.1433819891621,8.48757530416641,11.8274096877323));
#129561=CARTESIAN_POINT('Ctrl Pts',(23.1364522650283,8.34743150162177,11.7797432195329));
#129562=CARTESIAN_POINT('Ctrl Pts',(23.1295225408946,8.20935769125029,11.7259674819089));
#129563=CARTESIAN_POINT('Ctrl Pts',(23.1225928167608,8.07388595843718,11.6662888800555));
#129564=CARTESIAN_POINT('Ctrl Pts',(23.1156634748197,7.93842169724982,11.6066135696355));
#129565=CARTESIAN_POINT('Ctrl Pts',(23.1087341328786,7.80555952912581,11.5410361807239));
#129566=CARTESIAN_POINT('Ctrl Pts',(23.1018047909375,7.67581036564082,11.4698107541862));
#129567=CARTESIAN_POINT('Ctrl Pts',(23.0948738940547,7.54603208649339,11.3985693446901));
#129568=CARTESIAN_POINT('Ctrl Pts',(23.0879429971719,7.4193684981623,11.321677524493));
#129569=CARTESIAN_POINT('Ctrl Pts',(23.0810121002891,7.29630531956496,11.2394349744694));
#129570=CARTESIAN_POINT('Ctrl Pts',(23.0768805403151,7.22294642942954,11.1904095693044));
#129571=CARTESIAN_POINT('Ctrl Pts',(23.0727489803412,7.15086641510118,11.139483671144));
#129572=CARTESIAN_POINT('Ctrl Pts',(23.0686174203672,7.08016321996373,11.0867280557823));
#129573=CARTESIAN_POINT('Ctrl Pts',(23.0616832524995,6.96149912529913,10.9981861260548));
#129574=CARTESIAN_POINT('Ctrl Pts',(23.0547490846318,6.84667369731443,10.9044571565873));
#129575=CARTESIAN_POINT('Ctrl Pts',(23.0478149167641,6.73613270977454,10.805897979929));
#129576=CARTESIAN_POINT('Ctrl Pts',(23.0408820598754,6.62561262119616,10.7073574369422));
#129577=CARTESIAN_POINT('Ctrl Pts',(23.0339492029866,6.51937560346518,10.603988728551));
#129578=CARTESIAN_POINT('Ctrl Pts',(23.0270163460979,6.4178330651246,10.4961878617364));
#129579=CARTESIAN_POINT('Ctrl Pts',(23.0200832422255,6.3162869093225,10.3883831545067));
#129580=CARTESIAN_POINT('Ctrl Pts',(23.0131501383532,6.21943579656273,10.2761462111623));
#129581=CARTESIAN_POINT('Ctrl Pts',(23.0062170344808,6.127653461249,10.159909062028));
#129582=CARTESIAN_POINT('Ctrl Pts',(22.9992843056565,6.0358760909238,10.0436782007715));
#129583=CARTESIAN_POINT('Ctrl Pts',(22.9923515768321,5.94916715343914,9.92344782666485));
#129584=CARTESIAN_POINT('Ctrl Pts',(22.9854188480078,5.86785936094203,9.79968213615932));
#129585=CARTESIAN_POINT('Ctrl Pts',(22.9784845828,5.78653354957469,9.67588901755805));
#129586=CARTESIAN_POINT('Ctrl Pts',(22.9715503175923,5.71061145639965,9.54855929336527));
#129587=CARTESIAN_POINT('Ctrl Pts',(22.9646160523846,5.64038215784226,9.41818568336285));
#129588=CARTESIAN_POINT('Ctrl Pts',(22.9605012934094,5.59870843641641,9.34082262241638));
#129589=CARTESIAN_POINT('Ctrl Pts',(22.9563865344342,5.55903840082034,9.26238827233416));
#129590=CARTESIAN_POINT('Ctrl Pts',(22.952271775459,5.52142478724157,9.18298965493686));
#129591=CARTESIAN_POINT('Ctrl Pts',(22.9453381235802,5.45804326136591,9.04919752373096));
#129592=CARTESIAN_POINT('Ctrl Pts',(22.9384044717014,5.40048158569252,8.91262014426123));
#129593=CARTESIAN_POINT('Ctrl Pts',(22.9314708198227,5.34896652564976,8.77378146923933));
#129594=CARTESIAN_POINT('Ctrl Pts',(22.9245384819542,5.29746122832944,8.63496910581344));
#129595=CARTESIAN_POINT('Ctrl Pts',(22.9176061440857,5.25200037531062,8.49389661159093));
#129596=CARTESIAN_POINT('Ctrl Pts',(22.9106738062172,5.21276202370896,8.3511064623106));
#129597=CARTESIAN_POINT('Ctrl Pts',(22.9037412208191,5.17352227104248,8.20831121449157));
#129598=CARTESIAN_POINT('Ctrl Pts',(22.896808635421,5.14050555518979,8.06379850674376));
#129599=CARTESIAN_POINT('Ctrl Pts',(22.8898760500228,5.1138397764683,7.9181250035164));
#129600=CARTESIAN_POINT('Ctrl Pts',(22.8829438381066,5.08717543432276,7.77245934821475));
#129601=CARTESIAN_POINT('Ctrl Pts',(22.8760116261904,5.06686140326674,7.62563334790481));
#129602=CARTESIAN_POINT('Ctrl Pts',(22.8690794142742,5.05297427438577,7.4782128785143));
#129603=CARTESIAN_POINT('Ctrl Pts',(22.8621456590075,5.03908405374907,7.33075958822291));
#129604=CARTESIAN_POINT('Ctrl Pts',(22.8552119037409,5.03162362532709,7.18271189362287));
#129605=CARTESIAN_POINT('Ctrl Pts',(22.8482781484743,5.03061766757055,7.03464043935698));
#129606=CARTESIAN_POINT('Ctrl Pts',(22.8441608091664,5.03002031891117,6.94671399898356));
#129607=CARTESIAN_POINT('Ctrl Pts',(22.8400434698586,5.03169789774968,6.85877924044733));
#129608=CARTESIAN_POINT('Ctrl Pts',(22.8359261305508,5.03564687217782,6.77095565456406));
#129609=CARTESIAN_POINT('Ctrl Pts',(22.8289927902407,5.04229669662495,6.62306626225003));
#129610=CARTESIAN_POINT('Ctrl Pts',(22.8220594499305,5.05539250041431,6.475441072363));
#129611=CARTESIAN_POINT('Ctrl Pts',(22.8151261096204,5.07488932497261,6.32864917971366));
#129612=CARTESIAN_POINT('Ctrl Pts',(22.8081940896352,5.09438243672551,6.1818852408334));
#129613=CARTESIAN_POINT('Ctrl Pts',(22.80126206965,5.12027409374897,6.03595461015652));
#129614=CARTESIAN_POINT('Ctrl Pts',(22.7943300496648,5.15246762548975,5.89141994286524));
#129615=CARTESIAN_POINT('Ctrl Pts',(22.7873977885484,5.18466227708647,5.74688024791794));
#129616=CARTESIAN_POINT('Ctrl Pts',(22.7804655274321,5.22315917345089,5.60373693696147));
#129617=CARTESIAN_POINT('Ctrl Pts',(22.7735332663157,5.26781068180806,5.46254171654044));
#129618=CARTESIAN_POINT('Ctrl Pts',(22.7666013815341,5.31245976614917,5.32135416124642));
#129619=CARTESIAN_POINT('Ctrl Pts',(22.7596694967524,5.3632626933397,5.18211479983415));
#129620=CARTESIAN_POINT('Ctrl Pts',(22.7527376119707,5.42002218067565,5.04535945266349));
#129621=CARTESIAN_POINT('Ctrl Pts',(22.745804185402,5.4767942924346,4.90857368842192));
#129622=CARTESIAN_POINT('Ctrl Pts',(22.7388707588332,5.53952548479153,4.77427334785503));
#129623=CARTESIAN_POINT('Ctrl Pts',(22.7319373322644,5.60797037248141,4.64297415638445));
#129624=CARTESIAN_POINT('Ctrl Pts',(22.7278183833905,5.64863150738803,4.56497309132748));
#129625=CARTESIAN_POINT('Ctrl Pts',(22.7236994345165,5.69130821780815,4.48803078158937));
#129626=CARTESIAN_POINT('Ctrl Pts',(22.7195804856426,5.73594135530312,4.41225128043519));
#129627=CARTESIAN_POINT('Ctrl Pts',(22.712646772094,5.81107542461016,4.28468636765235));
#129628=CARTESIAN_POINT('Ctrl Pts',(22.7057130585453,5.89178185117034,4.16037392365949));
#129629=CARTESIAN_POINT('Ctrl Pts',(22.6987793449967,5.97775435333472,4.03979576964767));
#129630=CARTESIAN_POINT('Ctrl Pts',(22.6918469457557,6.0637105591351,3.91924047161232));
#129631=CARTESIAN_POINT('Ctrl Pts',(22.6849145465148,6.15493065717947,3.80241832029139));
#129632=CARTESIAN_POINT('Ctrl Pts',(22.6779821472738,6.25106569159728,3.68978122846771));
#129633=CARTESIAN_POINT('Ctrl Pts',(22.6710495015589,6.34720414399177,3.57714013195465));
#129634=CARTESIAN_POINT('Ctrl Pts',(22.664116855844,6.44825767038205,3.46868464626526));
#129635=CARTESIAN_POINT('Ctrl Pts',(22.6571842101292,6.55383741425312,3.36483314373467));
#129636=CARTESIAN_POINT('Ctrl Pts',(22.6502519386425,6.65941145886836,3.26098724716845));
#129637=CARTESIAN_POINT('Ctrl Pts',(22.6433196671559,6.76951099574575,3.16174506759461));
#129638=CARTESIAN_POINT('Ctrl Pts',(22.6363873956692,6.8837107393556,3.0674876890866));
#129639=CARTESIAN_POINT('Ctrl Pts',(22.6294535825151,6.99793587984121,2.97320934868449));
#129640=CARTESIAN_POINT('Ctrl Pts',(22.6225197693609,7.11626279402301,2.8839182349048));
#129641=CARTESIAN_POINT('Ctrl Pts',(22.6155859562067,7.23823310513727,2.79995514992151));
#129642=CARTESIAN_POINT('Ctrl Pts',(22.6114689177159,7.31065450652515,2.75010101555235));
#129643=CARTESIAN_POINT('Ctrl Pts',(22.6073518792252,7.38435979545037,2.70212451134012));
#129644=CARTESIAN_POINT('Ctrl Pts',(22.6032348407344,7.45924813015834,2.65608978550349));
#129645=CARTESIAN_POINT('Ctrl Pts',(22.5963013558529,7.58536721737681,2.57856292333585));
#129646=CARTESIAN_POINT('Ctrl Pts',(22.5893678709714,7.71488667542895,2.50651889974949));
#129647=CARTESIAN_POINT('Ctrl Pts',(22.5824343860899,7.84731029346206,2.44024001252563));
#129648=CARTESIAN_POINT('Ctrl Pts',(22.5755022191216,7.97970874048388,2.37397372355761));
#129649=CARTESIAN_POINT('Ctrl Pts',(22.5685700521532,8.11500995065018,2.31347053248644));
#129650=CARTESIAN_POINT('Ctrl Pts',(22.5616378851848,8.2526940110444,2.25896632791747));
#129651=CARTESIAN_POINT('Ctrl Pts',(22.5547054748914,8.39038290426868,2.20446021020359));
#129652=CARTESIAN_POINT('Ctrl Pts',(22.547773064598,8.53045450894213,2.15595362514326));
#129653=CARTESIAN_POINT('Ctrl Pts',(22.5408406543045,8.67236936204863,2.11363414141517));
#129654=CARTESIAN_POINT('Ctrl Pts',(22.5339086194588,8.81427652928533,2.07131694963916));
#129655=CARTESIAN_POINT('Ctrl Pts',(22.526976584613,8.95802642811843,2.03518628227907));
#129656=CARTESIAN_POINT('Ctrl Pts',(22.5200445497673,9.10306486807957,2.00537970212355));
#129657=CARTESIAN_POINT('Ctrl Pts',(22.5131109730705,9.2481355680739,1.97556649226858));
#129658=CARTESIAN_POINT('Ctrl Pts',(22.5061773963736,9.39449505792165,1.95208024682282));
#129659=CARTESIAN_POINT('Ctrl Pts',(22.4992438196768,9.54157877108378,1.9350074404211));
#129660=CARTESIAN_POINT('Ctrl Pts',(22.4951256117266,9.62893935615771,1.92486702226029));
#129661=CARTESIAN_POINT('Ctrl Pts',(22.4910074037764,9.7165552643328,1.91698814636579));
#129662=CARTESIAN_POINT('Ctrl Pts',(22.4868891958262,9.80430724843803,1.9113802780782));
#129663=CARTESIAN_POINT('Ctrl Pts',(22.4799556232921,9.95204984768639,1.90193865638155));
#129664=CARTESIAN_POINT('Ctrl Pts',(22.4730220507579,10.1002293919555,1.89893406231333));
#129665=CARTESIAN_POINT('Ctrl Pts',(22.4660884782238,10.2482752299219,1.90238355260451));
#129666=CARTESIAN_POINT('Ctrl Pts',(22.4591562219442,10.3962929631829,1.90583238805183));
#129667=CARTESIAN_POINT('Ctrl Pts',(22.4522239656647,10.5441767104752,1.91573285564485));
#129668=CARTESIAN_POINT('Ctrl Pts',(22.4452917093852,10.6913566113617,1.93204990669116));
#129669=CARTESIAN_POINT('Ctrl Pts',(22.4383592081633,10.838541712659,1.94836753427928));
#129670=CARTESIAN_POINT('Ctrl Pts',(22.4314267069415,10.9850225888615,1.9711021658943));
#129671=CARTESIAN_POINT('Ctrl Pts',(22.4244942057197,11.1302347335151,2.00016690347203));
#129672=CARTESIAN_POINT('Ctrl Pts',(22.4175620792479,11.2754390284404,2.02923006989818));
#129673=CARTESIAN_POINT('Ctrl Pts',(22.410629952776,11.4193744050801,2.06462259177438));
#129674=CARTESIAN_POINT('Ctrl Pts',(22.4036978263042,11.5614867616133,2.10620649040397));
#129675=CARTESIAN_POINT('Ctrl Pts',(22.3967641577058,11.7036307325799,2.14779963982234));
#129676=CARTESIAN_POINT('Ctrl Pts',(22.3898304891073,11.8439505557084,2.19558682522712));
#129677=CARTESIAN_POINT('Ctrl Pts',(22.3828968205088,11.9819068852309,2.24938006871217));
#129678=CARTESIAN_POINT('Ctrl Pts',(22.3787790639786,12.063836179762,2.28132671809408));
#129679=CARTESIAN_POINT('Ctrl Pts',(22.3746613074483,12.1449322010469,2.31539070984882));
#129680=CARTESIAN_POINT('Ctrl Pts',(22.370543550918,12.2250851901569,2.35152458210273));
#129681=CARTESIAN_POINT('Ctrl Pts',(22.3636099924989,12.3600483499194,2.41236749798139));
#129682=CARTESIAN_POINT('Ctrl Pts',(22.3566764340798,12.4923832519696,2.47910262136328));
#129683=CARTESIAN_POINT('Ctrl Pts',(22.3497428756607,12.6215776949439,2.55147780017193));
#129684=CARTESIAN_POINT('Ctrl Pts',(22.3428106341768,12.7507475991896,2.62383923229903));
#129685=CARTESIAN_POINT('Ctrl Pts',(22.3358783926929,12.8767779461898,2.7018384210654));
#129686=CARTESIAN_POINT('Ctrl Pts',(22.328946151209,12.9991816332476,2.78517754539985));
#129687=CARTESIAN_POINT('Ctrl Pts',(22.3220136656563,13.1215896298659,2.86851960391878));
#129688=CARTESIAN_POINT('Ctrl Pts',(22.3150811801037,13.2403704359038,2.95720179093612));
#129689=CARTESIAN_POINT('Ctrl Pts',(22.308148694551,13.3550659593708,3.0508829794816));
#129690=CARTESIAN_POINT('Ctrl Pts',(22.3012165842048,13.4697552751808,3.14455909772731));
#129691=CARTESIAN_POINT('Ctrl Pts',(22.2942844738585,13.580359495408,3.24323346626158));
#129692=CARTESIAN_POINT('Ctrl Pts',(22.2873523635122,13.6864536413925,3.34652469654105));
#129693=CARTESIAN_POINT('Ctrl Pts',(22.2804187116004,13.7925713806377,3.44983889676766));
#129694=CARTESIAN_POINT('Ctrl Pts',(22.2734850596885,13.8941768046595,3.55777177953251));
#129695=CARTESIAN_POINT('Ctrl Pts',(22.2665514077766,13.9908813866036,3.66990468797189));
#129696=CARTESIAN_POINT('Ctrl Pts',(22.2624335738543,14.0483133738203,3.73649942045101));
#129697=CARTESIAN_POINT('Ctrl Pts',(22.2583157399321,14.1040175187899,3.80457484120395));
#129698=CARTESIAN_POINT('Ctrl Pts',(22.2541979060098,14.1579190618731,3.874037610281));
#129699=CARTESIAN_POINT('Ctrl Pts',(22.2472642956059,14.248678501657,3.99099904861213));
#129700=CARTESIAN_POINT('Ctrl Pts',(22.240330685202,14.3343563570106,4.11193599116586));
#129701=CARTESIAN_POINT('Ctrl Pts',(22.2333970747981,14.4146181346602,4.23638577728254));
#129702=CARTESIAN_POINT('Ctrl Pts',(22.2264647807023,14.4948646750486,4.36081193728546));
#129703=CARTESIAN_POINT('Ctrl Pts',(22.2195324866065,14.569697010104,4.48874933264206));
#129704=CARTESIAN_POINT('Ctrl Pts',(22.2126001925108,14.6388242094336,4.61970670416093));
#129705=CARTESIAN_POINT('Ctrl Pts',(22.2056676539223,14.7079538467869,4.75066869437094));
#129706=CARTESIAN_POINT('Ctrl Pts',(22.1987351153338,14.7713777885139,4.88465058310104));
#129707=CARTESIAN_POINT('Ctrl Pts',(22.1918025767453,14.8288510170149,5.0211364324741));
#129708=CARTESIAN_POINT('Ctrl Pts',(22.1848704132515,14.8863211358465,5.1576148970895));
#129709=CARTESIAN_POINT('Ctrl Pts',(22.1779382497577,14.9378410582831,5.29659674622179));
#129710=CARTESIAN_POINT('Ctrl Pts',(22.1710060862639,14.9832138788456,5.43754597433969));
#129711=CARTESIAN_POINT('Ctrl Pts',(22.1640723815,15.028596787423,5.57852654055607));
#129712=CARTESIAN_POINT('Ctrl Pts',(22.1571386767362,15.0678297619024,5.72147504499835));
#129713=CARTESIAN_POINT('Ctrl Pts',(22.1502049719723,15.1007655570025,5.86583962255727));
#129714=CARTESIAN_POINT('Ctrl Pts',(22.1460874016821,15.1203244300737,5.95157031282543));
#129715=CARTESIAN_POINT('Ctrl Pts',(22.1419698313918,15.1376635206223,6.03780011735071));
#129716=CARTESIAN_POINT('Ctrl Pts',(22.1378522611016,15.1527604864707,6.12441157781638));
#129717=CARTESIAN_POINT('Ctrl Pts',(22.1309189472056,15.1781813040225,6.2702510899736));
#129718=CARTESIAN_POINT('Ctrl Pts',(22.1239856333095,15.1972510326479,6.41722360612239));
#129719=CARTESIAN_POINT('Ctrl Pts',(22.1170523194135,15.2098907721861,6.56476374015232));
#129720=CARTESIAN_POINT('Ctrl Pts',(22.1101203233419,15.2225281092719,6.71227583102898));
#129721=CARTESIAN_POINT('Ctrl Pts',(22.1031883272702,15.2287378674464,6.86035499529251));
#129722=CARTESIAN_POINT('Ctrl Pts',(22.0962563311985,15.2284930298674,7.00843097644207));
#129723=CARTESIAN_POINT('Ctrl Pts',(22.089324090006,15.2282481836308,7.15651219367546));
#129724=CARTESIAN_POINT('Ctrl Pts',(22.0823918488135,15.2215482821267,7.30458989694481));
#129725=CARTESIAN_POINT('Ctrl Pts',(22.075459607621,15.2084184326879,7.45209352362437));
#129726=CARTESIAN_POINT('Ctrl Pts',(22.0685277404533,15.195289291662,7.59958919183696));
#129727=CARTESIAN_POINT('Ctrl Pts',(22.0615958732855,15.1757309271479,7.74651051618775));
#129728=CARTESIAN_POINT('Ctrl Pts',(22.0546640061178,15.1498203546764,7.89229173279906));
#129729=CARTESIAN_POINT('Ctrl Pts',(22.0477305934374,15.1239040052451,8.03810545244515));
#129730=CARTESIAN_POINT('Ctrl Pts',(22.0407971807569,15.0916326758373,8.18277823079145));
#129731=CARTESIAN_POINT('Ctrl Pts',(22.0338637680765,15.0531346874517,8.3257535459212));
#129732=CARTESIAN_POINT('Ctrl Pts',(22.0297447174488,15.030263531423,8.41069332791269));
#129733=CARTESIAN_POINT('Ctrl Pts',(22.0256256668211,15.0051957146653,8.49503421516281));
#129734=CARTESIAN_POINT('Ctrl Pts',(22.0215066161934,14.9779665423999,8.57866183434857));
#129735=CARTESIAN_POINT('Ctrl Pts',(22.0142262297089,14.9298392150951,8.72647293051569));
#129736=CARTESIAN_POINT('Ctrl Pts',(22.0069458432244,14.8749389088111,8.87210820366851));
#129737=CARTESIAN_POINT('Ctrl Pts',(21.99966545674,14.8134928711808,9.01494709179358));
#129738=CARTESIAN_POINT('Ctrl Pts',(21.9923850702555,14.7520468335505,9.15778597991866));
#129739=CARTESIAN_POINT('Ctrl Pts',(21.985104683771,14.6840552228045,9.29782809214351));
#129740=CARTESIAN_POINT('Ctrl Pts',(21.9778242972865,14.6098038194187,9.43447708670711));
#129741=CARTESIAN_POINT('Origin',(26.8463464956315,10.1295,7.));
#129742=CARTESIAN_POINT('',(20.352563293369,14.6098038194187,9.43447708670712));
#129743=CARTESIAN_POINT('',(20.4776000250576,14.6098038194187,9.43447708670711));
#129744=CARTESIAN_POINT('',(26.8463464956315,14.6098038194187,9.43447708670711));
#129745=CARTESIAN_POINT('',(21.5963464956316,10.1298829051514,12.098999985623));
#129746=CARTESIAN_POINT('Ctrl Pts',(21.5963464956316,10.1298829051514,12.098999985623));
#129747=CARTESIAN_POINT('Ctrl Pts',(21.5886997577445,9.96656989073889,12.0990122494776));
#129748=CARTESIAN_POINT('Ctrl Pts',(21.5810530198574,9.80325714346398,12.0911738586918));
#129749=CARTESIAN_POINT('Ctrl Pts',(21.5734062819704,9.64065518488774,12.0755129540508));
#129750=CARTESIAN_POINT('Ctrl Pts',(21.5666845761133,9.49772331596717,12.0617465616352));
#129751=CARTESIAN_POINT('Ctrl Pts',(21.5599628702561,9.35531775886811,12.0419328173513));
#129752=CARTESIAN_POINT('Ctrl Pts',(21.553241164399,9.21397363696974,12.0161352133487));
#129753=CARTESIAN_POINT('Ctrl Pts',(21.5465211079346,9.07266419852288,11.9903439396408));
#129754=CARTESIAN_POINT('Ctrl Pts',(21.5398010514701,8.93241603785332,11.9585717981774));
#129755=CARTESIAN_POINT('Ctrl Pts',(21.5330809950056,8.79375579412643,11.9209336935662));
#129756=CARTESIAN_POINT('Ctrl Pts',(21.5263596207543,8.65506835945939,11.8832882082133));
#129757=CARTESIAN_POINT('Ctrl Pts',(21.5196382465029,8.51796982061406,11.8397745520151));
#129758=CARTESIAN_POINT('Ctrl Pts',(21.5129168722516,8.38297363001403,11.790558071764));
#129759=CARTESIAN_POINT('Ctrl Pts',(21.5061950124626,8.24796768757988,11.7413380362204));
#129760=CARTESIAN_POINT('Ctrl Pts',(21.4994731526736,8.11506473991455,11.6864144868448));
#129761=CARTESIAN_POINT('Ctrl Pts',(21.4927512928847,7.9847596072539,11.6260014751104));
#129762=CARTESIAN_POINT('Ctrl Pts',(21.4860249738077,7.85436803004691,11.5655483853277));
#129763=CARTESIAN_POINT('Ctrl Pts',(21.4792986547307,7.72657804372845,11.4995987153755));
#129764=CARTESIAN_POINT('Ctrl Pts',(21.4725723356537,7.60186164562879,11.4284134122179));
#129765=CARTESIAN_POINT('Ctrl Pts',(21.4674017694565,7.50599132118198,11.3736927963763));
#129766=CARTESIAN_POINT('Ctrl Pts',(21.4622312032594,7.41193676657903,11.3158793604137));
#129767=CARTESIAN_POINT('Ctrl Pts',(21.4570606370622,7.31990104245665,11.2551092462793));
#129768=CARTESIAN_POINT('Ctrl Pts',(21.4497821926166,7.19034522990356,11.1695650557955));
#129769=CARTESIAN_POINT('Ctrl Pts',(21.4425037481711,7.06471083663906,11.0781083746355));
#129770=CARTESIAN_POINT('Ctrl Pts',(21.4352253037255,6.94350501939066,10.9811100190188));
#129771=CARTESIAN_POINT('Ctrl Pts',(21.4279477400291,6.82231386900175,10.8841234009679));
#129772=CARTESIAN_POINT('Ctrl Pts',(21.4206701763327,6.70555042157178,10.7815966068709));
#129773=CARTESIAN_POINT('Ctrl Pts',(21.4133926126363,6.59368928068819,10.6739411477594));
#129774=CARTESIAN_POINT('Ctrl Pts',(21.4061193938006,6.48189492329082,10.5663499612524));
#129775=CARTESIAN_POINT('Ctrl Pts',(21.3988461749649,6.374997207616,10.4536364025609));
#129776=CARTESIAN_POINT('Ctrl Pts',(21.3915729561292,6.27343466828419,10.3362495646368));
#129777=CARTESIAN_POINT('Ctrl Pts',(21.3843045826288,6.17193978875607,10.2189409284834));
#129778=CARTESIAN_POINT('Ctrl Pts',(21.3770362091284,6.07577315665127,10.0969654188858));
#129779=CARTESIAN_POINT('Ctrl Pts',(21.369767835628,5.98533451912964,9.97080687140086));
#129780=CARTESIAN_POINT('Ctrl Pts',(21.362508451111,5.89500772938303,9.84480434741678));
#129781=CARTESIAN_POINT('Ctrl Pts',(21.3552490665939,5.81039493847136,9.71462931976104));
#129782=CARTESIAN_POINT('Ctrl Pts',(21.3479896820768,5.73185403598033,9.58079657763674));
#129783=CARTESIAN_POINT('Ctrl Pts',(21.3455647854359,5.70561853761555,9.53609160766829));
#129784=CARTESIAN_POINT('Ctrl Pts',(21.3431398887949,5.68006019676905,9.49097876732916));
#129785=CARTESIAN_POINT('Ctrl Pts',(21.340714992154,5.65519129922816,9.44547800035033));
#129786=CARTESIAN_POINT('Ctrl Pts',(21.3339842151457,5.58616278850139,9.31918168277893));
#129787=CARTESIAN_POINT('Ctrl Pts',(21.3272534381374,5.5224727999895,9.18993727191009));
#129788=CARTESIAN_POINT('Ctrl Pts',(21.320522661129,5.46436371111823,9.05822846306196));
#129789=CARTESIAN_POINT('Ctrl Pts',(21.3137921028903,5.4062565109596,8.92652393512921));
#129790=CARTESIAN_POINT('Ctrl Pts',(21.3070615446516,5.35372999568264,8.79235550376603));
#129791=CARTESIAN_POINT('Ctrl Pts',(21.300330986413,5.30697886832858,8.65622792350045));
#129792=CARTESIAN_POINT('Ctrl Pts',(21.2935969859559,5.26020383098292,8.52003072332438));
#129793=CARTESIAN_POINT('Ctrl Pts',(21.2868629854988,5.21921020433078,8.38187271779147));
#129794=CARTESIAN_POINT('Ctrl Pts',(21.2801289850417,5.18414331691862,8.24227544333062));
#129795=CARTESIAN_POINT('Ctrl Pts',(21.2733933187736,5.14906775489957,8.10264363625035));
#129796=CARTESIAN_POINT('Ctrl Pts',(21.2666576525055,5.11992193614123,7.96157220729983));
#129797=CARTESIAN_POINT('Ctrl Pts',(21.2599219862374,5.09680022375923,7.81959377878687));
#129798=CARTESIAN_POINT('Ctrl Pts',(21.2531800695621,5.07365705542761,7.67748360042942));
#129799=CARTESIAN_POINT('Ctrl Pts',(21.2464381528869,5.05654921504801,7.53446510332673));
#129800=CARTESIAN_POINT('Ctrl Pts',(21.2396962362117,5.04551934956642,7.39107767261366));
#129801=CARTESIAN_POINT('Ctrl Pts',(21.234587273223,5.03716101806671,7.28241998492099));
#129802=CARTESIAN_POINT('Ctrl Pts',(21.2294783102344,5.03229187939357,7.17355058473459));
#129803=CARTESIAN_POINT('Ctrl Pts',(21.2243693472458,5.03091055206464,7.06470426108234));
#129804=CARTESIAN_POINT('Ctrl Pts',(21.2176534134252,5.0290947426829,6.92162146563229));
#129805=CARTESIAN_POINT('Ctrl Pts',(21.2109374796046,5.03330466935425,6.77833298901328));
#129806=CARTESIAN_POINT('Ctrl Pts',(21.204221545784,5.04355373597305,6.63537471367122));
#129807=CARTESIAN_POINT('Ctrl Pts',(21.1975109705907,5.05379462488651,6.49253050438969));
#129808=CARTESIAN_POINT('Ctrl Pts',(21.1908003953973,5.0700650298353,6.35001633899631));
#129809=CARTESIAN_POINT('Ctrl Pts',(21.184089820204,5.092326300591,6.20836743246488));
#129810=CARTESIAN_POINT('Ctrl Pts',(21.177383231775,5.1145743458873,6.06680267979342));
#129811=CARTESIAN_POINT('Ctrl Pts',(21.170676643346,5.14280610952076,5.92610252631899));
#129812=CARTESIAN_POINT('Ctrl Pts',(21.163970054917,5.17693118965687,5.78679631602257));
#129813=CARTESIAN_POINT('Ctrl Pts',(21.1572660848589,5.21104294675723,5.64754449333819));
#129814=CARTESIAN_POINT('Ctrl Pts',(21.1505621148008,5.25104334803021,5.50968588807691));
#129815=CARTESIAN_POINT('Ctrl Pts',(21.1438581447427,5.29679107030568,5.37373882760094));
#129816=CARTESIAN_POINT('Ctrl Pts',(21.1371541064382,5.3425392582927,5.23779038318468));
#129817=CARTESIAN_POINT('Ctrl Pts',(21.1304500681338,5.39403477490237,5.10375387565751));
#129818=CARTESIAN_POINT('Ctrl Pts',(21.1237460298293,5.45108660716885,4.9721318766305));
#129819=CARTESIAN_POINT('Ctrl Pts',(21.1170416407376,5.50814142465893,4.8405029905136));
#129820=CARTESIAN_POINT('Ctrl Pts',(21.1103372516459,5.57075299036046,4.7112892041865));
#129821=CARTESIAN_POINT('Ctrl Pts',(21.1036328625542,5.63868250959758,4.58497220142382));
#129822=CARTESIAN_POINT('Ctrl Pts',(21.0969268835225,5.70662813826123,4.45862524269358));
#129823=CARTESIAN_POINT('Ctrl Pts',(21.0902209044908,5.77989405761444,4.33517676178452));
#129824=CARTESIAN_POINT('Ctrl Pts',(21.083514925459,5.85819603824447,4.21508286186258));
#129825=CARTESIAN_POINT('Ctrl Pts',(21.0768061164871,5.9365310625094,4.09493828200956));
#129826=CARTESIAN_POINT('Ctrl Pts',(21.0700973075152,6.01990617971834,3.97815141278116));
#129827=CARTESIAN_POINT('Ctrl Pts',(21.0633884985432,6.10799454326904,3.86514835096091));
#129828=CARTESIAN_POINT('Ctrl Pts',(21.0566717408833,6.19618727510909,3.75201140157848));
#129829=CARTESIAN_POINT('Ctrl Pts',(21.0499549832234,6.28910418051396,3.64266750672083));
#129830=CARTESIAN_POINT('Ctrl Pts',(21.0432382255635,6.38637840804699,3.53750931440167));
#129831=CARTESIAN_POINT('Ctrl Pts',(21.0365170846755,6.48371611488792,3.43228249784938));
#129832=CARTESIAN_POINT('Ctrl Pts',(21.0297959437875,6.58541655150024,3.33124709056119));
#129833=CARTESIAN_POINT('Ctrl Pts',(21.0230748028994,6.69107726063957,3.23475763523128));
#129834=CARTESIAN_POINT('Ctrl Pts',(21.0163437401092,6.79689394853999,3.13812573995541));
#129835=CARTESIAN_POINT('Ctrl Pts',(21.0096126773189,6.90668230663511,3.04605344237268));
#129836=CARTESIAN_POINT('Ctrl Pts',(21.0028816145286,7.02000750204106,2.95885444395564));
#129837=CARTESIAN_POINT('Ctrl Pts',(20.9991470954955,7.08288243165579,2.91047481515106));
#129838=CARTESIAN_POINT('Ctrl Pts',(20.9954125764625,7.14684556635783,2.86359453102167));
#129839=CARTESIAN_POINT('Ctrl Pts',(20.9916780574294,7.21181912996737,2.81826120607161));
#129840=CARTESIAN_POINT('Ctrl Pts',(20.9851848545906,7.32478857099484,2.73944021958085));
#129841=CARTESIAN_POINT('Ctrl Pts',(20.9786916517519,7.44117320825419,2.66504792986056));
#129842=CARTESIAN_POINT('Ctrl Pts',(20.9721984489131,7.5605842685465,2.59540320066743));
#129843=CARTESIAN_POINT('Ctrl Pts',(20.9657137060064,7.67983974930792,2.52584921092733));
#129844=CARTESIAN_POINT('Ctrl Pts',(20.9592289630997,7.80211347051053,2.46103068201201));
#129845=CARTESIAN_POINT('Ctrl Pts',(20.9527442201929,7.92698482267687,2.40122539216573));
#129846=CARTESIAN_POINT('Ctrl Pts',(20.9462662847788,8.05172508856619,2.34148288415577));
#129847=CARTESIAN_POINT('Ctrl Pts',(20.9397883493646,8.17905720344274,2.28674332075701));
#129848=CARTESIAN_POINT('Ctrl Pts',(20.9333104139505,8.30853331594534,2.23724015558595));
#129849=CARTESIAN_POINT('Ctrl Pts',(20.9268376417297,8.4379062304142,2.18777644656792));
#129850=CARTESIAN_POINT('Ctrl Pts',(20.9203648695088,8.56941937043855,2.14354097624593));
#129851=CARTESIAN_POINT('Ctrl Pts',(20.913892097288,8.70260256867763,2.10472015912414));
#129852=CARTESIAN_POINT('Ctrl Pts',(20.9074222385477,8.83572581939468,2.06591681576646));
#129853=CARTESIAN_POINT('Ctrl Pts',(20.9009523798074,8.97051725008775,2.0325233937257));
#129854=CARTESIAN_POINT('Ctrl Pts',(20.8944825210671,9.10648943525271,2.00467714913086));
#129855=CARTESIAN_POINT('Ctrl Pts',(20.8880140950404,9.24243151014611,1.97683707092942));
#129856=CARTESIAN_POINT('Ctrl Pts',(20.8815456690137,9.37955342700358,1.95454180910562));
#129857=CARTESIAN_POINT('Ctrl Pts',(20.8750772429871,9.51735593402644,1.93787785187938));
#129858=CARTESIAN_POINT('Ctrl Pts',(20.8686087712671,9.65515941449231,1.9212137769382));
#129859=CARTESIAN_POINT('Ctrl Pts',(20.8621402995472,9.79364309633967,1.91018113416146));
#129860=CARTESIAN_POINT('Ctrl Pts',(20.8556718278273,9.93230148100156,1.90481465066237));
#129861=CARTESIAN_POINT('Ctrl Pts',(20.8492018320787,10.0709925347955,1.89944690277268));
#129862=CARTESIAN_POINT('Ctrl Pts',(20.8427318363301,10.2098579723973,1.89974798431359));
#129863=CARTESIAN_POINT('Ctrl Pts',(20.8362618405815,10.348391704133,1.90570049743228));
#129864=CARTESIAN_POINT('Ctrl Pts',(20.8297845845163,10.4870808917277,1.91165969017352));
#129865=CARTESIAN_POINT('Ctrl Pts',(20.8233073284511,10.6254372286438,1.92328296238145));
#129866=CARTESIAN_POINT('Ctrl Pts',(20.8168300723859,10.7629587075596,1.94050090761774));
#129867=CARTESIAN_POINT('Ctrl Pts',(20.8103491685813,10.9005576332404,1.95772854933322));
#129868=CARTESIAN_POINT('Ctrl Pts',(20.8038682647766,11.0373203698811,1.98055707009204));
#129869=CARTESIAN_POINT('Ctrl Pts',(20.797387360972,11.1727557922092,2.00886602543851));
#129870=CARTESIAN_POINT('Ctrl Pts',(20.7908954455442,11.3084213311811,2.03722308017937));
#129871=CARTESIAN_POINT('Ctrl Pts',(20.7844035301164,11.4427546621861,2.07107907258841));
#129872=CARTESIAN_POINT('Ctrl Pts',(20.7779116146886,11.5752797124002,2.1102636039136));
#129873=CARTESIAN_POINT('Ctrl Pts',(20.77160333233,11.704056102916,2.14833974499001));
#129874=CARTESIAN_POINT('Ctrl Pts',(20.7652950499715,11.8311248479618,2.1914468562064));
#129875=CARTESIAN_POINT('Ctrl Pts',(20.758986767613,11.956069933585,2.23938624989138));
#129876=CARTESIAN_POINT('Ctrl Pts',(20.752255350081,12.089395852133,2.29054123262481));
#129877=CARTESIAN_POINT('Ctrl Pts',(20.7455239325489,12.2207429681633,2.34736702175228));
#129878=CARTESIAN_POINT('Ctrl Pts',(20.7387925150168,12.3496051713782,2.40969129273208));
#129879=CARTESIAN_POINT('Ctrl Pts',(20.7320693455013,12.4783094795322,2.47193919768429));
#129880=CARTESIAN_POINT('Ctrl Pts',(20.7253461759858,12.604534607748,2.53967200821282));
#129881=CARTESIAN_POINT('Ctrl Pts',(20.7186230064702,12.7277927942082,2.61266874335141));
#129882=CARTESIAN_POINT('Ctrl Pts',(20.7119067023597,12.8509251148298,2.68559093743474));
#129883=CARTESIAN_POINT('Ctrl Pts',(20.7051903982492,12.9710962113983,2.7637661629336));
#129884=CARTESIAN_POINT('Ctrl Pts',(20.6984740941386,13.0878414666366,2.84692682862695));
#129885=CARTESIAN_POINT('Ctrl Pts',(20.691763278558,13.2044913182398,2.93001953584278));
#129886=CARTESIAN_POINT('Ctrl Pts',(20.6850524629774,13.3177206051619,3.01808935397584));
#129887=CARTESIAN_POINT('Ctrl Pts',(20.6783416473968,13.427092417135,3.11082460533681));
#129888=CARTESIAN_POINT('Ctrl Pts',(20.6716350714244,13.5363951326426,3.20350127050457));
#129889=CARTESIAN_POINT('Ctrl Pts',(20.6649284954521,13.6418449478012,3.30083725726319));
#129890=CARTESIAN_POINT('Ctrl Pts',(20.6582219194797,13.7430369628603,3.40247979602026));
#129891=CARTESIAN_POINT('Ctrl Pts',(20.6515176619563,13.8441939960568,3.50408719716967));
#129892=CARTESIAN_POINT('Ctrl Pts',(20.6448134044329,13.9410958999718,3.60999792371146));
#129893=CARTESIAN_POINT('Ctrl Pts',(20.6381091469095,14.0333736471028,3.71982141531038));
#129894=CARTESIAN_POINT('Ctrl Pts',(20.6314059678938,14.1256365495977,3.82962723970549));
#129895=CARTESIAN_POINT('Ctrl Pts',(20.6247027888781,14.2132765396375,3.94334429217381));
#129896=CARTESIAN_POINT('Ctrl Pts',(20.6179996098624,14.2959640876569,4.060548009192));
#129897=CARTESIAN_POINT('Ctrl Pts',(20.6112962704155,14.378653614687,4.17775453131697));
#129898=CARTESIAN_POINT('Ctrl Pts',(20.6045929309686,14.456390251492,4.29844758149486));
#129899=CARTESIAN_POINT('Ctrl Pts',(20.5978895915217,14.5288871829675,4.42217273380445));
#129900=CARTESIAN_POINT('Ctrl Pts',(20.5911823410669,14.6014264121778,4.54597007253031));
#129901=CARTESIAN_POINT('Ctrl Pts',(20.5844750906121,14.668719640705,4.67280272880459));
#129902=CARTESIAN_POINT('Ctrl Pts',(20.5777678401573,14.7305252782473,4.80219032013015));
#129903=CARTESIAN_POINT('Ctrl Pts',(20.5710585028671,14.7923501454557,4.93161816798048));
#129904=CARTESIAN_POINT('Ctrl Pts',(20.564349165577,14.8486838674656,5.06360219779874));
#129905=CARTESIAN_POINT('Ctrl Pts',(20.5576398282869,14.8993327590442,5.19764142004176));
#129906=CARTESIAN_POINT('Ctrl Pts',(20.5509240694714,14.9500301268172,5.33180893159575));
#129907=CARTESIAN_POINT('Ctrl Pts',(20.544208310656,14.9950316728671,5.4680352158438));
#129908=CARTESIAN_POINT('Ctrl Pts',(20.5374925518406,15.0341932052633,5.60580289691735));
#129909=CARTESIAN_POINT('Ctrl Pts',(20.5337601938259,15.055957664548,5.68236882531709));
#129910=CARTESIAN_POINT('Ctrl Pts',(20.5300278358113,15.0759192163065,5.75941061027489));
#129911=CARTESIAN_POINT('Ctrl Pts',(20.5262954777967,15.0940599329618,5.83683807144917));
#129912=CARTESIAN_POINT('Ctrl Pts',(20.5195531565522,15.1268302456745,5.97670697318204));
#129913=CARTESIAN_POINT('Ctrl Pts',(20.5128108353077,15.1537122172889,6.11807599491532));
#129914=CARTESIAN_POINT('Ctrl Pts',(20.5060685140632,15.174579088646,6.26042039691011));
#129915=CARTESIAN_POINT('Ctrl Pts',(20.4993310938359,15.1954307918007,6.40266132825656));
#129916=CARTESIAN_POINT('Ctrl Pts',(20.4925936736085,15.210276051231,6.54587586687352));
#129917=CARTESIAN_POINT('Ctrl Pts',(20.4858562533812,15.2190391491384,6.68952898784726));
#129918=CARTESIAN_POINT('Ctrl Pts',(20.4791225787158,15.2277973753404,6.83310224714431));
#129919=CARTESIAN_POINT('Ctrl Pts',(20.4723889040505,15.2304801549966,6.97711323862747));
#129920=CARTESIAN_POINT('Ctrl Pts',(20.4656552293852,15.2270636067672,7.12102179540484));
#129921=CARTESIAN_POINT('Ctrl Pts',(20.4589238948687,15.2236482458881,7.26488033975022));
#129922=CARTESIAN_POINT('Ctrl Pts',(20.4521925603523,15.2141377896593,7.40863615508474));
#129923=CARTESIAN_POINT('Ctrl Pts',(20.4454612258358,15.1985604617482,7.5517490689985));
#129924=CARTESIAN_POINT('Ctrl Pts',(20.4387300007792,15.1829833871439,7.69485965571826));
#129925=CARTESIAN_POINT('Ctrl Pts',(20.4319987757226,15.1613396706609,7.83732699762378));
#129926=CARTESIAN_POINT('Ctrl Pts',(20.425267550666,15.1337094284331,7.97861585741374));
#129927=CARTESIAN_POINT('Ctrl Pts',(20.4201616447402,15.1127507743489,8.08578916099432));
#129928=CARTESIAN_POINT('Ctrl Pts',(20.4150557388143,15.0883486417902,8.19228444747359));
#129929=CARTESIAN_POINT('Ctrl Pts',(20.4099498328885,15.0605576408463,8.2978719284471));
#129930=CARTESIAN_POINT('Ctrl Pts',(20.4026905362803,15.0210459220998,8.44799040959878));
#129931=CARTESIAN_POINT('Ctrl Pts',(20.3954312396722,14.9746971733673,8.59621860003053));
#129932=CARTESIAN_POINT('Ctrl Pts',(20.3881719430641,14.9217188865059,8.74196416260962));
#129933=CARTESIAN_POINT('Ctrl Pts',(20.3809028745946,14.868669284681,8.88790591574319));
#129934=CARTESIAN_POINT('Ctrl Pts',(20.3736338061251,14.8089723919441,9.03135812139184));
#129935=CARTESIAN_POINT('Ctrl Pts',(20.3663647376557,14.7428843972005,9.17174708556652));
#129936=CARTESIAN_POINT('Ctrl Pts',(20.3617642562268,14.7010583236443,9.26059709780911));
#129937=CARTESIAN_POINT('Ctrl Pts',(20.3571637747979,14.6566732928353,9.34822058344851));
#129938=CARTESIAN_POINT('Ctrl Pts',(20.352563293369,14.6098038194187,9.43447708670712));
#129939=CARTESIAN_POINT('Ctrl Pts',(21.8525208814298,14.6095924811794,9.43436249769606));
#129940=CARTESIAN_POINT('Ctrl Pts',(21.8370464448822,14.4519305706909,9.72490119905027));
#129941=CARTESIAN_POINT('Ctrl Pts',(21.7827901266984,13.8010022388993,10.6901681055195));
#129942=CARTESIAN_POINT('Ctrl Pts',(21.6973986661381,12.2874582761103,11.804511236185));
#129943=CARTESIAN_POINT('Ctrl Pts',(21.6274816421253,10.7948600303933,12.0984964626806));
#129944=CARTESIAN_POINT('Ctrl Pts',(21.5963464997487,10.1298830029783,12.0991317633798));
#129945=CARTESIAN_POINT('',(21.7216535043236,10.1294562983577,12.0989999998127));
#129946=CARTESIAN_POINT('Ctrl Pts',(21.9778242972865,14.6098038194187,9.43447708670711));
#129947=CARTESIAN_POINT('Ctrl Pts',(21.9708912000632,14.5390943591803,9.5646076459575));
#129948=CARTESIAN_POINT('Ctrl Pts',(21.9639581028398,14.462708632086,9.69166097956588));
#129949=CARTESIAN_POINT('Ctrl Pts',(21.9570250056164,14.3809405674658,9.81514726103373));
#129950=CARTESIAN_POINT('Ctrl Pts',(21.9500922255905,14.2991762438321,9.9386278928569));
#129951=CARTESIAN_POINT('Ctrl Pts',(21.9431594455646,14.2120302589396,10.0585415242968));
#129952=CARTESIAN_POINT('Ctrl Pts',(21.9362266655387,14.1198398936231,10.1744272764327));
#129953=CARTESIAN_POINT('Ctrl Pts',(21.9292924040556,14.0276298282607,10.2903377920526));
#129954=CARTESIAN_POINT('Ctrl Pts',(21.9223581425725,13.9303734348502,10.4022184502355));
#129955=CARTESIAN_POINT('Ctrl Pts',(21.9154238810893,13.8284486805062,10.5096409586995));
#129956=CARTESIAN_POINT('Ctrl Pts',(21.9120029111546,13.7781648080188,10.5626371101512));
#129957=CARTESIAN_POINT('Ctrl Pts',(21.9085819412199,13.7267453168927,10.6145487329785));
#129958=CARTESIAN_POINT('Ctrl Pts',(21.9051609712852,13.6742389692849,10.6653276305991));
#129959=CARTESIAN_POINT('Ctrl Pts',(21.8982288511239,13.5678421526517,10.7682240098965));
#129960=CARTESIAN_POINT('Ctrl Pts',(21.8912967309625,13.4569435049872,10.8665024520393));
#129961=CARTESIAN_POINT('Ctrl Pts',(21.8843646108012,13.3419664401948,10.959780343734));
#129962=CARTESIAN_POINT('Ctrl Pts',(21.877433811209,13.2270112785383,11.0530404659862));
#129963=CARTESIAN_POINT('Ctrl Pts',(21.8705030116169,13.1079795066484,11.1413017300309));
#129964=CARTESIAN_POINT('Ctrl Pts',(21.8635722120248,12.9853276996924,11.2242217211777));
#129965=CARTESIAN_POINT('Ctrl Pts',(21.8566411598445,12.8626714227769,11.3071447342857));
#129966=CARTESIAN_POINT('Ctrl Pts',(21.8497101076642,12.7363951190217,11.3847258969099));
#129967=CARTESIAN_POINT('Ctrl Pts',(21.8427790554839,12.6069848824144,11.4566657556304));
#129968=CARTESIAN_POINT('Ctrl Pts',(21.8358483702673,12.4775814974174,11.5286018055031));
#129969=CARTESIAN_POINT('Ctrl Pts',(21.8289176850508,12.3450448012554,11.5948969892324));
#129970=CARTESIAN_POINT('Ctrl Pts',(21.8219869998343,12.209886058069,11.6552975038543));
#129971=CARTESIAN_POINT('Ctrl Pts',(21.8150547479171,12.0746967618723,11.7157116721808));
#129972=CARTESIAN_POINT('Ctrl Pts',(21.8081224959998,11.9368845365065,11.7702283738594));
#129973=CARTESIAN_POINT('Ctrl Pts',(21.8011902440826,11.7969818008886,11.8186414520802));
#129974=CARTESIAN_POINT('Ctrl Pts',(21.7970652715141,11.713733968355,11.847449207771));
#129975=CARTESIAN_POINT('Ctrl Pts',(21.7929402989456,11.6297463168938,11.8740967543871));
#129976=CARTESIAN_POINT('Ctrl Pts',(21.788815326377,11.5451338329821,11.8985489536103));
#129977=CARTESIAN_POINT('Ctrl Pts',(21.781841763805,11.4020903481749,11.939887153677));
#129978=CARTESIAN_POINT('Ctrl Pts',(21.7748682012329,11.2572131443299,11.9749619273583));
#129979=CARTESIAN_POINT('Ctrl Pts',(21.7678946386609,11.1110621236963,12.0036323603283));
#129980=CARTESIAN_POINT('Ctrl Pts',(21.7609226052006,10.9649431499895,12.0322965066555));
#129981=CARTESIAN_POINT('Ctrl Pts',(21.7539505717403,10.8175512332713,12.0545590528571));
#129982=CARTESIAN_POINT('Ctrl Pts',(21.7469785382801,10.669456698842,12.0703301434301));
#129983=CARTESIAN_POINT('Ctrl Pts',(21.7400073493926,10.5213801041739,12.0860993235369));
#129984=CARTESIAN_POINT('Ctrl Pts',(21.7330361605051,10.3726013821705,12.0953785825651));
#129985=CARTESIAN_POINT('Ctrl Pts',(21.7260649716176,10.2236966737367,12.0981298518826));
#129986=CARTESIAN_POINT('Ctrl Pts',(21.7245944825346,10.192287002918,12.0987101993042));
#129987=CARTESIAN_POINT('Ctrl Pts',(21.7231239934515,10.1608717378449,12.0990002690569));
#129988=CARTESIAN_POINT('Ctrl Pts',(21.7216535043684,10.1294562993151,12.0989999998127));
#129989=CARTESIAN_POINT('Ctrl Pts',(21.7216535043236,10.1294562983577,12.0989999998127));
#129990=CARTESIAN_POINT('Ctrl Pts',(21.7145780823896,9.97829741836422,12.0989987042859));
#129991=CARTESIAN_POINT('Ctrl Pts',(21.7075026604556,9.8271603213621,12.092271455827));
#129992=CARTESIAN_POINT('Ctrl Pts',(21.7004272385216,9.67663880551781,12.0788500409573));
#129993=CARTESIAN_POINT('Ctrl Pts',(21.6933497400828,9.52607311440785,12.065424687152));
#129994=CARTESIAN_POINT('Ctrl Pts',(21.686272241644,9.37612366434497,12.0453012699465));
#129995=CARTESIAN_POINT('Ctrl Pts',(21.6791947432053,9.22737926268248,12.0185634573353));
#129996=CARTESIAN_POINT('Ctrl Pts',(21.6769530559598,9.18026679336472,12.0100946722101));
#129997=CARTESIAN_POINT('Ctrl Pts',(21.6747113687143,9.13327515566229,12.0009627140914));
#129998=CARTESIAN_POINT('Ctrl Pts',(21.6724696814689,9.08642286948864,11.9911713154133));
#129999=CARTESIAN_POINT('Ctrl Pts',(21.6655384929631,8.94155786744673,11.960896784428));
#130000=CARTESIAN_POINT('Ctrl Pts',(21.6586073044574,8.79798658804774,11.9243058365266));
#130001=CARTESIAN_POINT('Ctrl Pts',(21.6516761159517,8.65626323121066,11.8815340235511));
#130002=CARTESIAN_POINT('Ctrl Pts',(21.64474624141,8.51456674125142,11.8387703189433));
#130003=CARTESIAN_POINT('Ctrl Pts',(21.6378163668684,8.37471779167141,11.7898281825944));
#130004=CARTESIAN_POINT('Ctrl Pts',(21.6308864923267,8.2372559332038,11.7348931763742));
#130005=CARTESIAN_POINT('Ctrl Pts',(21.6239563464653,8.09978869280394,11.6799560193284));
#130006=CARTESIAN_POINT('Ctrl Pts',(21.6170262006039,7.9647090391401,11.6190256426999));
#130007=CARTESIAN_POINT('Ctrl Pts',(21.6100960547425,7.83253754293167,11.5523361552964));
#130008=CARTESIAN_POINT('Ctrl Pts',(21.6031662631196,7.70037280274875,11.4856500767661));
#130009=CARTESIAN_POINT('Ctrl Pts',(21.5962364714968,7.57111621763294,11.4132056266103));
#130010=CARTESIAN_POINT('Ctrl Pts',(21.5893066798739,7.44526470784607,11.3352833697874));
#130011=CARTESIAN_POINT('Ctrl Pts',(21.5823752942246,7.31938424904482,11.2573431888844));
#130012=CARTESIAN_POINT('Ctrl Pts',(21.5754439085753,7.19691071214243,11.1739228579809));
#130013=CARTESIAN_POINT('Ctrl Pts',(21.568512522926,7.07831346210215,11.0853471958881));
#130014=CARTESIAN_POINT('Ctrl Pts',(21.5643830274709,7.00765705517126,11.0325766803587));
#130015=CARTESIAN_POINT('Ctrl Pts',(21.5602535320158,6.9383759408189,10.9779771655619));
#130016=CARTESIAN_POINT('Ctrl Pts',(21.5561240365606,6.87056406102977,10.9216243504048));
#130017=CARTESIAN_POINT('Ctrl Pts',(21.5491919803161,6.75673035668187,10.8270266232852));
#130018=CARTESIAN_POINT('Ctrl Pts',(21.5422599240716,6.64699821171827,10.7274524655712));
#130019=CARTESIAN_POINT('Ctrl Pts',(21.5353278678271,6.54179397638852,10.6232811770744));
#130020=CARTESIAN_POINT('Ctrl Pts',(21.5283971552673,6.43661013346749,10.5191300807637));
#130021=CARTESIAN_POINT('Ctrl Pts',(21.5214664427075,6.33595268411619,10.4103838641845));
#130022=CARTESIAN_POINT('Ctrl Pts',(21.5145357301477,6.24021162379281,10.297459162249));
#130023=CARTESIAN_POINT('Ctrl Pts',(21.5076047985457,6.14446753761436,10.1845308913768));
#130024=CARTESIAN_POINT('Ctrl Pts',(21.5006738669437,6.05364036800616,10.0674241210261));
#130025=CARTESIAN_POINT('Ctrl Pts',(21.4937429353417,5.96808061140313,9.94658949842187));
#130026=CARTESIAN_POINT('Ctrl Pts',(21.4868123893406,5.88252561489794,9.82576159842469));
#130027=CARTESIAN_POINT('Ctrl Pts',(21.4798818433394,5.80223763552051,9.7012065317229));
#130028=CARTESIAN_POINT('Ctrl Pts',(21.4729512973382,5.72752452675666,9.57340492984763));
#130029=CARTESIAN_POINT('Ctrl Pts',(21.4660192119694,5.65279482320388,9.44557494151323));
#130030=CARTESIAN_POINT('Ctrl Pts',(21.4590871266005,5.58364263152974,9.31449726290405));
#130031=CARTESIAN_POINT('Ctrl Pts',(21.4521550412316,5.5203307404732,9.18067873310885));
#130032=CARTESIAN_POINT('Ctrl Pts',(21.4480294913719,5.48265140599206,9.10103819387072));
#130033=CARTESIAN_POINT('Ctrl Pts',(21.4439039415122,5.44703976938654,9.02042734711839));
#130034=CARTESIAN_POINT('Ctrl Pts',(21.4397783916525,5.41354327869334,8.93895673050291));
#130035=CARTESIAN_POINT('Ctrl Pts',(21.4328288078177,5.35711766800913,8.8017175988741));
#130036=CARTESIAN_POINT('Ctrl Pts',(21.425879223983,5.3066782204933,8.66199295346232));
#130037=CARTESIAN_POINT('Ctrl Pts',(21.4189296401482,5.26242423305924,8.52032051846249));
#130038=CARTESIAN_POINT('Ctrl Pts',(21.4119812825149,5.21817805390603,8.37867308049059));
#130039=CARTESIAN_POINT('Ctrl Pts',(21.4050329248816,5.18011525469409,8.23507885105442));
#130040=CARTESIAN_POINT('Ctrl Pts',(21.3980845672483,5.14838550186882,8.09009144410335));
#130041=CARTESIAN_POINT('Ctrl Pts',(21.3911359899612,5.11665474599245,7.94509945376403));
#130042=CARTESIAN_POINT('Ctrl Pts',(21.3841874126742,5.09125751019233,7.79871451694216));
#130043=CARTESIAN_POINT('Ctrl Pts',(21.3772388353872,5.07229262147526,7.6515017502624));
#130044=CARTESIAN_POINT('Ctrl Pts',(21.3702906875388,5.05332890483344,7.50429808168186));
#130045=CARTESIAN_POINT('Ctrl Pts',(21.3633425396903,5.04079678109596,7.35626701042103));
#130046=CARTESIAN_POINT('Ctrl Pts',(21.3563943918419,5.03474335699634,7.20798016388597));
#130047=CARTESIAN_POINT('Ctrl Pts',(21.3494449282258,5.02868878656242,7.05966523633523));
#130048=CARTESIAN_POINT('Ctrl Pts',(21.3424954646096,5.02911538076994,6.91109476395886));
#130049=CARTESIAN_POINT('Ctrl Pts',(21.3355460009934,5.03601815715149,6.76284242248547));
#130050=CARTESIAN_POINT('Ctrl Pts',(21.331508249577,5.04002878252507,6.67670540028748));
#130051=CARTESIAN_POINT('Ctrl Pts',(21.3274704981606,5.04622466346145,6.59067577933083));
#130052=CARTESIAN_POINT('Ctrl Pts',(21.3234327467442,5.0545967490254,6.50486568161013));
#130053=CARTESIAN_POINT('Ctrl Pts',(21.31655060643,5.06886653971637,6.35860676866734));
#130054=CARTESIAN_POINT('Ctrl Pts',(21.3096684661157,5.08946675265018,6.21293115702204));
#130055=CARTESIAN_POINT('Ctrl Pts',(21.3027863258014,5.11632565505071,6.06839708719742));
#130056=CARTESIAN_POINT('Ctrl Pts',(21.2959056901371,5.14317868525947,5.92389461701757));
#130057=CARTESIAN_POINT('Ctrl Pts',(21.2890250544729,5.17628761360455,5.78053352530322));
#130058=CARTESIAN_POINT('Ctrl Pts',(21.2821444188086,5.21552937377503,5.63886309116306));
#130059=CARTESIAN_POINT('Ctrl Pts',(21.2752633519625,5.25477359306887,5.49718377910633));
#130060=CARTESIAN_POINT('Ctrl Pts',(21.2683822851165,5.30015132574767,5.35719566559861));
#130061=CARTESIAN_POINT('Ctrl Pts',(21.2615012182705,5.35148915214393,5.21943454549694));
#130062=CARTESIAN_POINT('Ctrl Pts',(21.2546203142567,5.4028257636912,5.08167668534937));
#130063=CARTESIAN_POINT('Ctrl Pts',(21.247739410243,5.46012206546334,4.946146031246));
#130064=CARTESIAN_POINT('Ctrl Pts',(21.2408585062293,5.52315589001064,4.81335989692717));
#130065=CARTESIAN_POINT('Ctrl Pts',(21.2339753023867,5.58621078257564,4.68052938102991));
#130066=CARTESIAN_POINT('Ctrl Pts',(21.2270920985441,5.65500688289976,4.55044552515016));
#130067=CARTESIAN_POINT('Ctrl Pts',(21.2202088947016,5.72927504815719,4.42360302492416));
#130068=CARTESIAN_POINT('Ctrl Pts',(21.2158349637464,5.7764687437722,4.34300097523082));
#130069=CARTESIAN_POINT('Ctrl Pts',(21.2114610327912,5.82587110691438,4.26370729362511));
#130070=CARTESIAN_POINT('Ctrl Pts',(21.2070871018361,5.87740373338063,4.1858432276432));
#130071=CARTESIAN_POINT('Ctrl Pts',(21.2000240344735,5.96061913294572,4.060107556734));
#130072=CARTESIAN_POINT('Ctrl Pts',(21.1929609671109,6.04941838500955,3.93806054204195));
#130073=CARTESIAN_POINT('Ctrl Pts',(21.1858978997482,6.14345469960175,3.820181787716));
#130074=CARTESIAN_POINT('Ctrl Pts',(21.178835666965,6.23747990276482,3.70231696206676));
#130075=CARTESIAN_POINT('Ctrl Pts',(21.1717734341818,6.33674074326747,3.58861965076045));
#130076=CARTESIAN_POINT('Ctrl Pts',(21.1647112013986,6.44084960845913,3.4795370632564));
#130077=CARTESIAN_POINT('Ctrl Pts',(21.1576495020065,6.54495061059453,3.37046271446018));
#130078=CARTESIAN_POINT('Ctrl Pts',(21.1505878026143,6.65389869778801,3.26600261454694));
#130079=CARTESIAN_POINT('Ctrl Pts',(21.1435261032221,6.76726836629837,3.16656819007615));
#130080=CARTESIAN_POINT('Ctrl Pts',(21.1364656539791,6.88061796471118,3.06715136871406));
#130081=CARTESIAN_POINT('Ctrl Pts',(21.129405204736,6.99838735271096,2.97275864623127));
#130082=CARTESIAN_POINT('Ctrl Pts',(21.122344755493,7.12011654019953,2.88376237422092));
#130083=CARTESIAN_POINT('Ctrl Pts',(21.1152853450695,7.24182781740339,2.794779196429));
#130084=CARTESIAN_POINT('Ctrl Pts',(21.108225934646,7.36749748609508,2.71119106380588));
#130085=CARTESIAN_POINT('Ctrl Pts',(21.1011665242225,7.4966345737675,2.6333284246065));
#130086=CARTESIAN_POINT('Ctrl Pts',(21.097691501791,7.56020281098323,2.5950002354853));
#130087=CARTESIAN_POINT('Ctrl Pts',(21.0942164793594,7.62461079760845,2.55805875715));
#130088=CARTESIAN_POINT('Ctrl Pts',(21.0907414569279,7.68979747601854,2.52253949269471));
#130089=CARTESIAN_POINT('Ctrl Pts',(21.0840196099996,7.81589015100785,2.45383344449506));
#130090=CARTESIAN_POINT('Ctrl Pts',(21.0772977630712,7.9449362626361,2.39043095335399));
#130091=CARTESIAN_POINT('Ctrl Pts',(21.0705759161429,8.07645702253597,2.33257934907452));
#130092=CARTESIAN_POINT('Ctrl Pts',(21.0638557183066,8.20794551603063,2.27474193771263));
#130093=CARTESIAN_POINT('Ctrl Pts',(21.0571355204702,8.34190711156151,2.22245284749552));
#130094=CARTESIAN_POINT('Ctrl Pts',(21.0504153226339,8.47784123377184,2.17591207377585));
#130095=CARTESIAN_POINT('Ctrl Pts',(21.0436938073277,8.61380200536455,2.12936217590945));
#130096=CARTESIAN_POINT('Ctrl Pts',(21.0369722920214,8.75173573007874,2.08856297103887));
#130097=CARTESIAN_POINT('Ctrl Pts',(21.0302507767151,8.89112448377531,2.05366528823461));
#130098=CARTESIAN_POINT('Ctrl Pts',(21.0235287760831,9.03052330201039,2.01876508564978));
#130099=CARTESIAN_POINT('Ctrl Pts',(21.0168067754511,9.17137700030015,1.98976733838324));
#130100=CARTESIAN_POINT('Ctrl Pts',(21.0100847748191,9.31315578902763,1.96677209643634));
#130101=CARTESIAN_POINT('Ctrl Pts',(21.0033583161372,9.45502860584993,1.94376160397975));
#130102=CARTESIAN_POINT('Ctrl Pts',(20.9966318574553,9.59782737480171,1.92676162587731));
#130103=CARTESIAN_POINT('Ctrl Pts',(20.9899053987734,9.74101492534841,1.91582058275154));
#130104=CARTESIAN_POINT('Ctrl Pts',(20.9847355365222,9.85106687800675,1.90741144972626));
#130105=CARTESIAN_POINT('Ctrl Pts',(20.9795656742709,9.96134831898086,1.90258042790854));
#130106=CARTESIAN_POINT('Ctrl Pts',(20.9743958120197,10.071614880693,1.90132857373974));
#130107=CARTESIAN_POINT('Ctrl Pts',(20.9671175717702,10.2268504534471,1.89956618724759));
#130108=CARTESIAN_POINT('Ctrl Pts',(20.9598393315207,10.38215201505,1.90489782475772));
#130109=CARTESIAN_POINT('Ctrl Pts',(20.9525610912711,10.5368917561104,1.91730062299045));
#130110=CARTESIAN_POINT('Ctrl Pts',(20.9452837330259,10.6916127452311,1.92970191820577));
#130111=CARTESIAN_POINT('Ctrl Pts',(20.9380063747807,10.8457717972154,1.94917264147978));
#130112=CARTESIAN_POINT('Ctrl Pts',(20.9307290165355,10.998745255065,1.97563798213674));
#130113=CARTESIAN_POINT('Ctrl Pts',(20.9234560005045,11.1516274375505,2.00208753159934));
#130114=CARTESIAN_POINT('Ctrl Pts',(20.9161829844736,11.3033251896582,2.03552331724142));
#130115=CARTESIAN_POINT('Ctrl Pts',(20.9089099684426,11.4532236629269,2.07581918851396));
#130116=CARTESIAN_POINT('Ctrl Pts',(20.9016417943633,11.6030223424974,2.11608823313558));
#130117=CARTESIAN_POINT('Ctrl Pts',(20.894373620284,11.7510238897501,2.16320818147162));
#130118=CARTESIAN_POINT('Ctrl Pts',(20.8871054462047,11.8966261080614,2.21700237108486));
#130119=CARTESIAN_POINT('Ctrl Pts',(20.8798462532636,12.0420484086068,2.27073008828768));
#130120=CARTESIAN_POINT('Ctrl Pts',(20.8725870603225,12.1850770620086,2.33111549332836));
#130121=CARTESIAN_POINT('Ctrl Pts',(20.8653278673814,12.3251271892484,2.39793282906112));
#130122=CARTESIAN_POINT('Ctrl Pts',(20.8629019672915,12.3719295843671,2.42026205795495));
#130123=CARTESIAN_POINT('Ctrl Pts',(20.8604760672015,12.4183994834494,2.44330918750438));
#130124=CARTESIAN_POINT('Ctrl Pts',(20.8580501671115,12.4645155072712,2.46706457350171));
#130125=CARTESIAN_POINT('Ctrl Pts',(20.851319308004,12.5924682041796,2.53297584365391));
#130126=CARTESIAN_POINT('Ctrl Pts',(20.8445884488965,12.7176517637429,2.60432077926021));
#130127=CARTESIAN_POINT('Ctrl Pts',(20.8378575897889,12.8395943566171,2.68083462018041));
#130128=CARTESIAN_POINT('Ctrl Pts',(20.8311269491109,12.9615329922165,2.75734597807738));
#130129=CARTESIAN_POINT('Ctrl Pts',(20.8243963084329,13.0802305615075,2.8390257118703));
#130130=CARTESIAN_POINT('Ctrl Pts',(20.8176656677548,13.1952429162414,2.92556490154576));
#130131=CARTESIAN_POINT('Ctrl Pts',(20.8109315848184,13.3103140918602,3.01214835004661));
#130132=CARTESIAN_POINT('Ctrl Pts',(20.804197501882,13.4216959931946,3.10359600184866));
#130133=CARTESIAN_POINT('Ctrl Pts',(20.7974634189456,13.52897595819,3.19955736661001));
#130134=CARTESIAN_POINT('Ctrl Pts',(20.790727670196,13.6362824610811,3.29554246937953));
#130135=CARTESIAN_POINT('Ctrl Pts',(20.7839919214463,13.7394847375183,3.3960432610415));
#130136=CARTESIAN_POINT('Ctrl Pts',(20.7772561726966,13.8382061214154,3.5006715065636));
#130137=CARTESIAN_POINT('Ctrl Pts',(20.7705141740967,13.9370191052046,3.60539683273453));
#130138=CARTESIAN_POINT('Ctrl Pts',(20.7637721754969,14.0313426428299,3.71425699380575));
#130139=CARTESIAN_POINT('Ctrl Pts',(20.757030176897,14.1208391087228,3.82682916955609));
#130140=CARTESIAN_POINT('Ctrl Pts',(20.7519216253324,14.1886524290741,3.91212743179073));
#130141=CARTESIAN_POINT('Ctrl Pts',(20.7468130737678,14.2536951325735,3.99955619341295));
#130142=CARTESIAN_POINT('Ctrl Pts',(20.7417045222033,14.3158368081123,4.08892028122819));
#130143=CARTESIAN_POINT('Ctrl Pts',(20.7349885913884,14.3975310395132,4.20640231571828));
#130144=CARTESIAN_POINT('Ctrl Pts',(20.7282726605735,14.4743500912044,4.3274317992558));
#130145=CARTESIAN_POINT('Ctrl Pts',(20.7215567297586,14.5459825288401,4.45157243139028));
#130146=CARTESIAN_POINT('Ctrl Pts',(20.7148461574089,14.6175578128304,4.57561401496664));
#130147=CARTESIAN_POINT('Ctrl Pts',(20.7081355850593,14.6839545411525,4.70276148394193));
#130148=CARTESIAN_POINT('Ctrl Pts',(20.7014250127097,14.7449047642867,4.83254991711475));
#130149=CARTESIAN_POINT('Ctrl Pts',(20.6947184269592,14.8058187782729,4.962261245917));
#130150=CARTESIAN_POINT('Ctrl Pts',(20.6880118412087,14.8612925759747,5.09461007959434));
#130151=CARTESIAN_POINT('Ctrl Pts',(20.6813052554582,14.9111043584523,5.22910735524996));
#130152=CARTESIAN_POINT('Ctrl Pts',(20.6746012879102,14.9608966947709,5.36355212414347));
#130153=CARTESIAN_POINT('Ctrl Pts',(20.6678973203622,15.0050312919063,5.50014331759118));
#130154=CARTESIAN_POINT('Ctrl Pts',(20.6611933528142,15.0433346977241,5.63837245788636));
#130155=CARTESIAN_POINT('Ctrl Pts',(20.6544893167563,15.0816384949762,5.77660301078764));
#130156=CARTESIAN_POINT('Ctrl Pts',(20.6477852806984,15.1141108743886,5.91647119019885));
#130157=CARTESIAN_POINT('Ctrl Pts',(20.6410812446405,15.1406283667068,6.05745371870328));
#130158=CARTESIAN_POINT('Ctrl Pts',(20.6343768576303,15.1671472471998,6.19844362755812));
#130159=CARTESIAN_POINT('Ctrl Pts',(20.6276724706202,15.1877105506822,6.34054763828436));
#130160=CARTESIAN_POINT('Ctrl Pts',(20.62096808361,15.2022460867859,6.48323299350801));
#130161=CARTESIAN_POINT('Ctrl Pts',(20.6142621064915,15.2167850703453,6.62595219003299));
#130162=CARTESIAN_POINT('Ctrl Pts',(20.6075561293729,15.2252934010757,6.76925263776888));
#130163=CARTESIAN_POINT('Ctrl Pts',(20.6008501522544,15.227750853798,6.91259730125182));
#130164=CARTESIAN_POINT('Ctrl Pts',(20.5941413450238,15.2302093436348,7.0560024602372));
#130165=CARTESIAN_POINT('Ctrl Pts',(20.5874325377932,15.2266118621726,7.19945150257343));
#130166=CARTESIAN_POINT('Ctrl Pts',(20.5807237305627,15.2169902963607,7.34240835917979));
#130167=CARTESIAN_POINT('Ctrl Pts',(20.5740069743707,15.2073573303917,7.48553459888278));
#130168=CARTESIAN_POINT('Ctrl Pts',(20.5672902181786,15.1916860472491,7.62816711857723));
#130169=CARTESIAN_POINT('Ctrl Pts',(20.5605734619866,15.1700602117556,7.76977513058459));
#130170=CARTESIAN_POINT('Ctrl Pts',(20.5538523224128,15.1484202631557,7.91147555654415));
#130171=CARTESIAN_POINT('Ctrl Pts',(20.5471311828389,15.1208180850618,8.05214977921517));
#130172=CARTESIAN_POINT('Ctrl Pts',(20.5404100432651,15.0873882866751,8.19127861428358));
#130173=CARTESIAN_POINT('Ctrl Pts',(20.5336789815349,15.0539091371805,8.33061283982655));
#130174=CARTESIAN_POINT('Ctrl Pts',(20.5269479198048,15.0145852798129,8.46839676418089));
#130175=CARTESIAN_POINT('Ctrl Pts',(20.5202168580746,14.9696010262843,8.60412688256317));
#130176=CARTESIAN_POINT('Ctrl Pts',(20.5164823161787,14.9446427676627,8.6794329537237));
#130177=CARTESIAN_POINT('Ctrl Pts',(20.5127477742828,14.9179429442996,8.75410715651368));
#130178=CARTESIAN_POINT('Ctrl Pts',(20.5090132323869,14.8895392850499,8.82806646618269));
#130179=CARTESIAN_POINT('Ctrl Pts',(20.5025204017193,14.8401570167588,8.95665125311397));
#130180=CARTESIAN_POINT('Ctrl Pts',(20.4960275710517,14.7854648740825,9.08348248766354));
#130181=CARTESIAN_POINT('Ctrl Pts',(20.4895347403842,14.7256061011462,9.20807828371341));
#130182=CARTESIAN_POINT('Ctrl Pts',(20.485556501942,14.6889298833625,9.28441968409128));
#130183=CARTESIAN_POINT('Ctrl Pts',(20.4815782634998,14.6503150272754,9.35992205380894));
#130184=CARTESIAN_POINT('Ctrl Pts',(20.4776000250576,14.6098038194187,9.43447708670711));
#130185=CARTESIAN_POINT('Origin',(26.8463464956315,10.1295,7.));
#130186=CARTESIAN_POINT('',(18.8525174992326,14.6098038194187,9.43447708670712));
#130187=CARTESIAN_POINT('',(18.9778214339751,14.6099559957068,9.43455988473872));
#130188=CARTESIAN_POINT('',(26.8463464956315,14.6098038194187,9.43447708670711));
#130189=CARTESIAN_POINT('',(20.0963464956032,10.1292828156512,12.0989999953747));
#130190=CARTESIAN_POINT('Ctrl Pts',(20.0963464956032,10.1292828156512,12.0989999953747));
#130191=CARTESIAN_POINT('Ctrl Pts',(20.0890161304489,9.9727687890773,12.0989933288916));
#130192=CARTESIAN_POINT('Ctrl Pts',(20.0816857652947,9.81628384987453,12.0917760164965));
#130193=CARTESIAN_POINT('Ctrl Pts',(20.0743554001404,9.66046609801297,12.0773820221436));
#130194=CARTESIAN_POINT('Ctrl Pts',(20.0698745661482,9.56521934502955,12.0685834019081));
#130195=CARTESIAN_POINT('Ctrl Pts',(20.065393732156,9.4702218440322,12.0571042223294));
#130196=CARTESIAN_POINT('Ctrl Pts',(20.0609128981638,9.37561849205956,12.0429617956103));
#130197=CARTESIAN_POINT('Ctrl Pts',(20.0540297945509,9.23029628755551,12.0212373156105));
#130198=CARTESIAN_POINT('Ctrl Pts',(20.0471466909379,9.0858734579511,11.9932209241342));
#130199=CARTESIAN_POINT('Ctrl Pts',(20.040263587325,8.94290407468458,11.9590111020268));
#130200=CARTESIAN_POINT('Ctrl Pts',(20.0333824104595,8.79997471201355,11.9248108560777));
#130201=CARTESIAN_POINT('Ctrl Pts',(20.0265012335941,8.65849831506874,11.8844207161138));
#130202=CARTESIAN_POINT('Ctrl Pts',(20.0196200567286,8.51901756866879,11.8379900101564));
#130203=CARTESIAN_POINT('Ctrl Pts',(20.0127390888202,8.37954105780559,11.7915607141354));
#130204=CARTESIAN_POINT('Ctrl Pts',(20.0058581209118,8.24206040107134,11.7390913207874));
#130205=CARTESIAN_POINT('Ctrl Pts',(19.9989771530033,8.10710237471126,11.6807807944003));
#130206=CARTESIAN_POINT('Ctrl Pts',(19.9920967087737,7.97215461938547,11.6224747057589));
#130207=CARTESIAN_POINT('Ctrl Pts',(19.985216264544,7.83972942282541,11.5583285083938));
#130208=CARTESIAN_POINT('Ctrl Pts',(19.9783358203144,7.71033280260142,11.4885889844171));
#130209=CARTESIAN_POINT('Ctrl Pts',(19.9714536339439,7.58090341892158,11.4188318022682));
#130210=CARTESIAN_POINT('Ctrl Pts',(19.9645714475735,7.45450444365356,11.3434786251353));
#130211=CARTESIAN_POINT('Ctrl Pts',(19.957689261203,7.33161704422618,11.2628220659312));
#130212=CARTESIAN_POINT('Ctrl Pts',(19.9533152585539,7.25351543788963,11.2115604486721));
#130213=CARTESIAN_POINT('Ctrl Pts',(19.9489412559048,7.17683173753798,11.1581575511211));
#130214=CARTESIAN_POINT('Ctrl Pts',(19.9445672532557,7.10168335770222,11.1026975736245));
#130215=CARTESIAN_POINT('Ctrl Pts',(19.9376178748488,6.9822882475402,11.0145832305441));
#130216=CARTESIAN_POINT('Ctrl Pts',(19.930668496442,6.8667251055417,10.921240950437));
#130217=CARTESIAN_POINT('Ctrl Pts',(19.9237191180351,6.75544289250122,10.8230275483361));
#130218=CARTESIAN_POINT('Ctrl Pts',(19.9167708710451,6.64417879713505,10.7248301361979));
#130219=CARTESIAN_POINT('Ctrl Pts',(19.9098226240551,6.53719448530056,10.6217634011466));
#130220=CARTESIAN_POINT('Ctrl Pts',(19.9028743770652,6.43490468373816,10.5142234489366));
#130221=CARTESIAN_POINT('Ctrl Pts',(19.8959257674772,6.33260954412695,10.4066778846959));
#130222=CARTESIAN_POINT('Ctrl Pts',(19.8889771578891,6.23500963255852,10.2946588716185));
#130223=CARTESIAN_POINT('Ctrl Pts',(19.8820285483011,6.14248214411779,10.1785986876101));
#130224=CARTESIAN_POINT('Ctrl Pts',(19.8750802871826,6.04995929588631,10.0625443239643));
#130225=CARTESIAN_POINT('Ctrl Pts',(19.868132026064,5.96250856499122,9.94244945163858));
#130226=CARTESIAN_POINT('Ctrl Pts',(19.8611837649454,5.88046626630638,9.8187786947424));
#130227=CARTESIAN_POINT('Ctrl Pts',(19.8542340645085,5.79840697272408,9.6950823196972));
#130228=CARTESIAN_POINT('Ctrl Pts',(19.8472843640716,5.72175853102108,9.56780885290348));
#130229=CARTESIAN_POINT('Ctrl Pts',(19.8403346636347,5.65081375603784,9.43745164631919));
#130230=CARTESIAN_POINT('Ctrl Pts',(19.8362969785389,5.60959576928118,9.36171581354087));
#130231=CARTESIAN_POINT('Ctrl Pts',(19.8322592934432,5.57030220177107,9.28493958658977));
#130232=CARTESIAN_POINT('Ctrl Pts',(19.8282216083474,5.53298336328829,9.20722355198392));
#130233=CARTESIAN_POINT('Ctrl Pts',(19.821289621329,5.46891355651218,9.07379894599301));
#130234=CARTESIAN_POINT('Ctrl Pts',(19.8143576343105,5.41064597993131,8.93755962820844));
#130235=CARTESIAN_POINT('Ctrl Pts',(19.807425647292,5.35841008944348,8.79902808910417));
#130236=CARTESIAN_POINT('Ctrl Pts',(19.800494976297,5.30618411583254,8.66052284992904));
#130237=CARTESIAN_POINT('Ctrl Pts',(19.7935643053021,5.25998766035838,8.51972656710486));
#130238=CARTESIAN_POINT('Ctrl Pts',(19.7866336343072,5.22000157021081,8.37718051391147));
#130239=CARTESIAN_POINT('Ctrl Pts',(19.7797027024116,5.18001397481245,8.23462909466308));
#130240=CARTESIAN_POINT('Ctrl Pts',(19.772771770516,5.14623730510447,8.09032809093049));
#130241=CARTESIAN_POINT('Ctrl Pts',(19.7658408386203,5.11880232749438,7.94483323118251));
#130242=CARTESIAN_POINT('Ctrl Pts',(19.7589102686247,5.09136878240709,7.7993459684775));
#130243=CARTESIAN_POINT('Ctrl Pts',(19.7519796986291,5.07027632712535,7.65266529985237));
#130244=CARTESIAN_POINT('Ctrl Pts',(19.7450491286335,5.05560446738238,7.50535643271154));
#130245=CARTESIAN_POINT('Ctrl Pts',(19.73811698291,5.04092927185914,7.35801407356488));
#130246=CARTESIAN_POINT('Ctrl Pts',(19.7311848371864,5.03267762147763,7.21004355990087));
#130247=CARTESIAN_POINT('Ctrl Pts',(19.7242526914629,5.03087713469774,7.06201513861103));
#130248=CARTESIAN_POINT('Ctrl Pts',(19.720127115455,5.02980559850131,6.97391795662521));
#130249=CARTESIAN_POINT('Ctrl Pts',(19.7160015394472,5.03101799301621,6.88580032960711));
#130250=CARTESIAN_POINT('Ctrl Pts',(19.7118759634393,5.03451137520289,6.7977825101827));
#130251=CARTESIAN_POINT('Ctrl Pts',(19.7049446719573,5.04038053144858,6.64990566562309));
#130252=CARTESIAN_POINT('Ctrl Pts',(19.6980133804754,5.05269303632925,6.50225813648039));
#130253=CARTESIAN_POINT('Ctrl Pts',(19.6910820889935,5.07140714354957,6.35540892379343));
#130254=CARTESIAN_POINT('Ctrl Pts',(19.684152155773,5.09011758353832,6.20858848779688));
#130255=CARTESIAN_POINT('Ctrl Pts',(19.6772222225525,5.11522708127017,6.06256638434082));
#130256=CARTESIAN_POINT('Ctrl Pts',(19.6702922893321,5.14664214325448,5.91790546648205));
#130257=CARTESIAN_POINT('Ctrl Pts',(19.6633621517524,5.1780581316483,5.77324028266798));
#130258=CARTESIAN_POINT('Ctrl Pts',(19.6564320141728,5.21577998959382,5.62993668900666));
#130259=CARTESIAN_POINT('Ctrl Pts',(19.6495018765932,5.25966320185875,5.48854687156054));
#130260=CARTESIAN_POINT('Ctrl Pts',(19.6425721311451,5.30354393105684,5.34716505444874));
#130261=CARTESIAN_POINT('Ctrl Pts',(19.6356423856971,5.35358521806554,5.20769711279096));
#130262=CARTESIAN_POINT('Ctrl Pts',(19.6287126402491,5.40959281113345,5.07067962005118));
#130263=CARTESIAN_POINT('Ctrl Pts',(19.6217813588474,5.46561281808696,4.93363175786706));
#130264=CARTESIAN_POINT('Ctrl Pts',(19.6148500774458,5.52760164817835,4.79903573639757));
#130265=CARTESIAN_POINT('Ctrl Pts',(19.6079187960441,5.59531683860089,4.6674082957181));
#130266=CARTESIAN_POINT('Ctrl Pts',(19.6037893035398,5.63565993752792,4.58898779911004));
#130267=CARTESIAN_POINT('Ctrl Pts',(19.5996598110354,5.67803469414855,4.51162059036806));
#130268=CARTESIAN_POINT('Ctrl Pts',(19.5955303185311,5.72238203724709,4.43541187275996));
#130269=CARTESIAN_POINT('Ctrl Pts',(19.5885944856084,5.79686716150288,4.30741286754781));
#130270=CARTESIAN_POINT('Ctrl Pts',(19.5816586526857,5.87694484651429,4.18263962042732));
#130271=CARTESIAN_POINT('Ctrl Pts',(19.5747228197629,5.96231102063768,4.06157576067015));
#130272=CARTESIAN_POINT('Ctrl Pts',(19.5677882683408,6.04766142206249,3.94053426930173));
#130273=CARTESIAN_POINT('Ctrl Pts',(19.5608537169187,6.138298172888,3.82320106750737));
#130274=CARTESIAN_POINT('Ctrl Pts',(19.5539191654965,6.23387438004653,3.71003008689105));
#130275=CARTESIAN_POINT('Ctrl Pts',(19.5469843393753,6.32945437327471,3.59685462322159));
#130276=CARTESIAN_POINT('Ctrl Pts',(19.5400495132541,6.42997400380587,3.48784196492398));
#130277=CARTESIAN_POINT('Ctrl Pts',(19.5331146871329,6.53504630945991,3.38341270441833));
#130278=CARTESIAN_POINT('Ctrl Pts',(19.526180224502,6.64011310772749,3.2789889175938));
#130279=CARTESIAN_POINT('Ctrl Pts',(19.5192457618712,6.74973186874695,3.17914827984244));
#130280=CARTESIAN_POINT('Ctrl Pts',(19.5123112992403,6.86347901257573,3.08427428058295));
#130281=CARTESIAN_POINT('Ctrl Pts',(19.5053752975239,6.97725140228127,2.98937922429105));
#130282=CARTESIAN_POINT('Ctrl Pts',(19.4984392958074,7.09515375203486,2.89945322061358));
#130283=CARTESIAN_POINT('Ctrl Pts',(19.491503294091,7.21672918432727,2.81483964759232));
#130284=CARTESIAN_POINT('Ctrl Pts',(19.4873970872683,7.28870348450164,2.76474726800027));
#130285=CARTESIAN_POINT('Ctrl Pts',(19.4832908804456,7.36196451810915,2.71651600682106));
#130286=CARTESIAN_POINT('Ctrl Pts',(19.4791846736229,7.43641261061583,2.67021001512314));
#130287=CARTESIAN_POINT('Ctrl Pts',(19.4722525172567,7.56209693210968,2.59203558577654));
#130288=CARTESIAN_POINT('Ctrl Pts',(19.4653203608905,7.69120946211311,2.51932363092219));
#130289=CARTESIAN_POINT('Ctrl Pts',(19.4583882045243,7.82325572183359,2.45235903688245));
#130290=CARTESIAN_POINT('Ctrl Pts',(19.4514573849167,7.95527651848407,2.38540735592446));
#130291=CARTESIAN_POINT('Ctrl Pts',(19.4445265653092,8.09022962124302,2.32420097417425));
#130292=CARTESIAN_POINT('Ctrl Pts',(19.4375957457017,8.22759659625989,2.26897849900872));
#130293=CARTESIAN_POINT('Ctrl Pts',(19.4306646979627,8.36496809277999,2.21375420616759));
#130294=CARTESIAN_POINT('Ctrl Pts',(19.4237336502237,8.50475331485511,2.1645143406319));
#130295=CARTESIAN_POINT('Ctrl Pts',(19.4168026024848,8.64641401791103,2.12144929618117));
#130296=CARTESIAN_POINT('Ctrl Pts',(19.4098719355473,8.78806693792938,2.07838661778434));
#130297=CARTESIAN_POINT('Ctrl Pts',(19.4029412686098,8.93159481592078,2.0414981770105));
#130298=CARTESIAN_POINT('Ctrl Pts',(19.3960106016723,9.07644441148998,2.01092444159163));
#130299=CARTESIAN_POINT('Ctrl Pts',(19.3890783892253,9.22132630791024,1.98034388835824));
#130300=CARTESIAN_POINT('Ctrl Pts',(19.3821461767782,9.36753018698955,1.95608092251632));
#130301=CARTESIAN_POINT('Ctrl Pts',(19.3752139643311,9.51449215978495,1.93822497966632));
#130302=CARTESIAN_POINT('Ctrl Pts',(19.3710889857923,9.60194115077144,1.92759988968118));
#130303=CARTESIAN_POINT('Ctrl Pts',(19.3669640072535,9.68965839362783,1.91924240856535));
#130304=CARTESIAN_POINT('Ctrl Pts',(19.3628390287147,9.77752407795016,1.91316267703624));
#130305=CARTESIAN_POINT('Ctrl Pts',(19.3559048075467,9.9252291102158,1.90294245342334));
#130306=CARTESIAN_POINT('Ctrl Pts',(19.3489705863787,10.0734048576221,1.89915811700655));
#130307=CARTESIAN_POINT('Ctrl Pts',(19.3420363652107,10.2214806592299,1.9018296852373));
#130308=CARTESIAN_POINT('Ctrl Pts',(19.335103451794,10.3695285346548,1.90450074962676));
#130309=CARTESIAN_POINT('Ctrl Pts',(19.3281705383774,10.5174761716726,1.91362528350658));
#130310=CARTESIAN_POINT('Ctrl Pts',(19.3212376249607,10.6647534305791,1.92917119545007));
#130311=CARTESIAN_POINT('Ctrl Pts',(19.3143044602487,10.8120360278019,1.94471767088173));
#130312=CARTESIAN_POINT('Ctrl Pts',(19.3073712955368,10.9586478693285,1.96668595872507));
#130313=CARTESIAN_POINT('Ctrl Pts',(19.3004381308248,11.1040238996176,1.99499209100783));
#130314=CARTESIAN_POINT('Ctrl Pts',(19.2935053388582,11.2493921141048,2.02329670147767));
#130315=CARTESIAN_POINT('Ctrl Pts',(19.2865725468916,11.3935243261183,2.05793841047807));
#130316=CARTESIAN_POINT('Ctrl Pts',(19.279639754925,11.535865618028,2.09878211579726));
#130317=CARTESIAN_POINT('Ctrl Pts',(19.2727054235545,11.678238516357,2.13963489032792));
#130318=CARTESIAN_POINT('Ctrl Pts',(19.2657710921841,11.8188193822447,2.18669232169525));
#130319=CARTESIAN_POINT('Ctrl Pts',(19.2588367608137,11.9570677921862,2.23976923196325));
#130320=CARTESIAN_POINT('Ctrl Pts',(19.2547223018113,12.0390969575754,2.27126221370942));
#130321=CARTESIAN_POINT('Ctrl Pts',(19.2506078428089,12.1203052653314,2.30487346637448));
#130322=CARTESIAN_POINT('Ctrl Pts',(19.2464933838065,12.2005829824517,2.34055622635073));
#130323=CARTESIAN_POINT('Ctrl Pts',(19.2395600659607,12.3358598021767,2.40068561793972));
#130324=CARTESIAN_POINT('Ctrl Pts',(19.2326267481149,12.4685396684855,2.4667205822027));
#130325=CARTESIAN_POINT('Ctrl Pts',(19.225693430269,12.5981090877672,2.53841169853235));
#130326=CARTESIAN_POINT('Ctrl Pts',(19.2187614321196,12.7276538446444,2.6100891690857));
#130327=CARTESIAN_POINT('Ctrl Pts',(19.2118294339701,12.8540890465733,2.68742048375259));
#130328=CARTESIAN_POINT('Ctrl Pts',(19.2048974358206,12.9769260564387,2.77011042069487));
#130329=CARTESIAN_POINT('Ctrl Pts',(19.1979651953757,13.0997673598497,2.85280324791448));
#130330=CARTESIAN_POINT('Ctrl Pts',(19.1910329549307,13.2190099433899,2.9408548903621));
#130331=CARTESIAN_POINT('Ctrl Pts',(19.1841007144858,13.3341939513471,3.03392666757164));
#130332=CARTESIAN_POINT('Ctrl Pts',(19.1771688496638,13.4493717180665,3.12699340169313));
#130333=CARTESIAN_POINT('Ctrl Pts',(19.1702369848419,13.5604910926603,3.22507951774791));
#130334=CARTESIAN_POINT('Ctrl Pts',(19.1633051200199,13.667125119773,3.3278058994722));
#130335=CARTESIAN_POINT('Ctrl Pts',(19.1563717121302,13.7737828841536,3.430555148603));
#130336=CARTESIAN_POINT('Ctrl Pts',(19.1494383042404,13.8759530677986,3.53794649789823));
#130337=CARTESIAN_POINT('Ctrl Pts',(19.1425048963507,13.9732449701325,3.64956337105432));
#130338=CARTESIAN_POINT('Ctrl Pts',(19.1383858438666,14.0310448945516,3.71587358472634));
#130339=CARTESIAN_POINT('Ctrl Pts',(19.1342667913824,14.0871237909435,3.78367446321953));
#130340=CARTESIAN_POINT('Ctrl Pts',(19.1301477388983,14.1414063406675,3.85287297464629));
#130341=CARTESIAN_POINT('Ctrl Pts',(19.1232141285398,14.2327802793352,3.96935498536888));
#130342=CARTESIAN_POINT('Ctrl Pts',(19.1162805181812,14.3190936323279,4.08983919704816));
#130343=CARTESIAN_POINT('Ctrl Pts',(19.1093469078227,14.400009475508,4.213864716207));
#130344=CARTESIAN_POINT('Ctrl Pts',(19.1024146136957,14.4809099581506,4.3378666911678));
#130345=CARTESIAN_POINT('Ctrl Pts',(19.0954823195687,14.5564147947404,4.46540835564231));
#130346=CARTESIAN_POINT('Ctrl Pts',(19.0885500254416,14.6262304728754,4.59599998870346));
#130347=CARTESIAN_POINT('Ctrl Pts',(19.0816174867073,14.6960486144694,4.72659622971433));
#130348=CARTESIAN_POINT('Ctrl Pts',(19.0746849479731,14.7601770371195,4.86024236471895));
#130349=CARTESIAN_POINT('Ctrl Pts',(19.0677524092388,14.8183680106684,4.99642375275354));
#130350=CARTESIAN_POINT('Ctrl Pts',(19.0608202455346,14.8765558362549,5.13259777377116));
#130351=CARTESIAN_POINT('Ctrl Pts',(19.0538880818305,14.928806726421,5.2713064690269));
#130352=CARTESIAN_POINT('Ctrl Pts',(19.0469559181264,14.9749209568293,5.41201487692134));
#130353=CARTESIAN_POINT('Ctrl Pts',(19.0400222130546,15.0210454407442,5.55275457135289));
#130354=CARTESIAN_POINT('Ctrl Pts',(19.0330885079828,15.061030435488,5.69549455262194));
#130355=CARTESIAN_POINT('Ctrl Pts',(19.0261548029109,15.0947257927471,5.83968373835435));
#130356=CARTESIAN_POINT('Ctrl Pts',(19.0220372332707,15.1147357266325,5.92531025512671));
#130357=CARTESIAN_POINT('Ctrl Pts',(19.0179196636304,15.1325285371395,6.01144756489171));
#130358=CARTESIAN_POINT('Ctrl Pts',(19.0138020939901,15.1480812641024,6.09797832864145));
#130359=CARTESIAN_POINT('Ctrl Pts',(19.0068685366312,15.1742704324482,6.243687100122));
#130360=CARTESIAN_POINT('Ctrl Pts',(18.9999349792723,15.1941141114036,6.39056233036988));
#130361=CARTESIAN_POINT('Ctrl Pts',(18.9930014219134,15.2075304301788,6.53803901660621));
#130362=CARTESIAN_POINT('Ctrl Pts',(18.9860691810523,15.2209442015525,6.68548770094879));
#130363=CARTESIAN_POINT('Ctrl Pts',(18.9791369401912,15.2279330176624,6.83353728439083));
#130364=CARTESIAN_POINT('Ctrl Pts',(18.9722046993301,15.2284668647841,6.98161762166019));
#130365=CARTESIAN_POINT('Ctrl Pts',(18.9652722137388,15.2290007307523,7.12970318663661));
#130366=CARTESIAN_POINT('Ctrl Pts',(18.9583397281476,15.2230791672004,7.277819177055));
#130367=CARTESIAN_POINT('Ctrl Pts',(18.9514072425563,15.2107242822434,7.42539486778772));
#130368=CARTESIAN_POINT('Ctrl Pts',(18.944475131797,15.1983700653015,7.57296257926426));
#130369=CARTESIAN_POINT('Ctrl Pts',(18.9375430210376,15.1795832514988,7.71998972015295));
#130370=CARTESIAN_POINT('Ctrl Pts',(18.9306109102783,15.1544378816705,7.8659100908022));
#130371=CARTESIAN_POINT('Ctrl Pts',(18.9236772573793,15.1292869179224,8.01186292336617));
#130372=CARTESIAN_POINT('Ctrl Pts',(18.9167436044803,15.0977746278607,8.15670816782282));
#130373=CARTESIAN_POINT('Ctrl Pts',(18.9098099515813,15.0600264057109,8.29988859622179));
#130374=CARTESIAN_POINT('Ctrl Pts',(18.9056921174149,15.0376080756969,8.38492216635021));
#130375=CARTESIAN_POINT('Ctrl Pts',(18.9015742832484,15.0129912650688,8.46936874673091));
#130376=CARTESIAN_POINT('Ctrl Pts',(18.8974564490819,14.9862106421525,8.55311388455654));
#130377=CARTESIAN_POINT('Ctrl Pts',(18.890522946704,14.9411181238125,8.69412177578796));
#130378=CARTESIAN_POINT('Ctrl Pts',(18.883589444326,14.8898727356053,8.83318887004119));
#130379=CARTESIAN_POINT('Ctrl Pts',(18.8766559419481,14.8326667134249,8.96977761834485));
#130380=CARTESIAN_POINT('Ctrl Pts',(18.8697236785937,14.7754709140157,9.10634195810776));
#130381=CARTESIAN_POINT('Ctrl Pts',(18.8627914152393,14.712316733052,9.2404285306325));
#130382=CARTESIAN_POINT('Ctrl Pts',(18.8558591518849,14.6434446407832,9.37151950865782));
#130383=CARTESIAN_POINT('Ctrl Pts',(18.8547452676674,14.6323781921101,9.39258336096776));
#130384=CARTESIAN_POINT('Ctrl Pts',(18.85363138345,14.6211642148427,9.41356991806466));
#130385=CARTESIAN_POINT('Ctrl Pts',(18.8525174992326,14.6098038194187,9.43447708670712));
#130386=CARTESIAN_POINT('Ctrl Pts',(20.352563293369,14.6098038194187,9.43447708670712));
#130387=CARTESIAN_POINT('Ctrl Pts',(20.3452868626689,14.5356719094128,9.57090617094612));
#130388=CARTESIAN_POINT('Ctrl Pts',(20.3380104319687,14.4553225791197,9.70391405302278));
#130389=CARTESIAN_POINT('Ctrl Pts',(20.3307340012685,14.3690871677716,9.83296693359918));
#130390=CARTESIAN_POINT('Ctrl Pts',(20.3234553596846,14.2828255545013,9.96205902583457));
#130391=CARTESIAN_POINT('Ctrl Pts',(20.3161767181007,14.1906744289206,10.0871935054699));
#130392=CARTESIAN_POINT('Ctrl Pts',(20.3088980765167,14.0930082832942,10.207865815189));
#130393=CARTESIAN_POINT('Ctrl Pts',(20.3038001136712,14.0246028843024,10.2923847387183));
#130394=CARTESIAN_POINT('Ctrl Pts',(20.2987021508257,13.9534929304548,10.3747153144459));
#130395=CARTESIAN_POINT('Ctrl Pts',(20.2936041879802,13.8798190021703,10.4546936741136));
#130396=CARTESIAN_POINT('Ctrl Pts',(20.2868777084082,13.7826103349796,10.5602206892792));
#130397=CARTESIAN_POINT('Ctrl Pts',(20.2801512288361,13.6808807511221,10.6617110339456));
#130398=CARTESIAN_POINT('Ctrl Pts',(20.2734247492641,13.5749966495666,10.7587702560579));
#130399=CARTESIAN_POINT('Ctrl Pts',(20.2667018516651,13.469168933226,10.8557777923645));
#130400=CARTESIAN_POINT('Ctrl Pts',(20.2599789540661,13.3591913769016,10.9483586585881));
#130401=CARTESIAN_POINT('Ctrl Pts',(20.2532560564671,13.2454670553348,11.0361553872551));
#130402=CARTESIAN_POINT('Ctrl Pts',(20.2465348108106,13.1317706779763,11.1239305426118));
#130403=CARTESIAN_POINT('Ctrl Pts',(20.2398135651542,13.0143296577915,11.2069236743742));
#130404=CARTESIAN_POINT('Ctrl Pts',(20.2330923194978,12.8935800092736,11.2848176976779));
#130405=CARTESIAN_POINT('Ctrl Pts',(20.2263722417576,12.7728513428002,11.3626981857385));
#130406=CARTESIAN_POINT('Ctrl Pts',(20.2196521640174,12.6488155039474,11.4354811335249));
#130407=CARTESIAN_POINT('Ctrl Pts',(20.2129320862772,12.5219371004028,11.5028930389935));
#130408=CARTESIAN_POINT('Ctrl Pts',(20.2062101801347,12.3950241757136,11.5703232859298));
#130409=CARTESIAN_POINT('Ctrl Pts',(20.1994882739921,12.2652674652434,11.6323793963712));
#130410=CARTESIAN_POINT('Ctrl Pts',(20.1927663678496,12.1331560519276,11.6888339089345));
#130411=CARTESIAN_POINT('Ctrl Pts',(20.1875970929237,12.0315598377311,11.7322485133716));
#130412=CARTESIAN_POINT('Ctrl Pts',(20.1824278179979,11.9285716059888,11.7723513056034));
#130413=CARTESIAN_POINT('Ctrl Pts',(20.1772585430721,11.8244215995656,11.8090583040057));
#130414=CARTESIAN_POINT('Ctrl Pts',(20.1702029153173,11.6822655551441,11.8591602855097));
#130415=CARTESIAN_POINT('Ctrl Pts',(20.1631472875625,11.5378982969924,11.9029508158294));
#130416=CARTESIAN_POINT('Ctrl Pts',(20.1560916598077,11.3918866567047,11.9402612207224));
#130417=CARTESIAN_POINT('Ctrl Pts',(20.1490358127607,11.245870478308,11.9775727852401));
#130418=CARTESIAN_POINT('Ctrl Pts',(20.1419799657137,11.0982101122984,12.0084037507865));
#130419=CARTESIAN_POINT('Ctrl Pts',(20.1349241186668,10.9494848386558,12.0326360750977));
#130420=CARTESIAN_POINT('Ctrl Pts',(20.1278666858757,10.8007261402202,12.0568738454262));
#130421=CARTESIAN_POINT('Ctrl Pts',(20.1208092530846,10.6509023569821,12.0745099618943));
#130422=CARTESIAN_POINT('Ctrl Pts',(20.1137518202935,10.5006010709216,12.0854778531777));
#130423=CARTESIAN_POINT('Ctrl Pts',(20.1079500454062,10.3770413782099,12.0944943380808));
#130424=CARTESIAN_POINT('Ctrl Pts',(20.1021482705188,10.2531592030081,12.0990052716912));
#130425=CARTESIAN_POINT('Ctrl Pts',(20.0963464956315,10.1292828162553,12.0989999953747));
#130426=CARTESIAN_POINT('',(20.2216535043684,10.1337426824875,12.0989982349129));
#130427=CARTESIAN_POINT('Ctrl Pts',(20.4776000250576,14.6098038194187,9.43447708670711));
#130428=CARTESIAN_POINT('Ctrl Pts',(20.4711196680077,14.5438130309703,9.55592361136169));
#130429=CARTESIAN_POINT('Ctrl Pts',(20.4646393109577,14.4727878484368,9.67485523573746));
#130430=CARTESIAN_POINT('Ctrl Pts',(20.4581589539078,14.3969502782224,9.79081871910371));
#130431=CARTESIAN_POINT('Ctrl Pts',(20.4516843951578,14.3211805636795,9.9066784441347));
#130432=CARTESIAN_POINT('Ctrl Pts',(20.4452098364078,14.2406072440856,10.0195749767462));
#130433=CARTESIAN_POINT('Ctrl Pts',(20.4387352776578,14.1554982256597,10.1290796229858));
#130434=CARTESIAN_POINT('Ctrl Pts',(20.4319680553625,14.0665421022753,10.2435341073896));
#130435=CARTESIAN_POINT('Ctrl Pts',(20.4252008330672,13.9726308486994,10.3542824951181));
#130436=CARTESIAN_POINT('Ctrl Pts',(20.4184336107719,13.8741212483996,10.4608687790834));
#130437=CARTESIAN_POINT('Ctrl Pts',(20.4119648781616,13.7799567247469,10.5627537387925));
#130438=CARTESIAN_POINT('Ctrl Pts',(20.4054961455513,13.6815911429066,10.6608355944725));
#130439=CARTESIAN_POINT('Ctrl Pts',(20.3990274129409,13.5793769002379,10.7547503742865));
#130440=CARTESIAN_POINT('Ctrl Pts',(20.3925591385534,13.4771698980755,10.8486585014998));
#130441=CARTESIAN_POINT('Ctrl Pts',(20.3860908641659,13.3711150722958,10.938399867969));
#130442=CARTESIAN_POINT('Ctrl Pts',(20.3796225897784,13.2616004380997,11.0236485738265));
#130443=CARTESIAN_POINT('Ctrl Pts',(20.3731532953867,13.1520685341682,11.1089107228425));
#130444=CARTESIAN_POINT('Ctrl Pts',(20.366684000995,13.0390760535248,11.1896785559707));
#130445=CARTESIAN_POINT('Ctrl Pts',(20.3602147066033,12.9230422847047,11.2656678848179));
#130446=CARTESIAN_POINT('Ctrl Pts',(20.3537429132159,12.8069636937012,11.3416865672548));
#130447=CARTESIAN_POINT('Ctrl Pts',(20.3472711198284,12.6878418136861,11.412922855206));
#130448=CARTESIAN_POINT('Ctrl Pts',(20.3407993264409,12.5661224834895,11.4791374027767));
#130449=CARTESIAN_POINT('Ctrl Pts',(20.3343198330908,12.4442583349656,11.5454307306038));
#130450=CARTESIAN_POINT('Ctrl Pts',(20.3278403397406,12.3197909209688,11.6066902022129));
#130451=CARTESIAN_POINT('Ctrl Pts',(20.3213608463905,12.1931884004942,11.6627235802335));
#130452=CARTESIAN_POINT('Ctrl Pts',(20.3148768275244,12.0664974561729,11.7187960940218));
#130453=CARTESIAN_POINT('Ctrl Pts',(20.3083928086584,11.9376688092067,11.7696351036927));
#130454=CARTESIAN_POINT('Ctrl Pts',(20.3019087897923,11.8071866552316,11.8150979727164));
#130455=CARTESIAN_POINT('Ctrl Pts',(20.2954150217898,11.676508313007,11.8606291980664));
#130456=CARTESIAN_POINT('Ctrl Pts',(20.2889212537874,11.5441718846024,11.9007680384156));
#130457=CARTESIAN_POINT('Ctrl Pts',(20.282427485785,11.4106729541157,11.9354226629178));
#130458=CARTESIAN_POINT('Ctrl Pts',(20.2803923047135,11.3688336866381,11.9462836046392));
#130459=CARTESIAN_POINT('Ctrl Pts',(20.278357123642,11.3268802787869,11.956606253736));
#130460=CARTESIAN_POINT('Ctrl Pts',(20.2763219425705,11.2848280760658,11.9663888326081));
#130461=CARTESIAN_POINT('Ctrl Pts',(20.2664266823321,11.0803659299939,12.0139527398677));
#130462=CARTESIAN_POINT('Ctrl Pts',(20.2565314220938,10.8730095382161,12.0488763230015));
#130463=CARTESIAN_POINT('Ctrl Pts',(20.2466361618554,10.6640303707002,12.0709050753094));
#130464=CARTESIAN_POINT('Ctrl Pts',(20.2383086093597,10.4881598078176,12.0894438086868));
#130465=CARTESIAN_POINT('Ctrl Pts',(20.2299810568641,10.3111395726563,12.098850629708));
#130466=CARTESIAN_POINT('Ctrl Pts',(20.2216535043684,10.1337426824875,12.0989982349129));
#130467=CARTESIAN_POINT('Ctrl Pts',(20.2216531628861,10.1337360354165,12.0997534730252));
#130468=CARTESIAN_POINT('Ctrl Pts',(20.1623123261755,8.86943546207591,12.0878187862941));
#130469=CARTESIAN_POINT('Ctrl Pts',(20.0641896078287,6.76854703791684,11.2892745934799));
#130470=CARTESIAN_POINT('Ctrl Pts',(19.9272850078459,5.12804044036981,8.75245917967931));
#130471=CARTESIAN_POINT('Ctrl Pts',(19.8109393629377,4.88151594588123,6.21192105474875));
#130472=CARTESIAN_POINT('Ctrl Pts',(19.6945937180295,5.86543450296868,3.84345751957051));
#130473=CARTESIAN_POINT('Ctrl Pts',(19.5782480731213,7.83815969325507,2.21543015947418));
#130474=CARTESIAN_POINT('Ctrl Pts',(19.4619024282131,10.3463489318624,1.69885207129888));
#130475=CARTESIAN_POINT('Ctrl Pts',(19.3455567833049,12.803119455071,2.41785981379941));
#130476=CARTESIAN_POINT('Ctrl Pts',(19.2292111383967,14.6377971005625,4.2031950129451));
#130477=CARTESIAN_POINT('Ctrl Pts',(19.1128654934886,15.4225339830853,6.640033572117));
#130478=CARTESIAN_POINT('Ctrl Pts',(19.029068925348,15.1001465815671,8.45540708667062));
#130479=CARTESIAN_POINT('Ctrl Pts',(18.9840542388435,14.6736170860257,9.31766124714267));
#130480=CARTESIAN_POINT('Ctrl Pts',(18.9778214339751,14.6099559957068,9.43455988473872));
#130481=CARTESIAN_POINT('Origin',(-18.734,19.211,-1.76670989022852));
#130482=CARTESIAN_POINT('',(-17.1724222331904,17.1782439613541,0.749817809475409));
#130483=CARTESIAN_POINT('',(-17.1763093433855,17.1833020606949,0.683386614791102));
#130484=CARTESIAN_POINT('',(-17.174464231106,17.180864983421,-1.76670989022852));
#130485=CARTESIAN_POINT('',(-21.2939992552734,19.212952690406,0.233290109771496));
#130486=CARTESIAN_POINT('Ctrl Pts',(-21.2960081472498,19.2129542227284,
0.233290109771496));
#130487=CARTESIAN_POINT('Ctrl Pts',(-21.2971424692952,19.3442911272882,
0.239839092339242));
#130488=CARTESIAN_POINT('Ctrl Pts',(-21.2281784359338,20.3246261525587,
0.288780010467465));
#130489=CARTESIAN_POINT('Ctrl Pts',(-19.9618263685217,21.9781789381743,
0.380112864156167));
#130490=CARTESIAN_POINT('Ctrl Pts',(-17.0720918237967,21.7409376748804,
0.507288670837602));
#130491=CARTESIAN_POINT('Ctrl Pts',(-15.7493319130901,19.2624152772813,
0.630523652610683));
#130492=CARTESIAN_POINT('Ctrl Pts',(-16.5648620620492,17.6518059357956,
0.711366698823284));
#130493=CARTESIAN_POINT('Ctrl Pts',(-17.1724222331904,17.1782439613541,
0.749817809475409));
#130494=CARTESIAN_POINT('',(-18.0722320621911,16.7380133044256,1.80302994756687E-11));
#130495=CARTESIAN_POINT('Ctrl Pts',(-18.0722320621911,16.7380133044256,
1.80300219199125E-11));
#130496=CARTESIAN_POINT('Ctrl Pts',(-18.1529464922157,16.7164142307207,
0.00418158398862037));
#130497=CARTESIAN_POINT('Ctrl Pts',(-18.2348706569439,16.6987304519573,
0.00836316795921058));
#130498=CARTESIAN_POINT('Ctrl Pts',(-18.3175895998167,16.6850937510234,
0.012544751929801));
#130499=CARTESIAN_POINT('Ctrl Pts',(-18.400190747281,16.6714764693507,0.0167203811411207));
#130500=CARTESIAN_POINT('Ctrl Pts',(-18.4835839741038,16.6618948926126,
0.0208960103524402));
#130501=CARTESIAN_POINT('Ctrl Pts',(-18.5673406239762,16.656430632693,0.02507163956376));
#130502=CARTESIAN_POINT('Ctrl Pts',(-18.6514938546105,16.6509404999577,
0.0292670400316576));
#130503=CARTESIAN_POINT('Ctrl Pts',(-18.7360135046785,16.6496069028829,
0.0334624404995552));
#130504=CARTESIAN_POINT('Ctrl Pts',(-18.8204558534901,16.6524603021651,
0.0376578409674528));
#130505=CARTESIAN_POINT('Ctrl Pts',(-18.9043486080215,16.6552951300557,
0.0418259356091481));
#130506=CARTESIAN_POINT('Ctrl Pts',(-18.9881645984016,16.6622626001438,
0.0459940302508442));
#130507=CARTESIAN_POINT('Ctrl Pts',(-19.0714668099551,16.6733404183818,
0.0501621248925395));
#130508=CARTESIAN_POINT('Ctrl Pts',(-19.1547409379247,16.684414501967,0.0543288143490282));
#130509=CARTESIAN_POINT('Ctrl Pts',(-19.2375011746968,16.6995961209329,
0.0584955038055169));
#130510=CARTESIAN_POINT('Ctrl Pts',(-19.3193159599542,16.7188111574315,
0.0626621932620057));
#130511=CARTESIAN_POINT('Ctrl Pts',(-19.4011278018881,16.7380255026606,
0.0668287328199814));
#130512=CARTESIAN_POINT('Ctrl Pts',(-19.481993811599,16.7612728705988,0.0709952723779566));
#130513=CARTESIAN_POINT('Ctrl Pts',(-19.5614943032478,16.7884283956728,
0.0751618119359323));
#130514=CARTESIAN_POINT('Ctrl Pts',(-19.6419503629735,16.8159103206512,
0.0793784318407133));
#130515=CARTESIAN_POINT('Ctrl Pts',(-19.721007396075,16.8473948424126,0.0835950517454946));
#130516=CARTESIAN_POINT('Ctrl Pts',(-19.7982496311477,16.8827017539409,
0.0878116716502757));
#130517=CARTESIAN_POINT('Ctrl Pts',(-19.8746816906651,16.9176383396154,
0.0919840644250511));
#130518=CARTESIAN_POINT('Ctrl Pts',(-19.9493364580842,16.9563172372311,
0.0961564571998266));
#130519=CARTESIAN_POINT('Ctrl Pts',(-20.0218360729121,16.9985176273456,
0.100328849974602));
#130520=CARTESIAN_POINT('Ctrl Pts',(-20.0954884255321,17.0413890001219,
0.104567583444386));
#130521=CARTESIAN_POINT('Ctrl Pts',(-20.1669160788343,17.0878945550855,
0.10880631691417));
#130522=CARTESIAN_POINT('Ctrl Pts',(-20.2357552271545,17.1377582780307,
0.113045050383954));
#130523=CARTESIAN_POINT('Ctrl Pts',(-20.3045943754748,17.187622000976,0.117283783853738));
#130524=CARTESIAN_POINT('Ctrl Pts',(-20.370844676157,17.2408435335627,0.121522517323522));
#130525=CARTESIAN_POINT('Ctrl Pts',(-20.4341804449292,17.2971069897509,
0.125761250793306));
#130526=CARTESIAN_POINT('Ctrl Pts',(-20.4958618563844,17.3519008204458,
0.129889266735435));
#130527=CARTESIAN_POINT('Ctrl Pts',(-20.5550187589506,17.4097927026216,
0.134017282677563));
#130528=CARTESIAN_POINT('Ctrl Pts',(-20.611317450137,17.4705175406195,0.138145298619692));
#130529=CARTESIAN_POINT('Ctrl Pts',(-20.6675250696014,17.5311441469278,
0.142266636866263));
#130530=CARTESIAN_POINT('Ctrl Pts',(-20.7208833454928,17.5945942591679,
0.146387975112834));
#130531=CARTESIAN_POINT('Ctrl Pts',(-20.7710927993391,17.6605636333984,
0.150509313359405));
#130532=CARTESIAN_POINT('Ctrl Pts',(-20.8212566260777,17.7264730589238,
0.154626906400053));
#130533=CARTESIAN_POINT('Ctrl Pts',(-20.8682770216554,17.7948968304612,
0.158744499440701));
#130534=CARTESIAN_POINT('Ctrl Pts',(-20.9118931634006,17.8654958681547,
0.162862092481349));
#130535=CARTESIAN_POINT('Ctrl Pts',(-20.9554835923167,17.9360532859129,
0.166977258095768));
#130536=CARTESIAN_POINT('Ctrl Pts',(-20.9956735017905,18.0087830229833,
0.171092423710186));
#130537=CARTESIAN_POINT('Ctrl Pts',(-21.0322449058945,18.0833163774666,
0.175207589324605));
#130538=CARTESIAN_POINT('Ctrl Pts',(-21.0688064212004,18.1578295783544,
0.179321642210581));
#130539=CARTESIAN_POINT('Ctrl Pts',(-21.1017511664475,18.2341450028519,
0.183435695096556));
#130540=CARTESIAN_POINT('Ctrl Pts',(-21.1309074513388,18.3118700484822,
0.187549747982531));
#130541=CARTESIAN_POINT('Ctrl Pts',(-21.1600799709319,18.3896383727037,
0.19166609164121));
#130542=CARTESIAN_POINT('Ctrl Pts',(-21.1854596457913,18.4688174432781,
0.195782435299889));
#130543=CARTESIAN_POINT('Ctrl Pts',(-21.2069235819087,18.5489962552674,
0.199898778958568));
#130544=CARTESIAN_POINT('Ctrl Pts',(-21.228393434594,18.6291971686732,0.204016257293894));
#130545=CARTESIAN_POINT('Ctrl Pts',(-21.2459452949941,18.710397909727,0.208133735629219));
#130546=CARTESIAN_POINT('Ctrl Pts',(-21.259507205158,18.7921762223861,0.212251213964544));
#130547=CARTESIAN_POINT('Ctrl Pts',(-21.2730871889122,18.8740635187863,
0.216374179551669));
#130548=CARTESIAN_POINT('Ctrl Pts',(-21.2826665466436,18.9565294532014,
0.220497145138794));
#130549=CARTESIAN_POINT('Ctrl Pts',(-21.2882251802136,19.0391461994527,
0.224620110725918));
#130550=CARTESIAN_POINT('Ctrl Pts',(-21.2921215137894,19.0970565470744,
0.227510110407777));
#130551=CARTESIAN_POINT('Ctrl Pts',(-21.2940434286409,19.1550409048321,
0.230400110089637));
#130552=CARTESIAN_POINT('Ctrl Pts',(-21.2939992552734,19.212952690406,0.233290109771496));
#130553=CARTESIAN_POINT('',(-19.3957372685685,16.7380050975816,0.));
#130554=CARTESIAN_POINT('Origin',(-18.734,19.211,0.));
#130555=CARTESIAN_POINT('',(-21.2914665409842,19.2078565222202,0.166709890228504));
#130556=CARTESIAN_POINT('Ctrl Pts',(-19.3957372685684,16.7380050975816,
-1.38777878078145E-15));
#130557=CARTESIAN_POINT('Ctrl Pts',(-20.2191097516036,16.9583275322964,
0.0423919355604767));
#130558=CARTESIAN_POINT('Ctrl Pts',(-21.1334433095435,17.8262083452195,
0.0979618989699786));
#130559=CARTESIAN_POINT('Ctrl Pts',(-21.2935044203301,18.9424073589822,
0.153531862379481));
#130560=CARTESIAN_POINT('Ctrl Pts',(-21.2914665409842,19.2078565222202,
0.166709890228504));
#130561=CARTESIAN_POINT('Ctrl Pts',(-21.2914665409842,19.2078565222202,
0.166709890228504));
#130562=CARTESIAN_POINT('Ctrl Pts',(-21.286948837742,19.7963214614176,0.195923797939959));
#130563=CARTESIAN_POINT('Ctrl Pts',(-20.7940989485341,21.2477394666147,
0.267529641211891));
#130564=CARTESIAN_POINT('Ctrl Pts',(-18.3819425041677,22.2167212403437,
0.381527420044301));
#130565=CARTESIAN_POINT('Ctrl Pts',(-16.0159517247016,20.543342471876,0.508703226725737));
#130566=CARTESIAN_POINT('Ctrl Pts',(-16.1161223324435,18.2509927299605,
0.609322958308004));
#130567=CARTESIAN_POINT('Ctrl Pts',(-16.9218454618781,17.3761757922868,
0.667550754329794));
#130568=CARTESIAN_POINT('Ctrl Pts',(-17.1763093433856,17.1833020606948,
0.683386614791108));
#130569=CARTESIAN_POINT('Origin',(-18.734,19.211,-1.76670989022852));
#130570=CARTESIAN_POINT('',(-17.1739275293696,17.1801545964507,1.55000082814523));
#130571=CARTESIAN_POINT('',(-17.174464231106,17.180864983421,1.4832495057092));
#130572=CARTESIAN_POINT('',(-17.174464231106,17.180864983421,-1.76670989022852));
#130573=CARTESIAN_POINT('',(-21.2964371839251,19.2091455679848,1.0332901097715));
#130574=CARTESIAN_POINT('Ctrl Pts',(-21.2964371839251,19.2091455679848,
1.0332901097715));
#130575=CARTESIAN_POINT('Ctrl Pts',(-21.2904549152958,19.943534301501,1.06991597459592));
#130576=CARTESIAN_POINT('Ctrl Pts',(-20.5735369997583,21.5381319822354,
1.14893377498083));
#130577=CARTESIAN_POINT('Ctrl Pts',(-17.8654473773764,22.1108088143134,
1.27034351092621));
#130578=CARTESIAN_POINT('Ctrl Pts',(-15.8255860744598,20.0502991614889,
1.39751931760764));
#130579=CARTESIAN_POINT('Ctrl Pts',(-16.2862201749042,17.975545059775,1.49073842334732));
#130580=CARTESIAN_POINT('Ctrl Pts',(-17.0385457352419,17.2819918267254,
1.54156559352652));
#130581=CARTESIAN_POINT('Ctrl Pts',(-17.1739275293697,17.1801545964506,
1.55000082814524));
#130582=CARTESIAN_POINT('Ctrl Pts',(-17.1724222331904,17.1782439613541,
0.749817809475409));
#130583=CARTESIAN_POINT('Ctrl Pts',(-17.2346906102321,17.1297089569582,
0.753758634383762));
#130584=CARTESIAN_POINT('Ctrl Pts',(-17.9939164716346,16.5951983123874,
0.800091394852595));
#130585=CARTESIAN_POINT('Ctrl Pts',(-20.0126665959802,16.4672456410459,
0.888816090881905));
#130586=CARTESIAN_POINT('Ctrl Pts',(-21.2376963893991,18.1288877895766,
0.979366032738913));
#130587=CARTESIAN_POINT('Ctrl Pts',(-21.2973789824122,19.0935295298239,
1.02752403903544));
#130588=CARTESIAN_POINT('Ctrl Pts',(-21.2964371839251,19.2091455679848,
1.0332901097715));
#130589=CARTESIAN_POINT('',(-21.293928833175,19.2123417088597,0.966709918231326));
#130590=CARTESIAN_POINT('Ctrl Pts',(-17.1763093433856,17.1833020606948,
0.683386614791108));
#130591=CARTESIAN_POINT('Ctrl Pts',(-17.6030346207299,16.8598608865745,
0.709942689890274));
#130592=CARTESIAN_POINT('Ctrl Pts',(-18.9689508657168,16.3489929032406,
0.77889070054992));
#130593=CARTESIAN_POINT('Ctrl Pts',(-20.8878309534133,17.3253417136014,
0.873331792362382));
#130594=CARTESIAN_POINT('Ctrl Pts',(-21.2880302326024,18.6981275094852,
0.941216809075682));
#130595=CARTESIAN_POINT('Ctrl Pts',(-21.2904840132329,19.212339338513,0.966709890228504));
#130596=CARTESIAN_POINT('Ctrl Pts',(-21.2939996483763,19.212341757587,0.96670991880698));
#130597=CARTESIAN_POINT('Ctrl Pts',(-21.2939507844152,19.3055715065957,
0.971325635711016));
#130598=CARTESIAN_POINT('Ctrl Pts',(-21.2888049367591,19.3986231740038,
0.975941352615052));
#130599=CARTESIAN_POINT('Ctrl Pts',(-21.2786449918221,19.4909676152607,
0.980557069519088));
#130600=CARTESIAN_POINT('Ctrl Pts',(-21.2684492414382,19.5836374946964,
0.985189053027621));
#130601=CARTESIAN_POINT('Ctrl Pts',(-21.2532041189474,19.6755948890935,
0.989821036536154));
#130602=CARTESIAN_POINT('Ctrl Pts',(-21.233043385604,19.7663216697276,0.994453020044687));
#130603=CARTESIAN_POINT('Ctrl Pts',(-21.2127838215892,19.8574932054453,
0.999107710169702));
#130604=CARTESIAN_POINT('Ctrl Pts',(-21.1875604649916,19.9474217736623,
1.00376240029472));
#130605=CARTESIAN_POINT('Ctrl Pts',(-21.1575575151709,20.035602310607,1.00841709041973));
#130606=CARTESIAN_POINT('Ctrl Pts',(-21.1382431318488,20.0923684853426,
1.01141354476365));
#130607=CARTESIAN_POINT('Ctrl Pts',(-21.1169489972049,20.1484106839985,
1.01440999910756));
#130608=CARTESIAN_POINT('Ctrl Pts',(-21.09373439265,20.2035994137337,1.01740645345148));
#130609=CARTESIAN_POINT('Ctrl Pts',(-21.0613129697488,20.2806757706407,
1.02159128947824));
#130610=CARTESIAN_POINT('Ctrl Pts',(-21.0250509503441,20.3563053098801,
1.02577612550499));
#130611=CARTESIAN_POINT('Ctrl Pts',(-20.9850989621192,20.4300789403257,
1.02996096153175));
#130612=CARTESIAN_POINT('Ctrl Pts',(-20.9452038243206,20.503747593209,1.0341398426681));
#130613=CARTESIAN_POINT('Ctrl Pts',(-20.9016293644686,20.57556518195,1.03831872380444));
#130614=CARTESIAN_POINT('Ctrl Pts',(-20.8545742375833,20.6451425671453,
1.04249760494079));
#130615=CARTESIAN_POINT('Ctrl Pts',(-20.8066785783708,20.7159627933522,
1.04675113224046));
#130616=CARTESIAN_POINT('Ctrl Pts',(-20.7551768665489,20.784461551568,1.05100465954013));
#130617=CARTESIAN_POINT('Ctrl Pts',(-20.7003275707681,20.8502546734529,
1.0552581868398));
#130618=CARTESIAN_POINT('Ctrl Pts',(-20.6465383521066,20.9147762059378,
1.05942950584669));
#130619=CARTESIAN_POINT('Ctrl Pts',(-20.5895301046939,20.9766953864738,
1.06360082485357));
#130620=CARTESIAN_POINT('Ctrl Pts',(-20.5295892191722,21.0356806175308,
1.06777214386046));
#130621=CARTESIAN_POINT('Ctrl Pts',(-20.4696684423106,21.0946460605258,
1.07194206349469));
#130622=CARTESIAN_POINT('Ctrl Pts',(-20.4068173088282,21.1506791864532,
1.07611198312893));
#130623=CARTESIAN_POINT('Ctrl Pts',(-20.341359759635,21.203484530205,1.08028190276316));
#130624=CARTESIAN_POINT('Ctrl Pts',(-20.2759045394191,21.2562879951444,
1.0844516740318));
#130625=CARTESIAN_POINT('Ctrl Pts',(-20.2078434464218,21.3058636181016,
1.08862144530044));
#130626=CARTESIAN_POINT('Ctrl Pts',(-20.137533188394,21.3519564659461,1.09279121656908));
#130627=CARTESIAN_POINT('Ctrl Pts',(-20.06475858035,21.3996648520281,1.09710713686606));
#130628=CARTESIAN_POINT('Ctrl Pts',(-19.9895746527788,21.4436414961582,
1.10142305716305));
#130629=CARTESIAN_POINT('Ctrl Pts',(-19.9124075159363,21.4836538949838,
1.10573897746003));
#130630=CARTESIAN_POINT('Ctrl Pts',(-19.8377462631117,21.5223669527317,
1.10991474488706));
#130631=CARTESIAN_POINT('Ctrl Pts',(-19.7612290811574,21.5573691376404,
1.11409051231409));
#130632=CARTESIAN_POINT('Ctrl Pts',(-19.6832632220047,21.5884985458143,
1.11826627974112));
#130633=CARTESIAN_POINT('Ctrl Pts',(-19.6013721661871,21.6211951662332,
1.12265227647308));
#130634=CARTESIAN_POINT('Ctrl Pts',(-19.5178832893452,21.6496186365429,
1.12703827320505));
#130635=CARTESIAN_POINT('Ctrl Pts',(-19.4332854194226,21.6736408390553,
1.13142426993701));
#130636=CARTESIAN_POINT('Ctrl Pts',(-19.3486875495,21.6976630415677,1.13581026666898));
#130637=CARTESIAN_POINT('Ctrl Pts',(-19.2629812685386,21.7172839209455,
1.14019626340094));
#130638=CARTESIAN_POINT('Ctrl Pts',(-19.1766642026735,21.7324377651791,
1.1445822601329));
#130639=CARTESIAN_POINT('Ctrl Pts',(-19.0943081662955,21.7468962101513,
1.14876698655741));
#130640=CARTESIAN_POINT('Ctrl Pts',(-19.0110898392259,21.7573423936353,
1.15295171298191));
#130641=CARTESIAN_POINT('Ctrl Pts',(-18.9274347142603,21.76368153347,1.15713643940641));
#130642=CARTESIAN_POINT('Ctrl Pts',(-18.8438986152898,21.7700116538642,
1.16131521172795));
#130643=CARTESIAN_POINT('Ctrl Pts',(-18.7599274076619,21.7722463033441,
1.1654939840495));
#130644=CARTESIAN_POINT('Ctrl Pts',(-18.6759558050627,21.7703418824835,
1.16967275637105));
#130645=CARTESIAN_POINT('Ctrl Pts',(-18.5904814673451,21.7684033805762,
1.17392631097285));
#130646=CARTESIAN_POINT('Ctrl Pts',(-18.5050071952172,21.7621761204825,
1.17817986557465));
#130647=CARTESIAN_POINT('Ctrl Pts',(-18.4199959426925,21.7516694889329,
1.18243342017646));
#130648=CARTESIAN_POINT('Ctrl Pts',(-18.336630364455,21.7413662480271,1.18660463314431));
#130649=CARTESIAN_POINT('Ctrl Pts',(-18.2537105165071,21.7269479013071,
1.19077584611216));
#130650=CARTESIAN_POINT('Ctrl Pts',(-18.1716702192111,21.7084757691793,
1.19494705908001));
#130651=CARTESIAN_POINT('Ctrl Pts',(-18.0896574199584,21.6900098284904,
1.19911687395207));
#130652=CARTESIAN_POINT('Ctrl Pts',(-18.00852403427,21.6674929018324,1.20328668882412));
#130653=CARTESIAN_POINT('Ctrl Pts',(-17.9286938256586,21.6410374411864,
1.20745650369618));
#130654=CARTESIAN_POINT('Ctrl Pts',(-17.8488664302294,21.6145829128194,
1.21162617162576));
#130655=CARTESIAN_POINT('Ctrl Pts',(-17.770342556957,21.584190271937,1.21579583955533));
#130656=CARTESIAN_POINT('Ctrl Pts',(-17.6935296236616,21.5500214612017,
1.21996550748491));
#130657=CARTESIAN_POINT('Ctrl Pts',(-17.6140201264992,21.5146531339729,
1.22428155409569));
#130658=CARTESIAN_POINT('Ctrl Pts',(-17.5363444143668,21.4752387864926,
1.22859760070648));
#130659=CARTESIAN_POINT('Ctrl Pts',(-17.4609286758951,21.4320108968084,
1.23291364731726));
#130660=CARTESIAN_POINT('Ctrl Pts',(-17.3879658074203,21.3901889788191,
1.23708931605134));
#130661=CARTESIAN_POINT('Ctrl Pts',(-17.3171185275023,21.3447980781215,
1.24126498478542));
#130662=CARTESIAN_POINT('Ctrl Pts',(-17.2487433858239,21.2960929931411,
1.2454406535195));
#130663=CARTESIAN_POINT('Ctrl Pts',(-17.1769202848533,21.2449318525502,
1.24982688906864));
#130664=CARTESIAN_POINT('Ctrl Pts',(-17.1078256590939,21.1901138543223,
1.25421312461778));
#130665=CARTESIAN_POINT('Ctrl Pts',(-17.041831884048,21.1319807566333,1.25859936016692));
#130666=CARTESIAN_POINT('Ctrl Pts',(-16.975838109002,21.0738476589442,1.26298559571606));
#130667=CARTESIAN_POINT('Ctrl Pts',(-16.9129455463668,21.0123999214843,
1.2673718312652));
#130668=CARTESIAN_POINT('Ctrl Pts',(-16.8534788428352,20.9480204884962,
1.27175806681434));
#130669=CARTESIAN_POINT('Ctrl Pts',(-16.7967467984314,20.8866016333375,
1.27594259521698));
#130670=CARTESIAN_POINT('Ctrl Pts',(-16.7429212490902,20.8222861496523,
1.28012712361962));
#130671=CARTESIAN_POINT('Ctrl Pts',(-16.6923122077179,20.755380444983,1.28431165202226));
#130672=CARTESIAN_POINT('Ctrl Pts',(-16.6417752234728,20.6885700006219,
1.2884902224955));
#130673=CARTESIAN_POINT('Ctrl Pts',(-16.5944459257278,20.6191770244767,
1.29266879296874));
#130674=CARTESIAN_POINT('Ctrl Pts',(-16.5505962863688,20.5475433862398,
1.29684736344198));
#130675=CARTESIAN_POINT('Ctrl Pts',(-16.5059592440483,20.4746234309496,
1.30110096802755));
#130676=CARTESIAN_POINT('Ctrl Pts',(-16.464928391305,20.3993819010164,1.30535457261313));
#130677=CARTESIAN_POINT('Ctrl Pts',(-16.4277464801528,20.3222131668551,
1.3096081771987));
#130678=CARTESIAN_POINT('Ctrl Pts',(-16.3912866103988,20.2465429845164,
1.3137791803658));
#130679=CARTESIAN_POINT('Ctrl Pts',(-16.3585277410935,20.1690202117747,
1.31795018353289));
#130680=CARTESIAN_POINT('Ctrl Pts',(-16.3296531424778,20.0900427684265,
1.32212118669999));
#130681=CARTESIAN_POINT('Ctrl Pts',(-16.3007882398716,20.0110918454832,
1.32629078925587));
#130682=CARTESIAN_POINT('Ctrl Pts',(-16.2758051753869,19.9306876537767,
1.33046039181175));
#130683=CARTESIAN_POINT('Ctrl Pts',(-16.2548387836586,19.8492473371575,
1.33462999436763));
#130684=CARTESIAN_POINT('Ctrl Pts',(-16.2338731420879,19.7678099343955,
1.3387994477391));
#130685=CARTESIAN_POINT('Ctrl Pts',(-16.2169240014122,19.6853369261729,
1.34296890111056));
#130686=CARTESIAN_POINT('Ctrl Pts',(-16.2040757356768,19.6022585037908,
1.34713835448203));
#130687=CARTESIAN_POINT('Ctrl Pts',(-16.1907749795004,19.5162542241176,
1.35145464773317));
#130688=CARTESIAN_POINT('Ctrl Pts',(-16.1818694215614,19.4296016124724,
1.35577094098432));
#130689=CARTESIAN_POINT('Ctrl Pts',(-16.1773942973163,19.3427849801954,
1.36008723423546));
#130690=CARTESIAN_POINT('Ctrl Pts',(-16.1730651983007,19.2588012119819,
1.36426268498077));
#130691=CARTESIAN_POINT('Ctrl Pts',(-16.1728818000995,19.1746644338099,
1.36843813572608));
#130692=CARTESIAN_POINT('Ctrl Pts',(-16.1768228602554,19.0908123302179,
1.37261358647138));
#130693=CARTESIAN_POINT('Ctrl Pts',(-16.1809633247949,19.0027175923177,
1.37700030097545));
#130694=CARTESIAN_POINT('Ctrl Pts',(-16.1896565650922,18.9149376772193,
1.38138701547952));
#130695=CARTESIAN_POINT('Ctrl Pts',(-16.2028167402278,18.8279708817217,
1.38577372998358));
#130696=CARTESIAN_POINT('Ctrl Pts',(-16.2159769153634,18.7410040862242,
1.39016044448765));
#130697=CARTESIAN_POINT('Ctrl Pts',(-16.2336038344097,18.6548509637838,
1.39454715899172));
#130698=CARTESIAN_POINT('Ctrl Pts',(-16.2555511520629,18.5699919593647,
1.39893387349578));
#130699=CARTESIAN_POINT('Ctrl Pts',(-16.2764836516381,18.4890567352055,
1.403117751496));
#130700=CARTESIAN_POINT('Ctrl Pts',(-16.3014237423075,18.4089973657718,
1.40730162949622));
#130701=CARTESIAN_POINT('Ctrl Pts',(-16.3302816105931,18.3302401550779,
1.41148550749644));
#130702=CARTESIAN_POINT('Ctrl Pts',(-16.3591010931301,18.2515877045299,
1.41566382024535));
#130703=CARTESIAN_POINT('Ctrl Pts',(-16.3918278499508,18.1742344017226,
1.41984213299427));
#130704=CARTESIAN_POINT('Ctrl Pts',(-16.4283216558807,18.0985938810581,
1.42402044574318));
#130705=CARTESIAN_POINT('Ctrl Pts',(-16.4647778709001,18.0230312748773,
1.42819445456772));
#130706=CARTESIAN_POINT('Ctrl Pts',(-16.5049932294979,17.9491783588005,
1.43236846339226));
#130707=CARTESIAN_POINT('Ctrl Pts',(-16.5487790116004,17.87742989241,1.4365424722168));
#130708=CARTESIAN_POINT('Ctrl Pts',(-16.592535947135,17.8057286947195,1.44071373115717));
#130709=CARTESIAN_POINT('Ctrl Pts',(-16.6398583963984,17.7361295853038,
1.44488499009755));
#130710=CARTESIAN_POINT('Ctrl Pts',(-16.6905117887282,17.6690026166063,
1.44905624903793));
#130711=CARTESIAN_POINT('Ctrl Pts',(-16.7411445842141,17.6019029432907,
1.4532258118477));
#130712=CARTESIAN_POINT('Ctrl Pts',(-16.7951053526934,17.5372737786853,
1.45739537465747));
#130713=CARTESIAN_POINT('Ctrl Pts',(-16.852117123077,17.4754548874938,1.46156493746724));
#130714=CARTESIAN_POINT('Ctrl Pts',(-16.9091415856326,17.4136222339513,
1.46573542852056));
#130715=CARTESIAN_POINT('Ctrl Pts',(-16.9692180992007,17.3546014460044,
1.46990591957388));
#130716=CARTESIAN_POINT('Ctrl Pts',(-17.0320310770586,17.2986972558349,
1.4740764106272));
#130717=CARTESIAN_POINT('Ctrl Pts',(-17.0780839607524,17.2577097202065,
1.47713410898787));
#130718=CARTESIAN_POINT('Ctrl Pts',(-17.1256069925995,17.2183967783007,
1.48019180734854));
#130719=CARTESIAN_POINT('Ctrl Pts',(-17.174464231106,17.180864983421,1.4832495057092));
#130720=CARTESIAN_POINT('Origin',(-18.734,19.211,-1.76670989022852));
#130721=CARTESIAN_POINT('',(-17.174464231106,17.180864983421,2.34989189146289));
#130722=CARTESIAN_POINT('',(-17.174464231106,17.180864983421,2.28327545488353));
#130723=CARTESIAN_POINT('',(-17.174464231106,17.180864983421,-1.76670989022852));
#130724=CARTESIAN_POINT('',(-21.2937660440385,19.2099923323681,1.83329006739986));
#130725=CARTESIAN_POINT('Ctrl Pts',(-21.293999801981,19.2099930953476,1.8332901097715));
#130726=CARTESIAN_POINT('Ctrl Pts',(-21.2940336318695,19.2960037294466,
1.83754657624536));
#130727=CARTESIAN_POINT('Ctrl Pts',(-21.289728450138,19.3819895209311,1.84180304271922));
#130728=CARTESIAN_POINT('Ctrl Pts',(-21.2811180404437,19.4674950058893,
1.84605950919308));
#130729=CARTESIAN_POINT('Ctrl Pts',(-21.2725026284394,19.5530501661775,
1.85031844850686));
#130730=CARTESIAN_POINT('Ctrl Pts',(-21.2595770559904,19.6381240344265,
1.85457738782065));
#130731=CARTESIAN_POINT('Ctrl Pts',(-21.2424267246312,19.7222683905308,
1.85883632713443));
#130732=CARTESIAN_POINT('Ctrl Pts',(-21.2252479654662,19.8065522214573,
1.86310232592114));
#130733=CARTESIAN_POINT('Ctrl Pts',(-21.203830549429,19.8899030384947,1.86736832470785));
#130734=CARTESIAN_POINT('Ctrl Pts',(-21.17831059956,19.9718848092049,1.87163432349455));
#130735=CARTESIAN_POINT('Ctrl Pts',(-21.1527682031271,20.0539386885619,
1.87590407452273));
#130736=CARTESIAN_POINT('Ctrl Pts',(-21.1231162332672,20.1346207166622,
1.88017382555091));
#130737=CARTESIAN_POINT('Ctrl Pts',(-21.0895392515833,20.2135142563825,
1.88444357657908));
#130738=CARTESIAN_POINT('Ctrl Pts',(-21.0558918629605,20.2925732264768,
1.88872228076758));
#130739=CARTESIAN_POINT('Ctrl Pts',(-21.0183032080418,20.3698358258174,
1.89300098495607));
#130740=CARTESIAN_POINT('Ctrl Pts',(-20.9770042478451,20.4449092122797,
1.89727968914457));
#130741=CARTESIAN_POINT('Ctrl Pts',(-20.9482314695913,20.4972124637696,
1.90026064087417));
#130742=CARTESIAN_POINT('Ctrl Pts',(-20.9176587209492,20.5484536579338,
1.90324159260377));
#130743=CARTESIAN_POINT('Ctrl Pts',(-20.8853760800086,20.5985089053289,
1.90622254433338));
#130744=CARTESIAN_POINT('Ctrl Pts',(-20.8400579767351,20.6687760459572,
1.91040717961721));
#130745=CARTESIAN_POINT('Ctrl Pts',(-20.79120937469,20.7369513806192,1.91459181490104));
#130746=CARTESIAN_POINT('Ctrl Pts',(-20.7390496454785,20.8026582293842,
1.91877645018487));
#130747=CARTESIAN_POINT('Ctrl Pts',(-20.6869641590402,20.8682715527659,
1.92295512916998));
#130748=CARTESIAN_POINT('Ctrl Pts',(-20.631577190453,20.9314230120947,1.92713380815509));
#130749=CARTESIAN_POINT('Ctrl Pts',(-20.5731519436452,20.9917639170272,
1.9313124871402));
#130750=CARTESIAN_POINT('Ctrl Pts',(-20.5136794822353,21.0531863728336,
1.93556606480165));
#130751=CARTESIAN_POINT('Ctrl Pts',(-20.4510590119848,21.1116961211984,
1.93981964246309));
#130752=CARTESIAN_POINT('Ctrl Pts',(-20.3856118363234,21.1669596984898,
1.94407322012453));
#130753=CARTESIAN_POINT('Ctrl Pts',(-20.3214334643362,21.2211518983045,
1.94824433502252));
#130754=CARTESIAN_POINT('Ctrl Pts',(-20.2545373774524,21.2722223583837,
1.9524154499205));
#130755=CARTESIAN_POINT('Ctrl Pts',(-20.185263188972,21.3198942970986,1.95658656481849));
#130756=CARTESIAN_POINT('Ctrl Pts',(-20.1160122460259,21.3675502390951,
1.96075628006393));
#130757=CARTESIAN_POINT('Ctrl Pts',(-20.0443851649613,21.4118096640091,
1.96492599530937));
#130758=CARTESIAN_POINT('Ctrl Pts',(-19.9707522614864,21.4524378964647,
1.9690957105548));
#130759=CARTESIAN_POINT('Ctrl Pts',(-19.8971219781181,21.493064683231,1.97326527742773));
#130760=CARTESIAN_POINT('Ctrl Pts',(-19.8214864174478,21.5300603129432,
1.97743484430066));
#130761=CARTESIAN_POINT('Ctrl Pts',(-19.7442411220081,21.5632357185035,
1.98160441117359));
#130762=CARTESIAN_POINT('Ctrl Pts',(-19.6642800151963,21.5975775141098,
1.98592057282703));
#130763=CARTESIAN_POINT('Ctrl Pts',(-19.5825943571934,21.6278252448874,
1.99023673448046));
#130764=CARTESIAN_POINT('Ctrl Pts',(-19.4996442824007,21.653823946343,1.9945528961339));
#130765=CARTESIAN_POINT('Ctrl Pts',(-19.4193962595356,21.6789757547542,
1.99872846125449));
#130766=CARTESIAN_POINT('Ctrl Pts',(-19.3379653982308,21.7001510303436,
2.00290402637507));
#130767=CARTESIAN_POINT('Ctrl Pts',(-19.2557808536483,21.7172611078589,
2.00707959149566));
#130768=CARTESIAN_POINT('Ctrl Pts',(-19.1694454234894,21.7352353621403,
2.01146605141552));
#130769=CARTESIAN_POINT('Ctrl Pts',(-19.0822787502276,21.7487228765315,
2.01585251133538));
#130770=CARTESIAN_POINT('Ctrl Pts',(-18.9947846789878,21.7576824205631,
2.02023897125524));
#130771=CARTESIAN_POINT('Ctrl Pts',(-18.907290607748,21.7666419645947,2.0246254311751));
#130772=CARTESIAN_POINT('Ctrl Pts',(-18.8194697218411,21.7710735849931,
2.02901189109496));
#130773=CARTESIAN_POINT('Ctrl Pts',(-18.7318236815475,21.7709990749291,
2.03339835101482));
#130774=CARTESIAN_POINT('Ctrl Pts',(-18.6482103252724,21.7709279931495,
2.03758298542427));
#130775=CARTESIAN_POINT('Ctrl Pts',(-18.5644448542258,21.7667560675599,
2.04176761983373));
#130776=CARTESIAN_POINT('Ctrl Pts',(-18.4809627381372,21.7584638651233,
2.04595225424318));
#130777=CARTESIAN_POINT('Ctrl Pts',(-18.3975994484511,21.7501834656048,
2.05013093234635));
#130778=CARTESIAN_POINT('Ctrl Pts',(-18.3145191664661,21.7377944834636,
2.05430961044952));
#130779=CARTESIAN_POINT('Ctrl Pts',(-18.232157552723,21.7213294919414,2.05848828855269));
#130780=CARTESIAN_POINT('Ctrl Pts',(-18.1483196667192,21.7045693773741,
2.06274186643367));
#130781=CARTESIAN_POINT('Ctrl Pts',(-18.0652269487603,21.6835856916693,
2.06699544431465));
#130782=CARTESIAN_POINT('Ctrl Pts',(-17.9833337046586,21.6584681025579,
2.07124902219563));
#130783=CARTESIAN_POINT('Ctrl Pts',(-17.9030281203093,21.6338374667446,
2.07542013619965));
#130784=CARTESIAN_POINT('Ctrl Pts',(-17.8238763766489,21.6052319257642,
2.07959125020367));
#130785=CARTESIAN_POINT('Ctrl Pts',(-17.7462950293383,21.57278722389,2.08376236420769));
#130786=CARTESIAN_POINT('Ctrl Pts',(-17.6687397151515,21.5403534091294,
2.08793207855663));
#130787=CARTESIAN_POINT('Ctrl Pts',(-17.592754174823,21.5040831693336,2.09210179290557));
#130788=CARTESIAN_POINT('Ctrl Pts',(-17.5187361779587,21.4641608559616,
2.09627150725451));
#130789=CARTESIAN_POINT('Ctrl Pts',(-17.4447208149285,21.4242399631732,
2.1004410732296));
#130790=CARTESIAN_POINT('Ctrl Pts',(-17.3726732606489,21.3806674743246,
2.10461063920469));
#130791=CARTESIAN_POINT('Ctrl Pts',(-17.3029665901884,21.3336736395411,
2.10878020517978));
#130792=CARTESIAN_POINT('Ctrl Pts',(-17.2308091202126,21.2850275601913,
2.11309636788948));
#130793=CARTESIAN_POINT('Ctrl Pts',(-17.1611606450012,21.2327153644064,
2.11741253059919));
#130794=CARTESIAN_POINT('Ctrl Pts',(-17.0944005275883,21.1770400733625,
2.12172869330889));
#130795=CARTESIAN_POINT('Ctrl Pts',(-17.0298151129693,21.1231783982271,
2.12590425753753));
#130796=CARTESIAN_POINT('Ctrl Pts',(-16.9679330839598,21.06616972251,2.13007982176617));
#130797=CARTESIAN_POINT('Ctrl Pts',(-16.9090612874293,21.006326904873,2.13425538599481));
#130798=CARTESIAN_POINT('Ctrl Pts',(-16.8472160178363,20.9434615702293,
2.13864184794505));
#130799=CARTESIAN_POINT('Ctrl Pts',(-16.7886934533832,20.8774687014113,
2.14302830989529));
#130800=CARTESIAN_POINT('Ctrl Pts',(-16.733800984635,20.8087496358731,2.14741477184553));
#130801=CARTESIAN_POINT('Ctrl Pts',(-16.6789085158868,20.740030570335,2.15180123379577));
#130802=CARTESIAN_POINT('Ctrl Pts',(-16.6276464192901,20.6685858238429,
2.156187695746));
#130803=CARTESIAN_POINT('Ctrl Pts',(-16.5802679097319,20.5948490103148,
2.16057415769624));
#130804=CARTESIAN_POINT('Ctrl Pts',(-16.5350693576789,20.5245049400697,
2.16475879184019));
#130805=CARTESIAN_POINT('Ctrl Pts',(-16.4932366287838,20.4518132565164,
2.16894342598413));
#130806=CARTESIAN_POINT('Ctrl Pts',(-16.4550217746911,20.3771296019601,
2.17312806012807));
#130807=CARTESIAN_POINT('Ctrl Pts',(-16.4168613147564,20.3025522504266,
2.17730673795853));
#130808=CARTESIAN_POINT('Ctrl Pts',(-16.3823087086574,20.225988965771,2.18148541578898));
#130809=CARTESIAN_POINT('Ctrl Pts',(-16.3515723822765,20.1478237007615,
2.18566409361943));
#130810=CARTESIAN_POINT('Ctrl Pts',(-16.320285126975,20.0682573735512,2.18991767156769));
#130811=CARTESIAN_POINT('Ctrl Pts',(-16.2929525719373,19.9870314754766,
2.19417124951595));
#130812=CARTESIAN_POINT('Ctrl Pts',(-16.2697452279946,19.904576541305,2.19842482746421));
#130813=CARTESIAN_POINT('Ctrl Pts',(-16.2469878054675,19.8237201632108,
2.20259594117976));
#130814=CARTESIAN_POINT('Ctrl Pts',(-16.2281972006316,19.74168244169,2.20676705489531));
#130815=CARTESIAN_POINT('Ctrl Pts',(-16.2134847477526,19.6588871098706,
2.21093816861085));
#130816=CARTESIAN_POINT('Ctrl Pts',(-16.1987772317894,19.5761195608809,
2.21510788266606));
#130817=CARTESIAN_POINT('Ctrl Pts',(-16.1881452304063,19.492595359046,2.21927759672127));
#130818=CARTESIAN_POINT('Ctrl Pts',(-16.1816490383843,19.408748751549,2.22344731077647));
#130819=CARTESIAN_POINT('Ctrl Pts',(-16.1751530775285,19.3249051277229,
2.22761687645293));
#130820=CARTESIAN_POINT('Ctrl Pts',(-16.1727926681034,19.2407395797697,
2.2317864421294));
#130821=CARTESIAN_POINT('Ctrl Pts',(-16.1745761446913,19.1566904347585,
2.23595600780586));
#130822=CARTESIAN_POINT('Ctrl Pts',(-16.1764223263664,19.0696862136876,
2.24027217085351));
#130823=CARTESIAN_POINT('Ctrl Pts',(-16.1827092038737,18.9828072606513,
2.24458833390116));
#130824=CARTESIAN_POINT('Ctrl Pts',(-16.1933873263915,18.896536579711,2.24890449694881));
#130825=CARTESIAN_POINT('Ctrl Pts',(-16.2037176087823,18.8130761685133,
2.25308006086957));
#130826=CARTESIAN_POINT('Ctrl Pts',(-16.2181573115163,18.7301854648529,
2.25725562479034));
#130827=CARTESIAN_POINT('Ctrl Pts',(-16.2366094603928,18.6482918228064,
2.2614311887111));
#130828=CARTESIAN_POINT('Ctrl Pts',(-16.2559935873461,18.5622619102627,
2.2658176513222));
#130829=CARTESIAN_POINT('Ctrl Pts',(-16.2798059943656,18.4773329921969,
2.27020411393329));
#130830=CARTESIAN_POINT('Ctrl Pts',(-16.3078756047625,18.3939807720541,
2.27459057654439));
#130831=CARTESIAN_POINT('Ctrl Pts',(-16.3359452151593,18.3106285519114,
2.27897703915549));
#130832=CARTESIAN_POINT('Ctrl Pts',(-16.3682717448907,18.2288535413148,
2.28336350176658));
#130833=CARTESIAN_POINT('Ctrl Pts',(-16.4046276535509,18.1491033611513,
2.28774996437768));
#130834=CARTESIAN_POINT('Ctrl Pts',(-16.4393112999297,18.0730214490394,
2.29193466292225));
#130835=CARTESIAN_POINT('Ctrl Pts',(-16.4777908907348,17.9984989913647,
2.29611936146682));
#130836=CARTESIAN_POINT('Ctrl Pts',(-16.5199038099004,17.925940444576,2.30030406001139));
#130837=CARTESIAN_POINT('Ctrl Pts',(-16.5619476212562,17.8535009672404,
2.30448189141503));
#130838=CARTESIAN_POINT('Ctrl Pts',(-16.6076126789151,17.7830193882166,
2.30865972281866));
#130839=CARTESIAN_POINT('Ctrl Pts',(-16.6566890878976,17.7148785562462,
2.3128375542223));
#130840=CARTESIAN_POINT('Ctrl Pts',(-16.7057182446351,17.6468033323214,
2.31701136308401));
#130841=CARTESIAN_POINT('Ctrl Pts',(-16.7581519651251,17.581064752514,2.32118517194572));
#130842=CARTESIAN_POINT('Ctrl Pts',(-16.8137358428997,17.518018734021,2.32535898080743));
#130843=CARTESIAN_POINT('Ctrl Pts',(-16.8692865796241,17.4550103057672,
2.32953030109846));
#130844=CARTESIAN_POINT('Ctrl Pts',(-16.9279834436642,17.3946915976913,
2.33370162138948));
#130845=CARTESIAN_POINT('Ctrl Pts',(-16.989531117982,17.337386293904,2.33787294168051));
#130846=CARTESIAN_POINT('Ctrl Pts',(-17.0486441689456,17.2823477992604,
2.34187925827464));
#130847=CARTESIAN_POINT('Ctrl Pts',(-17.1103864544927,17.2300890910807,
2.34588557486876));
#130848=CARTESIAN_POINT('Ctrl Pts',(-17.174464231106,17.180864983421,2.34989189146289));
#130849=CARTESIAN_POINT('Ctrl Pts',(-17.1739275293697,17.1801545964506,
1.55000082814524));
#130850=CARTESIAN_POINT('Ctrl Pts',(-17.7189175982832,16.7702008098065,
1.583957529087));
#130851=CARTESIAN_POINT('Ctrl Pts',(-19.3278236760405,16.3317553949947,
1.66030616558923));
#130852=CARTESIAN_POINT('Ctrl Pts',(-21.0477248457009,17.6266607733557,
1.75473569409313));
#130853=CARTESIAN_POINT('Ctrl Pts',(-21.2914432046423,18.8451666090485,
1.81520852165527));
#130854=CARTESIAN_POINT('Ctrl Pts',(-21.2901594433486,19.2099805605233,
1.83328941365693));
#130855=CARTESIAN_POINT('',(-21.2939995273705,19.2125555907563,1.76670989019937));
#130856=CARTESIAN_POINT('Ctrl Pts',(-17.174464231106,17.180864983421,1.4832495057092));
#130857=CARTESIAN_POINT('Ctrl Pts',(-17.2411722071231,17.1296203746538,
1.4874243808177));
#130858=CARTESIAN_POINT('Ctrl Pts',(-17.3103683086997,17.0816980612811,
1.49159925592621));
#130859=CARTESIAN_POINT('Ctrl Pts',(-17.381681384701,17.0373315886006,1.49577413103471));
#130860=CARTESIAN_POINT('Ctrl Pts',(-17.4530395947168,16.992937036399,1.49995164841983));
#130861=CARTESIAN_POINT('Ctrl Pts',(-17.5265170440586,16.9521030273264,
1.50412916580495));
#130862=CARTESIAN_POINT('Ctrl Pts',(-17.6017183868702,16.9150169102173,
1.50830668319008));
#130863=CARTESIAN_POINT('Ctrl Pts',(-17.6770427439097,16.8778701277013,
1.51249103415099));
#130864=CARTESIAN_POINT('Ctrl Pts',(-17.7540962011118,16.8444836556603,
1.51667538511191));
#130865=CARTESIAN_POINT('Ctrl Pts',(-17.8324643241877,16.8149963636844,
1.52085973607283));
#130866=CARTESIAN_POINT('Ctrl Pts',(-17.8652394801244,16.8026641735702,
1.52260971744095));
#130867=CARTESIAN_POINT('Ctrl Pts',(-17.8982444142715,16.791013376961,1.52435969880908));
#130868=CARTESIAN_POINT('Ctrl Pts',(-17.9314482086486,16.7800514974195,
1.52610968017721));
#130869=CARTESIAN_POINT('Ctrl Pts',(-18.0108467907137,16.7538389000734,
1.53029432358547));
#130870=CARTESIAN_POINT('Ctrl Pts',(-18.0916786884036,16.7314715385808,
1.53447896699374));
#130871=CARTESIAN_POINT('Ctrl Pts',(-18.1735366057567,16.7131047292344,
1.538663610402));
#130872=CARTESIAN_POINT('Ctrl Pts',(-18.2552780138067,16.6947640615763,
1.5428422977598));
#130873=CARTESIAN_POINT('Ctrl Pts',(-18.3380420957822,16.6804127357782,
1.5470209851176));
#130874=CARTESIAN_POINT('Ctrl Pts',(-18.421405029143,16.6701567572566,1.5511996724754));
#130875=CARTESIAN_POINT('Ctrl Pts',(-18.5062619492397,16.6597169764711,
1.5554532480747));
#130876=CARTESIAN_POINT('Ctrl Pts',(-18.5917389394536,16.6535209329784,
1.559706823674));
#130877=CARTESIAN_POINT('Ctrl Pts',(-18.6773765359446,16.651626290805,1.5639603992733));
#130878=CARTESIAN_POINT('Ctrl Pts',(-18.7613541238536,16.6497683745839,
1.56813152309571));
#130879=CARTESIAN_POINT('Ctrl Pts',(-18.8454856660802,16.6520466005361,
1.57230264691812));
#130880=CARTESIAN_POINT('Ctrl Pts',(-18.9293330503143,16.6584630268192,
1.57647377074053));
#130881=CARTESIAN_POINT('Ctrl Pts',(-19.0131523026761,16.6648773003091,
1.58064349509743));
#130882=CARTESIAN_POINT('Ctrl Pts',(-19.0966871280817,16.6754269816346,
1.58481321945433));
#130883=CARTESIAN_POINT('Ctrl Pts',(-19.1795019710685,16.6900620805395,
1.58898294381123));
#130884=CARTESIAN_POINT('Ctrl Pts',(-19.2623138707192,16.7046966592958,
1.59315251997126));
#130885=CARTESIAN_POINT('Ctrl Pts',(-19.3444053859658,16.7234162860397,
1.59732209613129));
#130886=CARTESIAN_POINT('Ctrl Pts',(-19.4253499785112,16.7461196363287,
1.60149167229132));
#130887=CARTESIAN_POINT('Ctrl Pts',(-19.5091400540413,16.7696210880709,
1.60580782350526));
#130888=CARTESIAN_POINT('Ctrl Pts',(-19.5917005594529,16.7973914247812,
1.6101239747192));
#130889=CARTESIAN_POINT('Ctrl Pts',(-19.6725761219549,16.8292622177712,
1.61444012593315));
#130890=CARTESIAN_POINT('Ctrl Pts',(-19.7508175783492,16.8600949833538,
1.61861570068712));
#130891=CARTESIAN_POINT('Ctrl Pts',(-19.8274817539353,16.8947649658156,
1.62279127544109));
#130892=CARTESIAN_POINT('Ctrl Pts',(-19.9021790183312,16.9330716031599,
1.62696685019507));
#130893=CARTESIAN_POINT('Ctrl Pts',(-19.9806484617505,16.9733127088547,
1.631353289639));
#130894=CARTESIAN_POINT('Ctrl Pts',(-20.0569466030573,17.0175671444772,
1.63573972908293));
#130895=CARTESIAN_POINT('Ctrl Pts',(-20.130655495903,17.0655505305965,1.64012616852686));
#130896=CARTESIAN_POINT('Ctrl Pts',(-20.2043643887487,17.1135339167158,
1.64451260797079));
#130897=CARTESIAN_POINT('Ctrl Pts',(-20.275483608608,17.1652458506084,1.64889904741472));
#130898=CARTESIAN_POINT('Ctrl Pts',(-20.3436364934689,17.2203542859431,
1.65328548685865));
#130899=CARTESIAN_POINT('Ctrl Pts',(-20.4078056279229,17.2722414599601,
1.6574155251252));
#130900=CARTESIAN_POINT('Ctrl Pts',(-20.4695977832764,17.3273436084189,
1.66154556339175));
#130901=CARTESIAN_POINT('Ctrl Pts',(-20.5286666498128,17.3854119807444,
1.6656756016583));
#130902=CARTESIAN_POINT('Ctrl Pts',(-20.5888757459544,17.4446012697411,
1.66988536368084));
#130903=CARTESIAN_POINT('Ctrl Pts',(-20.6462548736576,17.5068722657662,
1.67409512570339));
#130904=CARTESIAN_POINT('Ctrl Pts',(-20.7004701683271,17.5719163910649,
1.67830488772593));
#130905=CARTESIAN_POINT('Ctrl Pts',(-20.7535207653518,17.6355631848541,
1.68242421217099));
#130906=CARTESIAN_POINT('Ctrl Pts',(-20.8035417767949,17.7018647731871,
1.68654353661605));
#130907=CARTESIAN_POINT('Ctrl Pts',(-20.850256855771,17.7704942136866,1.69066286106111));
#130908=CARTESIAN_POINT('Ctrl Pts',(-20.8969436374088,17.8390820823739,
1.69477969025368));
#130909=CARTESIAN_POINT('Ctrl Pts',(-20.9403281944971,17.9099946152069,
1.69889651944625));
#130910=CARTESIAN_POINT('Ctrl Pts',(-20.9801755816481,17.9828732734739,
1.70301334863882));
#130911=CARTESIAN_POINT('Ctrl Pts',(-21.0200115244872,18.05573100073,1.70712899546334));
#130912=CARTESIAN_POINT('Ctrl Pts',(-21.0563120879347,18.1305533171676,
1.71124464228787));
#130913=CARTESIAN_POINT('Ctrl Pts',(-21.088887451558,18.206955633204,1.71536028911239));
#130914=CARTESIAN_POINT('Ctrl Pts',(-21.1227568123705,18.2863928925596,
1.71963942253631));
#130915=CARTESIAN_POINT('Ctrl Pts',(-21.1525985841264,18.3675378137456,
1.72391855596022));
#130916=CARTESIAN_POINT('Ctrl Pts',(-21.1782545843983,18.4499352677678,
1.72819768938414));
#130917=CARTESIAN_POINT('Ctrl Pts',(-21.2029529680662,18.5292572162836,
1.73231710308656));
#130918=CARTESIAN_POINT('Ctrl Pts',(-21.2237724320015,18.6097393655103,
1.73643651678898));
#130919=CARTESIAN_POINT('Ctrl Pts',(-21.2406233770012,18.6909622649548,
1.7405559304914));
#130920=CARTESIAN_POINT('Ctrl Pts',(-21.2574836176246,18.7722299700469,
1.74467761661945));
#130921=CARTESIAN_POINT('Ctrl Pts',(-21.2703709121366,18.8542387712825,
1.74879930274751));
#130922=CARTESIAN_POINT('Ctrl Pts',(-21.279247341302,18.9365624449985,1.75292098887556));
#130923=CARTESIAN_POINT('Ctrl Pts',(-21.2881358451795,19.0189981045868,
1.75704828178227));
#130924=CARTESIAN_POINT('Ctrl Pts',(-21.2930025796067,19.1017490200354,
1.76117557468897));
#130925=CARTESIAN_POINT('Ctrl Pts',(-21.2938616787506,19.1843882419918,
1.76530286759568));
#130926=CARTESIAN_POINT('Ctrl Pts',(-21.293959303024,19.19377900214,1.76577187513024));
#130927=CARTESIAN_POINT('Ctrl Pts',(-21.2940052315681,19.2031683255366,
1.76624088266481));
#130928=CARTESIAN_POINT('Ctrl Pts',(-21.2939995273705,19.2125555907563,
1.76670989019937));
#130929=CARTESIAN_POINT('Ctrl Pts',(-21.2939995273702,19.2125555913393,
1.7667098902285));
#130930=CARTESIAN_POINT('Ctrl Pts',(-21.2939437779102,19.3043011465908,
1.77129369133236));
#130931=CARTESIAN_POINT('Ctrl Pts',(-21.2889563823285,19.3958958079181,
1.77587749243622));
#130932=CARTESIAN_POINT('Ctrl Pts',(-21.2790836672346,19.4869513123279,
1.78046129354008));
#130933=CARTESIAN_POINT('Ctrl Pts',(-21.2700706759975,19.5700776312323,
1.78464593361015));
#130934=CARTESIAN_POINT('Ctrl Pts',(-21.2569640809886,19.6529166096931,
1.78883057368023));
#130935=CARTESIAN_POINT('Ctrl Pts',(-21.2397911343996,19.7350331962428,
1.7930152137503));
#130936=CARTESIAN_POINT('Ctrl Pts',(-21.2226426310956,19.817032901329,1.79719389757114));
#130937=CARTESIAN_POINT('Ctrl Pts',(-21.2014393661311,19.8983118104412,
1.80137258139199));
#130938=CARTESIAN_POINT('Ctrl Pts',(-21.1762603200948,19.9784402445079,
1.80555126521283));
#130939=CARTESIAN_POINT('Ctrl Pts',(-21.150630001539,20.0600047838296,1.80980484167153));
#130940=CARTESIAN_POINT('Ctrl Pts',(-21.1208800342882,20.1403767226468,
1.81405841813022));
#130941=CARTESIAN_POINT('Ctrl Pts',(-21.0871481593181,20.21911395204,1.81831199458892));
#130942=CARTESIAN_POINT('Ctrl Pts',(-21.0540701851445,20.2963248406336,
1.82248311440869));
#130943=CARTESIAN_POINT('Ctrl Pts',(-21.0171634957605,20.3719633904436,
1.82665423422847));
#130944=CARTESIAN_POINT('Ctrl Pts',(-20.9766076076857,20.4456299518278,
1.83082535404824));
#130945=CARTESIAN_POINT('Ctrl Pts',(-20.9360653282555,20.5192717941858,
1.83499507423679));
#130946=CARTESIAN_POINT('Ctrl Pts',(-20.8918765036875,20.5909425596168,
1.83916479442534));
#130947=CARTESIAN_POINT('Ctrl Pts',(-20.8442669697396,20.6602664752991,
1.84333451461389));
#130948=CARTESIAN_POINT('Ctrl Pts',(-20.7966591297285,20.7295879244518,
1.84750408644471));
#130949=CARTESIAN_POINT('Ctrl Pts',(-20.7456310834599,20.7965623111441,
1.85167365827553));
#130950=CARTESIAN_POINT('Ctrl Pts',(-20.691451661047,20.8608433242779,1.85584323010635));
#130951=CARTESIAN_POINT('Ctrl Pts',(-20.6353675257683,20.9273841782754,
1.86015938594928));
#130952=CARTESIAN_POINT('Ctrl Pts',(-20.5759066466623,20.9910383508709,
1.86447554179221));
#130953=CARTESIAN_POINT('Ctrl Pts',(-20.5134108769448,21.0514610647907,
1.86879169763514));
#130954=CARTESIAN_POINT('Ctrl Pts',(-20.4529507187175,21.1099156907698,
1.87296726769975));
#130955=CARTESIAN_POINT('Ctrl Pts',(-20.3896507250023,21.1653458615584,
1.87714283776436));
#130956=CARTESIAN_POINT('Ctrl Pts',(-20.3238547775404,21.2174799491478,
1.88131840782897));
#130957=CARTESIAN_POINT('Ctrl Pts',(-20.2547359396678,21.2722469627211,
1.88570485656106));
#130958=CARTESIAN_POINT('Ctrl Pts',(-20.1828628806314,21.3233758659983,
1.89009130529315));
#130959=CARTESIAN_POINT('Ctrl Pts',(-20.1086675060193,21.3706039562602,
1.89447775402525));
#130960=CARTESIAN_POINT('Ctrl Pts',(-20.0344721314073,21.417832046522,1.89886420275734));
#130961=CARTESIAN_POINT('Ctrl Pts',(-19.9579549835793,21.4611591040721,
1.90325065148943));
#130962=CARTESIAN_POINT('Ctrl Pts',(-19.8795742651121,21.5003797420072,
1.90763710022152));
#130963=CARTESIAN_POINT('Ctrl Pts',(-19.8047997208671,21.5377958997554,
1.91182173531048));
#130964=CARTESIAN_POINT('Ctrl Pts',(-19.7280509965254,21.5716144630821,
1.91600637039945));
#130965=CARTESIAN_POINT('Ctrl Pts',(-19.6497086514407,21.6016228614477,
1.92019100548841));
#130966=CARTESIAN_POINT('Ctrl Pts',(-19.5714778164362,21.6315885467837,
1.92436968429672));
#130967=CARTESIAN_POINT('Ctrl Pts',(-19.4916582921888,21.6577546763365,
1.92854836310503));
#130968=CARTESIAN_POINT('Ctrl Pts',(-19.4106541204075,21.6799550828915,
1.93272704191334));
#130969=CARTESIAN_POINT('Ctrl Pts',(-19.3281980247988,21.7025534109181,
1.93698061962124));
#130970=CARTESIAN_POINT('Ctrl Pts',(-19.2445148260133,21.7210422324063,
1.94123419732914));
#130971=CARTESIAN_POINT('Ctrl Pts',(-19.1600508252197,21.7352980597246,
1.94548777503704));
#130972=CARTESIAN_POINT('Ctrl Pts',(-19.0772243047676,21.7492775132415,
1.94965888980437));
#130973=CARTESIAN_POINT('Ctrl Pts',(-18.9936474610422,21.7591865556584,
1.95383000457171));
#130974=CARTESIAN_POINT('Ctrl Pts',(-18.9097535041071,21.7649598089622,
1.95800111933905));
#130975=CARTESIAN_POINT('Ctrl Pts',(-18.8258876981392,21.7707311250267,
1.96217083447142));
#130976=CARTESIAN_POINT('Ctrl Pts',(-18.7417054488562,21.7723693765771,
1.9663405496038));
#130977=CARTESIAN_POINT('Ctrl Pts',(-18.6576449614606,21.769861056816,1.97051026473618));
#130978=CARTESIAN_POINT('Ctrl Pts',(-18.5735874648611,21.7673528262987,
1.97467983151386));
#130979=CARTESIAN_POINT('Ctrl Pts',(-18.4896521813381,21.7606983323727,
1.97884939829154));
#130980=CARTESIAN_POINT('Ctrl Pts',(-18.4062758155005,21.7499361667624,
1.98301896506922));
#130981=CARTESIAN_POINT('Ctrl Pts',(-18.3199680751374,21.7387956212864,
1.9873351268887));
#130982=CARTESIAN_POINT('Ctrl Pts',(-18.2342598094107,21.7232532494571,
1.99165128870818));
#130983=CARTESIAN_POINT('Ctrl Pts',(-18.1496259628381,21.7034098749385,
1.99596745052765));
#130984=CARTESIAN_POINT('Ctrl Pts',(-18.0677490202285,21.6842128881249,
2.00014301559882));
#130985=CARTESIAN_POINT('Ctrl Pts',(-17.9868780138841,21.6609909777852,
2.00431858066999));
#130986=CARTESIAN_POINT('Ctrl Pts',(-17.907427475734,21.6338862668579,2.00849414574115));
#130987=CARTESIAN_POINT('Ctrl Pts',(-17.8239641319665,21.6054125792213,
2.01288060593478));
#130988=CARTESIAN_POINT('Ctrl Pts',(-17.7420690633812,21.5726537644299,
2.01726706612841));
#130989=CARTESIAN_POINT('Ctrl Pts',(-17.6621969477251,21.5358307932265,
2.02165352632205));
#130990=CARTESIAN_POINT('Ctrl Pts',(-17.5823248320691,21.4990078220231,
2.02603998651568));
#130991=CARTESIAN_POINT('Ctrl Pts',(-17.5044761476508,21.458121031537,2.03042644670931));
#130992=CARTESIAN_POINT('Ctrl Pts',(-17.4290716121317,21.4134445288214,
2.03481290690294));
#130993=CARTESIAN_POINT('Ctrl Pts',(-17.3571365542413,21.3708236601023,
2.03899753937618));
#130994=CARTESIAN_POINT('Ctrl Pts',(-17.287157912544,21.3245955127068,2.04318217184941));
#130995=CARTESIAN_POINT('Ctrl Pts',(-17.2195204146382,21.2749650155761,
2.04736680432265));
#130996=CARTESIAN_POINT('Ctrl Pts',(-17.1519791909019,21.2254051617284,
2.05154548045468));
#130997=CARTESIAN_POINT('Ctrl Pts',(-17.0867728595891,21.1724528473982,
2.0557241565867));
#130998=CARTESIAN_POINT('Ctrl Pts',(-17.0242598410811,21.1163578637568,
2.05990283271872));
#130999=CARTESIAN_POINT('Ctrl Pts',(-16.9606262846793,21.0592573846791,
2.06415641108813));
#131000=CARTESIAN_POINT('Ctrl Pts',(-16.8997839641052,20.9989007054076,
2.06840998945753));
#131001=CARTESIAN_POINT('Ctrl Pts',(-16.8420782881025,20.9355962530548,
2.07266356782693));
#131002=CARTESIAN_POINT('Ctrl Pts',(-16.7854913830301,20.8735191181162,
2.07683467978818));
#131003=CARTESIAN_POINT('Ctrl Pts',(-16.7319209084704,20.8086078458258,
2.08100579174944));
#131004=CARTESIAN_POINT('Ctrl Pts',(-16.6816563254009,20.7411913087366,
2.08517690371069));
#131005=CARTESIAN_POINT('Ctrl Pts',(-16.6314086093446,20.6737973942486,
2.08934661599456));
#131006=CARTESIAN_POINT('Ctrl Pts',(-16.5844648563589,20.6039002530621,
2.09351632827843));
#131007=CARTESIAN_POINT('Ctrl Pts',(-16.5410736157513,20.5318610348049,
2.0976860405623));
#131008=CARTESIAN_POINT('Ctrl Pts',(-16.4976839193695,20.4598243803099,
2.10185560445267));
#131009=CARTESIAN_POINT('Ctrl Pts',(-16.4578467206233,20.3856461948251,
2.10602516834305));
#131010=CARTESIAN_POINT('Ctrl Pts',(-16.421765949993,20.3097145662038,2.11019473223343));
#131011=CARTESIAN_POINT('Ctrl Pts',(-16.3844165850417,20.2311131932513,
2.11451089734601));
#131012=CARTESIAN_POINT('Ctrl Pts',(-16.3510929497969,20.1506332533461,
2.11882706245858));
#131013=CARTESIAN_POINT('Ctrl Pts',(-16.3219673468085,20.068728675012,2.12314322757116));
#131014=CARTESIAN_POINT('Ctrl Pts',(-16.2937905367765,19.989492212667,2.12731878968715));
#131015=CARTESIAN_POINT('Ctrl Pts',(-16.2695425396132,19.908922969202,2.13149435180313));
#131016=CARTESIAN_POINT('Ctrl Pts',(-16.2493282307314,19.827446428329,2.13566991391912));
#131017=CARTESIAN_POINT('Ctrl Pts',(-16.2280929123458,19.7418545687945,
2.14005638053));
#131018=CARTESIAN_POINT('Ctrl Pts',(-16.2113095991637,19.6552619180468,
2.14444284714087));
#131019=CARTESIAN_POINT('Ctrl Pts',(-16.1990385985768,19.5681703981218,
2.14882931375175));
#131020=CARTESIAN_POINT('Ctrl Pts',(-16.1867675979899,19.4810788781968,
2.15321578036263));
#131021=CARTESIAN_POINT('Ctrl Pts',(-16.1790088854247,19.3934890737652,
2.1576022469735));
#131022=CARTESIAN_POINT('Ctrl Pts',(-16.175759706546,19.3059031134812,2.16198871358438));
#131023=CARTESIAN_POINT('Ctrl Pts',(-16.1726599323334,19.222344555702,2.16617348044157));
#131024=CARTESIAN_POINT('Ctrl Pts',(-16.1736525434566,19.1384784652832,
2.17035824729877));
#131025=CARTESIAN_POINT('Ctrl Pts',(-16.1787734748956,19.0547393030766,
2.17454301415596));
#131026=CARTESIAN_POINT('Ctrl Pts',(-16.1838870736907,18.9711200466848,
2.17872178886007));
#131027=CARTESIAN_POINT('Ctrl Pts',(-16.1931172227512,18.8876278127959,
2.18290056356417));
#131028=CARTESIAN_POINT('Ctrl Pts',(-16.2064478895021,18.8046992139839,
2.18707933826827));
#131029=CARTESIAN_POINT('Ctrl Pts',(-16.219762654119,18.7218695405828,2.19125312811781));
#131030=CARTESIAN_POINT('Ctrl Pts',(-16.2371681394967,18.6396026174132,
2.19542691796735));
#131031=CARTESIAN_POINT('Ctrl Pts',(-16.258596457945,18.558330631957,2.19960070781689));
#131032=CARTESIAN_POINT('Ctrl Pts',(-16.2800107741408,18.4771117533682,
2.20377177031945));
#131033=CARTESIAN_POINT('Ctrl Pts',(-16.3054425870164,18.3968869651317,
2.20794283282201));
#131034=CARTESIAN_POINT('Ctrl Pts',(-16.3347730132237,18.3180779060164,
2.21211389532456));
#131035=CARTESIAN_POINT('Ctrl Pts',(-16.3640930721629,18.2392967031153,
2.21628348350409));
#131036=CARTESIAN_POINT('Ctrl Pts',(-16.3973088466592,18.1619306659659,
2.22045307168362));
#131037=CARTESIAN_POINT('Ctrl Pts',(-16.4342521396892,18.0863846084123,
2.22462265986315));
#131038=CARTESIAN_POINT('Ctrl Pts',(-16.471193456534,18.0108425919983,2.22879202500141));
#131039=CARTESIAN_POINT('Ctrl Pts',(-16.5118616920895,17.9371207741401,
2.23296139013968));
#131040=CARTESIAN_POINT('Ctrl Pts',(-16.5560418071037,17.865601133494,2.23713075527795));
#131041=CARTESIAN_POINT('Ctrl Pts',(-16.6002584544325,17.794022353617,2.24130356804326));
#131042=CARTESIAN_POINT('Ctrl Pts',(-16.6479925391717,17.7246497800717,
2.24547638080857));
#131043=CARTESIAN_POINT('Ctrl Pts',(-16.698984937016,17.6578375186645,2.24964919357389));
#131044=CARTESIAN_POINT('Ctrl Pts',(-16.749999304179,17.590996472185,2.25382380413372));
#131045=CARTESIAN_POINT('Ctrl Pts',(-16.8042744849681,17.5267182878878,
2.25799841469355));
#131046=CARTESIAN_POINT('Ctrl Pts',(-16.8615116627756,17.4653232180731,
2.26217302525338));
#131047=CARTESIAN_POINT('Ctrl Pts',(-16.9188352980411,17.4038354102537,
2.26635394161358));
#131048=CARTESIAN_POINT('Ctrl Pts',(-16.979129537148,17.3452397369253,2.27053485797377));
#131049=CARTESIAN_POINT('Ctrl Pts',(-17.0420596615868,17.2898186209392,
2.27471577433397));
#131050=CARTESIAN_POINT('Ctrl Pts',(-17.0850057301622,17.2519970042032,
2.27756900118382));
#131051=CARTESIAN_POINT('Ctrl Pts',(-17.1291786767271,17.2156530350981,
2.28042222803368));
#131052=CARTESIAN_POINT('Ctrl Pts',(-17.174464231106,17.180864983421,2.28327545488353));
#131053=CARTESIAN_POINT('Origin',(-18.734,19.211,-1.76670989022852));
#131054=CARTESIAN_POINT('',(-17.174464231106,17.180864983421,3.1498113662728));
#131055=CARTESIAN_POINT('',(-17.1746506278754,17.1811162280174,3.08342410660672));
#131056=CARTESIAN_POINT('',(-17.174464231106,17.180864983421,-1.76670989022852));
#131057=CARTESIAN_POINT('',(-21.2939989850552,19.2132795868247,2.63329010980608));
#131058=CARTESIAN_POINT('Ctrl Pts',(-21.2939989850552,19.2132795868247,
2.63329010980608));
#131059=CARTESIAN_POINT('Ctrl Pts',(-21.293907125607,19.3164386732131,2.63841342883254));
#131060=CARTESIAN_POINT('Ctrl Pts',(-21.2875761055109,19.4193213099601,
2.643536747859));
#131061=CARTESIAN_POINT('Ctrl Pts',(-21.2751280763078,19.5212710102476,
2.64866006688546));
#131062=CARTESIAN_POINT('Ctrl Pts',(-21.2624749613816,19.6249003682273,
2.6538677944211));
#131063=CARTESIAN_POINT('Ctrl Pts',(-21.2435016684883,19.7275658815507,
2.65907552195674));
#131064=CARTESIAN_POINT('Ctrl Pts',(-21.2183850428165,19.8286009707164,
2.66428324949238));
#131065=CARTESIAN_POINT('Ctrl Pts',(-21.2103562166331,19.8608980308362,
2.66594796113558));
#131066=CARTESIAN_POINT('Ctrl Pts',(-21.2017000059957,19.8930286552932,
2.66761267277878));
#131067=CARTESIAN_POINT('Ctrl Pts',(-21.1924232051054,19.9249715292638,
2.66927738442198));
#131068=CARTESIAN_POINT('Ctrl Pts',(-21.1691038390111,20.0052672670978,
2.67346201883512));
#131069=CARTESIAN_POINT('Ctrl Pts',(-21.1418030734501,20.0845687630516,
2.67764665324825));
#131070=CARTESIAN_POINT('Ctrl Pts',(-21.1106233366689,20.1624523191421,
2.68183128766138));
#131071=CARTESIAN_POINT('Ctrl Pts',(-21.0794879803815,20.240225017636,2.68600996576567));
#131072=CARTESIAN_POINT('Ctrl Pts',(-21.0444847892983,20.3165833617425,
2.69018864386997));
#131073=CARTESIAN_POINT('Ctrl Pts',(-21.0057661997906,20.3911179320259,
2.69436732197426));
#131074=CARTESIAN_POINT('Ctrl Pts',(-20.9663536076312,20.4669884804549,
2.69862089985464));
#131075=CARTESIAN_POINT('Ctrl Pts',(-20.923091244407,20.5409687666864,2.70287447773502));
#131076=CARTESIAN_POINT('Ctrl Pts',(-20.8761915739271,20.6126473381689,
2.7071280556154));
#131077=CARTESIAN_POINT('Ctrl Pts',(-20.8302011447919,20.6829362811089,
2.71129916961421));
#131078=CARTESIAN_POINT('Ctrl Pts',(-20.7807134458812,20.7510115566354,
2.71547028361302));
#131079=CARTESIAN_POINT('Ctrl Pts',(-20.7279747027012,20.8165107863192,
2.71964139761183));
#131080=CARTESIAN_POINT('Ctrl Pts',(-20.675253656514,20.8819880371064,2.72381111195321));
#131081=CARTESIAN_POINT('Ctrl Pts',(-20.6192840209112,20.9448906007769,
2.72798082629458));
#131082=CARTESIAN_POINT('Ctrl Pts',(-20.560353487436,21.0048876606215,2.73215054063596));
#131083=CARTESIAN_POINT('Ctrl Pts',(-20.5014250509605,21.0648825855149,
2.73632010660112));
#131084=CARTESIAN_POINT('Ctrl Pts',(-20.4395362490684,21.1219718845495,
2.74048967256628));
#131085=CARTESIAN_POINT('Ctrl Pts',(-20.3750119946268,21.1758612249955,
2.74465923853145));
#131086=CARTESIAN_POINT('Ctrl Pts',(-20.3082191477172,21.2316452475716,
2.74897540124578));
#131087=CARTESIAN_POINT('Ctrl Pts',(-20.2386024799585,21.2839997657249,
2.75329156396011));
#131088=CARTESIAN_POINT('Ctrl Pts',(-20.1665585536104,21.3326446428367,
2.75760772667444));
#131089=CARTESIAN_POINT('Ctrl Pts',(-20.0968614498344,21.3797049187001,
2.76178329088732));
#131090=CARTESIAN_POINT('Ctrl Pts',(-20.0248932222208,21.4232933214429,
2.76595885510019));
#131091=CARTESIAN_POINT('Ctrl Pts',(-19.9510397173094,21.463202106049,2.77013441931307));
#131092=CARTESIAN_POINT('Ctrl Pts',(-19.8734560486687,21.5051265878247,
2.77452088127813));
#131093=CARTESIAN_POINT('Ctrl Pts',(-19.7937921742969,21.5429897170771,
2.77890734324319));
#131094=CARTESIAN_POINT('Ctrl Pts',(-19.7125190809761,21.5766078305936,
2.78329380520824));
#131095=CARTESIAN_POINT('Ctrl Pts',(-19.6312459876554,21.61022594411,2.7876802671733));
#131096=CARTESIAN_POINT('Ctrl Pts',(-19.5483642476832,21.6395989197709,
2.79206672913836));
#131097=CARTESIAN_POINT('Ctrl Pts',(-19.4643607861727,21.6646041086575,
2.79645319110342));
#131098=CARTESIAN_POINT('Ctrl Pts',(-19.3842224476358,21.6884587719791,
2.80063782549364));
#131099=CARTESIAN_POINT('Ctrl Pts',(-19.3027650531594,21.7084275441982,
2.80482245988387));
#131100=CARTESIAN_POINT('Ctrl Pts',(-19.2204003081572,21.7243672115758,
2.80900709427409));
#131101=CARTESIAN_POINT('Ctrl Pts',(-19.1381527991746,21.7402841908099,
2.81318577235522));
#131102=CARTESIAN_POINT('Ctrl Pts',(-19.0550009527839,21.7521833699235,
2.81736445043635));
#131103=CARTESIAN_POINT('Ctrl Pts',(-18.97137153685,21.7599713128032,2.82154312851748));
#131104=CARTESIAN_POINT('Ctrl Pts',(-18.8862431236674,21.7678988489685,
2.82579670640362));
#131105=CARTESIAN_POINT('Ctrl Pts',(-18.8006203137736,21.7715661738213,
2.83005028428976));
#131106=CARTESIAN_POINT('Ctrl Pts',(-18.7149640762858,21.7709292243358,
2.8343038621759));
#131107=CARTESIAN_POINT('Ctrl Pts',(-18.630968452176,21.7703046233594,2.83847497615107));
#131108=CARTESIAN_POINT('Ctrl Pts',(-18.5469411662298,21.7655411558157,
2.84264609012625));
#131109=CARTESIAN_POINT('Ctrl Pts',(-18.4633201985508,21.7566497098162,
2.84681720410142));
#131110=CARTESIAN_POINT('Ctrl Pts',(-18.3797272906949,21.7477612474273,
2.85098691841903));
#131111=CARTESIAN_POINT('Ctrl Pts',(-18.2965408873982,21.734747606179,2.85515663273665));
#131112=CARTESIAN_POINT('Ctrl Pts',(-18.2141948751329,21.7176716243182,
2.85932634705426));
#131113=CARTESIAN_POINT('Ctrl Pts',(-18.1318517930915,21.7005962500939,
2.86349591299557));
#131114=CARTESIAN_POINT('Ctrl Pts',(-18.0503494928999,21.6794589169143,
2.86766547893688));
#131115=CARTESIAN_POINT('Ctrl Pts',(-17.9701113309735,21.6543735083554,
2.87183504487819));
#131116=CARTESIAN_POINT('Ctrl Pts',(-17.8870520941402,21.6284061277408,
2.87615120762041));
#131117=CARTESIAN_POINT('Ctrl Pts',(-17.8053480471357,21.5982080349101,
2.88046737036263));
#131118=CARTESIAN_POINT('Ctrl Pts',(-17.7254493921661,21.5639610433319,
2.88478353310486));
#131119=CARTESIAN_POINT('Ctrl Pts',(-17.6481534275864,21.5308296439486,
2.88895909729389));
#131120=CARTESIAN_POINT('Ctrl Pts',(-17.572547442585,21.4939093297973,2.89313466148293));
#131121=CARTESIAN_POINT('Ctrl Pts',(-17.4990149692544,21.4534120883179,
2.89731022567196));
#131122=CARTESIAN_POINT('Ctrl Pts',(-17.4217685453432,21.4108694273566,
2.90169668769078));
#131123=CARTESIAN_POINT('Ctrl Pts',(-17.3468111003271,21.3643793093811,
2.90608314970959));
#131124=CARTESIAN_POINT('Ctrl Pts',(-17.2745520021318,21.3142383463408,
2.91046961172841));
#131125=CARTESIAN_POINT('Ctrl Pts',(-17.2022929039366,21.2640973833005,
2.91485607374722));
#131126=CARTESIAN_POINT('Ctrl Pts',(-17.1327325650194,21.210305990306,2.91924253576604));
#131127=CARTESIAN_POINT('Ctrl Pts',(-17.0662376770537,21.1532072068038,
2.92362899778485));
#131128=CARTESIAN_POINT('Ctrl Pts',(-17.002802317601,21.0987356230989,2.92781363217408));
#131129=CARTESIAN_POINT('Ctrl Pts',(-16.9419203976439,21.0410515629429,
2.9319982665633));
#131130=CARTESIAN_POINT('Ctrl Pts',(-16.8839351856049,20.9804236865537,
2.93618290095253));
#131131=CARTESIAN_POINT('Ctrl Pts',(-16.8260325083393,20.9198821064435,
2.94036157903258));
#131132=CARTESIAN_POINT('Ctrl Pts',(-16.7710186644538,20.8564053626863,
2.94454025711262));
#131133=CARTESIAN_POINT('Ctrl Pts',(-16.7192032202845,20.7903017243225,
2.94871893519267));
#131134=CARTESIAN_POINT('Ctrl Pts',(-16.6664590214563,20.7230132256708,
2.95297251307907));
#131135=CARTESIAN_POINT('Ctrl Pts',(-16.6170293785849,20.6530030460409,
2.95722609096547));
#131136=CARTESIAN_POINT('Ctrl Pts',(-16.5712008555424,20.5806349370301,
2.96147966885187));
#131137=CARTESIAN_POINT('Ctrl Pts',(-16.5262608079,20.5096698251122,2.96565078282577));
#131138=CARTESIAN_POINT('Ctrl Pts',(-16.4847837540961,20.4364378006271,
2.96982189679967));
#131139=CARTESIAN_POINT('Ctrl Pts',(-16.4469976092755,20.3613130290578,
2.97399301077356));
#131140=CARTESIAN_POINT('Ctrl Pts',(-16.4092241439611,20.2862134663322,
2.97816272508983));
#131141=CARTESIAN_POINT('Ctrl Pts',(-16.3751393344488,20.2092228285331,
2.98233243940609));
#131142=CARTESIAN_POINT('Ctrl Pts',(-16.3449251982356,20.1307399586701,
2.98650215372236));
#131143=CARTESIAN_POINT('Ctrl Pts',(-16.3147121371714,20.0522598815654,
2.99067171966225));
#131144=CARTESIAN_POINT('Ctrl Pts',(-16.2883696400355,19.972288107597,2.99484128560214));
#131145=CARTESIAN_POINT('Ctrl Pts',(-16.2660311035614,19.8912422555324,
2.99901085154203));
#131146=CARTESIAN_POINT('Ctrl Pts',(-16.2429071716539,19.8073469311138,
3.00332701428572));
#131147=CARTESIAN_POINT('Ctrl Pts',(-16.2240741377499,19.7223011025938,
3.00764317702941));
#131148=CARTESIAN_POINT('Ctrl Pts',(-16.2096228114109,19.6365817309647,
3.0119593397731));
#131149=CARTESIAN_POINT('Ctrl Pts',(-16.1956422355369,19.5536546590259,
3.01613490396055));
#131150=CARTESIAN_POINT('Ctrl Pts',(-16.1857622912647,19.4700977247645,
3.02031046814801));
#131151=CARTESIAN_POINT('Ctrl Pts',(-16.1800123293527,19.3863481627553,
3.02448603233547));
#131152=CARTESIAN_POINT('Ctrl Pts',(-16.173971950515,19.29836860919,3.02887249435727));
#131153=CARTESIAN_POINT('Ctrl Pts',(-16.1724897391971,19.2101770410221,
3.03325895637908));
#131154=CARTESIAN_POINT('Ctrl Pts',(-16.175537874784,19.1222782223174,3.03764541840088));
#131155=CARTESIAN_POINT('Ctrl Pts',(-16.1785860103709,19.0343794036126,
3.04203188042268));
#131156=CARTESIAN_POINT('Ctrl Pts',(-16.1861643670755,18.9467739058737,
3.04641834244449));
#131157=CARTESIAN_POINT('Ctrl Pts',(-16.1981829862585,18.8599557395154,
3.05080480446629));
#131158=CARTESIAN_POINT('Ctrl Pts',(-16.2096452990133,18.7771561299727,
3.05498823010074));
#131159=CARTESIAN_POINT('Ctrl Pts',(-16.2251885633081,18.6947644704974,
3.05917165573519));
#131160=CARTESIAN_POINT('Ctrl Pts',(-16.2447727253535,18.6132144404924,
3.06335508136964));
#131161=CARTESIAN_POINT('Ctrl Pts',(-16.2643314314933,18.5317704109307,
3.06753306929951));
#131162=CARTESIAN_POINT('Ctrl Pts',(-16.2879205024912,18.4511662821532,
3.07171105722938));
#131163=CARTESIAN_POINT('Ctrl Pts',(-16.3154483597582,18.3718290022387,
3.07588904515925));
#131164=CARTESIAN_POINT('Ctrl Pts',(-16.3429486961517,18.2925710394765,
3.08006285616113));
#131165=CARTESIAN_POINT('Ctrl Pts',(-16.3743798496378,18.2145778427126,
3.08423666716302));
#131166=CARTESIAN_POINT('Ctrl Pts',(-16.4095998941466,18.1382632438904,
3.08841047816491));
#131167=CARTESIAN_POINT('Ctrl Pts',(-16.4447952944457,18.0620020440062,
3.09258136866301));
#131168=CARTESIAN_POINT('Ctrl Pts',(-16.4837741268733,17.9874175251811,
3.09675225916111));
#131169=CARTESIAN_POINT('Ctrl Pts',(-16.5263461035608,17.9149042189959,
3.10092314965921));
#131170=CARTESIAN_POINT('Ctrl Pts',(-16.568912884215,17.8423997632702,3.10509353108802));
#131171=CARTESIAN_POINT('Ctrl Pts',(-16.6150717177094,17.7719664217462,
3.10926391251683));
#131172=CARTESIAN_POINT('Ctrl Pts',(-16.6645865127571,17.7039738493254,
3.11343429394564));
#131173=CARTESIAN_POINT('Ctrl Pts',(-16.7140950873173,17.6359898187343,
3.11760415145416));
#131174=CARTESIAN_POINT('Ctrl Pts',(-16.7669585097326,17.5704463163712,
3.12177400896269));
#131175=CARTESIAN_POINT('Ctrl Pts',(-16.8228985547876,17.5076822768177,
3.12594386647121));
#131176=CARTESIAN_POINT('Ctrl Pts',(-16.8788810408977,17.4448706189247,
3.13011688760165));
#131177=CARTESIAN_POINT('Ctrl Pts',(-16.9379445037493,17.3848429786151,
3.13428990873209));
#131178=CARTESIAN_POINT('Ctrl Pts',(-16.9997721933365,17.3279031053621,
3.13846292986253));
#131179=CARTESIAN_POINT('Ctrl Pts',(-17.0558185269752,17.2762875403136,
3.14224574199928));
#131180=CARTESIAN_POINT('Ctrl Pts',(-17.1141356442521,17.2272089892714,
3.14602855413604));
#131181=CARTESIAN_POINT('Ctrl Pts',(-17.174464231106,17.180864983421,3.1498113662728));
#131182=CARTESIAN_POINT('Ctrl Pts',(-17.174464231106,17.180864983421,2.34989189146289));
#131183=CARTESIAN_POINT('Ctrl Pts',(-17.241152638798,17.1296354069067,2.3540614318011));
#131184=CARTESIAN_POINT('Ctrl Pts',(-17.3103705782716,17.081693266079,2.35823097213931));
#131185=CARTESIAN_POINT('Ctrl Pts',(-17.3817556972678,17.0372853577969,
2.36240051247752));
#131186=CARTESIAN_POINT('Ctrl Pts',(-17.4566944501041,16.9906667724457,
2.36677761735932));
#131187=CARTESIAN_POINT('Ctrl Pts',(-17.5340212921428,16.9479437450928,
2.37115472224112));
#131188=CARTESIAN_POINT('Ctrl Pts',(-17.6132860861713,16.9093483488263,
2.37553182712292));
#131189=CARTESIAN_POINT('Ctrl Pts',(-17.6888992754678,16.8725309819279,
2.37970728564841));
#131190=CARTESIAN_POINT('Ctrl Pts',(-17.7662753462856,16.8394694792919,
2.3838827441739));
#131191=CARTESIAN_POINT('Ctrl Pts',(-17.8450032186746,16.8103157802841,
2.3880582026994));
#131192=CARTESIAN_POINT('Ctrl Pts',(-17.9237867859504,16.7811414569165,
2.39223661509222));
#131193=CARTESIAN_POINT('Ctrl Pts',(-18.0039236197102,16.7558805757865,
2.39641502748503));
#131194=CARTESIAN_POINT('Ctrl Pts',(-18.084988586325,16.7346348845698,2.40059343987785));
#131195=CARTESIAN_POINT('Ctrl Pts',(-18.1661798043565,16.7133561050941,
2.40477835977331));
#131196=CARTESIAN_POINT('Ctrl Pts',(-18.248301589755,16.696105081518,2.40896327966877));
#131197=CARTESIAN_POINT('Ctrl Pts',(-18.3309204231734,16.6829321894488,
2.41314819956423));
#131198=CARTESIAN_POINT('Ctrl Pts',(-18.3426180491651,16.6810670993927,
2.41374072339586));
#131199=CARTESIAN_POINT('Ctrl Pts',(-18.3543256354134,16.6792836761072,
2.41433324722749));
#131200=CARTESIAN_POINT('Ctrl Pts',(-18.3660419494175,16.6775819782335,
2.41492577105912));
#131201=CARTESIAN_POINT('Ctrl Pts',(-18.4487871282914,16.6655639241848,
2.41911040544311));
#131202=CARTESIAN_POINT('Ctrl Pts',(-18.5322757027657,16.6575816378619,
2.42329503982711));
#131203=CARTESIAN_POINT('Ctrl Pts',(-18.6160795877535,16.6537173061283,
2.4274796742111));
#131204=CARTESIAN_POINT('Ctrl Pts',(-18.6997641882883,16.6498584747925,
2.43165835228623));
#131205=CARTESIAN_POINT('Ctrl Pts',(-18.7837627522538,16.6501059764733,
2.43583703036135));
#131206=CARTESIAN_POINT('Ctrl Pts',(-18.8676394869534,16.654490565727,2.44001570843648));
#131207=CARTESIAN_POINT('Ctrl Pts',(-18.9530196520664,16.6589537456037,
2.44426928632415));
#131208=CARTESIAN_POINT('Ctrl Pts',(-19.0382731002415,16.6677038557804,
2.44852286421182));
#131209=CARTESIAN_POINT('Ctrl Pts',(-19.122937334958,16.6807178518047,2.45277644209949));
#131210=CARTESIAN_POINT('Ctrl Pts',(-19.2059601880687,16.6934795460895,
2.45694755606923));
#131211=CARTESIAN_POINT('Ctrl Pts',(-19.2884159943217,16.7103412009493,
2.46111867003897));
#131212=CARTESIAN_POINT('Ctrl Pts',(-19.3698729492393,16.7312287217516,
2.4652897840087));
#131213=CARTESIAN_POINT('Ctrl Pts',(-19.4513025704941,16.7521092335459,
2.46945949832113));
#131214=CARTESIAN_POINT('Ctrl Pts',(-19.5317335608297,16.7770128141669,
2.47362921263355));
#131215=CARTESIAN_POINT('Ctrl Pts',(-19.6107456770759,16.8058145564783,
2.47779892694598));
#131216=CARTESIAN_POINT('Ctrl Pts',(-19.6897549817366,16.8346152739018,
2.48196849288232));
#131217=CARTESIAN_POINT('Ctrl Pts',(-19.7673450807731,16.8673137188663,
2.48613805881867));
#131218=CARTESIAN_POINT('Ctrl Pts',(-19.8431135303129,16.903735997577,2.49030762475501));
#131219=CARTESIAN_POINT('Ctrl Pts',(-19.9215459053923,16.9414388388313,
2.49462378750381));
#131220=CARTESIAN_POINT('Ctrl Pts',(-19.99802567382,16.9831320175021,2.4989399502526));
#131221=CARTESIAN_POINT('Ctrl Pts',(-20.07213364893,17.028570542354,2.5032561130014));
#131222=CARTESIAN_POINT('Ctrl Pts',(-20.1438275642621,17.0725289118643,
2.50743167718612));
#131223=CARTESIAN_POINT('Ctrl Pts',(-20.2133014733533,17.1199920607243,
2.51160724137085));
#131224=CARTESIAN_POINT('Ctrl Pts',(-20.2802065216071,17.1706947795637,
2.51578280555557));
#131225=CARTESIAN_POINT('Ctrl Pts',(-20.3504907852066,17.2239583725082,
2.5201692675864));
#131226=CARTESIAN_POINT('Ctrl Pts',(-20.417939415174,17.2807970211657,2.52455572961723));
#131227=CARTESIAN_POINT('Ctrl Pts',(-20.4821902270871,17.3408580455171,
2.52894219164806));
#131228=CARTESIAN_POINT('Ctrl Pts',(-20.5464410390001,17.4009190698685,
2.53332865367889));
#131229=CARTESIAN_POINT('Ctrl Pts',(-20.6074936847495,17.4642019995335,
2.53771511570972));
#131230=CARTESIAN_POINT('Ctrl Pts',(-20.665034920053,17.5303143846823,2.54210157774055));
#131231=CARTESIAN_POINT('Ctrl Pts',(-20.7194682477108,17.5928559186633,
2.54625111891261));
#131232=CARTESIAN_POINT('Ctrl Pts',(-20.7709705307844,17.6581717364551,
2.55040066008466));
#131233=CARTESIAN_POINT('Ctrl Pts',(-20.8192426277969,17.7259534743927,
2.55455020125671));
#131234=CARTESIAN_POINT('Ctrl Pts',(-20.8674506257227,17.7936452069694,
2.55869423237604));
#131235=CARTESIAN_POINT('Ctrl Pts',(-20.912436679677,17.8637959851797,2.56283826349536));
#131236=CARTESIAN_POINT('Ctrl Pts',(-20.953940279832,17.936062686255,2.56698229461468));
#131237=CARTESIAN_POINT('Ctrl Pts',(-20.9954017278126,18.0082559913218,
2.57112211694435));
#131238=CARTESIAN_POINT('Ctrl Pts',(-21.0333875106824,18.0825605501461,
2.57526193927403));
#131239=CARTESIAN_POINT('Ctrl Pts',(-21.0676798966809,18.1586036203847,
2.5794017616037));
#131240=CARTESIAN_POINT('Ctrl Pts',(-21.1019481578681,18.2345931940623,
2.58353867155416));
#131241=CARTESIAN_POINT('Ctrl Pts',(-21.1325279904635,18.3123184247114,
2.58767558150461));
#131242=CARTESIAN_POINT('Ctrl Pts',(-21.1592478841653,18.3913825890383,
2.59181249145506));
#131243=CARTESIAN_POINT('Ctrl Pts',(-21.185962767493,18.4704319276684,2.59594862567389));
#131244=CARTESIAN_POINT('Ctrl Pts',(-21.2088189905586,18.5508192612332,
2.60008475989273));
#131245=CARTESIAN_POINT('Ctrl Pts',(-21.2276938748212,18.6321296702378,
2.60422089411156));
#131246=CARTESIAN_POINT('Ctrl Pts',(-21.2465668271893,18.7134317569063,
2.60835660498608));
#131247=CARTESIAN_POINT('Ctrl Pts',(-21.261459151574,18.7956562735645,2.61249231586059));
#131248=CARTESIAN_POINT('Ctrl Pts',(-21.272298987946,18.8783767179039,2.61662802673511));
#131249=CARTESIAN_POINT('Ctrl Pts',(-21.2831447249188,18.9611421906275,
2.62076598885936));
#131250=CARTESIAN_POINT('Ctrl Pts',(-21.2899335186437,19.0444036643965,
2.62490395098361));
#131251=CARTESIAN_POINT('Ctrl Pts',(-21.2926453380231,19.1277291514849,
2.62904191310786));
#131252=CARTESIAN_POINT('Ctrl Pts',(-21.2935733586038,19.1562442389939,
2.63045797866241));
#131253=CARTESIAN_POINT('Ctrl Pts',(-21.2940243746441,19.1847668138181,
2.63187404421695));
#131254=CARTESIAN_POINT('Ctrl Pts',(-21.2939989850559,19.2132795861284,
2.6332901097715));
#131255=CARTESIAN_POINT('',(-21.2939990581246,19.2088040034447,2.5667098902285));
#131256=CARTESIAN_POINT('Ctrl Pts',(-17.174464231106,17.180864983421,2.28327545488353));
#131257=CARTESIAN_POINT('Ctrl Pts',(-17.2056207198402,17.156930782879,2.28523847667762));
#131258=CARTESIAN_POINT('Ctrl Pts',(-17.2373037248014,17.133732871778,2.28720149847172));
#131259=CARTESIAN_POINT('Ctrl Pts',(-17.2694745299327,17.1112940330789,
2.28916452026581));
#131260=CARTESIAN_POINT('Ctrl Pts',(-17.3380540324817,17.0634604650508,
2.29334915467525));
#131261=CARTESIAN_POINT('Ctrl Pts',(-17.4091070955312,17.0189012759421,
2.29753378908469));
#131262=CARTESIAN_POINT('Ctrl Pts',(-17.4822878905536,16.977881822414,2.30171842349413));
#131263=CARTESIAN_POINT('Ctrl Pts',(-17.5553645218218,16.9369207549729,
2.30589710159728));
#131264=CARTESIAN_POINT('Ctrl Pts',(-17.6305624715266,16.8994896383272,
2.31007577970043));
#131265=CARTESIAN_POINT('Ctrl Pts',(-17.7075059667129,16.865811308311,2.31425445780358));
#131266=CARTESIAN_POINT('Ctrl Pts',(-17.78582861831,16.8315293186269,2.31850803568457));
#131267=CARTESIAN_POINT('Ctrl Pts',(-17.8659596132366,16.8011362520549,
2.32276161356556));
#131268=CARTESIAN_POINT('Ctrl Pts',(-17.9474751923745,16.7748188230368,
2.32701519144654));
#131269=CARTESIAN_POINT('Ctrl Pts',(-18.0274104335289,16.7490116085464,
2.33118630545054));
#131270=CARTESIAN_POINT('Ctrl Pts',(-18.1086765943189,16.7271235613587,
2.33535741945454));
#131271=CARTESIAN_POINT('Ctrl Pts',(-18.1908544682415,16.7092820040359,
2.33952853345854));
#131272=CARTESIAN_POINT('Ctrl Pts',(-18.2730047666344,16.6914464336092,
2.34369824780747));
#131273=CARTESIAN_POINT('Ctrl Pts',(-18.3560657213856,16.6776547538851,
2.34786796215639));
#131274=CARTESIAN_POINT('Ctrl Pts',(-18.4396056840352,16.667983683354,2.35203767650531));
#131275=CARTESIAN_POINT('Ctrl Pts',(-18.5231426740241,16.6583129569554,
2.35620724248039));
#131276=CARTESIAN_POINT('Ctrl Pts',(-18.6071581809428,16.6527626002749,
2.36037680845546));
#131277=CARTESIAN_POINT('Ctrl Pts',(-18.6912145090001,16.6513575636898,
2.36454637443054));
#131278=CARTESIAN_POINT('Ctrl Pts',(-18.7782261526212,16.6499031277724,
2.36886253714026));
#131279=CARTESIAN_POINT('Ctrl Pts',(-18.8652810139809,16.6528909431617,
2.37317869984999));
#131280=CARTESIAN_POINT('Ctrl Pts',(-18.9518945613659,16.6602899106078,
2.37749486255972));
#131281=CARTESIAN_POINT('Ctrl Pts',(-19.035686682863,16.6674478575793,2.38167042678834));
#131282=CARTESIAN_POINT('Ctrl Pts',(-19.1190653399935,16.6787338735463,
2.38584599101697));
#131283=CARTESIAN_POINT('Ctrl Pts',(-19.2015998086533,16.694067259749,2.39002155524559));
#131284=CARTESIAN_POINT('Ctrl Pts',(-19.2883028951201,16.710175098466,2.39440801719587));
#131285=CARTESIAN_POINT('Ctrl Pts',(-19.3740737042672,16.7307497815342,
2.39879447914615));
#131286=CARTESIAN_POINT('Ctrl Pts',(-19.4584303876713,16.7556383945703,
2.40318094109642));
#131287=CARTESIAN_POINT('Ctrl Pts',(-19.5427870710755,16.7805270076064,
2.4075674030467));
#131288=CARTESIAN_POINT('Ctrl Pts',(-19.6257291067111,16.8097292861734,
2.41195386499698));
#131289=CARTESIAN_POINT('Ctrl Pts',(-19.7068005673283,16.8430348279154,
2.41634032694725));
#131290=CARTESIAN_POINT('Ctrl Pts',(-19.7841418063579,16.8748079308701,
2.42052496109111));
#131291=CARTESIAN_POINT('Ctrl Pts',(-19.8600687027665,16.9104332654798,
2.42470959523496));
#131292=CARTESIAN_POINT('Ctrl Pts',(-19.9341709431984,16.949763677299,2.42889422937882));
#131293=CARTESIAN_POINT('Ctrl Pts',(-20.0081677081793,16.9890381071006,
2.43307290720919));
#131294=CARTESIAN_POINT('Ctrl Pts',(-20.0803445731189,17.0320069250119,
2.43725158503956));
#131295=CARTESIAN_POINT('Ctrl Pts',(-20.1503107695878,17.0784747823415,
2.44143026286993));
#131296=CARTESIAN_POINT('Ctrl Pts',(-20.2215310652186,17.125775546187,2.44568384081822));
#131297=CARTESIAN_POINT('Ctrl Pts',(-20.290460214072,17.1767018411764,2.4499374187665));
#131298=CARTESIAN_POINT('Ctrl Pts',(-20.3567118459902,17.2309984179595,
2.45419099671478));
#131299=CARTESIAN_POINT('Ctrl Pts',(-20.421679055696,17.2842423455132,2.45836211043023));
#131300=CARTESIAN_POINT('Ctrl Pts',(-20.4840712680033,17.3407267365035,
2.46253322414569));
#131301=CARTESIAN_POINT('Ctrl Pts',(-20.5435545162614,17.4001680219639,
2.46670433786114));
#131302=CARTESIAN_POINT('Ctrl Pts',(-20.6030178043004,17.4595893612863,
2.47087405191626));
#131303=CARTESIAN_POINT('Ctrl Pts',(-20.6595737417694,17.5219652996142,
2.47504376597137));
#131304=CARTESIAN_POINT('Ctrl Pts',(-20.7129241774329,17.5869744152349,
2.47921348002649));
#131305=CARTESIAN_POINT('Ctrl Pts',(-20.7662727146278,17.6519812175144,
2.48338304570285));
#131306=CARTESIAN_POINT('Ctrl Pts',(-20.8164156856331,17.7196206546306,
2.48755261137921));
#131307=CARTESIAN_POINT('Ctrl Pts',(-20.863095194694,17.7895381989196,2.49172217705558));
#131308=CARTESIAN_POINT('Ctrl Pts',(-20.9114159042677,17.8619139676384,
2.49603834010334));
#131309=CARTESIAN_POINT('Ctrl Pts',(-20.9560247758967,17.9367305826506,
2.5003545031511));
#131310=CARTESIAN_POINT('Ctrl Pts',(-20.9966856911894,18.0135637959011,
2.50467066619885));
#131311=CARTESIAN_POINT('Ctrl Pts',(-21.0360220760754,18.0878941651683,
2.50884623011952));
#131312=CARTESIAN_POINT('Ctrl Pts',(-21.0716636083121,18.1641113216876,
2.51302179404019));
#131313=CARTESIAN_POINT('Ctrl Pts',(-21.1034449999947,18.2418094139954,
2.51719735796086));
#131314=CARTESIAN_POINT('Ctrl Pts',(-21.1368316009424,18.3234318686752,
2.52158382057216));
#131315=CARTESIAN_POINT('Ctrl Pts',(-21.1659576673028,18.4066882444733,
2.52597028318347));
#131316=CARTESIAN_POINT('Ctrl Pts',(-21.1906909603742,18.491090613191,2.53035674579477));
#131317=CARTESIAN_POINT('Ctrl Pts',(-21.2154242534456,18.5754929819087,
2.53474320840607));
#131318=CARTESIAN_POINT('Ctrl Pts',(-21.2357647130149,18.6610407614697,
2.53912967101737));
#131319=CARTESIAN_POINT('Ctrl Pts',(-21.251642469363,18.7472367021208,2.54351613362868));
#131320=CARTESIAN_POINT('Ctrl Pts',(-21.2744558894944,18.8710844400873,
2.54981867488504));
#131321=CARTESIAN_POINT('Ctrl Pts',(-21.288135817693,18.9966631545043,2.5561212161414));
#131322=CARTESIAN_POINT('Ctrl Pts',(-21.2924829866055,19.122881856295,2.56242375739777));
#131323=CARTESIAN_POINT('Ctrl Pts',(-21.293468437957,19.1514941308042,2.56385246834134));
#131324=CARTESIAN_POINT('Ctrl Pts',(-21.2939744691008,19.18013916897,2.56528117928492));
#131325=CARTESIAN_POINT('Ctrl Pts',(-21.2939990581246,19.2088040034447,
2.5667098902285));
#131326=CARTESIAN_POINT('Ctrl Pts',(-21.2953148853665,19.2088155456687,
2.56671052144854));
#131327=CARTESIAN_POINT('Ctrl Pts',(-21.2889869060013,19.9045867976347,
2.6013709944024));
#131328=CARTESIAN_POINT('Ctrl Pts',(-20.6359184624636,21.4617758669056,
2.67842340291674));
#131329=CARTESIAN_POINT('Ctrl Pts',(-18.0006016372723,22.1479062807659,
2.79786774699155));
#131330=CARTESIAN_POINT('Ctrl Pts',(-15.8675519701989,20.1840197011935,
2.92504355367299));
#131331=CARTESIAN_POINT('Ctrl Pts',(-16.2393387098563,18.0460023819557,
3.02022900687805));
#131332=CARTESIAN_POINT('Ctrl Pts',(-17.0075187134083,17.3068569533771,
3.07302252452263));
#131333=CARTESIAN_POINT('Ctrl Pts',(-17.1746506278756,17.1811162280172,
3.08342410660674));
#131334=CARTESIAN_POINT('Origin',(-18.734,19.211,-1.76670989022852));
#131335=CARTESIAN_POINT('',(-17.174464231106,17.180864983421,3.94993168719587));
#131336=CARTESIAN_POINT('',(-17.174464231106,17.180864983421,3.88329345071054));
#131337=CARTESIAN_POINT('',(-17.174464231106,17.180864983421,-1.76670989022852));
#131338=CARTESIAN_POINT('',(-21.2939999971965,19.2108801919503,3.43329010980363));
#131339=CARTESIAN_POINT('Ctrl Pts',(-21.2939999971965,19.2108801919503,
3.43329010980363));
#131340=CARTESIAN_POINT('Ctrl Pts',(-21.294003905102,19.2943824116244,3.43746913841141));
#131341=CARTESIAN_POINT('Ctrl Pts',(-21.2899179933662,19.3780422026729,
3.44164816701919));
#131342=CARTESIAN_POINT('Ctrl Pts',(-21.2817219740999,19.4614251239161,
3.44582719562696));
#131343=CARTESIAN_POINT('Ctrl Pts',(-21.2735376207105,19.5446893613373,
3.45000027597723));
#131344=CARTESIAN_POINT('Ctrl Pts',(-21.2612548239782,19.6276770564323,
3.45417335632749));
#131345=CARTESIAN_POINT('Ctrl Pts',(-21.2449053023278,19.7099534675119,
3.45834643667776));
#131346=CARTESIAN_POINT('Ctrl Pts',(-21.228391285294,19.7930576758855,3.46256150311585));
#131347=CARTESIAN_POINT('Ctrl Pts',(-21.2077282378307,19.875435728573,3.46677656955395));
#131348=CARTESIAN_POINT('Ctrl Pts',(-21.1830026840864,19.9566445891559,
3.47099163599204));
#131349=CARTESIAN_POINT('Ctrl Pts',(-21.1585674190593,20.0369000225192,
3.47515721572332));
#131350=CARTESIAN_POINT('Ctrl Pts',(-21.1301646741428,20.1160131199896,
3.47932279545459));
#131351=CARTESIAN_POINT('Ctrl Pts',(-21.0979289771719,20.1935679573886,
3.48348837518587));
#131352=CARTESIAN_POINT('Ctrl Pts',(-21.0657039544922,20.2710971138504,
3.48765257555778));
#131353=CARTESIAN_POINT('Ctrl Pts',(-21.0296486772609,20.347068609211,3.49181677592968));
#131354=CARTESIAN_POINT('Ctrl Pts',(-20.9899463178963,20.4210852080619,
3.49598097630159));
#131355=CARTESIAN_POINT('Ctrl Pts',(-20.9502451090693,20.4950996619801,
3.50014505599882));
#131356=CARTESIAN_POINT('Ctrl Pts',(-20.9068972472216,20.5671589258642,
3.50430913569605));
#131357=CARTESIAN_POINT('Ctrl Pts',(-20.8601318431733,20.6368903833901,
3.50847321539329));
#131358=CARTESIAN_POINT('Ctrl Pts',(-20.8123689128483,20.7081092430375,
3.51272611670985));
#131359=CARTESIAN_POINT('Ctrl Pts',(-20.7610412266545,20.7768994173757,
3.51697901802641));
#131360=CARTESIAN_POINT('Ctrl Pts',(-20.7064383509255,20.8428967344162,
3.52123191934297));
#131361=CARTESIAN_POINT('Ctrl Pts',(-20.6528987388227,20.9076089076671,
3.52540200532764));
#131362=CARTESIAN_POINT('Ctrl Pts',(-20.5962107113947,20.969635714652,3.5295720913123));
#131363=CARTESIAN_POINT('Ctrl Pts',(-20.5366855500212,21.0286701592271,
3.53374217729697));
#131364=CARTESIAN_POINT('Ctrl Pts',(-20.4753871892413,21.0894631852098,
3.53803648627948));
#131365=CARTESIAN_POINT('Ctrl Pts',(-20.411080380652,21.1470823903906,3.54233079526199));
#131366=CARTESIAN_POINT('Ctrl Pts',(-20.3441412203941,21.2012374859267,
3.54662510424449));
#131367=CARTESIAN_POINT('Ctrl Pts',(-20.2772020601362,21.2553925814628,
3.550919413227));
#131368=CARTESIAN_POINT('Ctrl Pts',(-20.2076310154016,21.306083314333,3.55521372220951));
#131369=CARTESIAN_POINT('Ctrl Pts',(-20.1358342086543,21.353069291934,3.55950803119202));
#131370=CARTESIAN_POINT('Ctrl Pts',(-20.0658710578792,21.3988552702266,
3.56369266558496));
#131371=CARTESIAN_POINT('Ctrl Pts',(-19.9935321931099,21.4412951999105,
3.56787729997789));
#131372=CARTESIAN_POINT('Ctrl Pts',(-19.9191711337672,21.4801340603157,
3.57206193437083));
#131373=CARTESIAN_POINT('Ctrl Pts',(-19.8449159181885,21.5189176384104,
3.57624061245465));
#131374=CARTESIAN_POINT('Ctrl Pts',(-19.7686446296092,21.5541101172785,
3.58041929053848));
#131375=CARTESIAN_POINT('Ctrl Pts',(-19.690739462204,21.5854998634368,3.58459796862231));
#131376=CARTESIAN_POINT('Ctrl Pts',(-19.6114379006597,21.6174522482367,
3.58885154650778));
#131377=CARTESIAN_POINT('Ctrl Pts',(-19.5304437130248,21.645463967428,3.59310512439324));
#131378=CARTESIAN_POINT('Ctrl Pts',(-19.4481859912097,21.6693609112496,
3.5973587022787));
#131379=CARTESIAN_POINT('Ctrl Pts',(-19.3675229958474,21.6927945661833,
3.60152981625654));
#131380=CARTESIAN_POINT('Ctrl Pts',(-19.2856454833722,21.7122714336375,
3.60570093023438));
#131381=CARTESIAN_POINT('Ctrl Pts',(-19.2029762398825,21.7276766352525,
3.60987204421222));
#131382=CARTESIAN_POINT('Ctrl Pts',(-19.1203347368559,21.7430766675032,
3.61404175853247));
#131383=CARTESIAN_POINT('Ctrl Pts',(-19.0369024823169,21.754407663177,3.61821147285273));
#131384=CARTESIAN_POINT('Ctrl Pts',(-18.9531132034119,21.7616056935737,
3.62238118717299));
#131385=CARTESIAN_POINT('Ctrl Pts',(-18.8693269060889,21.7688034678336,
3.62655075311692));
#131386=CARTESIAN_POINT('Ctrl Pts',(-18.7851840680774,21.7718685307012,
3.63072031906085));
#131387=CARTESIAN_POINT('Ctrl Pts',(-18.701122931338,21.7707888776921,3.63488988500478));
#131388=CARTESIAN_POINT('Ctrl Pts',(-18.6141063087263,21.769671265415,3.63920604774384));
#131389=CARTESIAN_POINT('Ctrl Pts',(-18.5271777668964,21.764112064791,3.64352221048289));
#131390=CARTESIAN_POINT('Ctrl Pts',(-18.4408207068909,21.7541566806023,
3.64783837322195));
#131391=CARTESIAN_POINT('Ctrl Pts',(-18.3572767190368,21.744525592007,3.65201393741352));
#131392=CARTESIAN_POINT('Ctrl Pts',(-18.2742680097319,21.7307804563761,
3.65618950160509));
#131393=CARTESIAN_POINT('Ctrl Pts',(-18.1922227301013,21.7130146661882,
3.66036506579666));
#131394=CARTESIAN_POINT('Ctrl Pts',(-18.1060335384334,21.6943515681706,
3.66475152780946));
#131395=CARTESIAN_POINT('Ctrl Pts',(-18.0209082233735,21.6712511277376,
3.66913798982226));
#131396=CARTESIAN_POINT('Ctrl Pts',(-17.937323903919,21.6438804323133,3.67352445183506));
#131397=CARTESIAN_POINT('Ctrl Pts',(-17.8537395844645,21.616509736889,3.67791091384786));
#131398=CARTESIAN_POINT('Ctrl Pts',(-17.7716967745983,21.584869066222,3.68229737586066));
#131399=CARTESIAN_POINT('Ctrl Pts',(-17.6916449845522,21.5491822045706,
3.68668383787346));
#131400=CARTESIAN_POINT('Ctrl Pts',(-17.6152764960367,21.5151373483269,
3.69086847226646));
#131401=CARTESIAN_POINT('Ctrl Pts',(-17.5404355759513,21.4772837399297,
3.69505310665946));
#131402=CARTESIAN_POINT('Ctrl Pts',(-17.4675280096793,21.4357805954145,
3.69923774105247));
#131403=CARTESIAN_POINT('Ctrl Pts',(-17.3947242183036,21.3943365254885,
3.70341641913637));
#131404=CARTESIAN_POINT('Ctrl Pts',(-17.3238487109965,21.3492534633187,
3.70759509722027));
#131405=CARTESIAN_POINT('Ctrl Pts',(-17.2552863124834,21.3007382205317,
3.71177377530417));
#131406=CARTESIAN_POINT('Ctrl Pts',(-17.185494982251,21.2513533768844,3.71602735318961));
#131407=CARTESIAN_POINT('Ctrl Pts',(-17.1181009417718,21.1984122950055,
3.72028093107506));
#131408=CARTESIAN_POINT('Ctrl Pts',(-17.0534828491143,21.142181530975,3.72453450896051));
#131409=CARTESIAN_POINT('Ctrl Pts',(-16.9901175042757,21.0870409100313,
3.72870562293841));
#131410=CARTESIAN_POINT('Ctrl Pts',(-16.9294217964541,21.0287373383807,
3.73287673691632));
#131411=CARTESIAN_POINT('Ctrl Pts',(-16.8717211662666,20.9675641307475,
3.73704785089422));
#131412=CARTESIAN_POINT('Ctrl Pts',(-16.8140398980829,20.9064114503749,
3.74121756521455));
#131413=CARTESIAN_POINT('Ctrl Pts',(-16.7593520269257,20.8423913807957,
3.74538727953487));
#131414=CARTESIAN_POINT('Ctrl Pts',(-16.7079460749928,20.7758340145085,
3.74955699385519));
#131415=CARTESIAN_POINT('Ctrl Pts',(-16.6565419523043,20.709279016618,3.75372655979918));
#131416=CARTESIAN_POINT('Ctrl Pts',(-16.6084197971687,20.6401872661385,
3.75789612574317));
#131417=CARTESIAN_POINT('Ctrl Pts',(-16.563826915519,20.5689207574061,3.76206569168716));
#131418=CARTESIAN_POINT('Ctrl Pts',(-16.5176662031606,20.4951486061414,
3.76638185442614));
#131419=CARTESIAN_POINT('Ctrl Pts',(-16.4752878401618,20.4190463693443,
3.77069801716511));
#131420=CARTESIAN_POINT('Ctrl Pts',(-16.4369153041021,20.3410450875393,
3.77501417990409));
#131421=CARTESIAN_POINT('Ctrl Pts',(-16.3997927493695,20.2655846892869,
3.77918974409572));
#131422=CARTESIAN_POINT('Ctrl Pts',(-16.3664191932582,20.1883475199533,
3.78336530828734));
#131423=CARTESIAN_POINT('Ctrl Pts',(-16.3369478575569,20.1097441384558,
3.78754087247896));
#131424=CARTESIAN_POINT('Ctrl Pts',(-16.3059879947494,20.0271706870175,
3.79192733449162));
#131425=CARTESIAN_POINT('Ctrl Pts',(-16.2793350909183,19.9430899381559,
3.79631379650427));
#131426=CARTESIAN_POINT('Ctrl Pts',(-16.257106907446,19.8579935146957,3.80070025851693));
#131427=CARTESIAN_POINT('Ctrl Pts',(-16.2348787239737,19.7728970912354,
3.80508672052958));
#131428=CARTESIAN_POINT('Ctrl Pts',(-16.2170753038451,19.6867855767773,
3.80947318254224));
#131429=CARTESIAN_POINT('Ctrl Pts',(-16.2037517912764,19.6001580684646,
3.81385964455489));
#131430=CARTESIAN_POINT('Ctrl Pts',(-16.1910413132713,19.5175164202231,
3.81804427894799));
#131431=CARTESIAN_POINT('Ctrl Pts',(-16.182360236898,19.4340976099864,3.8222289133411));
#131432=CARTESIAN_POINT('Ctrl Pts',(-16.1777943305988,19.3503290196653,
3.8264135477342));
#131433=CARTESIAN_POINT('Ctrl Pts',(-16.1732349233019,19.2666796635639,
3.83059222581821));
#131434=CARTESIAN_POINT('Ctrl Pts',(-16.1727790761929,19.182681971724,3.83477090390221));
#131435=CARTESIAN_POINT('Ctrl Pts',(-16.1764611917473,19.0987714640509,
3.83894958198622));
#131436=CARTESIAN_POINT('Ctrl Pts',(-16.1802093065767,19.0133569208348,
3.84320315987164));
#131437=CARTESIAN_POINT('Ctrl Pts',(-16.1882452624471,18.9280331946165,
3.84745673775706));
#131438=CARTESIAN_POINT('Ctrl Pts',(-16.2005498883094,18.8432629586582,
3.85171031564248));
#131439=CARTESIAN_POINT('Ctrl Pts',(-16.2126159649891,18.7601361591379,
3.85588142962049));
#131440=CARTESIAN_POINT('Ctrl Pts',(-16.2287866065493,18.6775420566423,
3.86005254359851));
#131441=CARTESIAN_POINT('Ctrl Pts',(-16.2489913365584,18.5959130609253,
3.86422365757652));
#131442=CARTESIAN_POINT('Ctrl Pts',(-16.2691892866753,18.5143114566062,
3.86839337189696));
#131443=CARTESIAN_POINT('Ctrl Pts',(-16.2934185263772,18.433674762078,3.87256308621739));
#131444=CARTESIAN_POINT('Ctrl Pts',(-16.3215576717044,18.3544242516581,
3.87673280053782));
#131445=CARTESIAN_POINT('Ctrl Pts',(-16.34969581572,18.2751765613115,3.88090236648193));
#131446=CARTESIAN_POINT('Ctrl Pts',(-16.3817434340024,18.1973153902312,
3.88507193242603));
#131447=CARTESIAN_POINT('Ctrl Pts',(-16.4175300086125,18.1212446242384,
3.88924149837014));
#131448=CARTESIAN_POINT('Ctrl Pts',(-16.4545747950374,18.0424993039591,
3.89355766110898));
#131449=CARTESIAN_POINT('Ctrl Pts',(-16.4956261286211,17.9656731098163,
3.89787382384783));
#131450=CARTESIAN_POINT('Ctrl Pts',(-16.5404425366714,17.8911872651488,
3.90218998658668));
#131451=CARTESIAN_POINT('Ctrl Pts',(-16.5837990549447,17.8191277890345,
3.90636555077843));
#131452=CARTESIAN_POINT('Ctrl Pts',(-16.6306788183656,17.749258894982,3.91054111497017));
#131453=CARTESIAN_POINT('Ctrl Pts',(-16.6808195479051,17.6819316460226,
3.91471667916191));
#131454=CARTESIAN_POINT('Ctrl Pts',(-16.7334927664929,17.6112038577767,
3.91910314117431));
#131455=CARTESIAN_POINT('Ctrl Pts',(-16.7897646588842,17.5432816689316,
3.92348960318672));
#131456=CARTESIAN_POINT('Ctrl Pts',(-16.8492855900873,17.4785302042842,
3.92787606519912));
#131457=CARTESIAN_POINT('Ctrl Pts',(-16.9088065212905,17.4137787396368,
3.93226252721152));
#131458=CARTESIAN_POINT('Ctrl Pts',(-16.9715760238565,17.3521983512227,
3.93664898922393));
#131459=CARTESIAN_POINT('Ctrl Pts',(-17.0372042845901,17.2941055584184,
3.94103545123633));
#131460=CARTESIAN_POINT('Ctrl Pts',(-17.0815714375447,17.2548326629447,
3.94400086322284));
#131461=CARTESIAN_POINT('Ctrl Pts',(-17.1273612095889,17.2170492008642,
3.94696627520936));
#131462=CARTESIAN_POINT('Ctrl Pts',(-17.174464231106,17.180864983421,3.94993168719587));
#131463=CARTESIAN_POINT('Ctrl Pts',(-17.174464231106,17.180864983421,3.1498113662728));
#131464=CARTESIAN_POINT('Ctrl Pts',(-17.2410961502261,17.1296788010395,
3.15398941925709));
#131465=CARTESIAN_POINT('Ctrl Pts',(-17.3101818955148,17.0818293110454,
3.15816747224137));
#131466=CARTESIAN_POINT('Ctrl Pts',(-17.3813458444593,17.0375403763818,
3.16234552522566));
#131467=CARTESIAN_POINT('Ctrl Pts',(-17.4526226812698,16.9931811858739,
3.16653020588439));
#131468=CARTESIAN_POINT('Ctrl Pts',(-17.5259838976535,16.95239404136,3.17071488654311));
#131469=CARTESIAN_POINT('Ctrl Pts',(-17.6010304532445,16.9153562980888,
3.17489956720183));
#131470=CARTESIAN_POINT('Ctrl Pts',(-17.6194485640172,16.906266403783,3.17592658185046));
#131471=CARTESIAN_POINT('Ctrl Pts',(-17.6379681017651,16.8974021130445,
3.17695359649909));
#131472=CARTESIAN_POINT('Ctrl Pts',(-17.6565830150582,16.8887655931067,
3.17798061114772));
#131473=CARTESIAN_POINT('Ctrl Pts',(-17.7324306249075,16.8535755610943,
3.18216524554016));
#131474=CARTESIAN_POINT('Ctrl Pts',(-17.8101452346758,16.8220398921685,
3.18634987993261));
#131475=CARTESIAN_POINT('Ctrl Pts',(-17.8893401694872,16.7943598176977,
3.19053451432505));
#131476=CARTESIAN_POINT('Ctrl Pts',(-17.9684223801113,16.7667191423868,
3.19471319240839));
#131477=CARTESIAN_POINT('Ctrl Pts',(-18.0489802999388,16.7429233111999,
3.19889187049173));
#131478=CARTESIAN_POINT('Ctrl Pts',(-18.1306051532976,16.7231264785016,
3.20307054857507));
#131479=CARTESIAN_POINT('Ctrl Pts',(-18.2136930735051,16.7029748018013,
3.20732412646065));
#131480=CARTESIAN_POINT('Ctrl Pts',(-18.297886115673,16.6869671007255,3.21157770434624));
#131481=CARTESIAN_POINT('Ctrl Pts',(-18.3827345240938,16.6752136199127,
3.21583128223183));
#131482=CARTESIAN_POINT('Ctrl Pts',(-18.4659379805342,16.6636880032625,
3.22000239620917));
#131483=CARTESIAN_POINT('Ctrl Pts',(-18.5497711422169,16.6562531921902,
3.22417351018651));
#131484=CARTESIAN_POINT('Ctrl Pts',(-18.6337990563683,16.6529617338876,
3.22834462416386));
#131485=CARTESIAN_POINT('Ctrl Pts',(-18.7177987741417,16.6496713800656,
3.23251433848362));
#131486=CARTESIAN_POINT('Ctrl Pts',(-18.8019926552977,16.6505216357632,
3.23668405280339));
#131487=CARTESIAN_POINT('Ctrl Pts',(-18.885942287003,16.6555130519957,3.24085376712315));
#131488=CARTESIAN_POINT('Ctrl Pts',(-18.9698889314202,16.6605042906123,
3.24502333306659));
#131489=CARTESIAN_POINT('Ctrl Pts',(-19.0535908844962,16.669636368619,3.24919289901003));
#131490=CARTESIAN_POINT('Ctrl Pts',(-19.1366127729526,16.6828578056099,
3.25336246495347));
#131491=CARTESIAN_POINT('Ctrl Pts',(-19.2225536086153,16.6965440920193,
3.25767862769311));
#131492=CARTESIAN_POINT('Ctrl Pts',(-19.3077651468771,16.7146125685867,
3.26199479043275));
#131493=CARTESIAN_POINT('Ctrl Pts',(-19.3917756297612,16.7369484199208,
3.26631095317239));
#131494=CARTESIAN_POINT('Ctrl Pts',(-19.4730494799765,16.7585566832404,
3.27048651736348));
#131495=CARTESIAN_POINT('Ctrl Pts',(-19.5531988875823,16.7841583830433,
3.27466208155456));
#131496=CARTESIAN_POINT('Ctrl Pts',(-19.6318137018712,16.8135992081564,
3.27883764574565));
#131497=CARTESIAN_POINT('Ctrl Pts',(-19.7143991635786,16.8445270193712,
3.28322410775957));
#131498=CARTESIAN_POINT('Ctrl Pts',(-19.7952903977548,16.8796917438777,
3.28761056977348));
#131499=CARTESIAN_POINT('Ctrl Pts',(-19.8740394547192,16.9188590702831,
3.2919970317874));
#131500=CARTESIAN_POINT('Ctrl Pts',(-19.9527885116835,16.9580263966884,
3.29638349380132));
#131501=CARTESIAN_POINT('Ctrl Pts',(-20.0293949232977,17.0011959738741,
3.30076995581524));
#131502=CARTESIAN_POINT('Ctrl Pts',(-20.1034462555219,17.0480813808104,
3.30515641782916));
#131503=CARTESIAN_POINT('Ctrl Pts',(-20.1740903761505,17.092809520654,3.30934105222176));
#131504=CARTESIAN_POINT('Ctrl Pts',(-20.2426723273843,17.1410855493988,
3.31352568661436));
#131505=CARTESIAN_POINT('Ctrl Pts',(-20.3088136057117,17.19269325739,3.31771032100697));
#131506=CARTESIAN_POINT('Ctrl Pts',(-20.374860740116,17.2442275081965,3.32188899909046));
#131507=CARTESIAN_POINT('Ctrl Pts',(-20.4384737424745,17.2990837381083,
3.32606767717394));
#131508=CARTESIAN_POINT('Ctrl Pts',(-20.4993017308437,17.3570016723092,
3.33024635525743));
#131509=CARTESIAN_POINT('Ctrl Pts',(-20.5612200171964,17.4159577438638,
3.33449993314298));
#131510=CARTESIAN_POINT('Ctrl Pts',(-20.6202520574043,17.4780861035065,
3.33875351102853));
#131511=CARTESIAN_POINT('Ctrl Pts',(-20.6760617089389,17.5430682511945,
3.34300708891408));
#131512=CARTESIAN_POINT('Ctrl Pts',(-20.7307893814672,17.6067905931385,
3.34717820289156));
#131513=CARTESIAN_POINT('Ctrl Pts',(-20.7824181813928,17.6732566930095,
3.35134931686903));
#131514=CARTESIAN_POINT('Ctrl Pts',(-20.8306684931563,17.742129267156,3.35552043084651));
#131515=CARTESIAN_POINT('Ctrl Pts',(-20.8789026140616,17.810978730445,3.3596901451664));
#131516=CARTESIAN_POINT('Ctrl Pts',(-20.923760234583,17.8822326878121,3.36385985948629));
#131517=CARTESIAN_POINT('Ctrl Pts',(-20.9650035868519,17.955522801699,3.36802957380618));
#131518=CARTESIAN_POINT('Ctrl Pts',(-21.0062454715054,18.028810307609,3.37219913974974));
#131519=CARTESIAN_POINT('Ctrl Pts',(-21.0438731187515,18.1041334246492,
3.37636870569329));
#131520=CARTESIAN_POINT('Ctrl Pts',(-21.0776941561666,18.1810982074244,
3.38053827163685));
#131521=CARTESIAN_POINT('Ctrl Pts',(-21.1127042995431,18.2607689770352,
3.38485443437633));
#131522=CARTESIAN_POINT('Ctrl Pts',(-21.1436349596428,18.3421985193634,
3.3891705971158));
#131523=CARTESIAN_POINT('Ctrl Pts',(-21.1703273243944,18.4249280132143,
3.39348675985528));
#131524=CARTESIAN_POINT('Ctrl Pts',(-21.1961501881654,18.5049626024847,
3.39766232404647));
#131525=CARTESIAN_POINT('Ctrl Pts',(-21.2180065643708,18.5862132848946,
3.40183788823765));
#131526=CARTESIAN_POINT('Ctrl Pts',(-21.2358041974883,18.6682516628954,
3.40601345242883));
#131527=CARTESIAN_POINT('Ctrl Pts',(-21.2545007467516,18.7544336043729,
3.41039991444246));
#131528=CARTESIAN_POINT('Ctrl Pts',(-21.2687176692139,18.8414843294195,
3.41478637645609));
#131529=CARTESIAN_POINT('Ctrl Pts',(-21.2784095170101,18.9289003549305,
3.41917283846971));
#131530=CARTESIAN_POINT('Ctrl Pts',(-21.2881013648063,19.0163163804415,
3.42355930048334));
#131531=CARTESIAN_POINT('Ctrl Pts',(-21.293268179777,19.1040971227328,3.42794576249697));
#131532=CARTESIAN_POINT('Ctrl Pts',(-21.2939275539577,19.1917407557754,
3.43233222451059));
#131533=CARTESIAN_POINT('Ctrl Pts',(-21.2939755504833,19.1981204260763,
3.43265151959756));
#131534=CARTESIAN_POINT('Ctrl Pts',(-21.2939996986147,19.2045002760229,
3.43297081468453));
#131535=CARTESIAN_POINT('Ctrl Pts',(-21.2939999971965,19.2108801913083,
3.4332901097715));
#131536=CARTESIAN_POINT('',(-21.2936055426903,19.2106176052578,3.36670986511441));
#131537=CARTESIAN_POINT('Ctrl Pts',(-17.1746506278756,17.1811162280172,
3.08342410660674));
#131538=CARTESIAN_POINT('Ctrl Pts',(-17.6886694547963,16.794397148351,3.11541446008311));
#131539=CARTESIAN_POINT('Ctrl Pts',(-19.2309397104083,16.3326325381546,
3.18979674911996));
#131540=CARTESIAN_POINT('Ctrl Pts',(-21.0089154299348,17.5465283377359,
3.28422525530949));
#131541=CARTESIAN_POINT('Ctrl Pts',(-21.290373212379,18.8060182046973,3.34666340802265));
#131542=CARTESIAN_POINT('Ctrl Pts',(-21.2898371856445,19.2106133247715,
3.36670962517532));
#131543=CARTESIAN_POINT('Ctrl Pts',(-21.2939999715072,19.2106180532905,
3.36670989022851));
#131544=CARTESIAN_POINT('Ctrl Pts',(-21.2940130064034,19.2979845189442,
3.37103154303559));
#131545=CARTESIAN_POINT('Ctrl Pts',(-21.2895493128086,19.3852864628676,
3.37535319584268));
#131546=CARTESIAN_POINT('Ctrl Pts',(-21.2806546261691,19.4720559614555,
3.37967484864976));
#131547=CARTESIAN_POINT('Ctrl Pts',(-21.2713805337796,19.5625266412119,
3.38418084296218));
#131548=CARTESIAN_POINT('Ctrl Pts',(-21.2572890869444,19.6524179424097,
3.38868683727459));
#131549=CARTESIAN_POINT('Ctrl Pts',(-21.2384911684206,19.7412112666692,
3.393192831587));
#131550=CARTESIAN_POINT('Ctrl Pts',(-21.2204017935413,19.8266577339088,
3.3975289829656));
#131551=CARTESIAN_POINT('Ctrl Pts',(-21.1979545494935,19.911087135192,3.40186513434419));
#131552=CARTESIAN_POINT('Ctrl Pts',(-21.1712990035409,19.9940540002698,
3.40620128572279));
#131553=CARTESIAN_POINT('Ctrl Pts',(-21.1446099328528,20.0771252129461,
3.41054289068797));
#131554=CARTESIAN_POINT('Ctrl Pts',(-21.1137021554183,20.1587298407179,
3.41488449565315));
#131555=CARTESIAN_POINT('Ctrl Pts',(-21.0787731611217,20.2384428562617,
3.41922610061834));
#131556=CARTESIAN_POINT('Ctrl Pts',(-21.0437703953367,20.3183242290092,
3.42357687523375));
#131557=CARTESIAN_POINT('Ctrl Pts',(-21.0047296348366,20.3963056454717,
3.42792764984916));
#131558=CARTESIAN_POINT('Ctrl Pts',(-20.9618940508659,20.4719869539834,
3.43227842446457));
#131559=CARTESIAN_POINT('Ctrl Pts',(-20.9570751477604,20.4805009243513,
3.43276787644263));
#131560=CARTESIAN_POINT('Ctrl Pts',(-20.9522082623986,20.4889858169837,
3.43325732842068));
#131561=CARTESIAN_POINT('Ctrl Pts',(-20.9472937739975,20.4974410868688,
3.43374678039873));
#131562=CARTESIAN_POINT('Ctrl Pts',(-20.9052767057113,20.5697305345463,
3.43793141479118));
#131563=CARTESIAN_POINT('Ctrl Pts',(-20.8596361007269,20.6400938357955,
3.44211604918362));
#131564=CARTESIAN_POINT('Ctrl Pts',(-20.8105736599315,20.7081445604478,
3.44630068357607));
#131565=CARTESIAN_POINT('Ctrl Pts',(-20.7615810534479,20.7760984233165,
3.45047936165941));
#131566=CARTESIAN_POINT('Ctrl Pts',(-20.7091765523538,20.8417458779045,
3.45465803974274));
#131567=CARTESIAN_POINT('Ctrl Pts',(-20.6536069384425,20.9047264247462,
3.45883671782608));
#131568=CARTESIAN_POINT('Ctrl Pts',(-20.5970412791288,20.9688358526383,
3.46309029571167));
#131569=CARTESIAN_POINT('Ctrl Pts',(-20.5371961639062,21.0301814068962,
3.46734387359725));
#131570=CARTESIAN_POINT('Ctrl Pts',(-20.4743771168498,21.0884151089052,
3.47159745148284));
#131571=CARTESIAN_POINT('Ctrl Pts',(-20.412775939613,21.1455198369568,3.47576856546018));
#131572=CARTESIAN_POINT('Ctrl Pts',(-20.3483154653815,21.1996319675306,
3.47993967943753));
#131573=CARTESIAN_POINT('Ctrl Pts',(-20.2813221318913,21.250459296029,3.48411079341487));
#131574=CARTESIAN_POINT('Ctrl Pts',(-20.2143512786613,21.3012695689265,
3.48828050773464));
#131575=CARTESIAN_POINT('Ctrl Pts',(-20.1448496203246,21.3487969510057,
3.4924502220544));
#131576=CARTESIAN_POINT('Ctrl Pts',(-20.0731762130974,21.3927898776633,
3.49661993637416));
#131577=CARTESIAN_POINT('Ctrl Pts',(-20.0015053563176,21.4367812388638,
3.50078950231759));
#131578=CARTESIAN_POINT('Ctrl Pts',(-19.9276632968144,21.4772381547836,
3.50495906826103));
#131579=CARTESIAN_POINT('Ctrl Pts',(-19.8520364016656,21.5139534525367,
3.50912863420446));
#131580=CARTESIAN_POINT('Ctrl Pts',(-19.7737505581546,21.5519596148775,
3.5134447969441));
#131581=CARTESIAN_POINT('Ctrl Pts',(-19.6935525085944,21.585955922694,3.51776095968374));
#131582=CARTESIAN_POINT('Ctrl Pts',(-19.6118947218442,21.6157662791544,
3.52207712242338));
#131583=CARTESIAN_POINT('Ctrl Pts',(-19.5328969289329,21.6446055663797,
3.52625268661447));
#131584=CARTESIAN_POINT('Ctrl Pts',(-19.4525335041393,21.6695273345314,
3.53042825080555));
#131585=CARTESIAN_POINT('Ctrl Pts',(-19.3712290384541,21.690423149152,3.53460381499663));
#131586=CARTESIAN_POINT('Ctrl Pts',(-19.2858180774511,21.712374361704,3.53899027701055));
#131587=CARTESIAN_POINT('Ctrl Pts',(-19.1993690855429,21.7298821146793,
3.54337673902448));
#131588=CARTESIAN_POINT('Ctrl Pts',(-19.1123834602667,21.7428819002861,
3.5477632010384));
#131589=CARTESIAN_POINT('Ctrl Pts',(-19.0253978349904,21.755881685893,3.55214966305232));
#131590=CARTESIAN_POINT('Ctrl Pts',(-18.9378761611969,21.7643735238079,
3.55653612506624));
#131591=CARTESIAN_POINT('Ctrl Pts',(-18.8503205710795,21.7683559636358,
3.56092258708016));
#131592=CARTESIAN_POINT('Ctrl Pts',(-18.7667935434871,21.7721551655022,
3.56510722147276));
#131593=CARTESIAN_POINT('Ctrl Pts',(-18.6829247485325,21.771864959913,3.56929185586537));
#131594=CARTESIAN_POINT('Ctrl Pts',(-18.5991482896985,21.7674457780733,
3.57347649025797));
#131595=CARTESIAN_POINT('Ctrl Pts',(-18.5154910762845,21.7630328863919,
3.57765516834146));
#131596=CARTESIAN_POINT('Ctrl Pts',(-18.4319263933964,21.7545027162291,
3.58183384642494));
#131597=CARTESIAN_POINT('Ctrl Pts',(-18.3488909423388,21.7418676404955,
3.58601252450843));
#131598=CARTESIAN_POINT('Ctrl Pts',(-18.264367140486,21.7290060901083,3.59026610239398));
#131599=CARTESIAN_POINT('Ctrl Pts',(-18.1803922116833,21.7118910039099,
3.59451968027953));
#131600=CARTESIAN_POINT('Ctrl Pts',(-18.0974241252639,21.6905909250729,
3.59877325816508));
#131601=CARTESIAN_POINT('Ctrl Pts',(-18.0160645371101,21.6697037898308,
3.60294437214255));
#131602=CARTESIAN_POINT('Ctrl Pts',(-17.9356735666136,21.6447926020537,
3.60711548612003));
#131603=CARTESIAN_POINT('Ctrl Pts',(-17.8566736061543,21.6159736794114,
3.61128660009751));
#131604=CARTESIAN_POINT('Ctrl Pts',(-17.7777001548947,21.5871644272369,
3.6154563144174));
#131605=CARTESIAN_POINT('Ctrl Pts',(-17.7001172184808,21.5544502019411,
3.61962602873729));
#131606=CARTESIAN_POINT('Ctrl Pts',(-17.6243306732528,21.5179967458313,
3.62379574305719));
#131607=CARTESIAN_POINT('Ctrl Pts',(-17.5485468248354,21.481544586892,3.62796530900075));
#131608=CARTESIAN_POINT('Ctrl Pts',(-17.4745596547068,21.4413536618678,
3.63213487494431));
#131609=CARTESIAN_POINT('Ctrl Pts',(-17.4027524956497,21.3976367055734,
3.63630444088787));
#131610=CARTESIAN_POINT('Ctrl Pts',(-17.3284206854458,21.3523827150154,
3.64062060362735));
#131611=CARTESIAN_POINT('Ctrl Pts',(-17.2564254874566,21.3033504035823,
3.64493676636682));
#131612=CARTESIAN_POINT('Ctrl Pts',(-17.1871598840616,21.2508249081045,
3.6492529291063));
#131613=CARTESIAN_POINT('Ctrl Pts',(-17.1201506004284,21.2000104251299,
3.65342849329749));
#131614=CARTESIAN_POINT('Ctrl Pts',(-17.0556961397385,21.1459271830849,
3.65760405748867));
#131615=CARTESIAN_POINT('Ctrl Pts',(-16.9941175012612,21.0888735022845,
3.66177962167986));
#131616=CARTESIAN_POINT('Ctrl Pts',(-16.92942867212,21.0289381756772,3.66616608369348));
#131617=CARTESIAN_POINT('Ctrl Pts',(-16.8679142228486,20.965724868959,3.6705525457071));
#131618=CARTESIAN_POINT('Ctrl Pts',(-16.8098997912682,20.899620261266,3.67493900772073));
#131619=CARTESIAN_POINT('Ctrl Pts',(-16.7518853596878,20.8335156535731,
3.67932546973435));
#131620=CARTESIAN_POINT('Ctrl Pts',(-16.6973712458222,20.7645202473232,
3.68371193174797));
#131621=CARTESIAN_POINT('Ctrl Pts',(-16.6466304638568,20.6930554711553,
3.68809839376159));
#131622=CARTESIAN_POINT('Ctrl Pts',(-16.5982243404927,20.6248788952851,
3.69228302815505));
#131623=CARTESIAN_POINT('Ctrl Pts',(-16.553071769447,20.5542014284548,3.69646766254851));
#131624=CARTESIAN_POINT('Ctrl Pts',(-16.511440993796,20.4813666651568,3.70065229694197));
#131625=CARTESIAN_POINT('Ctrl Pts',(-16.4698694744012,20.4086355731289,
3.70483097502634));
#131626=CARTESIAN_POINT('Ctrl Pts',(-16.4318100196565,20.3337536798782,
3.70900965311071));
#131627=CARTESIAN_POINT('Ctrl Pts',(-16.3974886040354,20.2570948793143,
3.71318833119508));
#131628=CARTESIAN_POINT('Ctrl Pts',(-16.3625520017101,20.1790620248538,
3.71744190908041));
#131629=CARTESIAN_POINT('Ctrl Pts',(-16.3314890444372,20.0991883275084,
3.72169548696574));
#131630=CARTESIAN_POINT('Ctrl Pts',(-16.3044899883693,20.0178959681312,
3.72594906485107));
#131631=CARTESIAN_POINT('Ctrl Pts',(-16.2780143616844,19.9381796197593,
3.73012017882945));
#131632=CARTESIAN_POINT('Ctrl Pts',(-16.2554466207296,19.8570995822354,
3.73429129280783));
#131633=CARTESIAN_POINT('Ctrl Pts',(-16.2369175937362,19.7750739812542,
3.73846240678621));
#131634=CARTESIAN_POINT('Ctrl Pts',(-16.2183947843368,19.6930759047555,
3.74263212110702));
#131635=CARTESIAN_POINT('Ctrl Pts',(-16.2039080986716,19.6101333433014,
3.74680183542783));
#131636=CARTESIAN_POINT('Ctrl Pts',(-16.1935378668542,19.5266772878306,
3.75097154974863));
#131637=CARTESIAN_POINT('Ctrl Pts',(-16.1831680040541,19.4432242020842,
3.75514111569312));
#131638=CARTESIAN_POINT('Ctrl Pts',(-16.1769143597415,19.3592581152781,
3.7593106816376));
#131639=CARTESIAN_POINT('Ctrl Pts',(-16.174805548368,19.2752164989395,3.76348024758209));
#131640=CARTESIAN_POINT('Ctrl Pts',(-16.1726225937887,19.1882200830664,
3.7677964103205));
#131641=CARTESIAN_POINT('Ctrl Pts',(-16.1748813730051,19.1011432548615,
3.77211257305891));
#131642=CARTESIAN_POINT('Ctrl Pts',(-16.1815548449752,19.0144707894728,
3.77642873579732));
#131643=CARTESIAN_POINT('Ctrl Pts',(-16.1880109292992,18.9306216705092,
3.78060429998944));
#131644=CARTESIAN_POINT('Ctrl Pts',(-16.1985983999138,18.8471514360442,
3.78477986418156));
#131645=CARTESIAN_POINT('Ctrl Pts',(-16.2132401674605,18.7644914707922,
3.78895542837368));
#131646=CARTESIAN_POINT('Ctrl Pts',(-16.2286214558734,18.6776565472293,
3.79334189038524));
#131647=CARTESIAN_POINT('Ctrl Pts',(-16.2484772384201,18.5917164663174,
3.7977283523968));
#131648=CARTESIAN_POINT('Ctrl Pts',(-16.272658640717,18.5071543400128,3.80211481440835));
#131649=CARTESIAN_POINT('Ctrl Pts',(-16.2968400430139,18.4225922137082,
3.80650127641991));
#131650=CARTESIAN_POINT('Ctrl Pts',(-16.3253468050044,18.3394085662324,
3.81088773843147));
#131651=CARTESIAN_POINT('Ctrl Pts',(-16.3579723492966,18.2580610706385,
3.81527420044303));
#131652=CARTESIAN_POINT('Ctrl Pts',(-16.3890953380446,18.1804599993008,
3.81945864581525));
#131653=CARTESIAN_POINT('Ctrl Pts',(-16.424081917038,18.1042408407701,3.82364309118746));
#131654=CARTESIAN_POINT('Ctrl Pts',(-16.4627883931758,18.0298150707755,
3.82782753655968));
#131655=CARTESIAN_POINT('Ctrl Pts',(-16.5014420742954,17.9554908163484,
3.83200627441491));
#131656=CARTESIAN_POINT('Ctrl Pts',(-16.5438053666935,17.8829554976016,
3.83618501227014));
#131657=CARTESIAN_POINT('Ctrl Pts',(-16.5896861940407,17.8126015226079,
3.84036375012537));
#131658=CARTESIAN_POINT('Ctrl Pts',(-16.635512417077,17.7423312782389,3.84453751472457));
#131659=CARTESIAN_POINT('Ctrl Pts',(-16.6848476027862,17.6742375999541,
3.84871127932376));
#131660=CARTESIAN_POINT('Ctrl Pts',(-16.7374540925027,17.6086877834655,
3.85288504392296));
#131661=CARTESIAN_POINT('Ctrl Pts',(-16.7900243343834,17.5431831332481,
3.8570559326425));
#131662=CARTESIAN_POINT('Ctrl Pts',(-16.8458611158911,17.4802192208169,
3.86122682136205));
#131663=CARTESIAN_POINT('Ctrl Pts',(-16.9046845018978,17.4201329450786,
3.86539771008159));
#131664=CARTESIAN_POINT('Ctrl Pts',(-16.9634896683862,17.3600652800165,
3.86956730694107));
#131665=CARTESIAN_POINT('Ctrl Pts',(-17.0252792822166,17.3028738113101,
3.87373690380055));
#131666=CARTESIAN_POINT('Ctrl Pts',(-17.0897351511635,17.2488600694954,
3.87790650066003));
#131667=CARTESIAN_POINT('Ctrl Pts',(-17.1174932740853,17.2255988815034,
3.87970215067687));
#131668=CARTESIAN_POINT('Ctrl Pts',(-17.1457454288767,17.2029265699414,
3.8814978006937));
#131669=CARTESIAN_POINT('Ctrl Pts',(-17.174464231106,17.180864983421,3.88329345071054));
#131670=CARTESIAN_POINT('Origin',(-18.734,19.211,-1.76670989022852));
#131671=CARTESIAN_POINT('',(-17.1762220704532,17.1831893817011,4.7499734657924));
#131672=CARTESIAN_POINT('',(-17.1735447493683,17.1796894255362,4.68319930527189));
#131673=CARTESIAN_POINT('',(-17.174464231106,17.180864983421,-1.76670989022852));
#131674=CARTESIAN_POINT('',(-21.2939990418858,19.2087851537695,4.23329008725203));
#131675=CARTESIAN_POINT('Ctrl Pts',(-21.2923873880696,19.2087870015046,
4.2332901097715));
#131676=CARTESIAN_POINT('Ctrl Pts',(-21.2874613882922,19.8078856368616,
4.26304769694121));
#131677=CARTESIAN_POINT('Ctrl Pts',(-20.7784814085672,21.2679844548948,
4.3351972196714));
#131678=CARTESIAN_POINT('Ctrl Pts',(-18.3440265327566,22.212868160657,4.44973867796206));
#131679=CARTESIAN_POINT('Ctrl Pts',(-15.9988186914362,20.5079483291182,
4.5769144846435));
#131680=CARTESIAN_POINT('Ctrl Pts',(-16.1279939788785,18.2299561235477,
4.67699274725361));
#131681=CARTESIAN_POINT('Ctrl Pts',(-16.9304194998099,17.3693100983237,
4.73467907430325));
#131682=CARTESIAN_POINT('Ctrl Pts',(-17.1762220704533,17.183189381701,4.74997346579241));
#131683=CARTESIAN_POINT('Ctrl Pts',(-17.174464231106,17.180864983421,3.94993168719587));
#131684=CARTESIAN_POINT('Ctrl Pts',(-17.2408642333853,17.1298569579628,
3.95411195751233));
#131685=CARTESIAN_POINT('Ctrl Pts',(-17.3098752464746,17.0820286544136,
3.95829222782878));
#131686=CARTESIAN_POINT('Ctrl Pts',(-17.3811592903901,17.0376564895484,
3.96247249814524));
#131687=CARTESIAN_POINT('Ctrl Pts',(-17.4523586048633,16.9933370662026,
3.9666477997204));
#131688=CARTESIAN_POINT('Ctrl Pts',(-17.5258251943333,16.9524658616689,
3.97082310129556));
#131689=CARTESIAN_POINT('Ctrl Pts',(-17.6011899553232,16.915277585883,3.97499840287073));
#131690=CARTESIAN_POINT('Ctrl Pts',(-17.6764915764994,16.8781204660482,
3.9791702064216));
#131691=CARTESIAN_POINT('Ctrl Pts',(-17.7536877979744,16.8446403465275,
3.98334200997247));
#131692=CARTESIAN_POINT('Ctrl Pts',(-17.832383755932,16.8150266803588,3.98751381352334));
#131693=CARTESIAN_POINT('Ctrl Pts',(-17.9110459750257,16.7854257102862,
3.99168382852096));
#131694=CARTESIAN_POINT('Ctrl Pts',(-17.9912062238471,16.7596880637534,
3.99585384351857));
#131695=CARTESIAN_POINT('Ctrl Pts',(-18.0724495705645,16.7379551097253,
4.00002385851619));
#131696=CARTESIAN_POINT('Ctrl Pts',(-18.1536824574235,16.7162249537556,
4.0041933366358));
#131697=CARTESIAN_POINT('Ctrl Pts',(-18.235997720657,16.6984985843148,4.0083628147554));
#131698=CARTESIAN_POINT('Ctrl Pts',(-18.3189664976901,16.6848671468111,
4.01253229287501));
#131699=CARTESIAN_POINT('Ctrl Pts',(-18.4019494810084,16.6712333752716,
4.01670248491132));
#131700=CARTESIAN_POINT('Ctrl Pts',(-18.4855857462034,16.6616960011917,
4.02087267694763));
#131701=CARTESIAN_POINT('Ctrl Pts',(-18.569438860629,16.6562946096646,4.02504286898394));
#131702=CARTESIAN_POINT('Ctrl Pts',(-18.6533844036521,16.6508872643569,
4.02921765768912));
#131703=CARTESIAN_POINT('Ctrl Pts',(-18.7375468131607,16.6496250298472,
4.0333924463943));
#131704=CARTESIAN_POINT('Ctrl Pts',(-18.8214877370601,16.6524953789637,
4.03756723509948));
#131705=CARTESIAN_POINT('Ctrl Pts',(-18.9054812334263,16.655367525789,4.04174463848807));
#131706=CARTESIAN_POINT('Ctrl Pts',(-18.9892525099869,16.6623773694637,
4.04592204187665));
#131707=CARTESIAN_POINT('Ctrl Pts',(-19.0723688153353,16.6734605333496,
4.05009944526523));
#131708=CARTESIAN_POINT('Ctrl Pts',(-19.1556216891913,16.6845619079962,
4.05428371255066));
#131709=CARTESIAN_POINT('Ctrl Pts',(-19.2382169920771,16.6997498783073,
4.0584679798361));
#131710=CARTESIAN_POINT('Ctrl Pts',(-19.3197330693514,16.7189091566582,
4.06265224712154));
#131711=CARTESIAN_POINT('Ctrl Pts',(-19.355832480369,16.7273938468827,4.06450525072028));
#131712=CARTESIAN_POINT('Ctrl Pts',(-19.391720451714,16.736656722528,4.06635825431902));
#131713=CARTESIAN_POINT('Ctrl Pts',(-19.4273615317729,16.7466847226344,
4.06821125791776));
#131714=CARTESIAN_POINT('Ctrl Pts',(-19.5078497129729,16.7693309356085,
4.0723958923108));
#131715=CARTESIAN_POINT('Ctrl Pts',(-19.5873770243864,16.7959667334644,
4.07658052670384));
#131716=CARTESIAN_POINT('Ctrl Pts',(-19.6655189252299,16.826493239276,4.08076516109689));
#131717=CARTESIAN_POINT('Ctrl Pts',(-19.7435496007498,16.8569762943851,
4.08494383918084));
#131718=CARTESIAN_POINT('Ctrl Pts',(-19.8201983578021,16.8913388913937,
4.08912251726478));
#131719=CARTESIAN_POINT('Ctrl Pts',(-19.8950545149197,16.9294320274459,
4.09330119534873));
#131720=CARTESIAN_POINT('Ctrl Pts',(-19.9712524148554,16.9682079555848,
4.09755477323417));
#131721=CARTESIAN_POINT('Ctrl Pts',(-20.0455923539259,17.0108493474662,
4.1018083511196));
#131722=CARTESIAN_POINT('Ctrl Pts',(-20.1176611149876,17.0571471919207,
4.10606192900504));
#131723=CARTESIAN_POINT('Ctrl Pts',(-20.1883326824854,17.1025474623176,
4.11023304298298));
#131724=CARTESIAN_POINT('Ctrl Pts',(-20.2568199436827,17.1514634154309,
4.11440415696093));
#131725=CARTESIAN_POINT('Ctrl Pts',(-20.3227584711506,17.2036518686717,
4.11857527093887));
#131726=CARTESIAN_POINT('Ctrl Pts',(-20.3886748723087,17.2558228095729,
4.12274498525923));
#131727=CARTESIAN_POINT('Ctrl Pts',(-20.4520438778608,17.3112637844568,
4.1269146995796));
#131728=CARTESIAN_POINT('Ctrl Pts',(-20.5125322737859,17.369689881877,4.13108441389996));
#131729=CARTESIAN_POINT('Ctrl Pts',(-20.5730185172744,17.4281139002461,
4.13525397984401));
#131730=CARTESIAN_POINT('Ctrl Pts',(-20.6306240246489,17.4895225097361,
4.13942354578805));
#131731=CARTESIAN_POINT('Ctrl Pts',(-20.685051752926,17.5535932733923,4.14359311173209));
#131732=CARTESIAN_POINT('Ctrl Pts',(-20.7413930929855,17.619916686059,4.14790927447102));
#131733=CARTESIAN_POINT('Ctrl Pts',(-20.7943286933424,17.6890925366907,
4.15222543720994));
#131734=CARTESIAN_POINT('Ctrl Pts',(-20.8435751066799,17.760726622572,4.15654159994887));
#131735=CARTESIAN_POINT('Ctrl Pts',(-20.8912173232827,17.8300272356402,
4.16071716414055));
#131736=CARTESIAN_POINT('Ctrl Pts',(-20.9354068051751,17.9016279637399,
4.16489272833223));
#131737=CARTESIAN_POINT('Ctrl Pts',(-20.9759325838399,17.9751447133596,
4.16906829252391));
#131738=CARTESIAN_POINT('Ctrl Pts',(-21.0185052232442,18.0523746192331,
4.17345475453645));
#131739=CARTESIAN_POINT('Ctrl Pts',(-21.0570340704739,18.1317186646461,
4.177841216549));
#131740=CARTESIAN_POINT('Ctrl Pts',(-21.091331525063,18.2127074171646,4.18222767856155));
#131741=CARTESIAN_POINT('Ctrl Pts',(-21.1256289796521,18.2936961696831,
4.1866141405741));
#131742=CARTESIAN_POINT('Ctrl Pts',(-21.1556949146933,18.3763290580523,
4.19100060258664));
#131743=CARTESIAN_POINT('Ctrl Pts',(-21.1814026084241,18.4601202011779,
4.19538706459919));
#131744=CARTESIAN_POINT('Ctrl Pts',(-21.211365847261,18.557781782967,4.20049964335899));
#131745=CARTESIAN_POINT('Ctrl Pts',(-21.2355013786602,18.6573099274653,
4.20561222211879));
#131746=CARTESIAN_POINT('Ctrl Pts',(-21.2536149670824,18.758075704279,4.21072480087859));
#131747=CARTESIAN_POINT('Ctrl Pts',(-21.271481685507,18.8574681448711,4.2157677003304));
#131748=CARTESIAN_POINT('Ctrl Pts',(-21.2834894543748,18.9580647258708,
4.22081059978222));
#131749=CARTESIAN_POINT('Ctrl Pts',(-21.289497836736,19.0592409592887,4.22585349923404));
#131750=CARTESIAN_POINT('Ctrl Pts',(-21.2924512874047,19.1089746473736,
4.2283323619067));
#131751=CARTESIAN_POINT('Ctrl Pts',(-21.293955837589,19.1588480714825,4.23081122457936));
#131752=CARTESIAN_POINT('Ctrl Pts',(-21.2939990418858,19.2087851537695,
4.23329008725203));
#131753=CARTESIAN_POINT('',(-21.2939989159607,19.2133559031925,4.16670989022851));
#131754=CARTESIAN_POINT('Ctrl Pts',(-17.174464231106,17.180864983421,3.88329345071054));
#131755=CARTESIAN_POINT('Ctrl Pts',(-17.2411551865789,17.1296334497189,
3.887463318742));
#131756=CARTESIAN_POINT('Ctrl Pts',(-17.3103645228761,17.0816983118158,
3.89163318677346));
#131757=CARTESIAN_POINT('Ctrl Pts',(-17.3817276205797,17.0373028242515,
3.89580305480492));
#131758=CARTESIAN_POINT('Ctrl Pts',(-17.4531659153384,16.9928605560677,
3.89997731672912));
#131759=CARTESIAN_POINT('Ctrl Pts',(-17.5267621115622,16.9519656290489,
3.90415157865332));
#131760=CARTESIAN_POINT('Ctrl Pts',(-17.6021248960207,16.914816481857,3.90832584057752));
#131761=CARTESIAN_POINT('Ctrl Pts',(-17.6775292444906,16.8776468462026,
3.91250240468669));
#131762=CARTESIAN_POINT('Ctrl Pts',(-17.7547016988925,16.8442272867161,
3.91667896879587));
#131763=CARTESIAN_POINT('Ctrl Pts',(-17.8332310067443,16.814708026807,3.92085553290504));
#131764=CARTESIAN_POINT('Ctrl Pts',(-17.9118959414518,16.7851377846021,
3.92503931029895));
#131765=CARTESIAN_POINT('Ctrl Pts',(-17.991921971515,16.7594814360342,3.92922308769286));
#131766=CARTESIAN_POINT('Ctrl Pts',(-18.0728829745269,16.7378392129444,
3.93340686508677));
#131767=CARTESIAN_POINT('Ctrl Pts',(-18.1312147786055,16.7222461512216,
3.936421245766));
#131768=CARTESIAN_POINT('Ctrl Pts',(-18.1900316496069,16.708735796216,3.93943562644523));
#131769=CARTESIAN_POINT('Ctrl Pts',(-18.249172131343,16.6973289917387,3.94245000712447));
#131770=CARTESIAN_POINT('Ctrl Pts',(-18.3312723437006,16.6814937965827,
3.94663464151747));
#131771=CARTESIAN_POINT('Ctrl Pts',(-18.4143019582715,16.6696556340513,
3.95081927591047));
#131772=CARTESIAN_POINT('Ctrl Pts',(-18.4978371529754,16.6619164176738,
3.95500391030347));
#131773=CARTESIAN_POINT('Ctrl Pts',(-18.5812534456692,16.6541882171128,
3.95918258838736));
#131774=CARTESIAN_POINT('Ctrl Pts',(-18.6651734349295,16.6505474159413,
3.96336126647126));
#131775=CARTESIAN_POINT('Ctrl Pts',(-18.7491632186827,16.651044907269,3.96753994455515));
#131776=CARTESIAN_POINT('Ctrl Pts',(-18.8346584589486,16.6515513157714,
3.9717935224406));
#131777=CARTESIAN_POINT('Ctrl Pts',(-18.9202255470369,16.6563459251098,
3.97604710032605));
#131778=CARTESIAN_POINT('Ctrl Pts',(-19.0054014154824,16.6654271230872,
3.9803006782115));
#131779=CARTESIAN_POINT('Ctrl Pts',(-19.0889259835097,16.6743322643211,
3.98447179218939));
#131780=CARTESIAN_POINT('Ctrl Pts',(-19.172073887133,16.6873592186152,3.98864290616729));
#131781=CARTESIAN_POINT('Ctrl Pts',(-19.2544103550733,16.7044539576675,
3.99281402014518));
#131782=CARTESIAN_POINT('Ctrl Pts',(-19.3367191942165,16.7215429604151,
3.9969837344655));
#131783=CARTESIAN_POINT('Ctrl Pts',(-19.4182166883867,16.7426969435999,
4.00115344878582));
#131784=CARTESIAN_POINT('Ctrl Pts',(-19.4984772632642,16.76781058574,4.00532316310613));
#131785=CARTESIAN_POINT('Ctrl Pts',(-19.5787349821259,16.792923334229,4.00949272905011));
#131786=CARTESIAN_POINT('Ctrl Pts',(-19.6577554304202,16.8219953233345,
4.0136622949941));
#131787=CARTESIAN_POINT('Ctrl Pts',(-19.7351285466043,16.8548714735452,
4.01783186093808));
#131788=CARTESIAN_POINT('Ctrl Pts',(-19.8152220061057,16.8889035086413,
4.02214802367707));
#131789=CARTESIAN_POINT('Ctrl Pts',(-19.8935496523609,16.9270119844455,
4.02646418641605));
#131790=CARTESIAN_POINT('Ctrl Pts',(-19.9696814080995,16.9689715751853,
4.03078034915504));
#131791=CARTESIAN_POINT('Ctrl Pts',(-20.0433331799005,17.0095643366689,
4.03495591334666));
#131792=CARTESIAN_POINT('Ctrl Pts',(-20.1149295504513,17.0537608783676,
4.03913147753828));
#131793=CARTESIAN_POINT('Ctrl Pts',(-20.1841097633269,17.1013124225839,
4.04330704172991));
#131794=CARTESIAN_POINT('Ctrl Pts',(-20.2567841042975,17.1512656822575,
4.04769350374257));
#131795=CARTESIAN_POINT('Ctrl Pts',(-20.3267913293723,17.2049214186621,
4.05207996575524));
#131796=CARTESIAN_POINT('Ctrl Pts',(-20.3937533178432,17.2619440942066,
4.0564664277679));
#131797=CARTESIAN_POINT('Ctrl Pts',(-20.4607153063142,17.318966769751,4.06085288978057));
#131798=CARTESIAN_POINT('Ctrl Pts',(-20.5246316886729,17.3793559306721,
4.06523935179323));
#131799=CARTESIAN_POINT('Ctrl Pts',(-20.5851713910718,17.4427340469043,
4.0696258138059));
#131800=CARTESIAN_POINT('Ctrl Pts',(-20.6421808499863,17.5024164036099,
4.07375648865202));
#131801=CARTESIAN_POINT('Ctrl Pts',(-20.6964202744402,17.5649836670307,
4.07788716349815));
#131802=CARTESIAN_POINT('Ctrl Pts',(-20.7475781317949,17.6301448177783,
4.08201783834428));
#131803=CARTESIAN_POINT('Ctrl Pts',(-20.7986699217384,17.6952218166719,
4.08614317866296));
#131804=CARTESIAN_POINT('Ctrl Pts',(-20.8466877493677,17.7628856907895,
4.09026851898165));
#131805=CARTESIAN_POINT('Ctrl Pts',(-20.8913569516644,17.8328088002366,
4.09439385930033));
#131806=CARTESIAN_POINT('Ctrl Pts',(-20.9359826817961,17.9026638603613,
4.09851518482883));
#131807=CARTESIAN_POINT('Ctrl Pts',(-20.977265999821,17.9747733973533,4.10263651035733));
#131808=CARTESIAN_POINT('Ctrl Pts',(-21.0149735460515,18.0487781269426,
4.10675783588582));
#131809=CARTESIAN_POINT('Ctrl Pts',(-21.0526563884393,18.122734372836,4.1108764613559));
#131810=CARTESIAN_POINT('Ctrl Pts',(-21.0867678956213,18.1985829265156,
4.11499508682597));
#131811=CARTESIAN_POINT('Ctrl Pts',(-21.117119754579,18.2759383788566,4.11911371229604));
#131812=CARTESIAN_POINT('Ctrl Pts',(-21.1474714047475,18.3532932990728,
4.12323230943427));
#131813=CARTESIAN_POINT('Ctrl Pts',(-21.174063267692,18.4321546644581,4.1273509065725));
#131814=CARTESIAN_POINT('Ctrl Pts',(-21.1967549321189,18.5121165016086,
4.13146950371073));
#131815=CARTESIAN_POINT('Ctrl Pts',(-21.2194452848828,18.5920737166658,
4.13558786277863));
#131816=CARTESIAN_POINT('Ctrl Pts',(-21.238235765403,18.6731308198826,4.13970622184654));
#131817=CARTESIAN_POINT('Ctrl Pts',(-21.2530362470694,18.7548680169614,
4.14382458091445));
#131818=CARTESIAN_POINT('Ctrl Pts',(-21.2678499327185,18.8366781344066,
4.14794661410212));
#131819=CARTESIAN_POINT('Ctrl Pts',(-21.2786664327327,18.9191690901919,
4.1520686472898));
#131820=CARTESIAN_POINT('Ctrl Pts',(-21.2854471635996,19.001913005284,4.15619068047748));
#131821=CARTESIAN_POINT('Ctrl Pts',(-21.2912151852698,19.0722990307271,
4.15969708372782));
#131822=CARTESIAN_POINT('Ctrl Pts',(-21.2940637843831,19.1428678239492,
4.16320348697816));
#131823=CARTESIAN_POINT('Ctrl Pts',(-21.2939989159607,19.2133559031925,
4.16670989022851));
#131824=CARTESIAN_POINT('Ctrl Pts',(-21.2939117877142,19.2133565885178,
4.16670992830965));
#131825=CARTESIAN_POINT('Ctrl Pts',(-21.2957664845097,19.4149927548523,
4.17674049236887));
#131826=CARTESIAN_POINT('Ctrl Pts',(-21.1817726734028,20.4667260333026,
4.22916299198858));
#131827=CARTESIAN_POINT('Ctrl Pts',(-19.7309870503076,22.0692002142848,
4.32397742716876));
#131828=CARTESIAN_POINT('Ctrl Pts',(-16.8703561207535,21.5963978986231,
4.4511532338502));
#131829=CARTESIAN_POINT('Ctrl Pts',(-15.78678603666,19.0907282468595,4.57089385988457));
#131830=CARTESIAN_POINT('Ctrl Pts',(-16.6213792270115,17.6125716320285,
4.64824255035846));
#131831=CARTESIAN_POINT('Ctrl Pts',(-17.1735447493682,17.1796894255362,
4.68319930527188));
#131832=CARTESIAN_POINT('Origin',(-18.734,19.211,-1.76670989022852));
#131833=CARTESIAN_POINT('',(-17.174464231106,17.180864983421,5.54983331567207));
#131834=CARTESIAN_POINT('',(-17.174464231106,17.180864983421,5.4833696502435));
#131835=CARTESIAN_POINT('',(-17.174464231106,17.180864983421,-1.76670989022852));
#131836=CARTESIAN_POINT('',(-21.2938494844892,19.2121967450766,5.03329016024561));
#131837=CARTESIAN_POINT('Ctrl Pts',(-21.2939997202205,19.2121968587231,
5.03329016239734));
#131838=CARTESIAN_POINT('Ctrl Pts',(-21.293956476523,19.3046921979846,5.03786858507676));
#131839=CARTESIAN_POINT('Ctrl Pts',(-21.2888961385951,19.397020737122,5.04244700775617));
#131840=CARTESIAN_POINT('Ctrl Pts',(-21.2788976615039,19.4886614709891,
5.04702543043559));
#131841=CARTESIAN_POINT('Ctrl Pts',(-21.2688681118718,19.5805869992732,
5.0516180816045));
#131842=CARTESIAN_POINT('Ctrl Pts',(-21.2538698091613,19.6718201549447,
5.0562107327734));
#131843=CARTESIAN_POINT('Ctrl Pts',(-21.234032630531,19.7618510200409,5.0608033839423));
#131844=CARTESIAN_POINT('Ctrl Pts',(-21.2141037578168,19.8522980379506,
5.06541726388317));
#131845=CARTESIAN_POINT('Ctrl Pts',(-21.1892913049467,19.9415313457699,
5.07003114382404));
#131846=CARTESIAN_POINT('Ctrl Pts',(-21.1597755903685,20.0290542678652,
5.07464502376491));
#131847=CARTESIAN_POINT('Ctrl Pts',(-21.1363775884239,20.0984363421481,
5.07830258629969));
#131848=CARTESIAN_POINT('Ctrl Pts',(-21.1100249393954,20.1667439285117,
5.08196014883446));
#131849=CARTESIAN_POINT('Ctrl Pts',(-21.0808281256645,20.233740313369,5.08561771136923));
#131850=CARTESIAN_POINT('Ctrl Pts',(-21.0474239145965,20.3103911904541,
5.08980234576228));
#131851=CARTESIAN_POINT('Ctrl Pts',(-21.010198294198,20.3855464442561,5.09398698015533));
#131852=CARTESIAN_POINT('Ctrl Pts',(-20.9693070771846,20.458798970463,5.09817161454838));
#131853=CARTESIAN_POINT('Ctrl Pts',(-20.9284740637573,20.5319472307656,
5.10235029263232));
#131854=CARTESIAN_POINT('Ctrl Pts',(-20.8839860396698,20.6031977447538,
5.10652897071627));
#131855=CARTESIAN_POINT('Ctrl Pts',(-20.8360465870688,20.6721639695093,
5.11070764880021));
#131856=CARTESIAN_POINT('Ctrl Pts',(-20.7872478542335,20.7423663642784,
5.11496122668565));
#131857=CARTESIAN_POINT('Ctrl Pts',(-20.734872934752,20.8102013305707,5.11921480457108));
#131858=CARTESIAN_POINT('Ctrl Pts',(-20.6791852047648,20.8752879916541,
5.12346838245652));
#131859=CARTESIAN_POINT('Ctrl Pts',(-20.6245770900892,20.9391128208062,
5.12763949643447));
#131860=CARTESIAN_POINT('Ctrl Pts',(-20.5667837820758,21.0002945906743,
5.13181061041242));
#131861=CARTESIAN_POINT('Ctrl Pts',(-20.506095860174,21.0585054160554,5.13598172439037));
#131862=CARTESIAN_POINT('Ctrl Pts',(-20.4454283026905,21.1166967082319,
5.14015143871074));
#131863=CARTESIAN_POINT('Ctrl Pts',(-20.381868392088,21.1719187176573,5.14432115303111));
#131864=CARTESIAN_POINT('Ctrl Pts',(-20.3157437934276,21.2238801683044,
5.14849086735148));
#131865=CARTESIAN_POINT('Ctrl Pts',(-20.2496215477641,21.2758397699402,
5.15266043329552));
#131866=CARTESIAN_POINT('Ctrl Pts',(-20.180935157738,21.3245387599149,5.15682999923957));
#131867=CARTESIAN_POINT('Ctrl Pts',(-20.1100445342432,21.3697268098996,
5.16099956518361));
#131868=CARTESIAN_POINT('Ctrl Pts',(-20.0366614838794,21.4165036159763,
5.16531572792253));
#131869=CARTESIAN_POINT('Ctrl Pts',(-19.9609167591477,21.4595177156538,
5.16963189066145));
#131870=CARTESIAN_POINT('Ctrl Pts',(-19.8832395142306,21.4985420299813,
5.17394805340037));
#131871=CARTESIAN_POINT('Ctrl Pts',(-19.8080925973965,21.5362951313742,
5.17812361759205));
#131872=CARTESIAN_POINT('Ctrl Pts',(-19.7311375805024,21.5703142429021,
5.18229918178373));
#131873=CARTESIAN_POINT('Ctrl Pts',(-19.6527837251099,21.6004427104396,
5.18647474597541));
#131874=CARTESIAN_POINT('Ctrl Pts',(-19.5704724027502,21.6320928952488,
5.19086120798796));
#131875=CARTESIAN_POINT('Ctrl Pts',(-19.4866177726057,21.6594488930308,
5.1952476700005));
#131876=CARTESIAN_POINT('Ctrl Pts',(-19.4017104542221,21.6823888300554,
5.19963413201304));
#131877=CARTESIAN_POINT('Ctrl Pts',(-19.3168031358385,21.7053287670799,
5.20402059402558));
#131878=CARTESIAN_POINT('Ctrl Pts',(-19.2308437124363,21.723852595477,5.20840705603813));
#131879=CARTESIAN_POINT('Ctrl Pts',(-19.1443308019265,21.7379009939035,
5.21279351805067));
#131880=CARTESIAN_POINT('Ctrl Pts',(-19.0617984786721,21.7513030046936,
5.21697815244372));
#131881=CARTESIAN_POINT('Ctrl Pts',(-18.9784552815194,21.7606822624715,
5.22116278683677));
#131882=CARTESIAN_POINT('Ctrl Pts',(-18.894727859237,21.7659494232303,5.22534742122981));
#131883=CARTESIAN_POINT('Ctrl Pts',(-18.8111196125767,21.7712090868378,
5.22952609931376));
#131884=CARTESIAN_POINT('Ctrl Pts',(-18.7271286822943,21.7723682508116,
5.23370477739771));
#131885=CARTESIAN_POINT('Ctrl Pts',(-18.6431902849674,21.7693888671693,
5.23788345548165));
#131886=CARTESIAN_POINT('Ctrl Pts',(-18.5577473521938,21.7663560802164,
5.24213703336709));
#131887=CARTESIAN_POINT('Ctrl Pts',(-18.4723593301117,21.7590348421053,
5.24639061125252));
#131888=CARTESIAN_POINT('Ctrl Pts',(-18.3874890362873,21.7474404491387,
5.25064418913796));
#131889=CARTESIAN_POINT('Ctrl Pts',(-18.3042641187194,21.7360708361043,
5.25481530311591));
#131890=CARTESIAN_POINT('Ctrl Pts',(-18.2215375109945,21.7205923416799,
5.25898641709386));
#131891=CARTESIAN_POINT('Ctrl Pts',(-18.1397421978238,21.7010718191555,
5.26315753107181));
#131892=CARTESIAN_POINT('Ctrl Pts',(-18.0579743318604,21.681557846931,5.26732724539218));
#131893=CARTESIAN_POINT('Ctrl Pts',(-17.977137586906,21.6580046470219,5.27149695971256));
#131894=CARTESIAN_POINT('Ctrl Pts',(-17.8976542388868,21.6305300717015,
5.27566667403293));
#131895=CARTESIAN_POINT('Ctrl Pts',(-17.8181737192262,21.6030564740444,
5.27983623997698));
#131896=CARTESIAN_POINT('Ctrl Pts',(-17.7400469352591,21.5716619295132,
5.28400580592102));
#131897=CARTESIAN_POINT('Ctrl Pts',(-17.6636791864352,21.536513568236,5.28817537186506));
#131898=CARTESIAN_POINT('Ctrl Pts',(-17.5846264417725,21.5001294339366,
5.29249153460398));
#131899=CARTESIAN_POINT('Ctrl Pts',(-17.5074592081876,21.4597228236283,
5.29680769734291));
#131900=CARTESIAN_POINT('Ctrl Pts',(-17.4326007161618,21.4155316745344,
5.30112386008182));
#131901=CARTESIAN_POINT('Ctrl Pts',(-17.3601807316399,21.3727800474741,
5.3052994242735));
#131902=CARTESIAN_POINT('Ctrl Pts',(-17.2899217514085,21.3264869565081,
5.30947498846518));
#131903=CARTESIAN_POINT('Ctrl Pts',(-17.2221770223173,21.276911731936,5.31365055265686));
#131904=CARTESIAN_POINT('Ctrl Pts',(-17.1510106680076,21.2248325806246,
5.3180370146694));
#131905=CARTESIAN_POINT('Ctrl Pts',(-17.0826196821851,21.1691313897079,
5.32242347668194));
#131906=CARTESIAN_POINT('Ctrl Pts',(-17.0173721044249,21.1101547246429,
5.32680993869448));
#131907=CARTESIAN_POINT('Ctrl Pts',(-16.9521245266647,21.0511780595779,
5.33119640070702));
#131908=CARTESIAN_POINT('Ctrl Pts',(-16.890020712904,20.9889263848495,5.33558286271956));
#131909=CARTESIAN_POINT('Ctrl Pts',(-16.8313804354228,20.923786849695,5.3399693247321));
#131910=CARTESIAN_POINT('Ctrl Pts',(-16.7754382840342,20.8616444811128,
5.34415395912515));
#131911=CARTESIAN_POINT('Ctrl Pts',(-16.7224397206527,20.7966428559978,
5.3483385935182));
#131912=CARTESIAN_POINT('Ctrl Pts',(-16.6726908063355,20.7290923582293,
5.35252322791125));
#131913=CARTESIAN_POINT('Ctrl Pts',(-16.62301270344,20.6616380102332,5.35670190599519));
#131914=CARTESIAN_POINT('Ctrl Pts',(-16.5765753324319,20.5916423631924,
5.36088058407914));
#131915=CARTESIAN_POINT('Ctrl Pts',(-16.533646260122,20.5194507707226,5.36505926216308));
#131916=CARTESIAN_POINT('Ctrl Pts',(-16.4899477150434,20.4459651958411,
5.36931284004852));
#131917=CARTESIAN_POINT('Ctrl Pts',(-16.4498848008427,20.3702045348862,
5.37356641793395));
#131918=CARTESIAN_POINT('Ctrl Pts',(-16.4136951701205,20.2925662237873,
5.37781999581939));
#131919=CARTESIAN_POINT('Ctrl Pts',(-16.378207146008,20.2164330828478,5.38199110979734));
#131920=CARTESIAN_POINT('Ctrl Pts',(-16.3464437665668,20.1384948820615,
5.38616222377529));
#131921=CARTESIAN_POINT('Ctrl Pts',(-16.3185831851716,20.0591518794675,
5.39033333775325));
#131922=CARTESIAN_POINT('Ctrl Pts',(-16.2907319526636,19.9798355011842,
5.39450305207362));
#131923=CARTESIAN_POINT('Ctrl Pts',(-16.2667810695588,19.8991156909808,
5.398672766394));
#131924=CARTESIAN_POINT('Ctrl Pts',(-16.2468600106956,19.8174113072848,
5.40284248071437));
#131925=CARTESIAN_POINT('Ctrl Pts',(-16.2269396607092,19.7357098309814,
5.40701204665841));
#131926=CARTESIAN_POINT('Ctrl Pts',(-16.2110489579958,19.6530242979865,
5.41118161260246));
#131927=CARTESIAN_POINT('Ctrl Pts',(-16.1992667534716,19.5697859653661,
5.4153511785465));
#131928=CARTESIAN_POINT('Ctrl Pts',(-16.1870703011713,19.4836210756562,
5.41966734128542));
#131929=CARTESIAN_POINT('Ctrl Pts',(-16.1792767060087,19.3968643124029,
5.42398350402434));
#131930=CARTESIAN_POINT('Ctrl Pts',(-16.1759149870658,19.3100003363692,
5.42829966676326));
#131931=CARTESIAN_POINT('Ctrl Pts',(-16.1726627757638,19.2259659452183,
5.43247523095494));
#131932=CARTESIAN_POINT('Ctrl Pts',(-16.1735580857934,19.1418316894465,
5.43665079514662));
#131933=CARTESIAN_POINT('Ctrl Pts',(-16.1785740672325,19.0580349643242,
5.4408263593383));
#131934=CARTESIAN_POINT('Ctrl Pts',(-16.1838433939698,18.9700058658238,
5.44521282135084));
#131935=CARTESIAN_POINT('Ctrl Pts',(-16.1936605371381,18.8823498716686,
5.44959928336338));
#131936=CARTESIAN_POINT('Ctrl Pts',(-16.2079333028748,18.7955640342065,
5.45398574537592));
#131937=CARTESIAN_POINT('Ctrl Pts',(-16.2222060686114,18.7087781967444,
5.45837220738847));
#131938=CARTESIAN_POINT('Ctrl Pts',(-16.2409342590202,18.6228630666792,
5.46275866940101));
#131939=CARTESIAN_POINT('Ctrl Pts',(-16.2639654295305,18.5382970784325,
5.46714513141355));
#131940=CARTESIAN_POINT('Ctrl Pts',(-16.2859330287302,18.4576363176213,
5.47132902816135));
#131941=CARTESIAN_POINT('Ctrl Pts',(-16.3118967078484,18.3779026599609,
5.47551292490916));
#131942=CARTESIAN_POINT('Ctrl Pts',(-16.3417612031297,18.2995212351631,
5.47969682165697));
#131943=CARTESIAN_POINT('Ctrl Pts',(-16.3715858706168,18.2212443411543,
5.48387513868956));
#131944=CARTESIAN_POINT('Ctrl Pts',(-16.4053008633433,18.1443165254295,
5.48805345572216));
#131945=CARTESIAN_POINT('Ctrl Pts',(-16.4427606710955,18.0691495992551,
5.49223177275476));
#131946=CARTESIAN_POINT('Ctrl Pts',(-16.480181764331,17.9940603577085,5.4964057715184));
#131947=CARTESIAN_POINT('Ctrl Pts',(-16.521339781578,17.9207288006143,5.50057977028204));
#131948=CARTESIAN_POINT('Ctrl Pts',(-16.5660409635037,17.8495472406015,
5.50475376904568));
#131949=CARTESIAN_POINT('Ctrl Pts',(-16.6107117825475,17.7784140300327,
5.50892493265764));
#131950=CARTESIAN_POINT('Ctrl Pts',(-16.6589207423336,17.7094283045759,
5.5130960962696));
#131951=CARTESIAN_POINT('Ctrl Pts',(-16.7104285669956,17.6429570619627,
5.51726725988155));
#131952=CARTESIAN_POINT('Ctrl Pts',(-16.7619153763033,17.5765129398254,
5.52143672164565));
#131953=CARTESIAN_POINT('Ctrl Pts',(-16.8166980925828,17.5125816237491,
5.52560618340975));
#131954=CARTESIAN_POINT('Ctrl Pts',(-16.8744954343627,17.4514992837814,
5.52977564517385));
#131955=CARTESIAN_POINT('Ctrl Pts',(-16.93230250686,17.3904066600364,5.53394580890543));
#131956=CARTESIAN_POINT('Ctrl Pts',(-16.9931249059284,17.332164308163,5.538115972637));
#131957=CARTESIAN_POINT('Ctrl Pts',(-17.0566432414669,17.2770728285162,
5.54228613636858));
#131958=CARTESIAN_POINT('Ctrl Pts',(-17.0949618222409,17.2438379004453,
5.54480186280308));
#131959=CARTESIAN_POINT('Ctrl Pts',(-17.1342608277126,17.2117489616349,
5.54731758923758));
#131960=CARTESIAN_POINT('Ctrl Pts',(-17.174464231106,17.180864983421,5.54983331567207));
#131961=CARTESIAN_POINT('Ctrl Pts',(-17.1762220704533,17.183189381701,4.74997346579241));
#131962=CARTESIAN_POINT('Ctrl Pts',(-17.6117180491967,16.8534335803771,
4.77707100986373));
#131963=CARTESIAN_POINT('Ctrl Pts',(-18.9946006232268,16.3463963590632,
4.84656048949553));
#131964=CARTESIAN_POINT('Ctrl Pts',(-20.9008595855074,17.3473638996065,
4.94099937082188));
#131965=CARTESIAN_POINT('Ctrl Pts',(-21.288210327615,18.7088774717577,5.00834070807693));
#131966=CARTESIAN_POINT('Ctrl Pts',(-21.2903253369841,19.2121940792196,
5.0332901097715));
#131967=CARTESIAN_POINT('',(-21.2942631007509,19.2101644346482,4.96670989022851));
#131968=CARTESIAN_POINT('Ctrl Pts',(-17.1735447493682,17.1796894255362,
4.68319930527188));
#131969=CARTESIAN_POINT('Ctrl Pts',(-17.2909884427537,17.0876168801257,
4.69063448591894));
#131970=CARTESIAN_POINT('Ctrl Pts',(-18.1310916530698,16.5418820156488,
4.74046160212649));
#131971=CARTESIAN_POINT('Ctrl Pts',(-20.2331956221585,16.5812273615557,
4.8326806538945));
#131972=CARTESIAN_POINT('Ctrl Pts',(-21.2762381336493,18.2701494254144,
4.91974900156631));
#131973=CARTESIAN_POINT('Ctrl Pts',(-21.2980949765117,19.1644257538227,
4.96442541367765));
#131974=CARTESIAN_POINT('Ctrl Pts',(-21.2979002687903,19.210163247625,4.96670989022851));
#131975=CARTESIAN_POINT('Ctrl Pts',(-21.2939998636668,19.210164520558,4.96670989022851));
#131976=CARTESIAN_POINT('Ctrl Pts',(-21.2940269378475,19.2931227545131,
4.97085977152528));
#131977=CARTESIAN_POINT('Ctrl Pts',(-21.2900172964774,19.3762448671897,
4.97500965282206));
#131978=CARTESIAN_POINT('Ctrl Pts',(-21.2819493183893,19.4591013319584,
4.97915953411883));
#131979=CARTESIAN_POINT('Ctrl Pts',(-21.273892503302,19.5418431550195,4.98330367356457));
#131980=CARTESIAN_POINT('Ctrl Pts',(-21.2617885455564,19.6243195978693,
4.9874478130103));
#131981=CARTESIAN_POINT('Ctrl Pts',(-21.2456678375727,19.7061006702713,
4.99159195245604));
#131982=CARTESIAN_POINT('Ctrl Pts',(-21.2295645603718,19.787793315532,4.99573161098226));
#131983=CARTESIAN_POINT('Ctrl Pts',(-21.2094532518121,19.8687916269892,
4.99987126950847));
#131984=CARTESIAN_POINT('Ctrl Pts',(-21.185415992005,19.9486717658566,5.00401092803468));
#131985=CARTESIAN_POINT('Ctrl Pts',(-21.1613926712712,20.0285055826756,
5.00814818599593));
#131986=CARTESIAN_POINT('Ctrl Pts',(-21.1334480518402,20.1072220663071,
5.01228544395718));
#131987=CARTESIAN_POINT('Ctrl Pts',(-21.1017147974227,20.1844097996556,
5.01642270191842));
#131988=CARTESIAN_POINT('Ctrl Pts',(-21.0699900384709,20.2615768686961,
5.02055885227398));
#131989=CARTESIAN_POINT('Ctrl Pts',(-21.0344788364884,20.3372155671953,
5.02469500262954));
#131990=CARTESIAN_POINT('Ctrl Pts',(-20.9953624823965,20.4109332161455,
5.02883115298509));
#131991=CARTESIAN_POINT('Ctrl Pts',(-20.9562443890678,20.4846541428155,
5.03296748724698));
#131992=CARTESIAN_POINT('Ctrl Pts',(-20.9135210465748,20.5564534375451,
5.03710382150886));
#131993=CARTESIAN_POINT('Ctrl Pts',(-20.8674196102005,20.6259631680054,
5.04124015577075));
#131994=CARTESIAN_POINT('Ctrl Pts',(-20.8212714994521,20.6955432720466,
5.04538067777227));
#131995=CARTESIAN_POINT('Ctrl Pts',(-20.7717387262307,20.7628287929985,
5.0495211997738));
#131996=CARTESIAN_POINT('Ctrl Pts',(-20.7190913321275,20.8274814886389,
5.05366172177532));
#131997=CARTESIAN_POINT('Ctrl Pts',(-20.6664157771977,20.8921687666814,
5.05780445852126));
#131998=CARTESIAN_POINT('Ctrl Pts',(-20.6106225991445,20.9542200685987,
5.0619471952672));
#131999=CARTESIAN_POINT('Ctrl Pts',(-20.5520199344765,21.0133327988598,
5.06608993201314));
#132000=CARTESIAN_POINT('Ctrl Pts',(-20.4933173061603,21.0725463628324,
5.07023973538449));
#132001=CARTESIAN_POINT('Ctrl Pts',(-20.4317959684764,21.1288110311776,
5.07438953875584));
#132002=CARTESIAN_POINT('Ctrl Pts',(-20.3677981562815,21.181863664623,5.07853934212718));
#132003=CARTESIAN_POINT('Ctrl Pts',(-20.3241391698325,21.218055905033,5.08137031717058));
#132004=CARTESIAN_POINT('Ctrl Pts',(-20.2793283343472,21.252754156268,5.08420129221397));
#132005=CARTESIAN_POINT('Ctrl Pts',(-20.2334815623284,21.2858867545572,
5.08703226725737));
#132006=CARTESIAN_POINT('Ctrl Pts',(-20.165712692572,21.3348620398235,5.09121690165042));
#132007=CARTESIAN_POINT('Ctrl Pts',(-20.0954157767524,21.38060482739,5.09540153604347));
#132008=CARTESIAN_POINT('Ctrl Pts',(-20.0229321512534,21.4228440065848,
5.09958617043652));
#132009=CARTESIAN_POINT('Ctrl Pts',(-19.9505516972236,21.4650230635362,
5.10376484852047));
#132010=CARTESIAN_POINT('Ctrl Pts',(-19.8759911100092,21.5037081881331,
5.10794352660441));
#132011=CARTESIAN_POINT('Ctrl Pts',(-19.7996223782742,21.5386702831203,
5.11212220468836));
#132012=CARTESIAN_POINT('Ctrl Pts',(-19.7218847919081,21.5742590485333,
5.1163757825738));
#132013=CARTESIAN_POINT('Ctrl Pts',(-19.6422739922293,21.6059897185086,
5.12062936045924));
#132014=CARTESIAN_POINT('Ctrl Pts',(-19.5612105522306,21.6336685085414,
5.12488293834467));
#132015=CARTESIAN_POINT('Ctrl Pts',(-19.4817186851986,21.6608106912187,
5.12905405232262));
#132016=CARTESIAN_POINT('Ctrl Pts',(-19.4008304551545,21.684056543659,5.13322516630057));
#132017=CARTESIAN_POINT('Ctrl Pts',(-19.3189628776792,21.7032717411505,
5.13739628027853));
#132018=CARTESIAN_POINT('Ctrl Pts',(-19.2371227716601,21.7224804907969,
5.1415659945989));
#132019=CARTESIAN_POINT('Ctrl Pts',(-19.1543044183624,21.7376611666004,
5.14573570891928));
#132020=CARTESIAN_POINT('Ctrl Pts',(-19.0709381209924,21.7487298324727,
5.14990542323965));
#132021=CARTESIAN_POINT('Ctrl Pts',(-18.9875747901528,21.7597981044745,
5.15407498918371));
#132022=CARTESIAN_POINT('Ctrl Pts',(-18.9036640101513,21.7667545977696,
5.15824455512777));
#132023=CARTESIAN_POINT('Ctrl Pts',(-18.8196429975834,21.7695670358552,
5.16241412107182));
#132024=CARTESIAN_POINT('Ctrl Pts',(-18.732667909865,21.7724783557944,5.16673028381074));
#132025=CARTESIAN_POINT('Ctrl Pts',(-18.6455752209298,21.7709487709587,
5.17104644654966));
#132026=CARTESIAN_POINT('Ctrl Pts',(-18.5588499153528,21.7650012623035,
5.17536260928857));
#132027=CARTESIAN_POINT('Ctrl Pts',(-18.4749496774831,21.7592474931172,
5.17953817348025));
#132028=CARTESIAN_POINT('Ctrl Pts',(-18.3913937177399,21.7493593099809,
5.18371373767193));
#132029=CARTESIAN_POINT('Ctrl Pts',(-18.3086140512028,21.7354101874628,
5.18788930186361));
#132030=CARTESIAN_POINT('Ctrl Pts',(-18.2216533804991,21.7207565279272,
5.19227576387614));
#132031=CARTESIAN_POINT('Ctrl Pts',(-18.135550055063,21.7016210383819,5.19666222588868));
#132032=CARTESIAN_POINT('Ctrl Pts',(-18.0507884164761,21.6781485427794,
5.20104868790121));
#132033=CARTESIAN_POINT('Ctrl Pts',(-17.9660267778892,21.654676047177,5.20543514991374));
#132034=CARTESIAN_POINT('Ctrl Pts',(-17.8826073525322,21.6268668011753,
5.20982161192628));
#132035=CARTESIAN_POINT('Ctrl Pts',(-17.8009895271363,21.5949235427183,
5.21420807393881));
#132036=CARTESIAN_POINT('Ctrl Pts',(-17.7231270588735,21.5644500409342,
5.21839270833185));
#132037=CARTESIAN_POINT('Ctrl Pts',(-17.6466142262365,21.5301011627873,
5.2225773427249));
#132038=CARTESIAN_POINT('Ctrl Pts',(-17.5718637493069,21.4920171710938,
5.22676197711794));
#132039=CARTESIAN_POINT('Ctrl Pts',(-17.497219670429,21.4539873872488,5.23094065520188));
#132040=CARTESIAN_POINT('Ctrl Pts',(-17.4243333709912,21.4122332570933,
5.23511933328581));
#132041=CARTESIAN_POINT('Ctrl Pts',(-17.3535988359381,21.366943558226,5.23929801136975));
#132042=CARTESIAN_POINT('Ctrl Pts',(-17.2815964351799,21.3208420740556,
5.24355158925519));
#132043=CARTESIAN_POINT('Ctrl Pts',(-17.2118241472901,21.2710772000459,
5.24780516714062));
#132044=CARTESIAN_POINT('Ctrl Pts',(-17.1446725625544,21.2178976796495,
5.25205874502606));
#132045=CARTESIAN_POINT('Ctrl Pts',(-17.0788228423243,21.1657491480273,
5.25622985900401));
#132046=CARTESIAN_POINT('Ctrl Pts',(-17.0154934944018,21.1103174864337,
5.26040097298197));
#132047=CARTESIAN_POINT('Ctrl Pts',(-16.9550231872364,21.051880631559,5.26457208695992));
#132048=CARTESIAN_POINT('Ctrl Pts',(-16.8945731714665,20.9934633857354,
5.26874180128029));
#132049=CARTESIAN_POINT('Ctrl Pts',(-16.836980621644,20.9320432687888,5.27291151560067));
#132050=CARTESIAN_POINT('Ctrl Pts',(-16.7825490297002,20.8679366646061,
5.27708122992104));
#132051=CARTESIAN_POINT('Ctrl Pts',(-16.7281193746661,20.8038323416116,
5.28125079586508));
#132052=CARTESIAN_POINT('Ctrl Pts',(-16.6768507509731,20.7370420726798,
5.28542036180911));
#132053=CARTESIAN_POINT('Ctrl Pts',(-16.6290069551027,20.6679160171177,
5.28958992775315));
#132054=CARTESIAN_POINT('Ctrl Pts',(-16.5794810303911,20.596359574718,5.29390609049207));
#132055=CARTESIAN_POINT('Ctrl Pts',(-16.5336255484986,20.5223004707795,
5.298222253231));
#132056=CARTESIAN_POINT('Ctrl Pts',(-16.4916836990305,20.4461589397347,
5.30253841596993));
#132057=CARTESIAN_POINT('Ctrl Pts',(-16.4511081008974,20.3724977110551,
5.30671398016161));
#132058=CARTESIAN_POINT('Ctrl Pts',(-16.4141952418313,20.296888085941,5.31088954435328));
#132059=CARTESIAN_POINT('Ctrl Pts',(-16.3811171829165,20.2197330910965,
5.31506510854496));
#132060=CARTESIAN_POINT('Ctrl Pts',(-16.3463684298815,20.138681180881,5.31945157055751));
#132061=CARTESIAN_POINT('Ctrl Pts',(-16.3158522513523,20.0559242327781,
5.32383803257006));
#132062=CARTESIAN_POINT('Ctrl Pts',(-16.2897090382154,19.9719478918678,
5.3282244945826));
#132063=CARTESIAN_POINT('Ctrl Pts',(-16.2635658250786,19.8879715509576,
5.33261095659515));
#132064=CARTESIAN_POINT('Ctrl Pts',(-16.2417956472861,19.8027763982257,
5.3369974186077));
#132065=CARTESIAN_POINT('Ctrl Pts',(-16.2244766916358,19.7168584434174,
5.34138388062024));
#132066=CARTESIAN_POINT('Ctrl Pts',(-16.2079546068078,19.6348937010709,
5.3455685150133));
#132067=CARTESIAN_POINT('Ctrl Pts',(-16.1954216323758,19.5519661209785,
5.34975314940634));
#132068=CARTESIAN_POINT('Ctrl Pts',(-16.1869832270606,19.4684986570164,
5.3539377837994));
#132069=CARTESIAN_POINT('Ctrl Pts',(-16.1785568327709,19.3851499986582,
5.35811646188333));
#132070=CARTESIAN_POINT('Ctrl Pts',(-16.1742134770096,19.3012634366144,
5.36229513996727));
#132071=CARTESIAN_POINT('Ctrl Pts',(-16.174007684269,19.2172724316078,5.36647381805121));
#132072=CARTESIAN_POINT('Ctrl Pts',(-16.1737982028414,19.1317759481995,
5.37072739593665));
#132073=CARTESIAN_POINT('Ctrl Pts',(-16.177876170323,19.0461717133521,5.37498097382208));
#132074=CARTESIAN_POINT('Ctrl Pts',(-16.1862438519479,18.9609227917969,
5.37923455170752));
#132075=CARTESIAN_POINT('Ctrl Pts',(-16.1944493097363,18.8773265869357,
5.38340566568547));
#132076=CARTESIAN_POINT('Ctrl Pts',(-16.2067795899915,18.7940725203434,
5.38757677966342));
#132077=CARTESIAN_POINT('Ctrl Pts',(-16.2231843067498,18.7115958004499,
5.39174789364137));
#132078=CARTESIAN_POINT('Ctrl Pts',(-16.2395835187469,18.6291467564163,
5.39591760796174));
#132079=CARTESIAN_POINT('Ctrl Pts',(-16.2600543622649,18.5474749918557,
5.40008732228212));
#132080=CARTESIAN_POINT('Ctrl Pts',(-16.2844950829501,18.467006948051,5.40425703660249));
#132081=CARTESIAN_POINT('Ctrl Pts',(-16.3089349339296,18.3865417676445,
5.40842660254654));
#132082=CARTESIAN_POINT('Ctrl Pts',(-16.3373442466934,18.307280662759,5.41259616849058));
#132083=CARTESIAN_POINT('Ctrl Pts',(-16.3695713807106,18.2296349790802,
5.41676573443463));
#132084=CARTESIAN_POINT('Ctrl Pts',(-16.4029315810032,18.1492593689496,
5.42108189717355));
#132085=CARTESIAN_POINT('Ctrl Pts',(-16.4403828646778,18.0706153771455,
5.42539805991247));
#132086=CARTESIAN_POINT('Ctrl Pts',(-16.4817035150009,17.9941349525684,
5.42971422265139));
#132087=CARTESIAN_POINT('Ctrl Pts',(-16.5216781494859,17.9201458697775,
5.43388978684307));
#132088=CARTESIAN_POINT('Ctrl Pts',(-16.5652736482195,17.8481819408652,
5.43806535103475));
#132089=CARTESIAN_POINT('Ctrl Pts',(-16.6122442629255,17.7786059926852,
5.44224091522643));
#132090=CARTESIAN_POINT('Ctrl Pts',(-16.6615872517183,17.7055159287636,
5.44662737723897));
#132091=CARTESIAN_POINT('Ctrl Pts',(-16.714654919849,17.6350618855121,5.45101383925151));
#132092=CARTESIAN_POINT('Ctrl Pts',(-16.7711149075846,17.5676247799199,
5.45540030126405));
#132093=CARTESIAN_POINT('Ctrl Pts',(-16.8275748953203,17.5001876743276,
5.45978676327659));
#132094=CARTESIAN_POINT('Ctrl Pts',(-16.8874267520075,17.4357678796896,
5.46417322528913));
#132095=CARTESIAN_POINT('Ctrl Pts',(-16.9502957329765,17.3746996193972,
5.46855968730167));
#132096=CARTESIAN_POINT('Ctrl Pts',(-17.0102748276238,17.3164384720464,
5.47274451766097));
#132097=CARTESIAN_POINT('Ctrl Pts',(-17.0732230246168,17.2610106350511,
5.47692934802027));
#132098=CARTESIAN_POINT('Ctrl Pts',(-17.1388417266104,17.2087337632481,
5.48111417837957));
#132099=CARTESIAN_POINT('Ctrl Pts',(-17.1506304271778,17.1993419836248,
5.48186600233421));
#132100=CARTESIAN_POINT('Ctrl Pts',(-17.1625052169379,17.1900518159241,
5.48261782628886));
#132101=CARTESIAN_POINT('Ctrl Pts',(-17.174464231106,17.180864983421,5.4833696502435));
#132102=CARTESIAN_POINT('Origin',(-18.734,19.211,-1.76670989022852));
#132103=CARTESIAN_POINT('',(-17.1721129728022,17.177834880393,6.34984102388608));
#132104=CARTESIAN_POINT('',(-17.174464231106,17.180864983421,6.28334279855885));
#132105=CARTESIAN_POINT('',(-17.174464231106,17.180864983421,-1.76670989022852));
#132106=CARTESIAN_POINT('',(-21.2939994369002,19.2126979607666,5.8332901097715));
#132107=CARTESIAN_POINT('Ctrl Pts',(-21.2967674808324,19.2126997967162,
5.8332901097715));
#132108=CARTESIAN_POINT('Ctrl Pts',(-21.2975540827487,19.3154768305114,
5.83841759033361));
#132109=CARTESIAN_POINT('Ctrl Pts',(-21.2452321516418,20.267165082075,5.8859370064562));
#132110=CARTESIAN_POINT('Ctrl Pts',(-20.0538051929683,21.9352257637231,
5.97584835813928));
#132111=CARTESIAN_POINT('Ctrl Pts',(-17.1577427696511,21.7953190404615,
6.10302416482071));
#132112=CARTESIAN_POINT('Ctrl Pts',(-15.7364333538251,19.3340467515488,
6.22768838673632));
#132113=CARTESIAN_POINT('Ctrl Pts',(-16.5413043832607,17.6674200121866,
6.30996067309144));
#132114=CARTESIAN_POINT('Ctrl Pts',(-17.1721129728022,17.177834880393,6.34984102388608));
#132115=CARTESIAN_POINT('Ctrl Pts',(-17.174464231106,17.180864983421,5.54983331567207));
#132116=CARTESIAN_POINT('Ctrl Pts',(-17.2411774753928,17.1296163276052,
5.55400789438973));
#132117=CARTESIAN_POINT('Ctrl Pts',(-17.3103823939862,17.0816880702098,
5.55818247310739));
#132118=CARTESIAN_POINT('Ctrl Pts',(-17.3817083728383,17.0373147985257,
5.56235705182505));
#132119=CARTESIAN_POINT('Ctrl Pts',(-17.4530770005447,16.992914994164,5.56653412670193));
#132120=CARTESIAN_POINT('Ctrl Pts',(-17.5265688111888,16.9520746303608,
5.57071120157881));
#132121=CARTESIAN_POINT('Ctrl Pts',(-17.6017888279468,16.9149821730052,
5.57488827645568));
#132122=CARTESIAN_POINT('Ctrl Pts',(-17.6771347920593,16.8778276085527,
5.57907234536889));
#132123=CARTESIAN_POINT('Ctrl Pts',(-17.7542143174781,16.8444336617759,
5.5832564142821));
#132124=CARTESIAN_POINT('Ctrl Pts',(-17.8326130703151,16.8149404007844,
5.58744048319531));
#132125=CARTESIAN_POINT('Ctrl Pts',(-17.8755871141844,16.7987737572368,
5.58973396816186));
#132126=CARTESIAN_POINT('Ctrl Pts',(-17.9189572740205,16.7837782551377,
5.59202745312842));
#132127=CARTESIAN_POINT('Ctrl Pts',(-17.9626538344085,16.7699704850561,
5.59432093809497));
#132128=CARTESIAN_POINT('Ctrl Pts',(-18.0423814681728,16.7447771786174,
5.59850557248802));
#132129=CARTESIAN_POINT('Ctrl Pts',(-18.1234930456338,16.7234471296282,
5.60269020688107));
#132130=CARTESIAN_POINT('Ctrl Pts',(-18.2055793173493,16.7061304261206,
5.60687484127411));
#132131=CARTESIAN_POINT('Ctrl Pts',(-18.2875487494172,16.688838370797,5.61105351935805));
#132132=CARTESIAN_POINT('Ctrl Pts',(-18.3704896737369,16.6755484082766,
5.61523219744199));
#132133=CARTESIAN_POINT('Ctrl Pts',(-18.4539769469564,16.6663611081798,
5.61941087552594));
#132134=CARTESIAN_POINT('Ctrl Pts',(-18.5389606695472,16.6570091323315,
5.62366445341137));
#132135=CARTESIAN_POINT('Ctrl Pts',(-18.6245100605659,16.6519084913031,
5.62791803129681));
#132136=CARTESIAN_POINT('Ctrl Pts',(-18.7101649534091,16.6511109612809,
5.63217160918225));
#132137=CARTESIAN_POINT('Ctrl Pts',(-18.7941592590127,16.6503288929346,
5.6363427231602));
#132138=CARTESIAN_POINT('Ctrl Pts',(-18.87825453103,16.6536845805936,5.64051383713815));
#132139=CARTESIAN_POINT('Ctrl Pts',(-18.9620126684401,16.6611744720411,
5.6446849511161));
#132140=CARTESIAN_POINT('Ctrl Pts',(-19.0457426999984,16.6686618501832,
5.64885466543648));
#132141=CARTESIAN_POINT('Ctrl Pts',(-19.1291353638019,16.6802806360297,
5.65302437975685));
#132142=CARTESIAN_POINT('Ctrl Pts',(-19.2117557819362,16.6959752659613,
5.65719409407723));
#132143=CARTESIAN_POINT('Ctrl Pts',(-19.2943732600815,16.7116693374106,
5.66136366002127));
#132144=CARTESIAN_POINT('Ctrl Pts',(-19.3762180954027,16.7314388778862,
5.66553322596532));
#132145=CARTESIAN_POINT('Ctrl Pts',(-19.4568650837658,16.7551771092621,
5.66970279190936));
#132146=CARTESIAN_POINT('Ctrl Pts',(-19.5403475207509,16.7797499475689,
5.67401895464828));
#132147=CARTESIAN_POINT('Ctrl Pts',(-19.6225458049916,16.808575598709,5.6783351173872));
#132148=CARTESIAN_POINT('Ctrl Pts',(-19.7030067527824,16.8414798137466,
5.68265128012612));
#132149=CARTESIAN_POINT('Ctrl Pts',(-19.7808466936618,16.8733121774403,
5.6868268443178));
#132150=CARTESIAN_POINT('Ctrl Pts',(-19.8570603406959,16.9089612248342,
5.69100240850948));
#132151=CARTESIAN_POINT('Ctrl Pts',(-19.9312606656525,16.9482214208011,
5.69517797270116));
#132152=CARTESIAN_POINT('Ctrl Pts',(-20.0092086726281,16.9894645559341,
5.6995644347137));
#132153=CARTESIAN_POINT('Ctrl Pts',(-20.0849341253746,17.0346929255447,
5.70395089672625));
#132154=CARTESIAN_POINT('Ctrl Pts',(-20.1580227463385,17.0836168145089,
5.70833735873879));
#132155=CARTESIAN_POINT('Ctrl Pts',(-20.2311113673024,17.132540703473,5.71272382075133));
#132156=CARTESIAN_POINT('Ctrl Pts',(-20.3015627371329,17.1851597036451,
5.71711028276387));
#132157=CARTESIAN_POINT('Ctrl Pts',(-20.3690044710744,17.2411369642621,
5.72149674477641));
#132158=CARTESIAN_POINT('Ctrl Pts',(-20.4324580482224,17.2938040179914,
5.72562381401755));
#132159=CARTESIAN_POINT('Ctrl Pts',(-20.4934979978141,17.3496514870446,
5.72975088325869));
#132160=CARTESIAN_POINT('Ctrl Pts',(-20.5517814829092,17.4084267059583,
5.73387795249984));
#132161=CARTESIAN_POINT('Ctrl Pts',(-20.6102782700972,17.4674170265802,
5.73802012571949));
#132162=CARTESIAN_POINT('Ctrl Pts',(-20.6659979620834,17.5293563204315,
5.74216229893914));
#132163=CARTESIAN_POINT('Ctrl Pts',(-20.7186255971237,17.5939467419898,
5.74630447215879));
#132164=CARTESIAN_POINT('Ctrl Pts',(-20.7709257203662,17.658135205051,5.75042086784547));
#132165=CARTESIAN_POINT('Ctrl Pts',(-20.8201718394843,17.7249415391099,
5.75453726353214));
#132166=CARTESIAN_POINT('Ctrl Pts',(-20.8660914253506,17.7940362905331,
5.75865365921881));
#132167=CARTESIAN_POINT('Ctrl Pts',(-20.9119829684087,17.8630888462171,
5.76276754104799));
#132168=CARTESIAN_POINT('Ctrl Pts',(-20.9545517475123,17.9344266527042,
5.76688142287717));
#132169=CARTESIAN_POINT('Ctrl Pts',(-20.9935669693931,18.0076891046668,
5.77099530470634));
#132170=CARTESIAN_POINT('Ctrl Pts',(-21.0325708263853,18.0809302157382,
5.77510798818763));
#132171=CARTESIAN_POINT('Ctrl Pts',(-21.0680229592547,18.1560944409463,
5.77922067166891));
#132172=CARTESIAN_POINT('Ctrl Pts',(-21.0997379788824,18.2327956168196,
5.7833333551502));
#132173=CARTESIAN_POINT('Ctrl Pts',(-21.1318415000295,18.3104363640289,
5.78749641803531));
#132174=CARTESIAN_POINT('Ctrl Pts',(-21.1601155043873,18.3896515290328,
5.79165948092042));
#132175=CARTESIAN_POINT('Ctrl Pts',(-21.1844181339266,18.4700202641611,
5.79582254380553));
#132176=CARTESIAN_POINT('Ctrl Pts',(-21.2084475698835,18.5494855487958,
5.79993880837768));
#132177=CARTESIAN_POINT('Ctrl Pts',(-21.2285944016388,18.6300781193823,
5.80405507294983));
#132178=CARTESIAN_POINT('Ctrl Pts',(-21.2447724368935,18.7113783730305,
5.80817133752198));
#132179=CARTESIAN_POINT('Ctrl Pts',(-21.2612263672264,18.7940650953984,
5.81235779956356));
#132180=CARTESIAN_POINT('Ctrl Pts',(-21.2735747867911,18.8774833595966,
5.81654426160515));
#132181=CARTESIAN_POINT('Ctrl Pts',(-21.281781944964,18.9611857471732,5.82073072364674));
#132182=CARTESIAN_POINT('Ctrl Pts',(-21.2899891031369,19.0448881347499,
5.82491718568833));
#132183=CARTESIAN_POINT('Ctrl Pts',(-21.2940550344004,19.1288741338655,
5.82910364772991));
#132184=CARTESIAN_POINT('Ctrl Pts',(-21.2939994369002,19.2126979607666,
5.8332901097715));
#132185=CARTESIAN_POINT('',(-21.2939992944986,19.2090994299067,5.76670989019962));
#132186=CARTESIAN_POINT('Ctrl Pts',(-17.174464231106,17.180864983421,5.4833696502435));
#132187=CARTESIAN_POINT('Ctrl Pts',(-17.2409183890944,17.1298153559192,
5.48754740496134));
#132188=CARTESIAN_POINT('Ctrl Pts',(-17.3099760635813,17.0819596693814,
5.49172515967919));
#132189=CARTESIAN_POINT('Ctrl Pts',(-17.381296247198,17.037571244058,5.49590291439703));
#132190=CARTESIAN_POINT('Ctrl Pts',(-17.4525396221523,16.9932306230924,
5.50007616985905));
#132191=CARTESIAN_POINT('Ctrl Pts',(-17.5260402745971,16.9523500835238,
5.50424942532106));
#132192=CARTESIAN_POINT('Ctrl Pts',(-17.6014266254566,16.9151608176365,
5.50842268078308));
#132193=CARTESIAN_POINT('Ctrl Pts',(-17.6767687012082,16.8779933933524,
5.51259348525319));
#132194=CARTESIAN_POINT('Ctrl Pts',(-17.7539938650333,16.8445131416642,
5.5167642897233));
#132195=CARTESIAN_POINT('Ctrl Pts',(-17.8327052167042,16.8149057377466,
5.5209350941934));
#132196=CARTESIAN_POINT('Ctrl Pts',(-17.911393952278,16.785306840911,5.52510470026815));
#132197=CARTESIAN_POINT('Ctrl Pts',(-17.9915675972202,16.7595787434778,
5.52927430634291));
#132198=CARTESIAN_POINT('Ctrl Pts',(-18.0728097832131,16.7378587793607,
5.53344391241766));
#132199=CARTESIAN_POINT('Ctrl Pts',(-18.1540529965122,16.716138540595,5.53761357121702));
#132200=CARTESIAN_POINT('Ctrl Pts',(-18.2363643329242,16.698426653361,5.54178323001638));
#132201=CARTESIAN_POINT('Ctrl Pts',(-18.3193141232468,16.6848100578893,
5.54595288881574));
#132202=CARTESIAN_POINT('Ctrl Pts',(-18.4023475185942,16.6711797382623,
5.55012675021075));
#132203=CARTESIAN_POINT('Ctrl Pts',(-18.4860201982849,16.661653030515,5.55430061160575));
#132204=CARTESIAN_POINT('Ctrl Pts',(-18.5698946588579,16.6562652902877,
5.55847447300076));
#132205=CARTESIAN_POINT('Ctrl Pts',(-18.6538097229503,16.6508749418623,
5.56265035495674));
#132206=CARTESIAN_POINT('Ctrl Pts',(-18.7379263019653,16.6496275592858,
5.56682623691272));
#132207=CARTESIAN_POINT('Ctrl Pts',(-18.8218066258234,16.6525063032203,
5.57100211886871));
#132208=CARTESIAN_POINT('Ctrl Pts',(-18.9058385141806,16.6553902487964,
5.57518554628264));
#132209=CARTESIAN_POINT('Ctrl Pts',(-18.9896328347449,16.6624151806863,
5.57936897369658));
#132210=CARTESIAN_POINT('Ctrl Pts',(-19.0727567278495,16.6735122898156,
5.58355240111052));
#132211=CARTESIAN_POINT('Ctrl Pts',(-19.1534486270523,16.6842847257286,
5.58761343206805));
#132212=CARTESIAN_POINT('Ctrl Pts',(-19.2335084226815,16.698894184328,5.59167446302558));
#132213=CARTESIAN_POINT('Ctrl Pts',(-19.3125527301388,16.7172324209243,
5.59573549398311));
#132214=CARTESIAN_POINT('Ctrl Pts',(-19.3940028670669,16.7361288086572,
5.59992012837615));
#132215=CARTESIAN_POINT('Ctrl Pts',(-19.4746778298125,16.7590549809083,
5.60410476276919));
#132216=CARTESIAN_POINT('Ctrl Pts',(-19.5541489559097,16.7859318174286,
5.60828939716224));
#132217=CARTESIAN_POINT('Ctrl Pts',(-19.6335069646957,16.8127703980989,
5.61246807524619));
#132218=CARTESIAN_POINT('Ctrl Pts',(-19.7116641083501,16.8435483273113,
5.61664675333013));
#132219=CARTESIAN_POINT('Ctrl Pts',(-19.7882032486925,16.8781357711075,
5.62082543141408));
#132220=CARTESIAN_POINT('Ctrl Pts',(-19.8661142981178,16.9133431699762,
5.62507900929951));
#132221=CARTESIAN_POINT('Ctrl Pts',(-19.9423482986085,16.9524978888715,
5.62933258718495));
#132222=CARTESIAN_POINT('Ctrl Pts',(-20.0164828014234,16.995410267208,5.63358616507039));
#132223=CARTESIAN_POINT('Ctrl Pts',(-20.0891800622395,17.0374907053539,
5.63775727904834));
#132224=CARTESIAN_POINT('Ctrl Pts',(-20.15985808817,17.0831841629369,5.64192839302629));
#132225=CARTESIAN_POINT('Ctrl Pts',(-20.2281415862035,17.1322645862503,
5.64609950700424));
#132226=CARTESIAN_POINT('Ctrl Pts',(-20.2964021710499,17.1813285401536,
5.65026922132462));
#132227=CARTESIAN_POINT('Ctrl Pts',(-20.3622694505382,17.2337769343483,
5.65443893564499));
#132228=CARTESIAN_POINT('Ctrl Pts',(-20.4253973801086,17.289340586222,5.65860864996537));
#132229=CARTESIAN_POINT('Ctrl Pts',(-20.4885230633163,17.3449022609025,
5.66277821590942));
#132230=CARTESIAN_POINT('Ctrl Pts',(-20.5489092456572,17.4035786682711,
5.66694778185346));
#132231=CARTESIAN_POINT('Ctrl Pts',(-20.6062442778987,17.4650614661805,
5.67111734779751));
#132232=CARTESIAN_POINT('Ctrl Pts',(-20.6655951391432,17.5287059234172,
5.67543351053643));
#132233=CARTESIAN_POINT('Ctrl Pts',(-20.7216759416723,17.5953574026464,
5.67974967327535));
#132234=CARTESIAN_POINT('Ctrl Pts',(-20.7741852955296,17.6646352435778,
5.68406583601427));
#132235=CARTESIAN_POINT('Ctrl Pts',(-20.8249841627081,17.7316563661277,
5.68824140020596));
#132236=CARTESIAN_POINT('Ctrl Pts',(-20.8724404611874,17.8011349549806,
5.69241696439764));
#132237=CARTESIAN_POINT('Ctrl Pts',(-20.9163256700512,17.872697093392,5.69659252858933));
#132238=CARTESIAN_POINT('Ctrl Pts',(-20.9624274164875,17.9478736652916,
5.70097899060187));
#132239=CARTESIAN_POINT('Ctrl Pts',(-21.004587562026,18.0253492855826,5.7053654526144));
#132240=CARTESIAN_POINT('Ctrl Pts',(-21.0425969786767,18.1046637084301,
5.70975191462694));
#132241=CARTESIAN_POINT('Ctrl Pts',(-21.0806063953274,18.1839781312776,
5.71413837663948));
#132242=CARTESIAN_POINT('Ctrl Pts',(-21.1144649298774,18.2651307919131,
5.71852483865201));
#132243=CARTESIAN_POINT('Ctrl Pts',(-21.1440235064309,18.3476421955815,
5.72291130066455));
#132244=CARTESIAN_POINT('Ctrl Pts',(-21.1768030234133,18.4391447059575,
5.72777574688617));
#132245=CARTESIAN_POINT('Ctrl Pts',(-21.2043967060816,18.5325974942123,
5.73264019310779));
#132246=CARTESIAN_POINT('Ctrl Pts',(-21.2266026211952,18.6274486545204,
5.73750463932941));
#132247=CARTESIAN_POINT('Ctrl Pts',(-21.2488226674981,18.722360175309,5.74237218114112));
#132248=CARTESIAN_POINT('Ctrl Pts',(-21.2656479288592,18.818671733481,5.74723972295282));
#132249=CARTESIAN_POINT('Ctrl Pts',(-21.2769239065508,18.9158085274062,
5.75210726476452));
#132250=CARTESIAN_POINT('Ctrl Pts',(-21.2881998842425,19.0129453213313,
5.75697480657622));
#132251=CARTESIAN_POINT('Ctrl Pts',(-21.2939263955806,19.1109072194806,
5.76184234838792));
#132252=CARTESIAN_POINT('Ctrl Pts',(-21.2939992944986,19.2090994299067,
5.76670989019962));
#132253=CARTESIAN_POINT('Ctrl Pts',(-21.293999294499,19.2090994304895,5.76670989022851));
#132254=CARTESIAN_POINT('Ctrl Pts',(-21.2940618231948,19.2933233519321,
5.77088500205647));
#132255=CARTESIAN_POINT('Ctrl Pts',(-21.2899635861128,19.3775880720651,
5.77506011388443));
#132256=CARTESIAN_POINT('Ctrl Pts',(-21.2817191504239,19.4614538491683,
5.77923522571239));
#132257=CARTESIAN_POINT('Ctrl Pts',(-21.2734754980237,19.5453116583388,
5.78340994087068));
#132258=CARTESIAN_POINT('Ctrl Pts',(-21.2610864747303,19.6287701442277,
5.78758465602897));
#132259=CARTESIAN_POINT('Ctrl Pts',(-21.2446185572459,19.7113943045362,
5.79175937118726));
#132260=CARTESIAN_POINT('Ctrl Pts',(-21.2281473245847,19.794035098017,5.79593492676264));
#132261=CARTESIAN_POINT('Ctrl Pts',(-21.2075956572653,19.8758407835678,
5.80011048233803));
#132262=CARTESIAN_POINT('Ctrl Pts',(-21.1830809475491,19.956387491411,5.80428603791341));
#132263=CARTESIAN_POINT('Ctrl Pts',(-21.1585369190256,20.0370305305357,
5.80846658731945));
#132264=CARTESIAN_POINT('Ctrl Pts',(-21.1300205198885,20.1164111473511,
5.8126471367255));
#132265=CARTESIAN_POINT('Ctrl Pts',(-21.0976986239764,20.1941219736187,
5.81682768613154));
#132266=CARTESIAN_POINT('Ctrl Pts',(-21.0653559283573,20.2718828081662,
5.82101092579446));
#132267=CARTESIAN_POINT('Ctrl Pts',(-21.0292030575738,20.347971299817,5.82519416545738));
#132268=CARTESIAN_POINT('Ctrl Pts',(-20.9894534545796,20.4220035979404,
5.8293774051203));
#132269=CARTESIAN_POINT('Ctrl Pts',(-20.9496320042093,20.4961697093846,
5.83356820598562));
#132270=CARTESIAN_POINT('Ctrl Pts',(-20.906201076148,20.5682718138337,5.83775900685095));
#132271=CARTESIAN_POINT('Ctrl Pts',(-20.8594180036074,20.6379542073737,
5.84194980771627));
#132272=CARTESIAN_POINT('Ctrl Pts',(-20.8291383592868,20.6830550948788,
5.84466224092617));
#132273=CARTESIAN_POINT('Ctrl Pts',(-20.7974553185202,20.7271429654288,
5.84737467413607));
#132274=CARTESIAN_POINT('Ctrl Pts',(-20.7644472985012,20.770129169764,5.85008710734597));
#132275=CARTESIAN_POINT('Ctrl Pts',(-20.7135238341689,20.8364465811685,
5.85427174173902));
#132276=CARTESIAN_POINT('Ctrl Pts',(-20.6592531496868,20.9003899294851,
5.85845637613207));
#132277=CARTESIAN_POINT('Ctrl Pts',(-20.6018847443057,20.9616017771012,
5.86264101052512));
#132278=CARTESIAN_POINT('Ctrl Pts',(-20.5445979957491,21.0227264972285,
5.86681968860906));
#132279=CARTESIAN_POINT('Ctrl Pts',(-20.4842225962896,21.0811271065652,
5.87099836669299));
#132280=CARTESIAN_POINT('Ctrl Pts',(-20.4210494366145,21.1364776546142,
5.87517704477693));
#132281=CARTESIAN_POINT('Ctrl Pts',(-20.3567439434538,21.1928203214575,
5.87943062266237));
#132282=CARTESIAN_POINT('Ctrl Pts',(-20.28953969747,21.2460021244011,5.8836842005478));
#132283=CARTESIAN_POINT('Ctrl Pts',(-20.2197842460679,21.2957170489388,
5.88793777843324));
#132284=CARTESIAN_POINT('Ctrl Pts',(-20.1513811402078,21.3444681526537,
5.89210889241119));
#132285=CARTESIAN_POINT('Ctrl Pts',(-20.0805252582506,21.3898853234968,
5.89628000638914));
#132286=CARTESIAN_POINT('Ctrl Pts',(-20.0075777510546,21.4317205389284,
5.9004511203671));
#132287=CARTESIAN_POINT('Ctrl Pts',(-19.9346547220992,21.4735417161496,
5.90462083468747));
#132288=CARTESIAN_POINT('Ctrl Pts',(-19.8596418605524,21.5117830963986,
5.90879054900784));
#132289=CARTESIAN_POINT('Ctrl Pts',(-19.7829274662088,21.5462411375772,
5.91296026332822));
#132290=CARTESIAN_POINT('Ctrl Pts',(-19.7062158016926,21.5806979525908,
5.91712982927226));
#132291=CARTESIAN_POINT('Ctrl Pts',(-19.6278031447569,21.6113715084927,
5.92129939521631));
#132292=CARTESIAN_POINT('Ctrl Pts',(-19.5480992000004,21.6381057852015,
5.92546896116035));
#132293=CARTESIAN_POINT('Ctrl Pts',(-19.4655929628717,21.6657800060991,
5.92978512389927));
#132294=CARTESIAN_POINT('Ctrl Pts',(-19.3817034451245,21.6892326159302,
5.93410128663819));
#132295=CARTESIAN_POINT('Ctrl Pts',(-19.2969019322698,21.708346875115,5.93841744937711));
#132296=CARTESIAN_POINT('Ctrl Pts',(-19.2148628197768,21.7268384893174,
5.9425930135688));
#132297=CARTESIAN_POINT('Ctrl Pts',(-19.13197068837,21.7412700216398,5.94676857776048));
#132298=CARTESIAN_POINT('Ctrl Pts',(-19.0486605152119,21.751588270493,5.95094414195216));
#132299=CARTESIAN_POINT('Ctrl Pts',(-18.9611425432588,21.7624276695664,
5.9553306039647));
#132300=CARTESIAN_POINT('Ctrl Pts',(-18.8731637715283,21.7687272994046,
5.95971706597724));
#132301=CARTESIAN_POINT('Ctrl Pts',(-18.7852297301452,21.7704873538951,
5.96410352798978));
#132302=CARTESIAN_POINT('Ctrl Pts',(-18.6972956887621,21.7722474083857,
5.96848999000232));
#132303=CARTESIAN_POINT('Ctrl Pts',(-18.6094069552492,21.7694679818952,
5.97287645201486));
#132304=CARTESIAN_POINT('Ctrl Pts',(-18.5220617179689,21.7622119011579,
5.9772629140274));
#132305=CARTESIAN_POINT('Ctrl Pts',(-18.4387353645324,21.7552896834514,
5.98144754842046));
#132306=CARTESIAN_POINT('Ctrl Pts',(-18.3555934356672,21.7442679479862,
5.98563218281351));
#132307=CARTESIAN_POINT('Ctrl Pts',(-18.2730715290521,21.7291630099478,
5.98981681720656));
#132308=CARTESIAN_POINT('Ctrl Pts',(-18.1906670821569,21.7140795719191,
5.9939954952905));
#132309=CARTESIAN_POINT('Ctrl Pts',(-18.108881353184,21.6949245577665,5.99817417337445));
#132310=CARTESIAN_POINT('Ctrl Pts',(-18.0281458685303,21.6717661297017,
6.0023528514584));
#132311=CARTESIAN_POINT('Ctrl Pts',(-17.9459632583377,21.6481926034575,
6.00660642934383));
#132312=CARTESIAN_POINT('Ctrl Pts',(-17.8648693945433,21.6204707691484,
6.01086000722927));
#132313=CARTESIAN_POINT('Ctrl Pts',(-17.7853097077372,21.5887272192929,
6.0151135851147));
#132314=CARTESIAN_POINT('Ctrl Pts',(-17.7072924407079,21.5575990800938,
6.01928469909265));
#132315=CARTESIAN_POINT('Ctrl Pts',(-17.6307508424367,21.5226039497267,
6.0234558130706));
#132316=CARTESIAN_POINT('Ctrl Pts',(-17.5560889447388,21.4839112490138,
6.02762692704856));
#132317=CARTESIAN_POINT('Ctrl Pts',(-17.4814521005618,21.4452315320103,
6.03179664136893));
#132318=CARTESIAN_POINT('Ctrl Pts',(-17.4086941123782,21.4028569203158,
6.0359663556893));
#132319=CARTESIAN_POINT('Ctrl Pts',(-17.3381963061957,21.3570037391305,
6.04013607000967));
#132320=CARTESIAN_POINT('Ctrl Pts',(-17.2677010086276,21.3111521895981,
6.04430563595371));
#132321=CARTESIAN_POINT('Ctrl Pts',(-17.1994661183239,21.261822568227,6.04847520189776));
#132322=CARTESIAN_POINT('Ctrl Pts',(-17.133844588811,21.2092749210363,6.0526447678418));
#132323=CARTESIAN_POINT('Ctrl Pts',(-17.0659158872733,21.1548797633949,
6.05696093058072));
#132324=CARTESIAN_POINT('Ctrl Pts',(-17.0007881489953,21.0970364076612,
6.06127709331964));
#132325=CARTESIAN_POINT('Ctrl Pts',(-16.9388146313976,21.0360779414469,
6.06559325605856));
#132326=CARTESIAN_POINT('Ctrl Pts',(-16.8788598946172,20.9771051908578,
6.06976882025024));
#132327=CARTESIAN_POINT('Ctrl Pts',(-16.8218573212167,20.9152175410394,
6.07394438444192));
#132328=CARTESIAN_POINT('Ctrl Pts',(-16.7680870902015,20.8507519419374,
6.0781199486336));
#132329=CARTESIAN_POINT('Ctrl Pts',(-16.7116010526442,20.7830303386771,
6.08250641064614));
#132330=CARTESIAN_POINT('Ctrl Pts',(-16.6586828203999,20.7124639847437,
6.08689287265868));
#132331=CARTESIAN_POINT('Ctrl Pts',(-16.6096058643084,20.6394780559179,
6.09127933467122));
#132332=CARTESIAN_POINT('Ctrl Pts',(-16.5605289082169,20.5664921270921,
6.09566579668377));
#132333=CARTESIAN_POINT('Ctrl Pts',(-16.5152934615327,20.4910871600581,
6.10005225869631));
#132334=CARTESIAN_POINT('Ctrl Pts',(-16.4741163568267,20.4137160593082,
6.10443872070885));
#132335=CARTESIAN_POINT('Ctrl Pts',(-16.4348338717473,20.3399049175952,
6.1086233551019));
#132336=CARTESIAN_POINT('Ctrl Pts',(-16.3990982578627,20.2640298565514,
6.11280798949495));
#132337=CARTESIAN_POINT('Ctrl Pts',(-16.3671315774457,20.1864659759906,
6.116992623888));
#132338=CARTESIAN_POINT('Ctrl Pts',(-16.3352103976415,20.1090124980131,
6.12117130197195));
#132339=CARTESIAN_POINT('Ctrl Pts',(-16.3070476692931,20.0298753969617,
6.12534998005591));
#132340=CARTESIAN_POINT('Ctrl Pts',(-16.2828196558214,19.949454413158,6.12952865813987));
#132341=CARTESIAN_POINT('Ctrl Pts',(-16.2581573726207,19.8675919410174,
6.1337822360253));
#132342=CARTESIAN_POINT('Ctrl Pts',(-16.2375724777941,19.7843995318231,
6.13803581391074));
#132343=CARTESIAN_POINT('Ctrl Pts',(-16.2211996301976,19.70032024434,6.14228939179617));
#132344=CARTESIAN_POINT('Ctrl Pts',(-16.2051442022007,19.6178709979119,
6.14646050577412));
#132345=CARTESIAN_POINT('Ctrl Pts',(-16.1931390533221,19.5345694264037,
6.15063161975207));
#132346=CARTESIAN_POINT('Ctrl Pts',(-16.18526042222,19.4508469609104,6.15480273373002));
#132347=CARTESIAN_POINT('Ctrl Pts',(-16.1773844348688,19.367152589299,6.1589724480504));
#132348=CARTESIAN_POINT('Ctrl Pts',(-16.1736322583368,19.2830380618257,
6.16314216237077));
#132349=CARTESIAN_POINT('Ctrl Pts',(-16.1740284019004,19.1989411060445,
6.16731187669115));
#132350=CARTESIAN_POINT('Ctrl Pts',(-16.1744245313676,19.114847142794,6.17148144263519));
#132351=CARTESIAN_POINT('Ctrl Pts',(-16.1789686844146,19.0307712100163,
6.17565100857923));
#132352=CARTESIAN_POINT('Ctrl Pts',(-16.187633250542,18.9471508437488,6.17982057452327));
#132353=CARTESIAN_POINT('Ctrl Pts',(-16.1966024521254,18.8605904885602,
6.18413673726219));
#132354=CARTESIAN_POINT('Ctrl Pts',(-16.2099871509034,18.7745188559838,
6.18845290000111));
#132355=CARTESIAN_POINT('Ctrl Pts',(-16.2276984844483,18.689413273613,6.19276906274002));
#132356=CARTESIAN_POINT('Ctrl Pts',(-16.2448328731659,18.6070799966363,
6.1969446269317));
#132357=CARTESIAN_POINT('Ctrl Pts',(-16.2660161808879,18.5256512422047,
6.20112019112338));
#132358=CARTESIAN_POINT('Ctrl Pts',(-16.291116741615,18.4455449811373,6.20529575531506));
#132359=CARTESIAN_POINT('Ctrl Pts',(-16.3174850719935,18.361392743258,6.2096822173276));
#132360=CARTESIAN_POINT('Ctrl Pts',(-16.3481765728436,18.2787006554451,
6.21406867934013));
#132361=CARTESIAN_POINT('Ctrl Pts',(-16.3829817631982,18.1979288029831,
6.21845514135267));
#132362=CARTESIAN_POINT('Ctrl Pts',(-16.4177869535528,18.1171569505211,
6.22284160336521));
#132363=CARTESIAN_POINT('Ctrl Pts',(-16.4567055084016,18.0383058200372,
6.22722806537775));
#132364=CARTESIAN_POINT('Ctrl Pts',(-16.4994739740983,17.9618028820207,
6.23161452739028));
#132365=CARTESIAN_POINT('Ctrl Pts',(-16.5415036475325,17.8866214732604,
6.23592521665433));
#132366=CARTESIAN_POINT('Ctrl Pts',(-16.5874123973693,17.8134194400118,
6.24023590591838));
#132367=CARTESIAN_POINT('Ctrl Pts',(-16.6369860604329,17.7426224813552,
6.24454659518243));
#132368=CARTESIAN_POINT('Ctrl Pts',(-16.6850336937779,17.6740048706875,
6.2487245881816));
#132369=CARTESIAN_POINT('Ctrl Pts',(-16.7365236311432,17.6076468533131,
6.25290258118077));
#132370=CARTESIAN_POINT('Ctrl Pts',(-16.7912139344855,17.5439120288232,
6.25708057417994));
#132371=CARTESIAN_POINT('Ctrl Pts',(-16.8485097468532,17.4771408039058,
6.26145761157643));
#132372=CARTESIAN_POINT('Ctrl Pts',(-16.9093182143514,17.4132493917059,
6.26583464897291));
#132373=CARTESIAN_POINT('Ctrl Pts',(-16.973310725425,17.3526207926269,6.2702116863694));
#132374=CARTESIAN_POINT('Ctrl Pts',(-17.0373032364986,17.291992193548,6.27458872376588));
#132375=CARTESIAN_POINT('Ctrl Pts',(-17.1044794046939,17.2346268461436,
6.27896576116237));
#132376=CARTESIAN_POINT('Ctrl Pts',(-17.174464231106,17.180864983421,6.28334279855885));
#132377=CARTESIAN_POINT('Origin',(-18.734,19.211,-1.76670989022852));
#132378=CARTESIAN_POINT('',(-17.174464231106,17.180864983421,7.14996297786979));
#132379=CARTESIAN_POINT('',(-17.174464231106,17.180864983421,7.08324142508076));
#132380=CARTESIAN_POINT('',(-17.174464231106,17.180864983421,-1.76670989022852));
#132381=CARTESIAN_POINT('',(-21.2939991231355,19.208881145288,6.6332901097715));
#132382=CARTESIAN_POINT('Ctrl Pts',(-21.2939991231355,19.208881145288,6.6332901097715));
#132383=CARTESIAN_POINT('Ctrl Pts',(-21.2940674480299,19.2914312459012,
6.63740642252224));
#132384=CARTESIAN_POINT('Ctrl Pts',(-21.2901386830331,19.374124140816,6.64152273527298));
#132385=CARTESIAN_POINT('Ctrl Pts',(-21.2821979940262,19.4565340775554,
6.64563904802373));
#132386=CARTESIAN_POINT('Ctrl Pts',(-21.2742662779566,19.5388508914942,
6.64975070936244));
#132387=CARTESIAN_POINT('Ctrl Pts',(-21.2623316869624,19.6208849121509,
6.65386237070115));
#132388=CARTESIAN_POINT('Ctrl Pts',(-21.2464314307688,19.7022110602224,
6.65797403203986));
#132389=CARTESIAN_POINT('Ctrl Pts',(-21.2305407999847,19.7834879765415,
6.66208320433541));
#132390=CARTESIAN_POINT('Ctrl Pts',(-21.2106893569246,19.864057405363,6.66619237663095));
#132391=CARTESIAN_POINT('Ctrl Pts',(-21.1869659077107,19.9435013690152,
6.6703015489265));
#132392=CARTESIAN_POINT('Ctrl Pts',(-21.1632492097461,20.0229227244029,
6.67440955182855));
#132393=CARTESIAN_POINT('Ctrl Pts',(-21.1356628286736,20.1012187954781,
6.6785175547306));
#132394=CARTESIAN_POINT('Ctrl Pts',(-21.1043458531985,20.1779852823206,
6.68262555763265));
#132395=CARTESIAN_POINT('Ctrl Pts',(-21.0730277445931,20.2547545467759,
6.68673370917301));
#132396=CARTESIAN_POINT('Ctrl Pts',(-21.0379789552761,20.3299936782021,
6.69084186071338));
#132397=CARTESIAN_POINT('Ctrl Pts',(-20.9993866849092,20.4033184003596,
6.69495001225374));
#132398=CARTESIAN_POINT('Ctrl Pts',(-20.960756173379,20.4767157801412,6.69906223457026));
#132399=CARTESIAN_POINT('Ctrl Pts',(-20.9185753946449,20.5481945435132,
6.70317445688679));
#132400=CARTESIAN_POINT('Ctrl Pts',(-20.8730771242595,20.6173957680787,
6.70728667920331));
#132401=CARTESIAN_POINT('Ctrl Pts',(-20.8275541489316,20.6866345679687,
6.71140113440066));
#132402=CARTESIAN_POINT('Ctrl Pts',(-20.7787103793541,20.7535929860942,
6.71551558959801));
#132403=CARTESIAN_POINT('Ctrl Pts',(-20.7268199445205,20.8179438909686,
6.71963004479536));
#132404=CARTESIAN_POINT('Ctrl Pts',(-20.6748438133911,20.8824010704232,
6.72375129495542));
#132405=CARTESIAN_POINT('Ctrl Pts',(-20.6198112918951,20.9442417891335,
6.72787254511548));
#132406=CARTESIAN_POINT('Ctrl Pts',(-20.5620341095488,21.003175017772,6.73199379527554));
#132407=CARTESIAN_POINT('Ctrl Pts',(-20.5297457003867,21.0361094760174,
6.73429692959298));
#132408=CARTESIAN_POINT('Ctrl Pts',(-20.4966007367166,21.0681366118251,
6.73660006391043));
#132409=CARTESIAN_POINT('Ctrl Pts',(-20.4626578964191,21.0992112903878,
6.73890319822788));
#132410=CARTESIAN_POINT('Ctrl Pts',(-20.400986123379,21.1556718136325,6.74308783262093));
#132411=CARTESIAN_POINT('Ctrl Pts',(-20.3364305466715,21.2092127933027,
6.74727246701397));
#132412=CARTESIAN_POINT('Ctrl Pts',(-20.2692989765722,21.2595255801518,
6.75145710140702));
#132413=CARTESIAN_POINT('Ctrl Pts',(-20.2022629599537,21.3097667529764,
6.75563577949096));
#132414=CARTESIAN_POINT('Ctrl Pts',(-20.1326585979523,21.3567885864285,
6.75981445757491));
#132415=CARTESIAN_POINT('Ctrl Pts',(-20.0608289916761,21.4003206313484,
6.76399313565886));
#132416=CARTESIAN_POINT('Ctrl Pts',(-19.9877118913304,21.4446329568876,
6.76824671354429));
#132417=CARTESIAN_POINT('Ctrl Pts',(-19.9122893426569,21.4853288288423,
6.77250029142973));
#132418=CARTESIAN_POINT('Ctrl Pts',(-19.8349567777299,21.5221672751168,
6.77675386931516));
#132419=CARTESIAN_POINT('Ctrl Pts',(-19.7591234554761,21.5582915362258,
6.78092498329311));
#132420=CARTESIAN_POINT('Ctrl Pts',(-19.6814539493099,21.5907063974351,
6.78509609727106));
#132421=CARTESIAN_POINT('Ctrl Pts',(-19.6023470115176,21.6192303601583,
6.78926721124901));
#132422=CARTESIAN_POINT('Ctrl Pts',(-19.5232666188223,21.6477447513905,
6.79343692556939));
#132423=CARTESIAN_POINT('Ctrl Pts',(-19.4427501848435,21.6723706812233,
6.79760663988976));
#132424=CARTESIAN_POINT('Ctrl Pts',(-19.3612154692016,21.6929751721551,
6.80177635421013));
#132425=CARTESIAN_POINT('Ctrl Pts',(-19.2796836549147,21.7135789298907,
6.80594592015418));
#132426=CARTESIAN_POINT('Ctrl Pts',(-19.1971340772293,21.7301614213603,
6.81011548609822));
#132427=CARTESIAN_POINT('Ctrl Pts',(-19.1139973178553,21.7426401873929,
6.81428505204227));
#132428=CARTESIAN_POINT('Ctrl Pts',(-19.0279375725821,21.755557691445,6.81860121478119));
#132429=CARTESIAN_POINT('Ctrl Pts',(-18.9412491083342,21.7640774486061,
6.82291737752011));
#132430=CARTESIAN_POINT('Ctrl Pts',(-18.8544163259005,21.7681663826307,
6.82723354025903));
#132431=CARTESIAN_POINT('Ctrl Pts',(-18.7704121122214,21.7721221200595,
6.83140910445071));
#132432=CARTESIAN_POINT('Ctrl Pts',(-18.68627330923,21.7719313177434,6.83558466864239));
#132433=CARTESIAN_POINT('Ctrl Pts',(-18.6024375216845,21.7676171622477,
6.83976023283407));
#132434=CARTESIAN_POINT('Ctrl Pts',(-18.5143673878107,21.7630851090138,
6.84414669484661));
#132435=CARTESIAN_POINT('Ctrl Pts',(-18.4266322652435,21.7540022746857,
6.84853315685916));
#132436=CARTESIAN_POINT('Ctrl Pts',(-18.3397299608673,21.7404566879554,
6.8529196188717));
#132437=CARTESIAN_POINT('Ctrl Pts',(-18.252827656491,21.7269111012251,6.85730608088424));
#132438=CARTESIAN_POINT('Ctrl Pts',(-18.1667587226473,21.7089029553708,
6.86169254289678));
#132439=CARTESIAN_POINT('Ctrl Pts',(-18.0820028534405,21.6865806835727,
6.86607900490932));
#132440=CARTESIAN_POINT('Ctrl Pts',(-18.0011467274142,21.6652854925895,
6.87026363930237));
#132441=CARTESIAN_POINT('Ctrl Pts',(-17.9211845272768,21.6399851855304,
6.87444827369542));
#132442=CARTESIAN_POINT('Ctrl Pts',(-17.8425423900639,21.6107715161421,
6.87863290808848));
#132443=CARTESIAN_POINT('Ctrl Pts',(-17.7640121901996,21.5815994287963,
6.88281158617241));
#132444=CARTESIAN_POINT('Ctrl Pts',(-17.6867987486328,21.5485252020904,
6.88699026425635));
#132445=CARTESIAN_POINT('Ctrl Pts',(-17.6113151844297,21.5116909407584,
6.89116894234028));
#132446=CARTESIAN_POINT('Ctrl Pts',(-17.5344786315872,21.4741964517643,
6.89542252022572));
#132447=CARTESIAN_POINT('Ctrl Pts',(-17.4594350484394,21.4328059278378,
6.89967609811115));
#132448=CARTESIAN_POINT('Ctrl Pts',(-17.3866010942662,21.3877214311499,
6.90392967599659));
#132449=CARTESIAN_POINT('Ctrl Pts',(-17.3151791684185,21.3435109854055,
6.90810078997454));
#132450=CARTESIAN_POINT('Ctrl Pts',(-17.2458823693354,21.2957487717616,
6.91227190395249));
#132451=CARTESIAN_POINT('Ctrl Pts',(-17.1790791456549,21.244671836045,6.91644301793044));
#132452=CARTESIAN_POINT('Ctrl Pts',(-17.1122983384412,21.1936120396874,
6.92061273225081));
#132453=CARTESIAN_POINT('Ctrl Pts',(-17.0480098099919,21.139240009464,6.92478244657119));
#132454=CARTESIAN_POINT('Ctrl Pts',(-16.9865514987009,21.0818350369039,
6.92895216089156));
#132455=CARTESIAN_POINT('Ctrl Pts',(-16.9250953743602,21.0244321070591,
6.93312172683561));
#132456=CARTESIAN_POINT('Ctrl Pts',(-16.8664696025459,20.9639967641002,
6.93729129277965));
#132457=CARTESIAN_POINT('Ctrl Pts',(-16.8109765840842,20.9008464255191,
6.9414608587237));
#132458=CARTESIAN_POINT('Ctrl Pts',(-16.7535324995515,20.8354757989379,
6.94577702146262));
#132459=CARTESIAN_POINT('Ctrl Pts',(-16.6994459105392,20.7671961022136,
6.95009318420154));
#132460=CARTESIAN_POINT('Ctrl Pts',(-16.649006825895,20.6963967362073,6.95440934694046));
#132461=CARTESIAN_POINT('Ctrl Pts',(-16.6002107891278,20.6279036521019,
6.95858491113214));
#132462=CARTESIAN_POINT('Ctrl Pts',(-16.5548284854399,20.5570529563656,
6.96276047532382));
#132463=CARTESIAN_POINT('Ctrl Pts',(-16.5130772857549,20.4842251557954,
6.9669360395155));
#132464=CARTESIAN_POINT('Ctrl Pts',(-16.469217332228,20.4077189961501,6.97132250152804));
#132465=CARTESIAN_POINT('Ctrl Pts',(-16.4293652006909,20.3290312765031,
6.97570896354058));
#132466=CARTESIAN_POINT('Ctrl Pts',(-16.3937163263691,20.2486282219257,
6.98009542555312));
#132467=CARTESIAN_POINT('Ctrl Pts',(-16.3580674520474,20.1682251673484,
6.98448188756566));
#132468=CARTESIAN_POINT('Ctrl Pts',(-16.3266219713968,20.0861073468905,
6.98886834957821));
#132469=CARTESIAN_POINT('Ctrl Pts',(-16.2995147249235,20.0027584514457,
6.99325481159075));
#132470=CARTESIAN_POINT('Ctrl Pts',(-16.2736547230431,19.9232445622331,
6.99743944598379));
#132471=CARTESIAN_POINT('Ctrl Pts',(-16.251646255088,19.8423144298573,7.00162408037684));
#132472=CARTESIAN_POINT('Ctrl Pts',(-16.233642830573,19.7603760326905,7.00580871476989));
#132473=CARTESIAN_POINT('Ctrl Pts',(-16.2156650317043,19.6785542646903,
7.00998739285383));
#132474=CARTESIAN_POINT('Ctrl Pts',(-16.2016810508028,19.595727528011,7.01416607093777));
#132475=CARTESIAN_POINT('Ctrl Pts',(-16.1917950137906,19.5123201090072,
7.01834474902171));
#132476=CARTESIAN_POINT('Ctrl Pts',(-16.1817317766699,19.4274176719615,
7.02259832690714));
#132477=CARTESIAN_POINT('Ctrl Pts',(-16.1759149888559,19.3419139888706,
7.02685190479258));
#132478=CARTESIAN_POINT('Ctrl Pts',(-16.1744002778054,19.256268776672,7.03110548267802));
#132479=CARTESIAN_POINT('Ctrl Pts',(-16.1729149323844,19.1722839640347,
7.03527659665598));
#132480=CARTESIAN_POINT('Ctrl Pts',(-16.1755663524988,19.0881635420986,
7.03944771063393));
#132481=CARTESIAN_POINT('Ctrl Pts',(-16.1823546543812,19.0043456262698,
7.04361882461188));
#132482=CARTESIAN_POINT('Ctrl Pts',(-16.1891406783834,18.9205558363522,
7.04778853893226));
#132483=CARTESIAN_POINT('Ctrl Pts',(-16.2000607901197,18.8370688090937,
7.05195825325264));
#132484=CARTESIAN_POINT('Ctrl Pts',(-16.2150630692561,18.7543198724111,
7.05612796757302));
#132485=CARTESIAN_POINT('Ctrl Pts',(-16.230064814547,18.671573880291,7.06029753351705));
#132486=CARTESIAN_POINT('Ctrl Pts',(-16.2491483555177,18.5895663790281,
7.06446709946109));
#132487=CARTESIAN_POINT('Ctrl Pts',(-16.2722104781216,18.5087234519295,
7.06863666540513));
#132488=CARTESIAN_POINT('Ctrl Pts',(-16.2960834365062,18.4250381872445,
7.07295282814405));
#132489=CARTESIAN_POINT('Ctrl Pts',(-16.3242198111559,18.3426014204634,
7.07726899088298));
#132490=CARTESIAN_POINT('Ctrl Pts',(-16.3564491538596,18.2618677784328,
7.0815851536219));
#132491=CARTESIAN_POINT('Ctrl Pts',(-16.3876286291147,18.1837640262997,
7.08576071781358));
#132492=CARTESIAN_POINT('Ctrl Pts',(-16.4226382716204,18.1072545529911,
7.08993628200526));
#132493=CARTESIAN_POINT('Ctrl Pts',(-16.4612757941353,18.0327280941665,
7.09411184619694));
#132494=CARTESIAN_POINT('Ctrl Pts',(-16.5018648060604,17.9544374810766,
7.09849830820948));
#132495=CARTESIAN_POINT('Ctrl Pts',(-16.5464575227364,17.878335974976,7.10288477022202));
#132496=CARTESIAN_POINT('Ctrl Pts',(-16.5947677080407,17.80484026475,7.10727123223456));
#132497=CARTESIAN_POINT('Ctrl Pts',(-16.643077893345,17.7313445545239,7.1116576942471));
#132498=CARTESIAN_POINT('Ctrl Pts',(-16.6951051426578,17.6604550629257,
7.11604415625964));
#132499=CARTESIAN_POINT('Ctrl Pts',(-16.7505157350918,17.592546982189,7.12043061827219));
#132500=CARTESIAN_POINT('Ctrl Pts',(-16.8033793819712,17.5277602935319,
7.1246154567425));
#132501=CARTESIAN_POINT('Ctrl Pts',(-16.8595189473393,17.4654457911716,
7.12880029521283));
#132502=CARTESIAN_POINT('Ctrl Pts',(-16.9186744386476,17.4059534337584,
7.13298513368314));
#132503=CARTESIAN_POINT('Ctrl Pts',(-16.9777385242404,17.3465530025786,
7.13716350583653));
#132504=CARTESIAN_POINT('Ctrl Pts',(-17.0398089529392,17.2899663736295,
7.14134187798991));
#132505=CARTESIAN_POINT('Ctrl Pts',(-17.1045853939259,17.236510688428,7.1455202501433));
#132506=CARTESIAN_POINT('Ctrl Pts',(-17.1275436242151,17.2175647890789,
7.14700115938546));
#132507=CARTESIAN_POINT('Ctrl Pts',(-17.1508414102745,17.1990118720507,
7.14848206862763));
#132508=CARTESIAN_POINT('Ctrl Pts',(-17.174464231106,17.180864983421,7.14996297786979));
#132509=CARTESIAN_POINT('Ctrl Pts',(-17.1721129728022,17.177834880393,6.34984102388608));
#132510=CARTESIAN_POINT('Ctrl Pts',(-17.211840036684,17.1470017875518,6.35235260865192));
#132511=CARTESIAN_POINT('Ctrl Pts',(-17.9391679592174,16.6183204949674,
6.39725612897823));
#132512=CARTESIAN_POINT('Ctrl Pts',(-19.9200693000182,16.4259449961135,
6.48455158486501));
#132513=CARTESIAN_POINT('Ctrl Pts',(-21.2201493011995,18.0710819511262,
6.57652302872765));
#132514=CARTESIAN_POINT('Ctrl Pts',(-21.2969229188781,19.0646440605456,
6.62610253702981));
#132515=CARTESIAN_POINT('Ctrl Pts',(-21.2956375040978,19.2088797892363,
6.6332901097715));
#132516=CARTESIAN_POINT('',(-21.293999428374,19.2127107672549,6.5667098902584));
#132517=CARTESIAN_POINT('Ctrl Pts',(-17.174464231106,17.180864983421,6.28334279855885));
#132518=CARTESIAN_POINT('Ctrl Pts',(-17.2411329207509,17.129650554175,6.28751243593184));
#132519=CARTESIAN_POINT('Ctrl Pts',(-17.3103497458901,17.0817061849628,
6.29168207330483));
#132520=CARTESIAN_POINT('Ctrl Pts',(-17.3817565908666,17.037284801899,6.29585171067782));
#132521=CARTESIAN_POINT('Ctrl Pts',(-17.4531632307407,16.992863546427,6.30002133607433));
#132522=CARTESIAN_POINT('Ctrl Pts',(-17.5267594866646,16.9519654989341,
6.30419096147084));
#132523=CARTESIAN_POINT('Ctrl Pts',(-17.6021597931636,16.914799280074,6.30836058686735));
#132524=CARTESIAN_POINT('Ctrl Pts',(-17.6781541978221,16.8773402191389,
6.31256306580105));
#132525=CARTESIAN_POINT('Ctrl Pts',(-17.7559807895149,16.8436722785943,
6.31676554473475));
#132526=CARTESIAN_POINT('Ctrl Pts',(-17.8352228883562,16.8139602206919,
6.32096802366844));
#132527=CARTESIAN_POINT('Ctrl Pts',(-17.9139613122198,16.784437017203,6.32514379099917));
#132528=CARTESIAN_POINT('Ctrl Pts',(-17.9940968401885,16.758819636878,6.32931955832989));
#132529=CARTESIAN_POINT('Ctrl Pts',(-18.0752057298362,16.7372194702037,
6.33349532566061));
#132530=CARTESIAN_POINT('Ctrl Pts',(-18.1570928770901,16.7154120451871,
6.33771116039579));
#132531=CARTESIAN_POINT('Ctrl Pts',(-18.2399716959823,16.6976994377661,
6.34192699513098));
#132532=CARTESIAN_POINT('Ctrl Pts',(-18.323397753023,16.6841430996637,6.34614282986616));
#132533=CARTESIAN_POINT('Ctrl Pts',(-18.4068238100637,16.6705867615613,
6.35035866460135));
#132534=CARTESIAN_POINT('Ctrl Pts',(-18.4907966255752,16.6611866818601,
6.35457449933654));
#132535=CARTESIAN_POINT('Ctrl Pts',(-18.5748705298082,16.6559505265619,
6.35879033407172));
#132536=CARTESIAN_POINT('Ctrl Pts',(-18.6583222240304,16.650753122744,6.36297496846477));
#132537=CARTESIAN_POINT('Ctrl Pts',(-18.7421841184714,16.6496388297569,
6.36715960285782));
#132538=CARTESIAN_POINT('Ctrl Pts',(-18.8260228331345,16.6526544802975,
6.37134423725088));
#132539=CARTESIAN_POINT('Ctrl Pts',(-18.9097422137643,16.6556658384329,
6.37552291533482));
#132540=CARTESIAN_POINT('Ctrl Pts',(-18.9934380243482,16.6627954472227,
6.37970159341876));
#132541=CARTESIAN_POINT('Ctrl Pts',(-19.0766734176216,16.6740382484445,
6.3838802715027));
#132542=CARTESIAN_POINT('Ctrl Pts',(-19.1614007454992,16.6854825687982,
6.38813384938813));
#132543=CARTESIAN_POINT('Ctrl Pts',(-19.2456505065471,16.7011890198917,
6.39238742727357));
#132544=CARTESIAN_POINT('Ctrl Pts',(-19.328963647833,16.7210967372692,6.396641005159));
#132545=CARTESIAN_POINT('Ctrl Pts',(-19.4106616013028,16.7406185046987,
6.40081211913695));
#132546=CARTESIAN_POINT('Ctrl Pts',(-19.4914584592904,16.7641799807698,
6.4049832331149));
#132547=CARTESIAN_POINT('Ctrl Pts',(-19.5709299408018,16.7916719374609,
6.40915434709286));
#132548=CARTESIAN_POINT('Ctrl Pts',(-19.65037475489,16.8191546689603,6.41332406141323));
#132549=CARTESIAN_POINT('Ctrl Pts',(-19.728494641376,16.8505651114306,6.4174937757336));
#132550=CARTESIAN_POINT('Ctrl Pts',(-19.8048810053294,16.8857443425669,
6.42166349005397));
#132551=CARTESIAN_POINT('Ctrl Pts',(-19.8812646511282,16.9209223218752,
6.42583305599801));
#132552=CARTESIAN_POINT('Ctrl Pts',(-19.9559144795495,16.9598686299933,
6.43000262194205));
#132553=CARTESIAN_POINT('Ctrl Pts',(-20.0284436491278,17.0023769811866,
6.43417218788609));
#132554=CARTESIAN_POINT('Ctrl Pts',(-20.1035228548341,17.046379873568,6.43848835062501));
#132555=CARTESIAN_POINT('Ctrl Pts',(-20.1763290473291,17.0941996856771,
6.44280451336393));
#132556=CARTESIAN_POINT('Ctrl Pts',(-20.2464645244674,17.1455579015069,
6.44712067610285));
#132557=CARTESIAN_POINT('Ctrl Pts',(-20.3143153458149,17.195243128858,6.45129624029454));
#132558=CARTESIAN_POINT('Ctrl Pts',(-20.3796664407518,17.2482394397191,
6.45547180448622));
#132559=CARTESIAN_POINT('Ctrl Pts',(-20.4421918593801,17.3042539310261,
6.4596473686779));
#132560=CARTESIAN_POINT('Ctrl Pts',(-20.5078752882632,17.3630975811272,
6.46403383069044));
#132561=CARTESIAN_POINT('Ctrl Pts',(-20.5704396751019,17.4252719095177,
6.46842029270298));
#132562=CARTESIAN_POINT('Ctrl Pts',(-20.6295529524492,17.490395744379,6.47280675471552));
#132563=CARTESIAN_POINT('Ctrl Pts',(-20.6886662297965,17.5555195792402,
6.47719321672806));
#132564=CARTESIAN_POINT('Ctrl Pts',(-20.7443280892574,17.6235924232491,
6.4815796787406));
#132565=CARTESIAN_POINT('Ctrl Pts',(-20.7962584977302,17.6941974787272,
6.48596614075314));
#132566=CARTESIAN_POINT('Ctrl Pts',(-20.8460908704134,17.7619500256716,
6.4901753857061));
#132567=CARTESIAN_POINT('Ctrl Pts',(-20.8926734978045,17.8322867639503,
6.49438463065905));
#132568=CARTESIAN_POINT('Ctrl Pts',(-20.9357293738867,17.9048653345981,
6.498593875612));
#132569=CARTESIAN_POINT('Ctrl Pts',(-20.9787228581407,17.9773387323842,
6.5027970209913));
#132570=CARTESIAN_POINT('Ctrl Pts',(-21.0181995127222,18.0520471246587,
6.50700016637059));
#132571=CARTESIAN_POINT('Ctrl Pts',(-21.0539239335172,18.1286170073888,
6.51120331174989));
#132572=CARTESIAN_POINT('Ctrl Pts',(-21.0896068791136,18.2050979943154,
6.51540157737787));
#132573=CARTESIAN_POINT('Ctrl Pts',(-21.1215460556625,18.283435770082,6.51959984300585));
#132574=CARTESIAN_POINT('Ctrl Pts',(-21.1495512259746,18.3632310015738,
6.52379810863383));
#132575=CARTESIAN_POINT('Ctrl Pts',(-21.177530608527,18.4429527559101,6.52799250840905));
#132576=CARTESIAN_POINT('Ctrl Pts',(-21.20158303815,18.5241288717761,6.53218690818426));
#132577=CARTESIAN_POINT('Ctrl Pts',(-21.2215663308331,18.6063399717978,
6.53638130795947));
#132578=CARTESIAN_POINT('Ctrl Pts',(-21.2415389226779,18.6885070486596,
6.54057346167871));
#132579=CARTESIAN_POINT('Ctrl Pts',(-21.2574466025638,18.7717075687081,
6.54476561539795));
#132580=CARTESIAN_POINT('Ctrl Pts',(-21.2691973211302,18.8555080269057,
6.54895776911719));
#132581=CARTESIAN_POINT('Ctrl Pts',(-21.2809466969547,18.9392989093157,
6.55314944380356));
#132582=CARTESIAN_POINT('Ctrl Pts',(-21.288539988214,19.0236891460417,6.55734111848993));
#132583=CARTESIAN_POINT('Ctrl Pts',(-21.2919366299884,19.1082371810269,
6.5615327931763));
#132584=CARTESIAN_POINT('Ctrl Pts',(-21.2933350165072,19.1430453357178,
6.56325849219371));
#132585=CARTESIAN_POINT('Ctrl Pts',(-21.294022704555,19.1778801783151,6.56498419121111));
#132586=CARTESIAN_POINT('Ctrl Pts',(-21.2939994283744,19.2127107666517,
6.56670989022851));
#132587=CARTESIAN_POINT('Ctrl Pts',(-21.293999428374,19.2127107672549,6.5667098902584));
#132588=CARTESIAN_POINT('Ctrl Pts',(-21.2939356382109,19.308166639887,6.57143929947813));
#132589=CARTESIAN_POINT('Ctrl Pts',(-21.2885288437516,19.4034153336882,
6.57616870869786));
#132590=CARTESIAN_POINT('Ctrl Pts',(-21.2778724975471,19.4979019278834,
6.5808981179176));
#132591=CARTESIAN_POINT('Ctrl Pts',(-21.2671635859907,19.5928546031339,
6.58565085624617));
#132592=CARTESIAN_POINT('Ctrl Pts',(-21.2511533349013,19.6870374428281,
6.59040359457474));
#132593=CARTESIAN_POINT('Ctrl Pts',(-21.2299860493109,19.7799056526747,
6.59515633290331));
#132594=CARTESIAN_POINT('Ctrl Pts',(-21.2086961910765,19.8733116311444,
6.59993659274384));
#132595=CARTESIAN_POINT('Ctrl Pts',(-21.1821895164634,19.965387517667,6.60471685258437));
#132596=CARTESIAN_POINT('Ctrl Pts',(-21.15066091743,20.055600503295,6.60949711242489));
#132597=CARTESIAN_POINT('Ctrl Pts',(-21.1426476472037,20.0785289255507,
6.61071205742812));
#132598=CARTESIAN_POINT('Ctrl Pts',(-21.134310213157,20.1013371264666,6.61192700243135));
#132599=CARTESIAN_POINT('Ctrl Pts',(-21.1256522921827,20.1240166007786,
6.61314194743458));
#132600=CARTESIAN_POINT('Ctrl Pts',(-21.0958318198279,20.2021315014283,
6.61732658182763));
#132601=CARTESIAN_POINT('Ctrl Pts',(-21.062124806143,20.2789292632222,6.62151121622068));
#132602=CARTESIAN_POINT('Ctrl Pts',(-21.0246680532229,20.3539960060928,
6.62569585061373));
#132603=CARTESIAN_POINT('Ctrl Pts',(-20.9872646153543,20.4289559007464,
6.62987452869768));
#132604=CARTESIAN_POINT('Ctrl Pts',(-20.9461222434274,20.5021892624269,
6.63405320678162));
#132605=CARTESIAN_POINT('Ctrl Pts',(-20.9014264094923,20.5733005393213,
6.63823188486556));
#132606=CARTESIAN_POINT('Ctrl Pts',(-20.8559294348563,20.6456864347473,
6.642485462751));
#132607=CARTESIAN_POINT('Ctrl Pts',(-20.8067505255349,20.715872969927,6.64673904063643));
#132608=CARTESIAN_POINT('Ctrl Pts',(-20.7541351457545,20.7834674854786,
6.65099261852187));
#132609=CARTESIAN_POINT('Ctrl Pts',(-20.7025398177816,20.8497515494465,
6.65516373249982));
#132610=CARTESIAN_POINT('Ctrl Pts',(-20.6476403712487,20.9135428198972,
6.65933484647777));
#132611=CARTESIAN_POINT('Ctrl Pts',(-20.5897118973506,20.9745003130228,
6.66350596045573));
#132612=CARTESIAN_POINT('Ctrl Pts',(-20.5318028619114,21.0354373512728,
6.6676756747761));
#132613=CARTESIAN_POINT('Ctrl Pts',(-20.4708671343699,21.0935421675084,
6.67184538909647));
#132614=CARTESIAN_POINT('Ctrl Pts',(-20.4072185463108,21.1485086312792,
6.67601510341685));
#132615=CARTESIAN_POINT('Ctrl Pts',(-20.3435722231416,21.2034731391074,
6.6801846693609));
#132616=CARTESIAN_POINT('Ctrl Pts',(-20.2772135801198,21.2552992164786,
6.68435423530495));
#132617=CARTESIAN_POINT('Ctrl Pts',(-20.2084905554454,21.3037201441908,
6.68852380124899));
#132618=CARTESIAN_POINT('Ctrl Pts',(-20.1373513140027,21.3538434919877,
6.69283996398791));
#132619=CARTESIAN_POINT('Ctrl Pts',(-20.0636787652558,21.4003174810233,
6.69715612672683));
#132620=CARTESIAN_POINT('Ctrl Pts',(-19.9878910926204,21.4428954114938,
6.70147228946575));
#132621=CARTESIAN_POINT('Ctrl Pts',(-19.9145721954497,21.4840863703576,
6.70564785365743));
#132622=CARTESIAN_POINT('Ctrl Pts',(-19.8392743011541,21.5216310329473,
6.70982341784911));
#132623=CARTESIAN_POINT('Ctrl Pts',(-19.7623989816004,21.555353969571,6.71399898204079));
#132624=CARTESIAN_POINT('Ctrl Pts',(-19.6816408724097,21.5907801715548,
6.71838544405333));
#132625=CARTESIAN_POINT('Ctrl Pts',(-19.5991423447412,21.6219882241026,
6.72277190606586));
#132626=CARTESIAN_POINT('Ctrl Pts',(-19.5153878511232,21.6488336748263,
6.7271583680784));
#132627=CARTESIAN_POINT('Ctrl Pts',(-19.4316333575051,21.67567912555,6.73154483009094));
#132628=CARTESIAN_POINT('Ctrl Pts',(-19.3466234783173,21.6981618996353,
6.73593129210348));
#132629=CARTESIAN_POINT('Ctrl Pts',(-19.2608535512399,21.7161996598167,
6.74031775411602));
#132630=CARTESIAN_POINT('Ctrl Pts',(-19.1790300256489,21.7334074759138,
6.74450238850907));
#132631=CARTESIAN_POINT('Ctrl Pts',(-19.096210294286,21.7466343835296,6.74868702290212));
#132632=CARTESIAN_POINT('Ctrl Pts',(-19.0128164131693,21.755771386146,6.75287165729516));
#132633=CARTESIAN_POINT('Ctrl Pts',(-18.9295412329201,21.7648953833701,
6.75705033537911));
#132634=CARTESIAN_POINT('Ctrl Pts',(-18.8456939795803,21.7699409891981,
6.76122901346306));
#132635=CARTESIAN_POINT('Ctrl Pts',(-18.7617076421301,21.7708500515787,
6.765407691547));
#132636=CARTESIAN_POINT('Ctrl Pts',(-18.6762159099411,21.7717754082492,
6.76966126943244));
#132637=CARTESIAN_POINT('Ctrl Pts',(-18.5905805302511,21.7684143685408,
6.77391484731787));
#132638=CARTESIAN_POINT('Ctrl Pts',(-18.5052645325906,21.7607607899466,
6.77816842520331));
#132639=CARTESIAN_POINT('Ctrl Pts',(-18.4216025520252,21.7532555909081,
6.78233953918126));
#132640=CARTESIAN_POINT('Ctrl Pts',(-18.3382481596057,21.7416228491976,
6.78651065315921));
#132641=CARTESIAN_POINT('Ctrl Pts',(-18.2556369703989,21.7259093049076,
6.79068176713716));
#132642=CARTESIAN_POINT('Ctrl Pts',(-18.1730535021745,21.7102010334492,
6.79485148145753));
#132643=CARTESIAN_POINT('Ctrl Pts',(-18.0912131934262,21.690414764858,6.79902119577791));
#132644=CARTESIAN_POINT('Ctrl Pts',(-18.010543322501,21.6666486792255,6.80319091009828));
#132645=CARTESIAN_POINT('Ctrl Pts',(-17.929876322156,21.6428834392923,6.80736047604232));
#132646=CARTESIAN_POINT('Ctrl Pts',(-17.850380117865,21.6151387947156,6.81153004198637));
#132647=CARTESIAN_POINT('Ctrl Pts',(-17.772467310616,21.5835629364141,6.81569960793041));
#132648=CARTESIAN_POINT('Ctrl Pts',(-17.69181518518,21.5508769098878,6.82001577066933));
#132649=CARTESIAN_POINT('Ctrl Pts',(-17.612860361743,21.5140854441413,6.82433193340825));
#132650=CARTESIAN_POINT('Ctrl Pts',(-17.5360366305503,21.4734066313235,
6.82864809614717));
#132651=CARTESIAN_POINT('Ctrl Pts',(-17.4617154243207,21.4340529265546,
6.83282366033885));
#132652=CARTESIAN_POINT('Ctrl Pts',(-17.3893889826097,21.3910615273711,
6.83699922453053));
#132653=CARTESIAN_POINT('Ctrl Pts',(-17.3194221772609,21.3446751353978,
6.84117478872221));
#132654=CARTESIAN_POINT('Ctrl Pts',(-17.2459215149042,21.295945877039,6.84556125073475));
#132655=CARTESIAN_POINT('Ctrl Pts',(-17.1750255931743,21.2434699978814,
6.84994771274729));
#132656=CARTESIAN_POINT('Ctrl Pts',(-17.1071180986345,21.1875766564971,
6.85433417475983));
#132657=CARTESIAN_POINT('Ctrl Pts',(-17.0392106040947,21.1316833151128,
6.85872063677237));
#132658=CARTESIAN_POINT('Ctrl Pts',(-16.9742919138006,21.0723729590137,
6.86310709878491));
#132659=CARTESIAN_POINT('Ctrl Pts',(-16.9126993772538,21.0100175211999,
6.86749356079745));
#132660=CARTESIAN_POINT('Ctrl Pts',(-16.8539408046156,20.9505311495128,
6.8716781951905));
#132661=CARTESIAN_POINT('Ctrl Pts',(-16.7979903187279,20.8880523361676,
6.87586282958355));
#132662=CARTESIAN_POINT('Ctrl Pts',(-16.7451680193311,20.8228769657355,
6.8800474639766));
#132663=CARTESIAN_POINT('Ctrl Pts',(-16.6924209059394,20.7577943643761,
6.88422614206054));
#132664=CARTESIAN_POINT('Ctrl Pts',(-16.6427934219786,20.6900231841701,
6.88840482014448));
#132665=CARTESIAN_POINT('Ctrl Pts',(-16.5965688328438,20.6198960237254,
6.89258349822842));
#132666=CARTESIAN_POINT('Ctrl Pts',(-16.5495157011699,20.5485118843294,
6.89683707611386));
#132667=CARTESIAN_POINT('Ctrl Pts',(-16.5059889968458,20.4746868150557,
6.9010906539993));
#132668=CARTESIAN_POINT('Ctrl Pts',(-16.4662445138507,20.3988068256411,
6.90534423188473));
#132669=CARTESIAN_POINT('Ctrl Pts',(-16.4272705552135,20.324397917889,6.90951534586268));
#132670=CARTESIAN_POINT('Ctrl Pts',(-16.3919336983952,20.2480134825273,
6.91368645984064));
#132671=CARTESIAN_POINT('Ctrl Pts',(-16.3604304325482,20.1700451024153,
6.91785757381859));
#132672=CARTESIAN_POINT('Ctrl Pts',(-16.3289377379264,20.0921028853462,
6.92202728813896));
#132673=CARTESIAN_POINT('Ctrl Pts',(-16.3012762516654,20.0125782052864,
6.92619700245933));
#132674=CARTESIAN_POINT('Ctrl Pts',(-16.2775946975111,19.9318834787288,
6.9303667167797));
#132675=CARTESIAN_POINT('Ctrl Pts',(-16.253913986048,19.8511916236358,6.93453628272375));
#132676=CARTESIAN_POINT('Ctrl Pts',(-16.2342130538339,19.7693302464836,
6.93870584866779));
#132677=CARTESIAN_POINT('Ctrl Pts',(-16.2185906288469,19.6867264923412,
6.94287541461184));
#132678=CARTESIAN_POINT('Ctrl Pts',(-16.2024189386698,19.6012184921059,
6.94719157735076));
#132679=CARTESIAN_POINT('Ctrl Pts',(-16.1906179905571,19.5149154578638,
6.95150774008967));
#132680=CARTESIAN_POINT('Ctrl Pts',(-16.1832392059578,19.4283001877062,
6.95582390282859));
#132681=CARTESIAN_POINT('Ctrl Pts',(-16.1761007844908,19.3445064008637,
6.95999946702027));
#132682=CARTESIAN_POINT('Ctrl Pts',(-16.1731008165489,19.2604208803106,
6.96417503121195));
#132683=CARTESIAN_POINT('Ctrl Pts',(-16.1742327266829,19.1764817953116,
6.96835059540363));
#132684=CARTESIAN_POINT('Ctrl Pts',(-16.175421806907,19.0883031466756,6.97273705741617));
#132685=CARTESIAN_POINT('Ctrl Pts',(-16.1811710990057,19.0002866979193,
6.97712351942872));
#132686=CARTESIAN_POINT('Ctrl Pts',(-16.1914115149699,18.912933236015,6.98150998144126));
#132687=CARTESIAN_POINT('Ctrl Pts',(-16.2016519309342,18.8255797741108,
6.9858964434538));
#132688=CARTESIAN_POINT('Ctrl Pts',(-16.2163832985703,18.7388898583324,
6.99028290546634));
#132689=CARTESIAN_POINT('Ctrl Pts',(-16.2354754819718,18.6533484665025,
6.99466936747888));
#132690=CARTESIAN_POINT('Ctrl Pts',(-16.2536851821496,18.571760988253,6.99885307745115));
#132691=CARTESIAN_POINT('Ctrl Pts',(-16.2759292313583,18.4909145868875,
7.00303678742343));
#132692=CARTESIAN_POINT('Ctrl Pts',(-16.3021321571691,18.4112382886104,
7.0072204973957));
#132693=CARTESIAN_POINT('Ctrl Pts',(-16.3283004575787,18.3316672771937,
7.0113986788771));
#132694=CARTESIAN_POINT('Ctrl Pts',(-16.3584171062891,18.2532637320032,
7.01557686035851));
#132695=CARTESIAN_POINT('Ctrl Pts',(-16.3923558259029,18.1764457182356,
7.01975504183991));
#132696=CARTESIAN_POINT('Ctrl Pts',(-16.426259882933,18.0997061608994,7.02392895602523));
#132697=CARTESIAN_POINT('Ctrl Pts',(-16.4639780734706,18.0245493373741,
7.02810287021055));
#132698=CARTESIAN_POINT('Ctrl Pts',(-16.5053350197041,17.95137608565,7.03227678439588));
#132699=CARTESIAN_POINT('Ctrl Pts',(-16.5474166608013,17.8769206241758,
7.03652383778628));
#132700=CARTESIAN_POINT('Ctrl Pts',(-16.5932656413836,17.8045193749155,
7.04077089117669));
#132701=CARTESIAN_POINT('Ctrl Pts',(-16.642647159626,17.734570761242,7.0450179445671));
#132702=CARTESIAN_POINT('Ctrl Pts',(-16.6911293348285,17.6658960613949,
7.04918765003378));
#132703=CARTESIAN_POINT('Ctrl Pts',(-16.7430161596747,17.5995857851865,
7.05335735550045));
#132704=CARTESIAN_POINT('Ctrl Pts',(-16.7980414116622,17.5359882554916,
7.05752706096713));
#132705=CARTESIAN_POINT('Ctrl Pts',(-16.8545977390559,17.4706211271108,
7.0618127883194));
#132706=CARTESIAN_POINT('Ctrl Pts',(-16.9144694416338,17.4081203624224,
7.06609851567167));
#132707=CARTESIAN_POINT('Ctrl Pts',(-16.9773240231389,17.3488266696359,
7.07038424302394));
#132708=CARTESIAN_POINT('Ctrl Pts',(-17.040178604644,17.2895329768495,7.07466997037622));
#132709=CARTESIAN_POINT('Ctrl Pts',(-17.1060156660477,17.2334467007285,
7.07895569772849));
#132710=CARTESIAN_POINT('Ctrl Pts',(-17.174464231106,17.180864983421,7.08324142508076));
#132711=CARTESIAN_POINT('Origin',(-18.734,19.211,-1.76670989022852));
#132712=CARTESIAN_POINT('',(-17.1770150831773,17.1841768308936,7.94987222090926));
#132713=CARTESIAN_POINT('',(-17.171894433269,17.1775280041638,7.88329696157113));
#132714=CARTESIAN_POINT('',(-17.174464231106,17.180864983421,-1.76670989022852));
#132715=CARTESIAN_POINT('',(-21.2936354886768,19.2104398261304,7.43329008494697));
#132716=CARTESIAN_POINT('Ctrl Pts',(-21.2898971261407,19.2104411453458,
7.4332901097715));
#132717=CARTESIAN_POINT('Ctrl Pts',(-21.2889976171803,19.6723917155128,
7.45617941928649));
#132718=CARTESIAN_POINT('Ctrl Pts',(-20.9482576239576,20.9911305382399,
7.52146066436197));
#132719=CARTESIAN_POINT('Ctrl Pts',(-18.8327965349617,22.2364802930772,
7.62913384499793));
#132720=CARTESIAN_POINT('Ctrl Pts',(-16.2435265567091,20.9317073508827,
7.75630965167935));
#132721=CARTESIAN_POINT('Ctrl Pts',(-15.9876140791817,18.5077088656147,
7.8632224436498));
#132722=CARTESIAN_POINT('Ctrl Pts',(-16.82314712442,17.4566899468327,7.92774330005977));
#132723=CARTESIAN_POINT('Ctrl Pts',(-17.1770150831773,17.1841768308936,
7.94987222090926));
#132724=CARTESIAN_POINT('Ctrl Pts',(-17.174464231106,17.180864983421,7.14996297786979));
#132725=CARTESIAN_POINT('Ctrl Pts',(-17.2410259123316,17.1297327573074,
7.15413571446225));
#132726=CARTESIAN_POINT('Ctrl Pts',(-17.3101705590919,17.0818270774072,
7.1583084510547));
#132727=CARTESIAN_POINT('Ctrl Pts',(-17.381550029553,17.0374133149474,7.16248118764716));
#132728=CARTESIAN_POINT('Ctrl Pts',(-17.4528913210709,16.9930233082048,
7.16665169235597));
#132729=CARTESIAN_POINT('Ctrl Pts',(-17.5264646731537,16.9521217531168,
7.17082219706478));
#132730=CARTESIAN_POINT('Ctrl Pts',(-17.6018924712092,16.9149310673991,
7.17499270177359));
#132731=CARTESIAN_POINT('Ctrl Pts',(-17.6773025517232,16.8777491175523,
7.17916222685563));
#132732=CARTESIAN_POINT('Ctrl Pts',(-17.7545658004615,16.8442765088668,
7.18333175193767));
#132733=CARTESIAN_POINT('Ctrl Pts',(-17.833280695483,16.8146893493392,7.18750127701971));
#132734=CARTESIAN_POINT('Ctrl Pts',(-17.9120007132346,16.7851002642925,
7.19167107345258));
#132735=CARTESIAN_POINT('Ctrl Pts',(-17.9921721337704,16.7593972911318,
7.19584086988545));
#132736=CARTESIAN_POINT('Ctrl Pts',(-18.0733754774907,16.7377076112478,
7.20001066631832));
#132737=CARTESIAN_POINT('Ctrl Pts',(-18.1546632779953,16.7159953726794,
7.20418479961198));
#132738=CARTESIAN_POINT('Ctrl Pts',(-18.2369846995719,16.698304881881,7.20835893290564));
#132739=CARTESIAN_POINT('Ctrl Pts',(-18.3199076637616,16.6847126970456,
7.2125330661993));
#132740=CARTESIAN_POINT('Ctrl Pts',(-18.4028746699408,16.671113293138,7.21670941645586));
#132741=CARTESIAN_POINT('Ctrl Pts',(-18.4864433975924,16.6616165818563,
7.22088576671241));
#132742=CARTESIAN_POINT('Ctrl Pts',(-18.570176627374,16.6562471934488,7.22506211696897));
#132743=CARTESIAN_POINT('Ctrl Pts',(-18.6540564596485,16.650868404165,7.22924577929698));
#132744=CARTESIAN_POINT('Ctrl Pts',(-18.7381009088209,16.6496313792551,
7.23342944162499));
#132745=CARTESIAN_POINT('Ctrl Pts',(-18.8218729238928,16.6525085794073,
7.23761310395301));
#132746=CARTESIAN_POINT('Ctrl Pts',(-18.8885737051579,16.6547994577853,
7.24094421095321));
#132747=CARTESIAN_POINT('Ctrl Pts',(-18.9551017385725,16.6596975633221,
7.24427531795342));
#132748=CARTESIAN_POINT('Ctrl Pts',(-19.0212404493958,16.6671657042506,
7.24760642495362));
#132749=CARTESIAN_POINT('Ctrl Pts',(-19.1043258393295,16.6765474021004,
7.25179105934667));
#132750=CARTESIAN_POINT('Ctrl Pts',(-19.1871057341706,16.6900213769478,
7.25597569373972));
#132751=CARTESIAN_POINT('Ctrl Pts',(-19.2691452086513,16.7075584477249,
7.26016032813276));
#132752=CARTESIAN_POINT('Ctrl Pts',(-19.3510679100948,16.7250705566525,
7.26433900621671));
#132753=CARTESIAN_POINT('Ctrl Pts',(-19.4322518385269,16.7466341786848,
7.26851768430066));
#132754=CARTESIAN_POINT('Ctrl Pts',(-19.5122676703941,16.7721684286898,
7.27269636238461));
#132755=CARTESIAN_POINT('Ctrl Pts',(-19.5937177285411,16.798160361775,7.27694994027005));
#132756=CARTESIAN_POINT('Ctrl Pts',(-19.6739569228737,16.8282666158666,
7.28120351815548));
#132757=CARTESIAN_POINT('Ctrl Pts',(-19.7525437584805,16.8623474901424,
7.28545709604092));
#132758=CARTESIAN_POINT('Ctrl Pts',(-19.8296070349296,16.8957676401671,
7.28962821001887));
#132759=CARTESIAN_POINT('Ctrl Pts',(-19.9050810078235,16.9330094826423,
7.29379932399683));
#132760=CARTESIAN_POINT('Ctrl Pts',(-19.9785668286283,16.9738917305866,
7.29797043797478));
#132761=CARTESIAN_POINT('Ctrl Pts',(-20.0520279905562,17.0147602600976,
7.30214015229516));
#132762=CARTESIAN_POINT('Ctrl Pts',(-20.1235019236784,17.0592665455509,
7.30630986661553));
#132763=CARTESIAN_POINT('Ctrl Pts',(-20.1926138614937,17.1071830870871,
7.31047958093591));
#132764=CARTESIAN_POINT('Ctrl Pts',(-20.2617233400095,17.155097923547,7.31464914687994));
#132765=CARTESIAN_POINT('Ctrl Pts',(-20.3284706127603,17.2064225119979,
7.31881871282398));
#132766=CARTESIAN_POINT('Ctrl Pts',(-20.3925105653945,17.2608864893358,
7.32298827876801));
#132767=CARTESIAN_POINT('Ctrl Pts',(-20.4588020837616,17.3172653529285,
7.32730444150693));
#132768=CARTESIAN_POINT('Ctrl Pts',(-20.5221919593123,17.3770081330231,
7.33162060424585));
#132769=CARTESIAN_POINT('Ctrl Pts',(-20.582336932496,17.4397714478444,7.33593676698477));
#132770=CARTESIAN_POINT('Ctrl Pts',(-20.6405226895044,17.500490254287,7.34011233117645));
#132771=CARTESIAN_POINT('Ctrl Pts',(-20.6956714299403,17.5640354429536,
7.34428789536813));
#132772=CARTESIAN_POINT('Ctrl Pts',(-20.7475130548915,17.6300619310734,
7.34846345955981));
#132773=CARTESIAN_POINT('Ctrl Pts',(-20.8019730770773,17.699423260145,7.35284992157235));
#132774=CARTESIAN_POINT('Ctrl Pts',(-20.8527827827184,17.771522659754,7.35723638358489));
#132775=CARTESIAN_POINT('Ctrl Pts',(-20.8996813854342,17.8459270580721,
7.36162284559743));
#132776=CARTESIAN_POINT('Ctrl Pts',(-20.94657998815,17.9203314563902,7.36600930760997));
#132777=CARTESIAN_POINT('Ctrl Pts',(-20.9895672706481,17.9970403100744,
7.37039576962251));
#132778=CARTESIAN_POINT('Ctrl Pts',(-21.0284398795321,18.0755945044995,
7.37478223163505));
#132779=CARTESIAN_POINT('Ctrl Pts',(-21.0682036058612,18.1559494788324,
7.37926924910127));
#132780=CARTESIAN_POINT('Ctrl Pts',(-21.103794382086,18.2385006465155,7.38375626656748));
#132781=CARTESIAN_POINT('Ctrl Pts',(-21.1349820909848,18.3228080169409,
7.3882432840337));
#132782=CARTESIAN_POINT('Ctrl Pts',(-21.1660643193882,18.4068302499356,
7.39271512587973));
#132783=CARTESIAN_POINT('Ctrl Pts',(-21.1927730322953,18.4925965155768,
7.39718696772576));
#132784=CARTESIAN_POINT('Ctrl Pts',(-21.214925712994,18.5796462112212,7.40165880957179));
#132785=CARTESIAN_POINT('Ctrl Pts',(-21.2370311427379,18.6665102326671,
7.40612111312312));
#132786=CARTESIAN_POINT('Ctrl Pts',(-21.2545997969947,18.7546518909174,
7.41058341667445));
#132787=CARTESIAN_POINT('Ctrl Pts',(-21.2674980351242,18.8435932689487,
7.41504572022578));
#132788=CARTESIAN_POINT('Ctrl Pts',(-21.2803582069864,18.9322721563795,
7.41949485428542));
#132789=CARTESIAN_POINT('Ctrl Pts',(-21.2885753721633,19.0217457093728,
7.42394398834505));
#132790=CARTESIAN_POINT('Ctrl Pts',(-21.292066600817,19.1115250494615,7.42839312240469));
#132791=CARTESIAN_POINT('Ctrl Pts',(-21.2933474798424,19.1444637323838,
7.43002544244541));
#132792=CARTESIAN_POINT('Ctrl Pts',(-21.2939927168566,19.1774434535922,
7.43165776248613));
#132793=CARTESIAN_POINT('Ctrl Pts',(-21.2939999386838,19.2104396975212,
7.43329008252684));
#132794=CARTESIAN_POINT('',(-21.2941234764334,19.2121301833364,7.36670989022851));
#132795=CARTESIAN_POINT('Ctrl Pts',(-17.174464231106,17.180864983421,7.08324142508076));
#132796=CARTESIAN_POINT('Ctrl Pts',(-17.2411541047993,17.1296342807345,
7.08741703658648));
#132797=CARTESIAN_POINT('Ctrl Pts',(-17.3103224735721,17.0817304249996,
7.09159264809219));
#132798=CARTESIAN_POINT('Ctrl Pts',(-17.3815968316152,17.0373841944486,
7.09576825959791));
#132799=CARTESIAN_POINT('Ctrl Pts',(-17.4557821871669,16.9912267688173,
7.10011441202498));
#132800=CARTESIAN_POINT('Ctrl Pts',(-17.5322487591342,16.9489240726657,
7.10446056445205));
#132801=CARTESIAN_POINT('Ctrl Pts',(-17.6105502686896,16.9106824781743,
7.10880671687912));
#132802=CARTESIAN_POINT('Ctrl Pts',(-17.688851778245,16.8724408836828,7.11315286930619));
#132803=CARTESIAN_POINT('Ctrl Pts',(-17.7689876871541,16.8382605409109,
7.11749902173325));
#132804=CARTESIAN_POINT('Ctrl Pts',(-17.8504927560597,16.8082900820313,
7.12184517416032));
#132805=CARTESIAN_POINT('Ctrl Pts',(-17.9289688151197,16.7794334289094,
7.12602980855337));
#132806=CARTESIAN_POINT('Ctrl Pts',(-18.0090061529611,16.7543718340009,
7.13021444294642));
#132807=CARTESIAN_POINT('Ctrl Pts',(-18.0902029058994,16.733274167381,7.13439907733947));
#132808=CARTESIAN_POINT('Ctrl Pts',(-18.17128408531,16.7122065306782,7.13857775542341));
#132809=CARTESIAN_POINT('Ctrl Pts',(-18.2535209603945,16.6950917298573,
7.14275643350736));
#132810=CARTESIAN_POINT('Ctrl Pts',(-18.3364934985375,16.6820499053372,
7.1469351115913));
#132811=CARTESIAN_POINT('Ctrl Pts',(-18.4209532597953,16.6687743154856,
7.15118868947673));
#132812=CARTESIAN_POINT('Ctrl Pts',(-18.5061748645252,16.6597193207395,
7.15544226736217));
#132813=CARTESIAN_POINT('Ctrl Pts',(-18.5917010358989,16.654957941501,7.1596958452476));
#132814=CARTESIAN_POINT('Ctrl Pts',(-18.6755691155499,16.6502888708901,
7.16386695922556));
#132815=CARTESIAN_POINT('Ctrl Pts',(-18.7597295775162,16.6497484479464,
7.16803807320351));
#132816=CARTESIAN_POINT('Ctrl Pts',(-18.8437446259188,16.6533534026215,
7.17220918718146));
#132817=CARTESIAN_POINT('Ctrl Pts',(-18.9277314822606,16.6569571476192,
7.17637890150183));
#132818=CARTESIAN_POINT('Ctrl Pts',(-19.0115725627189,16.6647034879404,
7.18054861582221));
#132819=CARTESIAN_POINT('Ctrl Pts',(-19.0948308836175,16.6765570486934,
7.18471833014258));
#132820=CARTESIAN_POINT('Ctrl Pts',(-19.1780862418277,16.6884101876458,
7.18888789608662));
#132821=CARTESIAN_POINT('Ctrl Pts',(-19.2607584263887,16.7043701907563,
7.19305746203066));
#132822=CARTESIAN_POINT('Ctrl Pts',(-19.3424177464726,16.7243500757491,
7.19722702797471));
#132823=CARTESIAN_POINT('Ctrl Pts',(-19.426948107513,16.7450324288504,7.20154319071363));
#132824=CARTESIAN_POINT('Ctrl Pts',(-19.5103925419324,16.7700224760727,
7.20585935345255));
#132825=CARTESIAN_POINT('Ctrl Pts',(-19.5922902863025,16.799167131736,7.21017551619147));
#132826=CARTESIAN_POINT('Ctrl Pts',(-19.6715202202638,16.8273624033065,
7.21435108038315));
#132827=CARTESIAN_POINT('Ctrl Pts',(-19.7493022661266,16.8594455439839,
7.21852664457483));
#132828=CARTESIAN_POINT('Ctrl Pts',(-19.8252402968867,16.8952291532946,
7.22270220876651));
#132829=CARTESIAN_POINT('Ctrl Pts',(-19.9050137770549,16.9328201076441,
7.22708867077905));
#132830=CARTESIAN_POINT('Ctrl Pts',(-19.982751549524,16.9744949002993,7.23147513279159));
#132831=CARTESIAN_POINT('Ctrl Pts',(-20.0580263707389,17.0199833023028,
7.23586159480413));
#132832=CARTESIAN_POINT('Ctrl Pts',(-20.1333011919539,17.0654717043063,
7.24024805681667));
#132833=CARTESIAN_POINT('Ctrl Pts',(-20.2061126241217,17.1147733273606,
7.24463451882921));
#132834=CARTESIAN_POINT('Ctrl Pts',(-20.2760730898188,17.1675689183003,
7.24902098084175));
#132835=CARTESIAN_POINT('Ctrl Pts',(-20.3421228419793,17.2174132934338,
7.25316224442401));
#132836=CARTESIAN_POINT('Ctrl Pts',(-20.4058887674611,17.270565700162,7.25730350800627));
#132837=CARTESIAN_POINT('Ctrl Pts',(-20.4670153688585,17.3267872383141,
7.26144477158854));
#132838=CARTESIAN_POINT('Ctrl Pts',(-20.5280546973635,17.3829285067286,
7.26558012252323));
#132839=CARTESIAN_POINT('Ctrl Pts',(-20.5864618395734,17.4421298917808,
7.26971547345792));
#132840=CARTESIAN_POINT('Ctrl Pts',(-20.6419120481561,17.5041105435615,
7.27385082439261));
#132841=CARTESIAN_POINT('Ctrl Pts',(-20.6972986881793,17.5660201402308,
7.27798143452815));
#132842=CARTESIAN_POINT('Ctrl Pts',(-20.7497348173451,17.6307023247237,
7.28211204466368));
#132843=CARTESIAN_POINT('Ctrl Pts',(-20.7989315869956,17.6978385608179,
7.28624265479922));
#132844=CARTESIAN_POINT('Ctrl Pts',(-20.8480980593209,17.7649334517507,
7.29037072114094));
#132845=CARTESIAN_POINT('Ctrl Pts',(-20.8940288533085,17.8344790168689,
7.29449878748265));
#132846=CARTESIAN_POINT('Ctrl Pts',(-20.9364753744698,17.9061236744987,
7.29862685382437));
#132847=CARTESIAN_POINT('Ctrl Pts',(-20.9789091334294,17.9777467910562,
7.30275367899922));
#132848=CARTESIAN_POINT('Ctrl Pts',(-21.0178604599825,18.0514673424199,
7.30688050417407));
#132849=CARTESIAN_POINT('Ctrl Pts',(-21.0531249145872,18.1269060785426,
7.31100732934892));
#132850=CARTESIAN_POINT('Ctrl Pts',(-21.0883898804923,18.2023459084539,
7.31513421435873));
#132851=CARTESIAN_POINT('Ctrl Pts',(-21.1199676712092,18.2795035453347,
7.31926109936855));
#132852=CARTESIAN_POINT('Ctrl Pts',(-21.147701166054,18.3579779129534,7.32338798437837));
#132853=CARTESIAN_POINT('Ctrl Pts',(-21.175460263615,18.4365247257135,7.32751867920249));
#132854=CARTESIAN_POINT('Ctrl Pts',(-21.1993678247307,18.5163902510463,
7.33164937402661));
#132855=CARTESIAN_POINT('Ctrl Pts',(-21.2193162430201,18.5971570459961,
7.33578006885072));
#132856=CARTESIAN_POINT('Ctrl Pts',(-21.2392749611598,18.6779655427927,
7.33991289645234));
#132857=CARTESIAN_POINT('Ctrl Pts',(-21.2552703785523,18.7596757735081,
7.34404572405396));
#132858=CARTESIAN_POINT('Ctrl Pts',(-21.267246258349,18.8418612800574,7.34817855165558));
#132859=CARTESIAN_POINT('Ctrl Pts',(-21.2792406903518,18.9241741027191,
7.35231778154839));
#132860=CARTESIAN_POINT('Ctrl Pts',(-21.2872031132021,19.0069632027568,
7.35645701144119));
#132861=CARTESIAN_POINT('Ctrl Pts',(-21.291129302603,19.0897988045891,7.360596241334));
#132862=CARTESIAN_POINT('Ctrl Pts',(-21.2930622985235,19.1305815748695,
7.36263412429883));
#132863=CARTESIAN_POINT('Ctrl Pts',(-21.2940177418851,19.1713756409973,
7.36467200726367));
#132864=CARTESIAN_POINT('Ctrl Pts',(-21.2939997505486,19.2121301287168,
7.36670989022851));
#132865=CARTESIAN_POINT('Ctrl Pts',(-21.2976211331247,19.2121317273999,
7.36670989022851));
#132866=CARTESIAN_POINT('Ctrl Pts',(-21.2979709119767,19.2754624155768,
7.36987218932674));
#132867=CARTESIAN_POINT('Ctrl Pts',(-21.2671018166522,20.1874206516717,
7.41542642398545));
#132868=CARTESIAN_POINT('Ctrl Pts',(-20.178486706887,21.871216118483,7.50337259420462));
#132869=CARTESIAN_POINT('Ctrl Pts',(-17.2790524902644,21.8655092554602,
7.63054840088606));
#132870=CARTESIAN_POINT('Ctrl Pts',(-15.7210162867422,19.4347114151187,
7.75718985667495));
#132871=CARTESIAN_POINT('Ctrl Pts',(-16.5081485987195,17.6886843918709,
7.84143937690338));
#132872=CARTESIAN_POINT('Ctrl Pts',(-17.171894433272,17.1775280041615,7.88329696157133));
#132873=CARTESIAN_POINT('Origin',(-18.734,19.211,-1.76670989022852));
#132874=CARTESIAN_POINT('',(-17.174464231106,17.180864983421,8.74981199461744));
#132875=CARTESIAN_POINT('',(-17.174464231106,17.180864983421,8.68337762993461));
#132876=CARTESIAN_POINT('',(-17.174464231106,17.180864983421,-1.76670989022852));
#132877=CARTESIAN_POINT('',(-21.2939989173812,19.2133543591349,8.2332901225083));
#132878=CARTESIAN_POINT('Ctrl Pts',(-21.2939989173812,19.2133543591349,
8.2332901225083));
#132879=CARTESIAN_POINT('Ctrl Pts',(-21.2938985191577,19.3225217922602,
8.2387181286671));
#132880=CARTESIAN_POINT('Ctrl Pts',(-21.2868114603045,19.4313771443117,
8.2441461348259));
#132881=CARTESIAN_POINT('Ctrl Pts',(-21.2728791636074,19.5391654957492,
8.2495741409847));
#132882=CARTESIAN_POINT('Ctrl Pts',(-21.2596700733155,19.6413587017587,
8.2547203867915));
#132883=CARTESIAN_POINT('Ctrl Pts',(-21.2403084403105,19.7425933354651,
8.2598666325983));
#132884=CARTESIAN_POINT('Ctrl Pts',(-21.2149532278239,19.84224565848,8.26501287840509));
#132885=CARTESIAN_POINT('Ctrl Pts',(-21.1943358111288,19.9232772597465,
8.26919751279814));
#132886=CARTESIAN_POINT('Ctrl Pts',(-21.1697059337058,20.0034485022604,
8.27338214719119));
#132887=CARTESIAN_POINT('Ctrl Pts',(-21.1411517779373,20.0823324956486,
8.27756678158424));
#132888=CARTESIAN_POINT('Ctrl Pts',(-21.1126382654752,20.1611042074361,
8.28174545966818));
#132889=CARTESIAN_POINT('Ctrl Pts',(-21.0802117249137,20.2385918806366,
8.28592413775212));
#132890=CARTESIAN_POINT('Ctrl Pts',(-21.04401079686,20.3143812207891,8.29010281583607));
#132891=CARTESIAN_POINT('Ctrl Pts',(-21.0071609931882,20.391529030395,8.2943563937215));
#132892=CARTESIAN_POINT('Ctrl Pts',(-20.9664002781982,20.466916555597,8.29860997160694));
#132893=CARTESIAN_POINT('Ctrl Pts',(-20.9219272181894,20.5401254598066,
8.30286354949238));
#132894=CARTESIAN_POINT('Ctrl Pts',(-20.8783163552309,20.6119150665525,
8.30703466347033));
#132895=CARTESIAN_POINT('Ctrl Pts',(-20.8311360546878,20.6816093608382,
8.31120577744828));
#132896=CARTESIAN_POINT('Ctrl Pts',(-20.7806202689677,20.7488379221005,
8.31537689142623));
#132897=CARTESIAN_POINT('Ctrl Pts',(-20.7301214343075,20.8160439241698,
8.3195466057466));
#132898=CARTESIAN_POINT('Ctrl Pts',(-20.6762896134471,20.880785468974,8.32371632006697));
#132899=CARTESIAN_POINT('Ctrl Pts',(-20.6194012584855,20.9427222913912,
8.32788603438734));
#132900=CARTESIAN_POINT('Ctrl Pts',(-20.5625149278558,21.0046569098304,
8.33205560033138));
#132901=CARTESIAN_POINT('Ctrl Pts',(-20.5025725911955,21.0637866660878,
8.33622516627542));
#132902=CARTESIAN_POINT('Ctrl Pts',(-20.4398891227943,21.1198065121253,
8.34039473221946));
#132903=CARTESIAN_POINT('Ctrl Pts',(-20.3750017809724,21.1777959468417,
8.34471089495838));
#132904=CARTESIAN_POINT('Ctrl Pts',(-20.3071773578721,21.2324523620815,
8.3490270576973));
#132905=CARTESIAN_POINT('Ctrl Pts',(-20.2368028123899,21.2834824986168,
8.35334322043622));
#132906=CARTESIAN_POINT('Ctrl Pts',(-20.1687207103247,21.3328503338218,
8.3575187846279));
#132907=CARTESIAN_POINT('Ctrl Pts',(-20.0982524952706,21.3788242964684,
8.36169434881958));
#132908=CARTESIAN_POINT('Ctrl Pts',(-20.0257768405867,21.4211838371782,
8.36586991301126));
#132909=CARTESIAN_POINT('Ctrl Pts',(-19.949640612879,21.4656828575891,8.37025637502381));
#132910=CARTESIAN_POINT('Ctrl Pts',(-19.8712893431909,21.5061924632349,
8.37464283703635));
#132911=CARTESIAN_POINT('Ctrl Pts',(-19.7911876038236,21.5425133219267,
8.3790292990489));
#132912=CARTESIAN_POINT('Ctrl Pts',(-19.7110858644562,21.5788341806186,
8.38341576106144));
#132913=CARTESIAN_POINT('Ctrl Pts',(-19.6292342232969,21.6109661511407,
8.38780222307398));
#132914=CARTESIAN_POINT('Ctrl Pts',(-19.5461152252309,21.638770347654,8.39218868508653));
#132915=CARTESIAN_POINT('Ctrl Pts',(-19.4668206554779,21.66529523187,8.39637331947957));
#132916=CARTESIAN_POINT('Ctrl Pts',(-19.3860776423915,21.6879805757247,
8.40055795387262));
#132917=CARTESIAN_POINT('Ctrl Pts',(-19.3042928646695,21.7066694589843,
8.40474258826567));
#132918=CARTESIAN_POINT('Ctrl Pts',(-19.2226244974556,21.7253317409318,
8.40892126634962));
#132919=CARTESIAN_POINT('Ctrl Pts',(-19.1399177555961,21.7400087597643,
8.41309994443356));
#132920=CARTESIAN_POINT('Ctrl Pts',(-19.0565960387004,21.7505928405583,
8.41727862251751));
#132921=CARTESIAN_POINT('Ctrl Pts',(-18.9717808399116,21.7613666333938,
8.42153220040294));
#132922=CARTESIAN_POINT('Ctrl Pts',(-18.8863288596153,21.7678991601646,
8.42578577828838));
#132923=CARTESIAN_POINT('Ctrl Pts',(-18.8006993328509,21.7701309460434,
8.43003935617382));
#132924=CARTESIAN_POINT('Ctrl Pts',(-18.7167299015551,21.7723194643981,
8.43421047015177));
#132925=CARTESIAN_POINT('Ctrl Pts',(-18.6325902275832,21.7703724977257,
8.43838158412972));
#132926=CARTESIAN_POINT('Ctrl Pts',(-18.5487184100094,21.7642862613523,
8.44255269810767));
#132927=CARTESIAN_POINT('Ctrl Pts',(-18.4648747364341,21.7582020672743,
8.44672241242804));
#132928=CARTESIAN_POINT('Ctrl Pts',(-18.3812991991948,21.7479813952831,
8.45089212674842));
#132929=CARTESIAN_POINT('Ctrl Pts',(-18.2984275456889,21.7336725187874,
8.45506184106879));
#132930=CARTESIAN_POINT('Ctrl Pts',(-18.2155588411121,21.719364151463,8.45923140701283));
#132931=CARTESIAN_POINT('Ctrl Pts',(-18.1333944236485,21.7009679479898,
8.46340097295687));
#132932=CARTESIAN_POINT('Ctrl Pts',(-18.0523612259042,21.6785835510979,
8.46757053890091));
#132933=CARTESIAN_POINT('Ctrl Pts',(-17.9684790008924,21.6554121464255,
8.47188670163983));
#132934=CARTESIAN_POINT('Ctrl Pts',(-17.8858095314087,21.6279670209743,
8.47620286437875));
#132935=CARTESIAN_POINT('Ctrl Pts',(-17.8048088555661,21.5964148102805,
8.48051902711767));
#132936=CARTESIAN_POINT('Ctrl Pts',(-17.7264467682192,21.5658904095313,
8.48469459130935));
#132937=CARTESIAN_POINT('Ctrl Pts',(-17.6496468328974,21.5315226265231,
8.48887015550103));
#132938=CARTESIAN_POINT('Ctrl Pts',(-17.5747994654322,21.4935104864288,
8.49304571969271));
#132939=CARTESIAN_POINT('Ctrl Pts',(-17.496171735369,21.4535784435037,8.49743218170525));
#132940=CARTESIAN_POINT('Ctrl Pts',(-17.4196995115722,21.4096245062639,
8.5018186437178));
#132941=CARTESIAN_POINT('Ctrl Pts',(-17.3458018650431,21.3619314117614,
8.50620510573034));
#132942=CARTESIAN_POINT('Ctrl Pts',(-17.2719042185139,21.314238317259,8.51059156774288));
#132943=CARTESIAN_POINT('Ctrl Pts',(-17.200581575379,21.2628064665597,8.51497802975541));
#132944=CARTESIAN_POINT('Ctrl Pts',(-17.1322119090443,21.2079664272772,
8.51936449176795));
#132945=CARTESIAN_POINT('Ctrl Pts',(-17.0669880324057,21.1556496594946,
8.523549126161));
#132946=CARTESIAN_POINT('Ctrl Pts',(-17.004208586686,21.1000367097147,8.52773376055405));
#132947=CARTESIAN_POINT('Ctrl Pts',(-16.9442256444347,21.0413845924179,
8.5319183949471));
#132948=CARTESIAN_POINT('Ctrl Pts',(-16.8843280804773,20.9828159591503,
8.53609707303104));
#132949=CARTESIAN_POINT('Ctrl Pts',(-16.8272194396166,20.9212170697946,
8.54027575111499));
#132950=CARTESIAN_POINT('Ctrl Pts',(-16.7732194376017,20.8568856540237,
8.54445442919893));
#132951=CARTESIAN_POINT('Ctrl Pts',(-16.7182515243598,20.7914011438592,
8.54870800708437));
#132952=CARTESIAN_POINT('Ctrl Pts',(-16.6665051669309,20.7230854843409,
8.5529615849698));
#132953=CARTESIAN_POINT('Ctrl Pts',(-16.6182789494494,20.6522926268656,
8.55721516285524));
#132954=CARTESIAN_POINT('Ctrl Pts',(-16.5709876912995,20.5828722270732,
8.56138627683319));
#132955=CARTESIAN_POINT('Ctrl Pts',(-16.527081572471,20.5110702205223,8.56555739081114));
#132956=CARTESIAN_POINT('Ctrl Pts',(-16.4868009099953,20.4372529306314,
8.56972850478909));
#132957=CARTESIAN_POINT('Ctrl Pts',(-16.446533764085,20.363460410845,8.57389821910947));
#132958=CARTESIAN_POINT('Ctrl Pts',(-16.4098898786011,20.2876543542439,
8.57806793342984));
#132959=CARTESIAN_POINT('Ctrl Pts',(-16.3770645250476,20.2102272849111,
8.58223764775021));
#132960=CARTESIAN_POINT('Ctrl Pts',(-16.3442403395611,20.1328029707657,
8.58640721369426));
#132961=CARTESIAN_POINT('Ctrl Pts',(-16.3152345946181,20.0537581824513,
8.5905767796383));
#132962=CARTESIAN_POINT('Ctrl Pts',(-16.2901945969737,19.973505837446,8.59474634558234));
#132963=CARTESIAN_POINT('Ctrl Pts',(-16.2642742239022,19.8904319189922,
8.59906250832126));
#132964=CARTESIAN_POINT('Ctrl Pts',(-16.2426038152404,19.8060644520148,
8.60337867106019));
#132965=CARTESIAN_POINT('Ctrl Pts',(-16.225290101654,19.7208770890524,8.60769483379911));
#132966=CARTESIAN_POINT('Ctrl Pts',(-16.2085403804666,19.6384646954784,
8.61187039799079));
#132967=CARTESIAN_POINT('Ctrl Pts',(-16.1958678987932,19.5552854746203,
8.61604596218246));
#132968=CARTESIAN_POINT('Ctrl Pts',(-16.1873166326445,19.471775432959,8.62022152637414));
#132969=CARTESIAN_POINT('Ctrl Pts',(-16.1783334623714,19.3840474976197,
8.62460798838669));
#132970=CARTESIAN_POINT('Ctrl Pts',(-16.173898803398,19.2959550268228,8.62899445039923));
#132971=CARTESIAN_POINT('Ctrl Pts',(-16.1740017537922,19.2080034331647,
8.63338091241177));
#132972=CARTESIAN_POINT('Ctrl Pts',(-16.1741047041864,19.1200518395067,
8.63776737442431));
#132973=CARTESIAN_POINT('Ctrl Pts',(-16.1787451573697,19.0322416983818,
8.64215383643685));
#132974=CARTESIAN_POINT('Ctrl Pts',(-16.1878497481281,18.9450697555886,
8.64654029844939));
#132975=CARTESIAN_POINT('Ctrl Pts',(-16.1967810779015,18.8595567008307,
8.65084328578973));
#132976=CARTESIAN_POINT('Ctrl Pts',(-16.2100422563569,18.7743304265415,
8.65514627313006));
#132977=CARTESIAN_POINT('Ctrl Pts',(-16.2276047148296,18.6898640537483,
8.6594492604704));
#132978=CARTESIAN_POINT('Ctrl Pts',(-16.2446561859346,18.6078552668085,
8.66362705052256));
#132979=CARTESIAN_POINT('Ctrl Pts',(-16.2657620106882,18.526563267255,8.66780484057472));
#132980=CARTESIAN_POINT('Ctrl Pts',(-16.2908434939132,18.4464175735962,
8.67198263062689));
#132981=CARTESIAN_POINT('Ctrl Pts',(-16.3159003387464,18.3663506097709,
8.67615631669416));
#132982=CARTESIAN_POINT('Ctrl Pts',(-16.3449249508829,18.2874281524481,
8.68033000276144));
#132983=CARTESIAN_POINT('Ctrl Pts',(-16.3777879155978,18.2100681275347,
8.68450368882872));
#132984=CARTESIAN_POINT('Ctrl Pts',(-16.4106284573715,18.1327608866383,
8.68867452712137));
#132985=CARTESIAN_POINT('Ctrl Pts',(-16.4473019700395,18.0570143826501,
8.69284536541402));
#132986=CARTESIAN_POINT('Ctrl Pts',(-16.4876301165927,17.9832287074049,
8.69701620370667));
#132987=CARTESIAN_POINT('Ctrl Pts',(-16.5279428446235,17.9094712423847,
8.70118544737697));
#132988=CARTESIAN_POINT('Ctrl Pts',(-16.5719072084086,17.8376735188971,
8.70535469104727));
#132989=CARTESIAN_POINT('Ctrl Pts',(-16.6192985302658,17.7682118333227,
8.70952393471757));
#132990=CARTESIAN_POINT('Ctrl Pts',(-16.666700849621,17.6987340286633,8.71369414589093));
#132991=CARTESIAN_POINT('Ctrl Pts',(-16.7175314608585,17.6315937280806,
8.71786435706428));
#132992=CARTESIAN_POINT('Ctrl Pts',(-16.7715224094598,17.5671381728906,
8.72203456823764));
#132993=CARTESIAN_POINT('Ctrl Pts',(-16.8255216994708,17.5026726595463,
8.72620542369381));
#132994=CARTESIAN_POINT('Ctrl Pts',(-16.8826819940177,17.4408930619735,
8.73037627914997));
#132995=CARTESIAN_POINT('Ctrl Pts',(-16.9426963407412,17.3821120317728,
8.73454713460613));
#132996=CARTESIAN_POINT('Ctrl Pts',(-17.0027604759684,17.3232822362403,
8.73872145024579));
#132997=CARTESIAN_POINT('Ctrl Pts',(-17.0656830493498,17.2674562830652,
8.74289576588546));
#132998=CARTESIAN_POINT('Ctrl Pts',(-17.1311223695951,17.2149079926147,
8.74707008152512));
#132999=CARTESIAN_POINT('Ctrl Pts',(-17.145450381212,17.2034024862433,8.74798405255589));
#133000=CARTESIAN_POINT('Ctrl Pts',(-17.1598989273243,17.1920539496951,
8.74889802358666));
#133001=CARTESIAN_POINT('Ctrl Pts',(-17.174464231106,17.180864983421,8.74981199461743));
#133002=CARTESIAN_POINT('Ctrl Pts',(-17.1770150831773,17.1841768308936,
7.94987222090926));
#133003=CARTESIAN_POINT('Ctrl Pts',(-17.5010449670934,16.9346419658738,
7.97013523562024));
#133004=CARTESIAN_POINT('Ctrl Pts',(-18.6774627144846,16.3911012243001,
8.03279018589171));
#133005=CARTESIAN_POINT('Ctrl Pts',(-20.7208250384235,17.0720883649514,
8.12726281551246));
#133006=CARTESIAN_POINT('Ctrl Pts',(-21.28776986438,18.5735386239974,8.20147243042222));
#133007=CARTESIAN_POINT('Ctrl Pts',(-21.2935817164968,19.2133537193276,
8.23329010977151));
#133008=CARTESIAN_POINT('',(-21.2939989424941,19.2086731074563,8.16670989022852));
#133009=CARTESIAN_POINT('Ctrl Pts',(-17.171894433272,17.1775280041615,7.88329696157133));
#133010=CARTESIAN_POINT('Ctrl Pts',(-17.1803677644956,17.1710026187585,
7.88383131246386));
#133011=CARTESIAN_POINT('Ctrl Pts',(-17.8646300971893,16.6514603543991,
7.92675759891687));
#133012=CARTESIAN_POINT('Ctrl Pts',(-19.7898863352068,16.3740305446598,
8.01207582093035));
#133013=CARTESIAN_POINT('Ctrl Pts',(-21.194097770004,17.9910561083639,8.10601244625689));
#133014=CARTESIAN_POINT('Ctrl Pts',(-21.29615524784,19.0247813417565,8.15755713602294));
#133015=CARTESIAN_POINT('Ctrl Pts',(-21.2944497293802,19.2086726977168,
8.16670989022852));
#133016=CARTESIAN_POINT('Ctrl Pts',(-21.2939989424941,19.2086731074563,
8.16670989022852));
#133017=CARTESIAN_POINT('Ctrl Pts',(-21.294074804776,19.2921352174732,8.17086478789788));
#133018=CARTESIAN_POINT('Ctrl Pts',(-21.2900646933588,19.3757219830021,
8.17501968556724));
#133019=CARTESIAN_POINT('Ctrl Pts',(-21.2819596922617,19.458994771335,8.17917458323661));
#133020=CARTESIAN_POINT('Ctrl Pts',(-21.2739328413916,19.5414646248839,
8.18328941845664));
#133021=CARTESIAN_POINT('Ctrl Pts',(-21.2618897634889,19.6236260477268,
8.18740425367667));
#133022=CARTESIAN_POINT('Ctrl Pts',(-21.2458740550218,19.7050533692914,
8.1915190888967));
#133023=CARTESIAN_POINT('Ctrl Pts',(-21.229865310909,19.7864452825742,8.19563213480029));
#133024=CARTESIAN_POINT('Ctrl Pts',(-21.2098874553345,19.867103263636,8.19974518070388));
#133025=CARTESIAN_POINT('Ctrl Pts',(-21.1860355605652,19.9466096857189,
8.20385822660747));
#133026=CARTESIAN_POINT('Ctrl Pts',(-21.1621864189586,20.0261069305809,
8.2079707977528));
#133027=CARTESIAN_POINT('Ctrl Pts',(-21.1344642632168,20.1044524267967,
8.21208336889812));
#133028=CARTESIAN_POINT('Ctrl Pts',(-21.1030141994638,20.1812431255818,
8.21619594004345));
#133029=CARTESIAN_POINT('Ctrl Pts',(-21.0710029255604,20.2594041147406,
8.2203818978976));
#133030=CARTESIAN_POINT('Ctrl Pts',(-21.0351295718013,20.3359537977659,
8.22456785575175));
#133031=CARTESIAN_POINT('Ctrl Pts',(-20.9955977974884,20.4104896424712,
8.22875381360589));
#133032=CARTESIAN_POINT('Ctrl Pts',(-20.9567081892514,20.4838147044139,
8.23287177349699));
#133033=CARTESIAN_POINT('Ctrl Pts',(-20.9142784405329,20.5551904907364,
8.23698973338808));
#133034=CARTESIAN_POINT('Ctrl Pts',(-20.8685472200438,20.624261534679,8.24110769327918));
#133035=CARTESIAN_POINT('Ctrl Pts',(-20.8216832918827,20.6950433858241,
8.24532765011485));
#133036=CARTESIAN_POINT('Ctrl Pts',(-20.7713524862058,20.7634043768936,
8.24954760695052));
#133037=CARTESIAN_POINT('Ctrl Pts',(-20.7178552814756,20.8289982145112,
8.2537675637862));
#133038=CARTESIAN_POINT('Ctrl Pts',(-20.6643580767454,20.8945920521287,
8.25798752062187));
#133039=CARTESIAN_POINT('Ctrl Pts',(-20.6076948817588,20.9574183953714,
8.26220747745755));
#133040=CARTESIAN_POINT('Ctrl Pts',(-20.5482046419776,21.0171731691692,
8.26642743429322));
#133041=CARTESIAN_POINT('Ctrl Pts',(-20.4892123552949,21.0764277756309,
8.27061206868627));
#133042=CARTESIAN_POINT('Ctrl Pts',(-20.4272042190729,21.1328994502154,
8.27479670307932));
#133043=CARTESIAN_POINT('Ctrl Pts',(-20.3624734272384,21.1862656268913,
8.27898133747237));
#133044=CARTESIAN_POINT('Ctrl Pts',(-20.297834771674,21.2395558434202,8.28316001555632));
#133045=CARTESIAN_POINT('Ctrl Pts',(-20.2304815101079,21.2897490519969,
8.28733869364026));
#133046=CARTESIAN_POINT('Ctrl Pts',(-20.1607438576393,21.3365592122283,
8.29151737172421));
#133047=CARTESIAN_POINT('Ctrl Pts',(-20.0897562078699,21.3842084109399,
8.29577094960965));
#133048=CARTESIAN_POINT('Ctrl Pts',(-20.0162981861696,21.4283517444168,
8.30002452749508));
#133049=CARTESIAN_POINT('Ctrl Pts',(-19.9407536469186,21.4687301954947,
8.30427810538052));
#133050=CARTESIAN_POINT('Ctrl Pts',(-19.866673685974,21.5083258315064,8.30844921935847));
#133051=CARTESIAN_POINT('Ctrl Pts',(-19.7905878123474,21.5443010347692,
8.31262033333642));
#133052=CARTESIAN_POINT('Ctrl Pts',(-19.7128859499198,21.5764560442015,
8.31679144731437));
#133053=CARTESIAN_POINT('Ctrl Pts',(-19.6352101611025,21.6086002637099,
8.32096116163474));
#133054=CARTESIAN_POINT('Ctrl Pts',(-19.555919885142,21.6369266595076,8.32513087595511));
#133055=CARTESIAN_POINT('Ctrl Pts',(-19.4754262787738,21.6612830598002,
8.32930059027549));
#133056=CARTESIAN_POINT('Ctrl Pts',(-19.3949355367136,21.6856385933875,
8.33347015621952));
#133057=CARTESIAN_POINT('Ctrl Pts',(-19.3132419899458,21.7060242799308,
8.33763972216356));
#133058=CARTESIAN_POINT('Ctrl Pts',(-19.2307719418924,21.7223378183248,
8.3418092881076));
#133059=CARTESIAN_POINT('Ctrl Pts',(-19.145402348687,21.7392249206038,8.34612545084652));
#133060=CARTESIAN_POINT('Ctrl Pts',(-19.0592011520728,21.7517480910506,
8.35044161358545));
#133061=CARTESIAN_POINT('Ctrl Pts',(-18.9726507026519,21.7598518674344,
8.35475777632437));
#133062=CARTESIAN_POINT('Ctrl Pts',(-18.8889196250174,21.7676916641548,
8.35893334051605));
#133063=CARTESIAN_POINT('Ctrl Pts',(-18.8048621716343,21.7713955951849,
8.36310890470773));
#133064=CARTESIAN_POINT('Ctrl Pts',(-18.7209165514645,21.770966566847,8.36728446889941));
#133065=CARTESIAN_POINT('Ctrl Pts',(-18.6327310375816,21.7705158693076,
8.37167093091195));
#133066=CARTESIAN_POINT('Ctrl Pts',(-18.5446695341431,21.7655037616187,
8.37605739292449));
#133067=CARTESIAN_POINT('Ctrl Pts',(-18.4572333890564,21.7559951361578,
8.38044385493703));
#133068=CARTESIAN_POINT('Ctrl Pts',(-18.3697972439697,21.7464865106968,
8.38483031694958));
#133069=CARTESIAN_POINT('Ctrl Pts',(-18.2829870179306,21.7324815349687,
8.38921677896212));
#133070=CARTESIAN_POINT('Ctrl Pts',(-18.1972887614195,21.7141062794818,
8.39360324097466));
#133071=CARTESIAN_POINT('Ctrl Pts',(-18.1155336087259,21.6965764967386,
8.39778787536772));
#133072=CARTESIAN_POINT('Ctrl Pts',(-18.034486039177,21.6750045135588,8.40197250976076));
#133073=CARTESIAN_POINT('Ctrl Pts',(-17.9545759800696,21.649462260761,8.40615714415381));
#133074=CARTESIAN_POINT('Ctrl Pts',(-17.8747796630406,21.6239563641985,
8.41033582223775));
#133075=CARTESIAN_POINT('Ctrl Pts',(-17.7961180748451,21.5944915619193,
8.41451450032169));
#133076=CARTESIAN_POINT('Ctrl Pts',(-17.7190104693571,21.5611906843244,
8.41869317840563));
#133077=CARTESIAN_POINT('Ctrl Pts',(-17.6405207654569,21.5272929124315,
8.42294675629106));
#133078=CARTESIAN_POINT('Ctrl Pts',(-17.5636417739319,21.4894202903321,
8.4272003341765));
#133079=CARTESIAN_POINT('Ctrl Pts',(-17.4887990603227,21.4477553777351,
8.43145391206194));
#133080=CARTESIAN_POINT('Ctrl Pts',(-17.4154073187604,21.4068982207712,
8.43562502603989));
#133081=CARTESIAN_POINT('Ctrl Pts',(-17.3439740257043,21.3623947371042,
8.43979614001785));
#133082=CARTESIAN_POINT('Ctrl Pts',(-17.2748782070125,21.3144646641265,
8.4439672539958));
#133083=CARTESIAN_POINT('Ctrl Pts',(-17.2058055740901,21.2665506745478,
8.44813696831618));
#133084=CARTESIAN_POINT('Ctrl Pts',(-17.1390692354552,21.2152126412159,
8.45230668263655));
#133085=CARTESIAN_POINT('Ctrl Pts',(-17.0750196948479,21.1607139141724,
8.45647639695692));
#133086=CARTESIAN_POINT('Ctrl Pts',(-17.0109724333982,21.1062171264274,
8.46064596290096));
#133087=CARTESIAN_POINT('Ctrl Pts',(-16.9496121296953,21.0485601673606,
8.464815528845));
#133088=CARTESIAN_POINT('Ctrl Pts',(-16.8912555527362,20.9880461170376,
8.46898509478904));
#133089=CARTESIAN_POINT('Ctrl Pts',(-16.8308472305218,20.9254044673573,
8.47330125752796));
#133090=CARTESIAN_POINT('Ctrl Pts',(-16.7736581532185,20.859701457282,8.47761742026688));
#133091=CARTESIAN_POINT('Ctrl Pts',(-16.7199960430177,20.7913126466809,
8.4819335830058));
#133092=CARTESIAN_POINT('Ctrl Pts',(-16.6680819704125,20.7251515943919,
8.48610914719748));
#133093=CARTESIAN_POINT('Ctrl Pts',(-16.6194688453354,20.6564774460931,
8.49028471138916));
#133094=CARTESIAN_POINT('Ctrl Pts',(-16.5743914182291,20.5856602393105,
8.49446027558084));
#133095=CARTESIAN_POINT('Ctrl Pts',(-16.527037237441,20.5112662237653,8.49884673759338));
#133096=CARTESIAN_POINT('Ctrl Pts',(-16.4835856052314,20.4345074765787,
8.50323319960592));
#133097=CARTESIAN_POINT('Ctrl Pts',(-16.4442533274937,20.3558406770141,
8.50761966161846));
#133098=CARTESIAN_POINT('Ctrl Pts',(-16.4049210497559,20.2771738774495,
8.51200612363101));
#133099=CARTESIAN_POINT('Ctrl Pts',(-16.369708289139,20.1965995876304,8.51639258564355));
#133100=CARTESIAN_POINT('Ctrl Pts',(-16.3387721302028,20.1145947386671,
8.52077904765609));
#133101=CARTESIAN_POINT('Ctrl Pts',(-16.3092593897977,20.0363630543649,
8.52496368204914));
#133102=CARTESIAN_POINT('Ctrl Pts',(-16.2835285016034,19.9565383690801,
8.52914831644219));
#133103=CARTESIAN_POINT('Ctrl Pts',(-16.2617516946766,19.8755211184195,
8.53333295083523));
#133104=CARTESIAN_POINT('Ctrl Pts',(-16.240005884339,19.7946191857874,8.53751162891917));
#133105=CARTESIAN_POINT('Ctrl Pts',(-16.2222030943946,19.7125284999517,
8.54169030700311));
#133106=CARTESIAN_POINT('Ctrl Pts',(-16.2084669780845,19.6296680728384,
8.54586898508705));
#133107=CARTESIAN_POINT('Ctrl Pts',(-16.1944846517615,19.5453224321197,
8.55012256297248));
#133108=CARTESIAN_POINT('Ctrl Pts',(-16.1847163934877,19.4601796345801,
8.55437614085792));
#133109=CARTESIAN_POINT('Ctrl Pts',(-16.179239049994,19.3746963295997,8.55862971874336));
#133110=CARTESIAN_POINT('Ctrl Pts',(-16.1738678954921,19.2908702852934,
8.56280083272131));
#133111=CARTESIAN_POINT('Ctrl Pts',(-16.1726227957354,19.2067172987634,
8.56697194669926));
#133112=CARTESIAN_POINT('Ctrl Pts',(-16.1755241458591,19.1226750104571,
8.57114306067721));
#133113=CARTESIAN_POINT('Ctrl Pts',(-16.1784245224067,19.0386609233523,
8.57531277499758));
#133114=CARTESIAN_POINT('Ctrl Pts',(-16.1854685696705,18.9547579200753,
8.57948248931794));
#133115=CARTESIAN_POINT('Ctrl Pts',(-16.1966245729685,18.8714032651857,
8.58365220363831));
#133116=CARTESIAN_POINT('Ctrl Pts',(-16.207780179288,18.7880515764123,8.58782176958235));
#133117=CARTESIAN_POINT('Ctrl Pts',(-16.2230473888474,18.7052486530845,
8.5919913355264));
#133118=CARTESIAN_POINT('Ctrl Pts',(-16.242342820325,18.6234248992902,8.59616090147044));
#133119=CARTESIAN_POINT('Ctrl Pts',(-16.2623166553699,18.538724323253,8.60047706420936));
#133120=CARTESIAN_POINT('Ctrl Pts',(-16.2866071262488,18.455073566411,8.60479322694829));
#133121=CARTESIAN_POINT('Ctrl Pts',(-16.3150650107312,18.3729346578631,
8.60910938968721));
#133122=CARTESIAN_POINT('Ctrl Pts',(-16.3425958826198,18.2934714156217,
8.6132849538789));
#133123=CARTESIAN_POINT('Ctrl Pts',(-16.3740266108361,18.2154234566597,
8.61746051807058));
#133124=CARTESIAN_POINT('Ctrl Pts',(-16.4091731183427,18.1391884632439,
8.62163608226227));
#133125=CARTESIAN_POINT('Ctrl Pts',(-16.4460947923905,18.059103021542,8.62602254427481));
#133126=CARTESIAN_POINT('Ctrl Pts',(-16.4871172070497,17.9810190212164,
8.63040900628735));
#133127=CARTESIAN_POINT('Ctrl Pts',(-16.5319737202488,17.9053659535363,
8.6347954682999));
#133128=CARTESIAN_POINT('Ctrl Pts',(-16.576830233448,17.8297128858562,8.63918193031244));
#133129=CARTESIAN_POINT('Ctrl Pts',(-16.6255204605689,17.7564911918507,
8.64356839232499));
#133130=CARTESIAN_POINT('Ctrl Pts',(-16.677728404917,17.6860911085397,8.64795485433754));
#133131=CARTESIAN_POINT('Ctrl Pts',(-16.7275305668981,17.6189351153988,
8.6521391847953));
#133132=CARTESIAN_POINT('Ctrl Pts',(-16.7807187430267,17.5540964632713,
8.65632351525307));
#133133=CARTESIAN_POINT('Ctrl Pts',(-16.8370495093169,17.491936639941,8.66050784571084));
#133134=CARTESIAN_POINT('Ctrl Pts',(-16.8932939076247,17.4298721218744,
8.66468576063046));
#133135=CARTESIAN_POINT('Ctrl Pts',(-16.952671014844,17.3704786082901,8.66886367555008));
#133136=CARTESIAN_POINT('Ctrl Pts',(-17.0148956024391,17.3140866993226,
8.6730415904697));
#133137=CARTESIAN_POINT('Ctrl Pts',(-17.0662095397694,17.2675827208387,
8.67648693695801));
#133138=CARTESIAN_POINT('Ctrl Pts',(-17.1194590718192,17.2231195687963,
8.67993228344631));
#133139=CARTESIAN_POINT('Ctrl Pts',(-17.174464231106,17.180864983421,8.68337762993461));
#133140=CARTESIAN_POINT('Origin',(-18.734,19.211,-1.76670989022852));
#133141=CARTESIAN_POINT('',(-17.1725834074896,17.1783793283469,9.54996332099649));
#133142=CARTESIAN_POINT('',(-17.174464231106,17.180864983421,9.48328065598191));
#133143=CARTESIAN_POINT('',(-17.174464231106,17.180864983421,-1.76670989022852));
#133144=CARTESIAN_POINT('',(-21.2943302600992,19.210357489227,9.03329016591285));
#133145=CARTESIAN_POINT('Ctrl Pts',(-21.2980344970333,19.2103691601534,
9.03329079544681));
#133146=CARTESIAN_POINT('Ctrl Pts',(-21.2952860334465,20.0241271385548,
9.07394170535625));
#133147=CARTESIAN_POINT('Ctrl Pts',(-20.4360629396139,21.691476034616,9.15698455082618));
#133148=CARTESIAN_POINT('Ctrl Pts',(-17.5947352470201,22.0155262669008,
9.28241933185656));
#133149=CARTESIAN_POINT('Ctrl Pts',(-15.7591748325173,19.7710955115256,
9.40959513853801));
#133150=CARTESIAN_POINT('Ctrl Pts',(-16.3858468785065,17.8368644049063,
9.49877646825131));
#133151=CARTESIAN_POINT('Ctrl Pts',(-17.1023021432777,17.2315279292858,
9.54556586240414));
#133152=CARTESIAN_POINT('Ctrl Pts',(-17.1725834074896,17.1783793283469,
9.54996332099649));
#133153=CARTESIAN_POINT('Ctrl Pts',(-17.174464231106,17.180864983421,8.74981199461743));
#133154=CARTESIAN_POINT('Ctrl Pts',(-17.2411338659978,17.1296498280428,
8.75399550605232));
#133155=CARTESIAN_POINT('Ctrl Pts',(-17.3102517202361,17.0817815881081,
8.7581790174872));
#133156=CARTESIAN_POINT('Ctrl Pts',(-17.3814398259537,17.0374818897502,
8.76236252892209));
#133157=CARTESIAN_POINT('Ctrl Pts',(-17.4458386446654,16.9974071017674,
8.766147054325));
#133158=CARTESIAN_POINT('Ctrl Pts',(-17.5119310943407,16.9602521707291,
8.76993157972792));
#133159=CARTESIAN_POINT('Ctrl Pts',(-17.5794224113971,16.926147577655,8.77371610513083));
#133160=CARTESIAN_POINT('Ctrl Pts',(-17.6540490703618,16.8884373662162,
8.77790073952388));
#133161=CARTESIAN_POINT('Ctrl Pts',(-17.730664056125,16.8543169479217,8.78208537391692));
#133162=CARTESIAN_POINT('Ctrl Pts',(-17.8088876493305,16.8240003898956,
8.78627000830997));
#133163=CARTESIAN_POINT('Ctrl Pts',(-17.8869999009332,16.7937269837373,
8.79044868639392));
#133164=CARTESIAN_POINT('Ctrl Pts',(-17.9667157867297,16.7672468481168,
8.79462736447786));
#133165=CARTESIAN_POINT('Ctrl Pts',(-18.0476319224909,16.7447277396491,
8.79880604256181));
#133166=CARTESIAN_POINT('Ctrl Pts',(-18.1299984218322,16.7218049923463,
8.80305962044724));
#133167=CARTESIAN_POINT('Ctrl Pts',(-18.213608193011,16.7029868892008,8.80731319833267));
#133168=CARTESIAN_POINT('Ctrl Pts',(-18.2980154243377,16.6883986740302,
8.81156677621811));
#133169=CARTESIAN_POINT('Ctrl Pts',(-18.380786256778,16.6740932798773,8.81573789019606));
#133170=CARTESIAN_POINT('Ctrl Pts',(-18.4643234304655,16.6638553099794,
8.81990900417401));
#133171=CARTESIAN_POINT('Ctrl Pts',(-18.5481939962223,16.6577518473599,
8.82408011815197));
#133172=CARTESIAN_POINT('Ctrl Pts',(-18.6320364184008,16.6516504328163,
8.82824983247234));
#133173=CARTESIAN_POINT('Ctrl Pts',(-18.7162115520294,16.6496808035662,
8.83241954679271));
#133174=CARTESIAN_POINT('Ctrl Pts',(-18.8002812486104,16.6518581914863,
8.83658926111308));
#133175=CARTESIAN_POINT('Ctrl Pts',(-18.8843479536308,16.6540355019256,
8.84075882705713));
#133176=CARTESIAN_POINT('Ctrl Pts',(-18.9683087692067,16.660359523368,8.84492839300117));
#133177=CARTESIAN_POINT('Ctrl Pts',(-19.0517268423097,16.6707933836643,
8.84909795894522));
#133178=CARTESIAN_POINT('Ctrl Pts',(-19.1380777919556,16.681594085617,8.85341412168414));
#133179=CARTESIAN_POINT('Ctrl Pts',(-19.2238466000237,16.6967989420232,
8.85773028442306));
#133180=CARTESIAN_POINT('Ctrl Pts',(-19.3085579282895,16.7163089996876,
8.86204644716198));
#133181=CARTESIAN_POINT('Ctrl Pts',(-19.3905097939472,16.7351835192757,
8.86622201135366));
#133182=CARTESIAN_POINT('Ctrl Pts',(-19.4714715762059,16.758086889941,8.87039757554534));
#133183=CARTESIAN_POINT('Ctrl Pts',(-19.551028186959,16.7848786218092,8.87457313973702));
#133184=CARTESIAN_POINT('Ctrl Pts',(-19.6346030129933,16.8130235403628,
8.87895960174956));
#133185=CARTESIAN_POINT('Ctrl Pts',(-19.716626443602,16.8454597306831,8.8833460637621));
#133186=CARTESIAN_POINT('Ctrl Pts',(-19.7966429339306,16.8819680133224,
8.88773252577464));
#133187=CARTESIAN_POINT('Ctrl Pts',(-19.8766594242591,16.9184762959617,
8.89211898778718));
#133188=CARTESIAN_POINT('Ctrl Pts',(-19.9546684946739,16.959056335675,8.89650544979972));
#133189=CARTESIAN_POINT('Ctrl Pts',(-20.0302483510423,17.003435683288,8.90089191181226));
#133190=CARTESIAN_POINT('Ctrl Pts',(-20.102350666183,17.0457730713314,8.90507654620531));
#133191=CARTESIAN_POINT('Ctrl Pts',(-20.1725107769709,17.0917254144961,
8.90926118059836));
#133192=CARTESIAN_POINT('Ctrl Pts',(-20.240343151946,17.1410892993693,8.91344581499141));
#133193=CARTESIAN_POINT('Ctrl Pts',(-20.3080789759311,17.1903829208624,
8.91762449307535));
#133194=CARTESIAN_POINT('Ctrl Pts',(-20.373493276466,17.243078170329,8.9218031711593));
#133195=CARTESIAN_POINT('Ctrl Pts',(-20.4362266525528,17.2989266689431,
8.92598184924324));
#133196=CARTESIAN_POINT('Ctrl Pts',(-20.5000844793203,17.3557762117573,
8.93023542712868));
#133197=CARTESIAN_POINT('Ctrl Pts',(-20.5611639093906,17.4158929154665,
8.93448900501411));
#133198=CARTESIAN_POINT('Ctrl Pts',(-20.6191183231213,17.4789697150938,
8.93874258289955));
#133199=CARTESIAN_POINT('Ctrl Pts',(-20.6759491774531,17.5408236478761,
8.9429136968775));
#133200=CARTESIAN_POINT('Ctrl Pts',(-20.7297747776526,17.6055235719756,
8.94708481085545));
#133201=CARTESIAN_POINT('Ctrl Pts',(-20.7803043703348,17.6727417564177,
8.9512559248334));
#133202=CARTESIAN_POINT('Ctrl Pts',(-20.8308170073241,17.7399373851488,
8.95542563915377));
#133203=CARTESIAN_POINT('Ctrl Pts',(-20.8780355571482,17.8096492285708,
8.95959535347414));
#133204=CARTESIAN_POINT('Ctrl Pts',(-20.9217100507379,17.8815171178612,
8.96376506779451));
#133205=CARTESIAN_POINT('Ctrl Pts',(-20.9653829902017,17.9533824497836,
8.96793463373855));
#133206=CARTESIAN_POINT('Ctrl Pts',(-21.0055118859952,18.0274032814579,
8.9721041996826));
#133207=CARTESIAN_POINT('Ctrl Pts',(-21.0418912815019,18.1031923304257,
8.97627376562664));
#133208=CARTESIAN_POINT('Ctrl Pts',(-21.0795497316758,18.1816460288594,
8.98058992836556));
#133209=CARTESIAN_POINT('Ctrl Pts',(-21.1131898827321,18.2619941236263,
8.98490609110448));
#133210=CARTESIAN_POINT('Ctrl Pts',(-21.1426376470828,18.3437833690158,
8.9892222538434));
#133211=CARTESIAN_POINT('Ctrl Pts',(-21.171126153607,18.4229083383394,8.99339781803508));
#133212=CARTESIAN_POINT('Ctrl Pts',(-21.1956911205896,18.5033815448835,
8.99757338222676));
#133213=CARTESIAN_POINT('Ctrl Pts',(-21.2162259984621,18.5847779207351,
9.00174894641844));
#133214=CARTESIAN_POINT('Ctrl Pts',(-21.2377980441989,18.6702854340294,
9.00613540843098));
#133215=CARTESIAN_POINT('Ctrl Pts',(-21.254922068569,18.7568112533014,9.01052187044352));
#133216=CARTESIAN_POINT('Ctrl Pts',(-21.2675357890124,18.8438536997419,
9.01490833245606));
#133217=CARTESIAN_POINT('Ctrl Pts',(-21.2801495094559,18.9308961461825,
9.01929479446861));
#133218=CARTESIAN_POINT('Ctrl Pts',(-21.288252948244,19.0184546350337,9.02368125648114));
#133219=CARTESIAN_POINT('Ctrl Pts',(-21.2918468828523,19.10602703261,9.02806771849369));
#133220=CARTESIAN_POINT('Ctrl Pts',(-21.2932731600888,19.1407807303868,
9.02980851558629));
#133221=CARTESIAN_POINT('Ctrl Pts',(-21.2939911726516,19.1755636940745,
9.0315493126789));
#133222=CARTESIAN_POINT('Ctrl Pts',(-21.2939999191096,19.2103564484228,
9.0332901097715));
#133223=CARTESIAN_POINT('',(-21.293999998394,19.2110906788005,8.96670989026365));
#133224=CARTESIAN_POINT('Ctrl Pts',(-17.174464231106,17.180864983421,8.68337762993461));
#133225=CARTESIAN_POINT('Ctrl Pts',(-17.2410629602576,17.1297042973452,
8.68754916039799));
#133226=CARTESIAN_POINT('Ctrl Pts',(-17.3102360430907,17.0817825735557,
8.69172069086136));
#133227=CARTESIAN_POINT('Ctrl Pts',(-17.3816325649282,17.0373619619271,
8.69589222132474));
#133228=CARTESIAN_POINT('Ctrl Pts',(-17.4530009748456,16.9929588406279,
8.70006210927489));
#133229=CARTESIAN_POINT('Ctrl Pts',(-17.526590695086,16.952054336701,8.70423199722505));
#133230=CARTESIAN_POINT('Ctrl Pts',(-17.6020218660579,16.9148672720688,
8.70840188517521));
#133231=CARTESIAN_POINT('Ctrl Pts',(-17.6774459640613,16.8776836943628,
8.71257138212671));
#133232=CARTESIAN_POINT('Ctrl Pts',(-17.7547107568408,16.844217066174,8.71674087907822));
#133233=CARTESIAN_POINT('Ctrl Pts',(-17.8334130523661,16.8146396035338,
8.72091037602972));
#133234=CARTESIAN_POINT('Ctrl Pts',(-17.9121315766146,16.7850560419044,
8.72508073274792));
#133235=CARTESIAN_POINT('Ctrl Pts',(-17.9922877611872,16.7593633988364,
8.72925108946611));
#133236=CARTESIAN_POINT('Ctrl Pts',(-18.0734610672701,16.7376847515232,
8.7334214461843));
#133237=CARTESIAN_POINT('Ctrl Pts',(-18.1547254427102,16.7159817826617,
8.73759648167837));
#133238=CARTESIAN_POINT('Ctrl Pts',(-18.2370087716157,16.6983019143779,
8.74177151717243));
#133239=CARTESIAN_POINT('Ctrl Pts',(-18.3198786279348,16.684717456578,8.7459465526665));
#133240=CARTESIAN_POINT('Ctrl Pts',(-18.4028029852764,16.6711240646871,
8.75012433395637));
#133241=CARTESIAN_POINT('Ctrl Pts',(-18.4863141811532,16.6616314953346,
8.75430211524624));
#133242=CARTESIAN_POINT('Ctrl Pts',(-18.5699753170643,16.6562601104246,
8.75847989653611));
#133243=CARTESIAN_POINT('Ctrl Pts',(-18.6537710890963,16.6508800813285,
8.76266440114214));
#133244=CARTESIAN_POINT('Ctrl Pts',(-18.7377168237858,16.6496344772215,
8.76684890574817));
#133245=CARTESIAN_POINT('Ctrl Pts',(-18.8213768080935,16.6524915881695,
8.77103341035419));
#133246=CARTESIAN_POINT('Ctrl Pts',(-18.8486819858539,16.6534240999667,
8.77239916057579));
#133247=CARTESIAN_POINT('Ctrl Pts',(-18.8759567793247,16.6547932460373,
8.77376491079738));
#133248=CARTESIAN_POINT('Ctrl Pts',(-18.903186241511,16.6565967398073,8.77513066101897));
#133249=CARTESIAN_POINT('Ctrl Pts',(-18.9866168294529,16.6621226126484,
8.77931529541202));
#133250=CARTESIAN_POINT('Ctrl Pts',(-19.0699316687707,16.6717505167587,
8.78349992980507));
#133251=CARTESIAN_POINT('Ctrl Pts',(-19.1526949496535,16.6854714337124,
8.78768456419812));
#133252=CARTESIAN_POINT('Ctrl Pts',(-19.23534042725,16.6991728206392,8.79186324228206));
#133253=CARTESIAN_POINT('Ctrl Pts',(-19.3174354558612,16.7169555737484,
8.79604192036601));
#133254=CARTESIAN_POINT('Ctrl Pts',(-19.3985474281628,16.7387587666811,
8.80022059844996));
#133255=CARTESIAN_POINT('Ctrl Pts',(-19.4811132742737,16.7609527661774,
8.8044741763354));
#133256=CARTESIAN_POINT('Ctrl Pts',(-19.5626599937769,16.7873127240843,
8.80872775422083));
#133257=CARTESIAN_POINT('Ctrl Pts',(-19.6427400986364,16.8177195247673,
8.81298133210626));
#133258=CARTESIAN_POINT('Ctrl Pts',(-19.7212676943998,16.847536830285,8.81715244608422));
#133259=CARTESIAN_POINT('Ctrl Pts',(-19.7983845845479,16.8812452961239,
8.82132356006216));
#133260=CARTESIAN_POINT('Ctrl Pts',(-19.8736839568168,16.9186822910917,
8.82549467404011));
#133261=CARTESIAN_POINT('Ctrl Pts',(-19.9489580616541,16.9561067237144,
8.82966438836048));
#133262=CARTESIAN_POINT('Ctrl Pts',(-20.0224154482673,16.9972569960432,
8.83383410268086));
#133263=CARTESIAN_POINT('Ctrl Pts',(-20.0936712215606,17.0419231988563,
8.83800381700123));
#133264=CARTESIAN_POINT('Ctrl Pts',(-20.1649244592674,17.086587812254,8.84217338294525));
#133265=CARTESIAN_POINT('Ctrl Pts',(-20.2339758500889,17.1347678623259,
8.84634294888928));
#133266=CARTESIAN_POINT('Ctrl Pts',(-20.3004681352879,17.186209250039,8.85051251483331));
#133267=CARTESIAN_POINT('Ctrl Pts',(-20.3692982072077,17.2394592534845,
8.85482867757223));
#133268=CARTESIAN_POINT('Ctrl Pts',(-20.4353854517824,17.2962038761398,
8.85914484031115));
#133269=CARTESIAN_POINT('Ctrl Pts',(-20.4983710832762,17.3561159927104,
8.86346100305008));
#133270=CARTESIAN_POINT('Ctrl Pts',(-20.5593049644491,17.4140764783854,
8.86763656724176));
#133271=CARTESIAN_POINT('Ctrl Pts',(-20.6173359087925,17.4750008911685,
8.87181213143345));
#133272=CARTESIAN_POINT('Ctrl Pts',(-20.6721781340604,17.5385570202096,
8.87598769562513));
#133273=CARTESIAN_POINT('Ctrl Pts',(-20.7297903097516,17.6053232182383,
8.88037415763768));
#133274=CARTESIAN_POINT('Ctrl Pts',(-20.7838828183067,17.6749935141293,
8.88476061965022));
#133275=CARTESIAN_POINT('Ctrl Pts',(-20.8341751072843,17.7471473712346,
8.88914708166276));
#133276=CARTESIAN_POINT('Ctrl Pts',(-20.8844673962619,17.8193012283399,
8.89353354367531));
#133277=CARTESIAN_POINT('Ctrl Pts',(-20.930959223453,17.8939381139567,8.89792000568785));
#133278=CARTESIAN_POINT('Ctrl Pts',(-20.9734262024012,17.9706088181549,
8.9023064677004));
#133279=CARTESIAN_POINT('Ctrl Pts',(-21.0159038253685,18.047298739271,8.90669402914565));
#133280=CARTESIAN_POINT('Ctrl Pts',(-21.054500797719,18.1262856298352,8.91108159059091));
#133281=CARTESIAN_POINT('Ctrl Pts',(-21.0889748257326,18.2071605854691,
8.91546915203617));
#133282=CARTESIAN_POINT('Ctrl Pts',(-21.1233545067053,18.2878142059939,
8.91984470579149));
#133283=CARTESIAN_POINT('Ctrl Pts',(-21.1536335666927,18.3703452363822,
8.92422025954681));
#133284=CARTESIAN_POINT('Ctrl Pts',(-21.1796158858341,18.4543211123894,
8.92859581330213));
#133285=CARTESIAN_POINT('Ctrl Pts',(-21.2055560013422,18.5381605845955,
8.93296425975244));
#133286=CARTESIAN_POINT('Ctrl Pts',(-21.2272131436812,18.6234398583861,
8.93733270620275));
#133287=CARTESIAN_POINT('Ctrl Pts',(-21.2444392039475,18.7097066694204,
8.94170115265306));
#133288=CARTESIAN_POINT('Ctrl Pts',(-21.2616295048393,18.7957944002037,
8.94606053069714));
#133289=CARTESIAN_POINT('Ctrl Pts',(-21.274406969619,18.8828651985172,8.95041990874123));
#133290=CARTESIAN_POINT('Ctrl Pts',(-21.2826736357252,18.9704533339265,
8.95477928678531));
#133291=CARTESIAN_POINT('Ctrl Pts',(-21.2902149496553,19.0503561166423,
8.95875615459971));
#133292=CARTESIAN_POINT('Ctrl Pts',(-21.2940028463113,19.1306890276033,
8.96273302241411));
#133293=CARTESIAN_POINT('Ctrl Pts',(-21.293999998394,19.2110906780901,8.96670989022851));
#133294=CARTESIAN_POINT('Ctrl Pts',(-21.293999998394,19.2110906788005,8.96670989026365));
#133295=CARTESIAN_POINT('Ctrl Pts',(-21.2939968622716,19.2996281672638,
8.97108917708311));
#133296=CARTESIAN_POINT('Ctrl Pts',(-21.2893963356695,19.3880718027693,
8.97546846390256));
#133297=CARTESIAN_POINT('Ctrl Pts',(-21.2802532223815,19.4759424985004,
8.97984775072202));
#133298=CARTESIAN_POINT('Ctrl Pts',(-21.2710840473103,19.5640636632957,
8.98423952038189));
#133299=CARTESIAN_POINT('Ctrl Pts',(-21.2573464424813,19.6516082364874,
8.98863129004176));
#133300=CARTESIAN_POINT('Ctrl Pts',(-21.2391468026208,19.7381048257401,
8.99302305970162));
#133301=CARTESIAN_POINT('Ctrl Pts',(-21.2209205771356,19.824727767266,8.99742124475988));
#133302=CARTESIAN_POINT('Ctrl Pts',(-21.1982194166657,19.9102992971048,
9.00181942981815));
#133303=CARTESIAN_POINT('Ctrl Pts',(-21.1711995861977,19.9943633748381,
9.00621761487641));
#133304=CARTESIAN_POINT('Ctrl Pts',(-21.1441046030879,20.0786612674182,
9.01062803299537));
#133305=CARTESIAN_POINT('Ctrl Pts',(-21.1126670698914,20.1614429605725,
9.01503845111432));
#133306=CARTESIAN_POINT('Ctrl Pts',(-21.0770917883153,20.2422714829421,
9.01944886923327));
#133307=CARTESIAN_POINT('Ctrl Pts',(-21.0501146625114,20.3035646370618,
9.02279333761612));
#133308=CARTESIAN_POINT('Ctrl Pts',(-21.0207591774505,20.3637350853212,
9.02613780599898));
#133309=CARTESIAN_POINT('Ctrl Pts',(-20.989131617054,20.4226028184861,9.02948227438183));
#133310=CARTESIAN_POINT('Ctrl Pts',(-20.9495588772781,20.4962587519987,
9.03366690877488));
#133311=CARTESIAN_POINT('Ctrl Pts',(-20.9063001320242,20.5681109610611,
9.03785154316793));
#133312=CARTESIAN_POINT('Ctrl Pts',(-20.8595440286337,20.6377664778581,
9.04203617756098));
#133313=CARTESIAN_POINT('Ctrl Pts',(-20.8128544767691,20.7073228486487,
9.04621485564492));
#133314=CARTESIAN_POINT('Ctrl Pts',(-20.7626777089519,20.7746883591287,
9.05039353372887));
#133315=CARTESIAN_POINT('Ctrl Pts',(-20.7092482964898,20.8394944480145,
9.05457221181281));
#133316=CARTESIAN_POINT('Ctrl Pts',(-20.6548612002085,20.9054621394682,
9.05882578969825));
#133317=CARTESIAN_POINT('Ctrl Pts',(-20.5971039332158,20.9687773268415,
9.06307936758368));
#133318=CARTESIAN_POINT('Ctrl Pts',(-20.5362701954423,21.0290819955712,
9.06733294546912));
#133319=CARTESIAN_POINT('Ctrl Pts',(-20.4766158383828,21.0882175406228,
9.07150405944707));
#133320=CARTESIAN_POINT('Ctrl Pts',(-20.4140035745828,21.1444579161298,
9.07567517342502));
#133321=CARTESIAN_POINT('Ctrl Pts',(-20.3487498736145,21.1975001499275,
9.07984628740298));
#133322=CARTESIAN_POINT('Ctrl Pts',(-20.2835180691556,21.2505245848914,
9.08401600172335));
#133323=CARTESIAN_POINT('Ctrl Pts',(-20.2156469445306,21.3003527195436,
9.08818571604372));
#133324=CARTESIAN_POINT('Ctrl Pts',(-20.1454869304126,21.3467211066229,
9.0923554303641));
#133325=CARTESIAN_POINT('Ctrl Pts',(-20.0753294128889,21.3930878437159,
9.09652499630814));
#133326=CARTESIAN_POINT('Ctrl Pts',(-20.0028835520723,21.4359948250819,
9.10069456225219));
#133327=CARTESIAN_POINT('Ctrl Pts',(-19.92852856073,21.4752220557181,9.10486412819624));
#133328=CARTESIAN_POINT('Ctrl Pts',(-19.851559339619,21.5158284673914,9.10918029093516));
#133329=CARTESIAN_POINT('Ctrl Pts',(-19.7725447065604,21.5524913076845,
9.11349645367408));
#133330=CARTESIAN_POINT('Ctrl Pts',(-19.6919309796754,21.585019426664,9.117812616413));
#133331=CARTESIAN_POINT('Ctrl Pts',(-19.6139432364646,21.6164879455891,
9.12198818060468));
#133332=CARTESIAN_POINT('Ctrl Pts',(-19.5344594409714,21.6440868736177,
9.12616374479635));
#133333=CARTESIAN_POINT('Ctrl Pts',(-19.4539003149002,21.6676936187906,
9.13033930898803));
#133334=CARTESIAN_POINT('Ctrl Pts',(-19.3692723388823,21.6924926845425,
9.13472577100057));
#133335=CARTESIAN_POINT('Ctrl Pts',(-19.2834581156083,21.7128855434687,
9.13911223301312));
#133336=CARTESIAN_POINT('Ctrl Pts',(-19.1969566012277,21.7287909336122,
9.14349869502565));
#133337=CARTESIAN_POINT('Ctrl Pts',(-19.110455086847,21.7446963237556,9.14788515703819));
#133338=CARTESIAN_POINT('Ctrl Pts',(-19.0232668665414,21.756114245197,9.15227161905073));
#133339=CARTESIAN_POINT('Ctrl Pts',(-18.9358937423135,21.7630264334083,
9.15665808106326));
#133340=CARTESIAN_POINT('Ctrl Pts',(-18.8525407850492,21.7696205815937,
9.16084271545631));
#133341=CARTESIAN_POINT('Ctrl Pts',(-18.7687093097474,21.7721390606606,
9.16502734984936));
#133342=CARTESIAN_POINT('Ctrl Pts',(-18.68483185138,21.7705277871438,9.16921198424241));
#133343=CARTESIAN_POINT('Ctrl Pts',(-18.6010737821926,21.7689188070754,
9.17339066232635));
#133344=CARTESIAN_POINT('Ctrl Pts',(-18.5172703159603,21.7631917591217,
9.1775693404103));
#133345=CARTESIAN_POINT('Ctrl Pts',(-18.4338583233966,21.7533443853982,
9.18174801849424));
#133346=CARTESIAN_POINT('Ctrl Pts',(-18.3489512308133,21.7433205045778,
9.18600159637968));
#133347=CARTESIAN_POINT('Ctrl Pts',(-18.2644502649081,21.7290270933803,
9.19025517426511));
#133348=CARTESIAN_POINT('Ctrl Pts',(-18.1808154334733,21.7105173204754,
9.19450875215055));
#133349=CARTESIAN_POINT('Ctrl Pts',(-18.0988020264459,21.6923663956372,
9.1986798661285));
#133350=CARTESIAN_POINT('Ctrl Pts',(-18.0176219400175,21.6701612389658,
9.20285098010646));
#133351=CARTESIAN_POINT('Ctrl Pts',(-17.9377012248092,21.6440039582026,
9.20702209408441));
#133352=CARTESIAN_POINT('Ctrl Pts',(-17.8578073277689,21.6178554547676,
9.21119180840478));
#133353=CARTESIAN_POINT('Ctrl Pts',(-17.7791723995178,21.5877576040183,
9.21536152272516));
#133354=CARTESIAN_POINT('Ctrl Pts',(-17.7022076389883,21.5538624636879,
9.21953123704553));
#133355=CARTESIAN_POINT('Ctrl Pts',(-17.6252456171953,21.5199685294921,
9.22370080298958));
#133356=CARTESIAN_POINT('Ctrl Pts',(-17.549954065628,21.4822777605696,9.22787036893362));
#133357=CARTESIAN_POINT('Ctrl Pts',(-17.4767232259472,21.4409899357233,
9.23203993487766));
#133358=CARTESIAN_POINT('Ctrl Pts',(-17.4009176802832,21.3982504818895,
9.23635609761658));
#133359=CARTESIAN_POINT('Ctrl Pts',(-17.3273209113734,21.3516565799089,
9.24067226035551));
#133360=CARTESIAN_POINT('Ctrl Pts',(-17.2563352295955,21.3014800468565,
9.24498842309443));
#133361=CARTESIAN_POINT('Ctrl Pts',(-17.1876618989351,21.2529380090907,
9.24916398728611));
#133362=CARTESIAN_POINT('Ctrl Pts',(-17.121432497117,21.201043491951,9.25333955147779));
#133363=CARTESIAN_POINT('Ctrl Pts',(-17.0579778332573,21.146083899108,9.25751511566947));
#133364=CARTESIAN_POINT('Ctrl Pts',(-16.9913182251752,21.0883484278846,
9.26190157768201));
#133365=CARTESIAN_POINT('Ctrl Pts',(-16.9277214465954,21.027230514262,9.26628803969455));
#133366=CARTESIAN_POINT('Ctrl Pts',(-16.867525901464,20.9631057158443,9.27067450170709));
#133367=CARTESIAN_POINT('Ctrl Pts',(-16.8073303563327,20.8989809174267,
9.27506096371963));
#133368=CARTESIAN_POINT('Ctrl Pts',(-16.7505363613297,20.8318497263028,
9.27944742573217));
#133369=CARTESIAN_POINT('Ctrl Pts',(-16.6974308899393,20.7621241923026,
9.28383388774471));
#133370=CARTESIAN_POINT('Ctrl Pts',(-16.6467688800087,20.6956068334797,
9.28801852213775));
#133371=CARTESIAN_POINT('Ctrl Pts',(-16.5992748500802,20.6264810343216,
9.2922031565308));
#133372=CARTESIAN_POINT('Ctrl Pts',(-16.5552283987657,20.5550812139358,
9.29638779092385));
#133373=CARTESIAN_POINT('Ctrl Pts',(-16.5112446421229,20.4837830223567,
9.30056646900779));
#133374=CARTESIAN_POINT('Ctrl Pts',(-16.4706989563139,20.4102176270061,
9.30474514709174));
#133375=CARTESIAN_POINT('Ctrl Pts',(-16.4338297096935,20.3347511448677,
9.30892382517568));
#133376=CARTESIAN_POINT('Ctrl Pts',(-16.396299608325,20.2579319802738,9.31317740306112));
#133377=CARTESIAN_POINT('Ctrl Pts',(-16.3625793350038,20.17914328813,9.31743098094655));
#133378=CARTESIAN_POINT('Ctrl Pts',(-16.3328731767862,20.0988006413846,
9.32168455883199));
#133379=CARTESIAN_POINT('Ctrl Pts',(-16.3037429304124,20.0200155936222,
9.32585567280994));
#133380=CARTESIAN_POINT('Ctrl Pts',(-16.2784727120491,19.939736757811,9.33002678678789));
#133381=CARTESIAN_POINT('Ctrl Pts',(-16.2572072783656,19.8583776440833,
9.33419790076584));
#133382=CARTESIAN_POINT('Ctrl Pts',(-16.2359489805037,19.7770458311919,
9.33836761508621));
#133383=CARTESIAN_POINT('Ctrl Pts',(-16.2186929146628,19.6946349050202,
9.34253732940659));
#133384=CARTESIAN_POINT('Ctrl Pts',(-16.2055337985359,19.6115729247638,
9.34670704372696));
#133385=CARTESIAN_POINT('Ctrl Pts',(-16.1923751506668,19.528513900209,9.350876609671));
#133386=CARTESIAN_POINT('Ctrl Pts',(-16.1833132337911,19.4448043221315,
9.35504617561504));
#133387=CARTESIAN_POINT('Ctrl Pts',(-16.1783912959603,19.3608804584879,
9.35921574155909));
#133388=CARTESIAN_POINT('Ctrl Pts',(-16.1732963088673,19.2740059353298,
9.36353190429801));
#133389=CARTESIAN_POINT('Ctrl Pts',(-16.1726378716504,19.1869023041989,
9.36784806703693));
#133390=CARTESIAN_POINT('Ctrl Pts',(-16.1764051921425,19.1000549738833,
9.37216422977585));
#133391=CARTESIAN_POINT('Ctrl Pts',(-16.1800497925657,19.016036686218,9.37633979396753));
#133392=CARTESIAN_POINT('Ctrl Pts',(-16.1878361499306,18.9322587224488,
9.38051535815921));
#133393=CARTESIAN_POINT('Ctrl Pts',(-16.1997016639331,18.8491548068462,
9.38469092235089));
#133394=CARTESIAN_POINT('Ctrl Pts',(-16.2121664768403,18.7618535100274,
9.38907738436343));
#133395=CARTESIAN_POINT('Ctrl Pts',(-16.2291332400404,18.6752967161991,
9.39346384637597));
#133396=CARTESIAN_POINT('Ctrl Pts',(-16.2504693406595,18.5899722517346,
9.39785030838852));
#133397=CARTESIAN_POINT('Ctrl Pts',(-16.2718054412786,18.5046477872702,
9.40223677040106));
#133398=CARTESIAN_POINT('Ctrl Pts',(-16.2975106369606,18.4205561848056,
9.4066232324136));
#133399=CARTESIAN_POINT('Ctrl Pts',(-16.3273937923111,18.3381617783842,
9.41100969442614));
#133400=CARTESIAN_POINT('Ctrl Pts',(-16.3558995253308,18.2595652271093,
9.41519396859545));
#133401=CARTESIAN_POINT('Ctrl Pts',(-16.3883126378428,18.1822203306847,
9.41937824276476));
#133402=CARTESIAN_POINT('Ctrl Pts',(-16.4245033134286,18.1065430951298,
9.42356251693406));
#133403=CARTESIAN_POINT('Ctrl Pts',(-16.4606449439981,18.0309684161363,
9.42774112064292));
#133404=CARTESIAN_POINT('Ctrl Pts',(-16.5005537757522,17.9570573217751,
9.43191972435178));
#133405=CARTESIAN_POINT('Ctrl Pts',(-16.5440510006764,17.8852083948216,
9.43609832806064));
#133406=CARTESIAN_POINT('Ctrl Pts',(-16.5874980215117,17.8134423952254,
9.44027210886431));
#133407=CARTESIAN_POINT('Ctrl Pts',(-16.6345249665165,17.7437342236777,
9.44444588966797));
#133408=CARTESIAN_POINT('Ctrl Pts',(-16.6849066106035,17.6764589345568,
9.44861967047164));
#133409=CARTESIAN_POINT('Ctrl Pts',(-16.7352537172963,17.6092297636844,
9.45279059008417));
#133410=CARTESIAN_POINT('Ctrl Pts',(-16.7889506803249,17.5444305296909,
9.45696150969671));
#133411=CARTESIAN_POINT('Ctrl Pts',(-16.8457290001088,17.4824073264734,
9.46113242930925));
#133412=CARTESIAN_POINT('Ctrl Pts',(-16.9024956626441,17.4203968573399,
9.46530249258354));
#133413=CARTESIAN_POINT('Ctrl Pts',(-16.9623421216396,17.3611616320101,
9.46947255585784));
#133414=CARTESIAN_POINT('Ctrl Pts',(-17.0249603576165,17.3050137721479,
9.47364261913213));
#133415=CARTESIAN_POINT('Ctrl Pts',(-17.073202380668,17.2617566233716,9.47685529808206));
#133416=CARTESIAN_POINT('Ctrl Pts',(-17.1230887135075,17.2203313029939,
9.48006797703199));
#133417=CARTESIAN_POINT('Ctrl Pts',(-17.174464231106,17.180864983421,9.48328065598192));
#133418=CARTESIAN_POINT('Origin',(-18.734,19.211,-1.76670989022852));
#133419=CARTESIAN_POINT('',(-17.174464231106,17.180864983421,10.3499274761209));
#133420=CARTESIAN_POINT('',(-17.174464231106,17.180864983421,10.283238218494));
#133421=CARTESIAN_POINT('',(-17.174464231106,17.180864983421,-1.76670989022852));
#133422=CARTESIAN_POINT('',(-21.2939992159918,19.2089964727374,9.8332901097715));
#133423=CARTESIAN_POINT('Ctrl Pts',(-21.2939992159918,19.2089964727374,
9.8332901097715));
#133424=CARTESIAN_POINT('Ctrl Pts',(-21.2940649620946,19.2930033015151,
9.83745593779552));
#133425=CARTESIAN_POINT('Ctrl Pts',(-21.2899913508454,19.3770604200798,
9.84162176581953));
#133426=CARTESIAN_POINT('Ctrl Pts',(-21.281790209728,19.4607299485725,9.84578759384355));
#133427=CARTESIAN_POINT('Ctrl Pts',(-21.2735905258927,19.544384609609,9.84995268163075));
#133428=CARTESIAN_POINT('Ctrl Pts',(-21.2612648140692,19.6276513592372,
9.85411776941795));
#133429=CARTESIAN_POINT('Ctrl Pts',(-21.2448768408732,19.7100966739687,
9.85828285720515));
#133430=CARTESIAN_POINT('Ctrl Pts',(-21.2284868533627,19.7925521223993,
9.86244845694073));
#133431=CARTESIAN_POINT('Ctrl Pts',(-21.2080337038204,19.8741854840197,
9.86661405667632));
#133432=CARTESIAN_POINT('Ctrl Pts',(-21.183632148948,19.9545740278144,9.8707796564119));
#133433=CARTESIAN_POINT('Ctrl Pts',(-21.159203008195,20.0350534506039,9.87494996534483));
#133434=CARTESIAN_POINT('Ctrl Pts',(-21.1308166833999,20.114284804087,9.87912027427776));
#133435=CARTESIAN_POINT('Ctrl Pts',(-21.0986375209739,20.1918615572049,
9.88329058321069));
#133436=CARTESIAN_POINT('Ctrl Pts',(-21.066439637101,20.2694834435379,9.88746331837884));
#133437=CARTESIAN_POINT('Ctrl Pts',(-21.0304447198545,20.3454483968716,
9.89163605354698));
#133438=CARTESIAN_POINT('Ctrl Pts',(-20.9908638255709,20.4193731513193,
9.89580878871513));
#133439=CARTESIAN_POINT('Ctrl Pts',(-20.9512104382913,20.4934333000532,
9.89998916630974));
#133440=CARTESIAN_POINT('Ctrl Pts',(-20.907958193034,20.5654453913561,9.90416954390436));
#133441=CARTESIAN_POINT('Ctrl Pts',(-20.8613622504221,20.6350540212643,
9.90834992149897));
#133442=CARTESIAN_POINT('Ctrl Pts',(-20.8243993123263,20.6902721225411,
9.91166606942056));
#133443=CARTESIAN_POINT('Ctrl Pts',(-20.7853331875374,20.7439783287845,
9.91498221734216));
#133444=CARTESIAN_POINT('Ctrl Pts',(-20.7443085775785,20.7960108589263,
9.91829836526375));
#133445=CARTESIAN_POINT('Ctrl Pts',(-20.6925397790042,20.8616705099241,
9.9224829996568));
#133446=CARTESIAN_POINT('Ctrl Pts',(-20.6374544461771,20.9249134154189,
9.92666763404984));
#133447=CARTESIAN_POINT('Ctrl Pts',(-20.5793066365797,20.9853853631595,
9.93085226844289));
#133448=CARTESIAN_POINT('Ctrl Pts',(-20.5212415931921,21.0457712365674,
9.93503094652683));
#133449=CARTESIAN_POINT('Ctrl Pts',(-20.4601230476226,21.1033936577093,
9.93920962461076));
#133450=CARTESIAN_POINT('Ctrl Pts',(-20.3962460420505,21.1579304290825,
9.9433883026947));
#133451=CARTESIAN_POINT('Ctrl Pts',(-20.3312240870609,21.2134447328878,
9.94764188058014));
#133452=CARTESIAN_POINT('Ctrl Pts',(-20.2633441071063,21.2657612997089,
9.95189545846558));
#133453=CARTESIAN_POINT('Ctrl Pts',(-20.1929575410587,21.3145785921586,
9.95614903635102));
#133454=CARTESIAN_POINT('Ctrl Pts',(-20.1239355559419,21.3624494661351,
9.96032015032897));
#133455=CARTESIAN_POINT('Ctrl Pts',(-20.0525037029722,21.4069552612257,
9.96449126430692));
#133456=CARTESIAN_POINT('Ctrl Pts',(-19.979026280494,21.4478526015094,9.96866237828488));
#133457=CARTESIAN_POINT('Ctrl Pts',(-19.9055735140746,21.4887362182955,
9.97283209260525));
#133458=CARTESIAN_POINT('Ctrl Pts',(-19.8300769429976,21.5260135615003,
9.97700180692563));
#133459=CARTESIAN_POINT('Ctrl Pts',(-19.7529274425308,21.5594860797666,
9.981171521246));
#133460=CARTESIAN_POINT('Ctrl Pts',(-19.6757806873741,21.5929574069372,
9.98534108719005));
#133461=CARTESIAN_POINT('Ctrl Pts',(-19.5969815421365,21.6226239960434,
9.98951065313409));
#133462=CARTESIAN_POINT('Ctrl Pts',(-19.5169416763858,21.6483350880374,
9.99368021907814));
#133463=CARTESIAN_POINT('Ctrl Pts',(-19.4340877076953,21.6749501503077,
9.99799638181706));
#133464=CARTESIAN_POINT('Ctrl Pts',(-19.3499046498554,21.6973262283484,
10.002312544556));
#133465=CARTESIAN_POINT('Ctrl Pts',(-19.264865245119,21.7153526292287,10.0066287072949));
#133466=CARTESIAN_POINT('Ctrl Pts',(-19.1825959900472,21.7327918219964,
10.0108042714866));
#133467=CARTESIAN_POINT('Ctrl Pts',(-19.0995257948678,21.7461603390116,
10.0149798356783));
#133468=CARTESIAN_POINT('Ctrl Pts',(-19.0160902825553,21.7554105550182,
10.0191553998699));
#133469=CARTESIAN_POINT('Ctrl Pts',(-18.928440640865,21.7651279774449,10.0235418618825));
#133470=CARTESIAN_POINT('Ctrl Pts',(-18.840388390719,21.7703001003684,10.027928323895));
#133471=CARTESIAN_POINT('Ctrl Pts',(-18.7524390182804,21.7709335933975,
10.0323147859076));
#133472=CARTESIAN_POINT('Ctrl Pts',(-18.6644896458417,21.7715670864265,
10.0367012479201));
#133473=CARTESIAN_POINT('Ctrl Pts',(-18.576643727377,21.767662051318,10.0410877099326));
#133474=CARTESIAN_POINT('Ctrl Pts',(-18.4893986055751,21.759287691342,10.0454741719452));
#133475=CARTESIAN_POINT('Ctrl Pts',(-18.4061677611557,21.7512986480824,
10.0496588063382));
#133476=CARTESIAN_POINT('Ctrl Pts',(-18.3231738401582,21.7392127858656,
10.0538434407313));
#133477=CARTESIAN_POINT('Ctrl Pts',(-18.2408521955269,21.7230519984553,
10.0580280751243));
#133478=CARTESIAN_POINT('Ctrl Pts',(-18.1586477255675,21.7069142139257,
10.0622067532083));
#133479=CARTESIAN_POINT('Ctrl Pts',(-18.0771140788212,21.6867131129898,
10.0663854312922));
#133480=CARTESIAN_POINT('Ctrl Pts',(-17.9966818731345,21.6625223800316,
10.0705641093761));
#133481=CARTESIAN_POINT('Ctrl Pts',(-17.9148079779664,21.6378980455705,
10.0748176872616));
#133482=CARTESIAN_POINT('Ctrl Pts',(-17.8340758788423,21.6091396900265,
10.079071265147));
#133483=CARTESIAN_POINT('Ctrl Pts',(-17.7549293481812,21.5763796014059,
10.0833248430324));
#133484=CARTESIAN_POINT('Ctrl Pts',(-17.6773172274588,21.5442546310292,
10.0874959570104));
#133485=CARTESIAN_POINT('Ctrl Pts',(-17.6012301897821,21.5082818897809,
10.0916670709883));
#133486=CARTESIAN_POINT('Ctrl Pts',(-17.5270700635701,21.4686359601471,
10.0958381849663));
#133487=CARTESIAN_POINT('Ctrl Pts',(-17.4529348225046,21.4290033340878,
10.1000078992867));
#133488=CARTESIAN_POINT('Ctrl Pts',(-17.3807256141186,21.3857001842595,
10.104177613607));
#133489=CARTESIAN_POINT('Ctrl Pts',(-17.3108209620507,21.3389477028211,
10.1083473279274));
#133490=CARTESIAN_POINT('Ctrl Pts',(-17.2409187974905,21.2921968850367,
10.1125168938714));
#133491=CARTESIAN_POINT('Ctrl Pts',(-17.1733214081187,21.241997236139,10.1166864598155));
#133492=CARTESIAN_POINT('Ctrl Pts',(-17.1083783873658,21.1886133020731,
10.1208560257595));
#133493=CARTESIAN_POINT('Ctrl Pts',(-17.0411520501189,21.1333524547415,
10.1251721884984));
#133494=CARTESIAN_POINT('Ctrl Pts',(-16.976770617027,21.0746795720034,10.1294883512374));
#133495=CARTESIAN_POINT('Ctrl Pts',(-16.9155830497423,21.0129322392963,
10.1338045139763));
#133496=CARTESIAN_POINT('Ctrl Pts',(-16.8563886610263,20.9531963194576,
10.137980078168));
#133497=CARTESIAN_POINT('Ctrl Pts',(-16.8001835327305,20.8905835561615,
10.1421556423596));
#133498=CARTESIAN_POINT('Ctrl Pts',(-16.7472435046123,20.825434460743,10.1463312065513));
#133499=CARTESIAN_POINT('Ctrl Pts',(-16.6916296015266,20.756994839392,10.1507176685639));
#133500=CARTESIAN_POINT('Ctrl Pts',(-16.639619651693,20.6857564036312,10.1551041305764));
#133501=CARTESIAN_POINT('Ctrl Pts',(-16.5914816570987,20.6121477974616,
10.159490592589));
#133502=CARTESIAN_POINT('Ctrl Pts',(-16.5433436625044,20.538539191292,10.1638770546015));
#133503=CARTESIAN_POINT('Ctrl Pts',(-16.49907784951,20.4625609543416,10.1682635166141));
#133504=CARTESIAN_POINT('Ctrl Pts',(-16.4588952312818,20.3846687315233,
10.1726499786266));
#133505=CARTESIAN_POINT('Ctrl Pts',(-16.4205614748832,20.310360445341,10.1768346130197));
#133506=CARTESIAN_POINT('Ctrl Pts',(-16.3858007370466,20.2340338438632,
10.1810192474127));
#133507=CARTESIAN_POINT('Ctrl Pts',(-16.3548302568731,20.1560668406994,
10.1852038818058));
#133508=CARTESIAN_POINT('Ctrl Pts',(-16.3239038593448,20.0782108139142,
10.1893825598897));
#133509=CARTESIAN_POINT('Ctrl Pts',(-16.2967571717624,19.9987194471873,
10.1935612379737));
#133510=CARTESIAN_POINT('Ctrl Pts',(-16.273561322493,19.9179947059404,10.1977399160576));
#133511=CARTESIAN_POINT('Ctrl Pts',(-16.2499497042961,19.8358230317225,
10.201993493943));
#133512=CARTESIAN_POINT('Ctrl Pts',(-16.2304321761497,19.7523737600802,
10.2062470718285));
#133513=CARTESIAN_POINT('Ctrl Pts',(-16.2151377103691,19.6680916383782,
10.2105006497139));
#133514=CARTESIAN_POINT('Ctrl Pts',(-16.2001397576524,19.5854434900685,
10.2146717636919));
#133515=CARTESIAN_POINT('Ctrl Pts',(-16.189202669843,19.5019949698565,10.2188428776698));
#133516=CARTESIAN_POINT('Ctrl Pts',(-16.1823971528001,19.4181784500404,
10.2230139916478));
#133517=CARTESIAN_POINT('Ctrl Pts',(-16.1755939194141,19.3343900556669,
10.2271837059681));
#133518=CARTESIAN_POINT('Ctrl Pts',(-16.1729195406043,19.2502343650763,
10.2313534202885));
#133519=CARTESIAN_POINT('Ctrl Pts',(-16.1743929164357,19.1661493838666,
10.2355231346089));
#133520=CARTESIAN_POINT('Ctrl Pts',(-16.1758662398381,19.0820673947613,
10.2396927005529));
#133521=CARTESIAN_POINT('Ctrl Pts',(-16.1814870155134,18.9980565699815,
10.243862266497));
#133522=CARTESIAN_POINT('Ctrl Pts',(-16.1912220304804,18.9145540559805,
10.248031832441));
#133523=CARTESIAN_POINT('Ctrl Pts',(-16.2012993165642,18.8281156965988,
10.25234799518));
#133524=CARTESIAN_POINT('Ctrl Pts',(-16.2157854771197,18.7422225813443,
10.2566641579189));
#133525=CARTESIAN_POINT('Ctrl Pts',(-16.234585542542,18.657350860337,10.2609803206578));
#133526=CARTESIAN_POINT('Ctrl Pts',(-16.2527731978104,18.5752438267145,
10.2651558848495));
#133527=CARTESIAN_POINT('Ctrl Pts',(-16.2749978531259,18.4940931072449,
10.2693314490412));
#133528=CARTESIAN_POINT('Ctrl Pts',(-16.3011224991717,18.4143149518389,
10.2735070132328));
#133529=CARTESIAN_POINT('Ctrl Pts',(-16.3285666389838,18.3305073914578,
10.2778934752454));
#133530=CARTESIAN_POINT('Ctrl Pts',(-16.3603148903336,18.2482152402673,
10.2822799372579));
#133531=CARTESIAN_POINT('Ctrl Pts',(-16.3961518958431,18.1678958623944,
10.2866663992705));
#133532=CARTESIAN_POINT('Ctrl Pts',(-16.4319889013526,18.0875764845216,
10.291052861283));
#133533=CARTESIAN_POINT('Ctrl Pts',(-16.4719143298048,18.0092303623902,
10.2954393232955));
#133534=CARTESIAN_POINT('Ctrl Pts',(-16.5156592733601,17.9332815566289,
10.2998257853081));
#133535=CARTESIAN_POINT('Ctrl Pts',(-16.5573791055758,17.8608486952323,
10.3040091821606));
#133536=CARTESIAN_POINT('Ctrl Pts',(-16.6027278790349,17.7903265695032,
10.3081925790132));
#133537=CARTESIAN_POINT('Ctrl Pts',(-16.6515056001532,17.7221020603793,
10.3123759758657));
#133538=CARTESIAN_POINT('Ctrl Pts',(-16.7002227477591,17.6539622743228,
10.3165541776612));
#133539=CARTESIAN_POINT('Ctrl Pts',(-16.7523601281725,17.5881148134606,
10.3207323794568));
#133540=CARTESIAN_POINT('Ctrl Pts',(-16.8076724801956,17.5249210319667,
10.3249105812523));
#133541=CARTESIAN_POINT('Ctrl Pts',(-16.8629267561818,17.4617936017354,
10.329084396082));
#133542=CARTESIAN_POINT('Ctrl Pts',(-16.9213490806808,17.4013146604626,
10.3332582109116));
#133543=CARTESIAN_POINT('Ctrl Pts',(-16.9826524925986,17.3438144419156,
10.3374320257413));
#133544=CARTESIAN_POINT('Ctrl Pts',(-17.0438286406382,17.2864335919419,
10.3415971758678));
#133545=CARTESIAN_POINT('Ctrl Pts',(-17.1078736103551,17.2320194406792,
10.3457623259944));
#133546=CARTESIAN_POINT('Ctrl Pts',(-17.174464231106,17.180864983421,10.3499274761209));
#133547=CARTESIAN_POINT('Ctrl Pts',(-17.1725834074896,17.1783793283469,
9.54996332099649));
#133548=CARTESIAN_POINT('Ctrl Pts',(-17.7798204782461,16.7191701619952,
9.58795779796462));
#133549=CARTESIAN_POINT('Ctrl Pts',(-19.5298543890223,16.338845415249,9.66834421049323));
#133550=CARTESIAN_POINT('Ctrl Pts',(-21.1196060595483,17.7909993809188,
9.76278617061903));
#133551=CARTESIAN_POINT('Ctrl Pts',(-21.2937097337482,18.9257985538188,
9.81923365377672));
#133552=CARTESIAN_POINT('Ctrl Pts',(-21.2916489871171,19.2089800104295,
9.83328920137392));
#133553=CARTESIAN_POINT('',(-21.2939989766127,19.2132890482675,9.7667098901893));
#133554=CARTESIAN_POINT('Ctrl Pts',(-17.174464231106,17.180864983421,9.48328065598192));
#133555=CARTESIAN_POINT('Ctrl Pts',(-17.2411531716825,17.1296349975485,
9.48745093329683));
#133556=CARTESIAN_POINT('Ctrl Pts',(-17.3103521302254,17.0817075111554,
9.49162121061175));
#133557=CARTESIAN_POINT('Ctrl Pts',(-17.3816949027239,17.0373231786024,
9.49579148792666));
#133558=CARTESIAN_POINT('Ctrl Pts',(-17.4531170616135,16.992889457557,9.49996640570135));
#133559=CARTESIAN_POINT('Ctrl Pts',(-17.5266874037677,16.952007001496,9.50414132347604));
#133560=CARTESIAN_POINT('Ctrl Pts',(-17.602013491345,16.9148714007654,9.50831624125073));
#133561=CARTESIAN_POINT('Ctrl Pts',(-17.6773880098046,16.877711923713,9.51249384328738));
#133562=CARTESIAN_POINT('Ctrl Pts',(-17.7545200986259,16.8443042791516,
9.51667144532403));
#133563=CARTESIAN_POINT('Ctrl Pts',(-17.8329978366507,16.8147956886693,
9.52084904736067));
#133564=CARTESIAN_POINT('Ctrl Pts',(-17.9116031056638,16.7852391449737,
9.52503343824891));
#133565=CARTESIAN_POINT('Ctrl Pts',(-17.9915579506763,16.7595944403009,
9.52921782913714));
#133566=CARTESIAN_POINT('Ctrl Pts',(-18.072436301939,16.7379586591794,9.53340222002537));
#133567=CARTESIAN_POINT('Ctrl Pts',(-18.103254318857,16.7297145263771,9.53499664705277));
#133568=CARTESIAN_POINT('Ctrl Pts',(-18.1342063322878,16.7220519272115,
9.53659107408017));
#133569=CARTESIAN_POINT('Ctrl Pts',(-18.1652685194102,16.7149742583487,
9.53818550110756));
#133570=CARTESIAN_POINT('Ctrl Pts',(-18.2467924112676,16.6963986471497,
9.54237013550062));
#133571=CARTESIAN_POINT('Ctrl Pts',(-18.3293790330748,16.6817867038644,
9.54655476989366));
#133572=CARTESIAN_POINT('Ctrl Pts',(-18.4126082132396,16.6712544774323,
9.55073940428671));
#133573=CARTESIAN_POINT('Ctrl Pts',(-18.4957189269681,16.6607372423208,
9.55491808237065));
#133574=CARTESIAN_POINT('Ctrl Pts',(-18.5794699298767,16.654288246849,9.55909676045459));
#133575=CARTESIAN_POINT('Ctrl Pts',(-18.6634292675077,16.6519728857014,
9.56327543853853));
#133576=CARTESIAN_POINT('Ctrl Pts',(-18.7488935159254,16.6496160233692,
9.56752901642397));
#133577=CARTESIAN_POINT('Ctrl Pts',(-18.8345731712375,16.6515425508617,
9.57178259430941));
#133578=CARTESIAN_POINT('Ctrl Pts',(-18.9200053717023,16.6577663636679,
9.57603617219484));
#133579=CARTESIAN_POINT('Ctrl Pts',(-19.0037813022539,16.663869515718,9.5802072861728));
#133580=CARTESIAN_POINT('Ctrl Pts',(-19.0873188071791,16.6741047825048,
9.58437840015075));
#133581=CARTESIAN_POINT('Ctrl Pts',(-19.1701815497895,16.6884327252533,
9.5885495141287));
#133582=CARTESIAN_POINT('Ctrl Pts',(-19.2530164870063,16.7027558601221,
9.59271922844908));
#133583=CARTESIAN_POINT('Ctrl Pts',(-19.3351766586591,16.7211688651668,
9.59688894276945));
#133584=CARTESIAN_POINT('Ctrl Pts',(-19.4162332022014,16.7435807292205,
9.60105865708982));
#133585=CARTESIAN_POINT('Ctrl Pts',(-19.4972868614039,16.7659917957639,
9.60522822303387));
#133586=CARTESIAN_POINT('Ctrl Pts',(-19.5772365274095,16.7924013149753,
9.60939778897792));
#133587=CARTESIAN_POINT('Ctrl Pts',(-19.6556671754964,16.8226680260876,
9.61356735492196));
#133588=CARTESIAN_POINT('Ctrl Pts',(-19.7368553484154,16.8539988774245,
9.61788351766088));
#133589=CARTESIAN_POINT('Ctrl Pts',(-19.8164152065818,16.8894630151456,
9.6221996803998));
#133590=CARTESIAN_POINT('Ctrl Pts',(-19.8939093684295,16.9288496418883,
9.62651584313872));
#133591=CARTESIAN_POINT('Ctrl Pts',(-19.9688791661059,16.9669532534076,
9.6306914073304));
#133592=CARTESIAN_POINT('Ctrl Pts',(-20.0419153954164,17.0087274533692,
9.63486697152208));
#133593=CARTESIAN_POINT('Ctrl Pts',(-20.112649171425,17.0539356842855,9.63904253571376));
#133594=CARTESIAN_POINT('Ctrl Pts',(-20.1869555423063,17.1014272754729,
9.6434289977263));
#133595=CARTESIAN_POINT('Ctrl Pts',(-20.2587202783153,17.1527085808079,
9.64781545973885));
#133596=CARTESIAN_POINT('Ctrl Pts',(-20.3275542346358,17.2074569130477,
9.65220192175139));
#133597=CARTESIAN_POINT('Ctrl Pts',(-20.3963881909563,17.2622052452876,
9.65658838376393));
#133598=CARTESIAN_POINT('Ctrl Pts',(-20.4622909830917,17.3204201632972,
9.66097484577647));
#133599=CARTESIAN_POINT('Ctrl Pts',(-20.5249190804939,17.3817354354487,
9.66536130778901));
#133600=CARTESIAN_POINT('Ctrl Pts',(-20.5852113014986,17.440763796406,9.66958416538902));
#133601=CARTESIAN_POINT('Ctrl Pts',(-20.6427127908696,17.5029045422552,
9.67380702298903));
#133602=CARTESIAN_POINT('Ctrl Pts',(-20.6970796830689,17.5678572314245,
9.67802988058905));
#133603=CARTESIAN_POINT('Ctrl Pts',(-20.7500936846377,17.6311936081461,
9.68214765466765));
#133604=CARTESIAN_POINT('Ctrl Pts',(-20.8001269202378,17.697203245602,9.68626542874624));
#133605=CARTESIAN_POINT('Ctrl Pts',(-20.8468954124061,17.7655682388181,
9.69038320282484));
#133606=CARTESIAN_POINT('Ctrl Pts',(-20.89361966769,17.8338685676809,9.69449708202705));
#133607=CARTESIAN_POINT('Ctrl Pts',(-20.9370850392269,17.9045194435154,
9.69861096122926));
#133608=CARTESIAN_POINT('Ctrl Pts',(-20.9770478427322,17.9771700379653,
9.70272484043147));
#133609=CARTESIAN_POINT('Ctrl Pts',(-21.016985643432,18.0497751784301,9.70683614577719));
#133610=CARTESIAN_POINT('Ctrl Pts',(-21.0534249974544,18.1243771397533,
9.71094745112291));
#133611=CARTESIAN_POINT('Ctrl Pts',(-21.0861664418209,18.2005975900803,
9.71505875646863));
#133612=CARTESIAN_POINT('Ctrl Pts',(-21.1204445396303,18.2803952930204,
9.71936301761202));
#133613=CARTESIAN_POINT('Ctrl Pts',(-21.1506688210159,18.3619666588744,
9.72366727875541));
#133614=CARTESIAN_POINT('Ctrl Pts',(-21.1766659614561,18.4448518415192,
9.7279715398988));
#133615=CARTESIAN_POINT('Ctrl Pts',(-21.2014998963996,18.5240284432037,
9.73208321292915));
#133616=CARTESIAN_POINT('Ctrl Pts',(-21.2224767553181,18.6044033134951,
9.7361948859595));
#133617=CARTESIAN_POINT('Ctrl Pts',(-21.2394965458158,18.6855601281733,
9.74030655898986));
#133618=CARTESIAN_POINT('Ctrl Pts',(-21.2565208804897,18.7667386112071,
9.74441932981087));
#133619=CARTESIAN_POINT('Ctrl Pts',(-21.2695859645565,18.8486989864203,
9.74853210063189));
#133620=CARTESIAN_POINT('Ctrl Pts',(-21.2786432445869,18.9310165044542,
9.7526448714529));
#133621=CARTESIAN_POINT('Ctrl Pts',(-21.2877094512627,19.0134151527261,
9.75676169572553));
#133622=CARTESIAN_POINT('Ctrl Pts',(-21.2927599450141,19.0961711731438,
9.76087851999816));
#133623=CARTESIAN_POINT('Ctrl Pts',(-21.2937982075177,19.1788575547119,
9.76499534427079));
#133624=CARTESIAN_POINT('Ctrl Pts',(-21.2939423435977,19.1903364349236,
9.76556685957696));
#133625=CARTESIAN_POINT('Ctrl Pts',(-21.2940092371596,19.2018139780893,
9.76613837488313));
#133626=CARTESIAN_POINT('Ctrl Pts',(-21.2939989766127,19.2132890482674,
9.7667098901893));
#133627=CARTESIAN_POINT('Ctrl Pts',(-21.293998976612,19.2132890490549,9.76670989022852));
#133628=CARTESIAN_POINT('Ctrl Pts',(-21.2938920610985,19.3328599270272,
9.77266511192853));
#133629=CARTESIAN_POINT('Ctrl Pts',(-21.2854044483393,19.4520702292311,
9.77862033362855));
#133630=CARTESIAN_POINT('Ctrl Pts',(-21.2687069780215,19.5699714968758,
9.78457555532857));
#133631=CARTESIAN_POINT('Ctrl Pts',(-21.2612660069347,19.6225123852221,
9.78722940837586));
#133632=CARTESIAN_POINT('Ctrl Pts',(-21.2521952261605,19.6747937484515,
9.78988326142315));
#133633=CARTESIAN_POINT('Ctrl Pts',(-21.2415125421986,19.7267333135613,
9.79253711447044));
#133634=CARTESIAN_POINT('Ctrl Pts',(-21.2246679295087,19.8086323813113,
9.79672174886349));
#133635=CARTESIAN_POINT('Ctrl Pts',(-21.2037753333228,19.8898577370366,
9.80090638325654));
#133636=CARTESIAN_POINT('Ctrl Pts',(-21.1789030820534,19.9699788662181,
9.80509101764959));
#133637=CARTESIAN_POINT('Ctrl Pts',(-21.154066233355,20.0499859528893,9.80926969573354));
#133638=CARTESIAN_POINT('Ctrl Pts',(-21.125261116367,20.1288914993745,9.81344837381749));
#133639=CARTESIAN_POINT('Ctrl Pts',(-21.0926070466711,20.2062752380087,
9.81762705190143));
#133640=CARTESIAN_POINT('Ctrl Pts',(-21.0593676762441,20.2850460245431,
9.82188062978687));
#133641=CARTESIAN_POINT('Ctrl Pts',(-21.022140108072,20.362239437543,9.8261342076723));
#133642=CARTESIAN_POINT('Ctrl Pts',(-20.9811033321017,20.4374283977703,
9.83038778555774));
#133643=CARTESIAN_POINT('Ctrl Pts',(-20.9408621341102,20.5111596732845,
9.83455889953569));
#133644=CARTESIAN_POINT('Ctrl Pts',(-20.8969583386824,20.5829631005171,
9.83873001351364));
#133645=CARTESIAN_POINT('Ctrl Pts',(-20.8496085018329,20.6524578269836,
9.84290112749159));
#133646=CARTESIAN_POINT('Ctrl Pts',(-20.8022745536785,20.7219292338234,
9.84707084181197));
#133647=CARTESIAN_POINT('Ctrl Pts',(-20.7514971194517,20.7890930986179,
9.85124055613234));
#133648=CARTESIAN_POINT('Ctrl Pts',(-20.6975366051101,20.853596724821,9.85541027045272));
#133649=CARTESIAN_POINT('Ctrl Pts',(-20.643578010915,20.9180980557084,9.85957983639676));
#133650=CARTESIAN_POINT('Ctrl Pts',(-20.5864368576391,20.9799389839169,
9.86374940234081));
#133651=CARTESIAN_POINT('Ctrl Pts',(-20.5264135623405,21.0388002137919,
9.86791896828486));
#133652=CARTESIAN_POINT('Ctrl Pts',(-20.4642799220261,21.099730931896,9.87223513102378));
#133653=CARTESIAN_POINT('Ctrl Pts',(-20.3990580731255,21.1574681514492,
9.87655129376269));
#133654=CARTESIAN_POINT('Ctrl Pts',(-20.3311209857105,21.2117010163947,
9.88086745650161));
#133655=CARTESIAN_POINT('Ctrl Pts',(-20.2653969417723,21.264167251469,9.88504302069329));
#133656=CARTESIAN_POINT('Ctrl Pts',(-20.1971322502975,21.3133536974901,
9.88921858488498));
#133657=CARTESIAN_POINT('Ctrl Pts',(-20.1266949702183,21.3590225138319,
9.89339414907666));
#133658=CARTESIAN_POINT('Ctrl Pts',(-20.0527000705711,21.4069979535197,
9.89778061108919));
#133659=CARTESIAN_POINT('Ctrl Pts',(-19.9763078452047,21.4510907819034,
9.90216707310173));
#133660=CARTESIAN_POINT('Ctrl Pts',(-19.8979731420051,21.4910803768049,
9.90655353511427));
#133661=CARTESIAN_POINT('Ctrl Pts',(-19.8196384388055,21.5310699717064,
9.91093999712681));
#133662=CARTESIAN_POINT('Ctrl Pts',(-19.7393618185147,21.5669561657756,
9.91532645913934));
#133663=CARTESIAN_POINT('Ctrl Pts',(-19.6576188802167,21.5985778865007,
9.91971292115187));
#133664=CARTESIAN_POINT('Ctrl Pts',(-19.5796370556819,21.6287446449807,
9.92389755554492));
#133665=CARTESIAN_POINT('Ctrl Pts',(-19.5000306196521,21.6551430224068,
9.92808218993797));
#133666=CARTESIAN_POINT('Ctrl Pts',(-19.4191985515815,21.6775974428168,
9.93226682433101));
#133667=CARTESIAN_POINT('Ctrl Pts',(-19.3384815379547,21.7000199021387,
9.93644550241496));
#133668=CARTESIAN_POINT('Ctrl Pts',(-19.2565427969408,21.7185094330108,
9.9406241804989));
#133669=CARTESIAN_POINT('Ctrl Pts',(-19.1738002903986,21.7329388780391,
9.94480285858285));
#133670=CARTESIAN_POINT('Ctrl Pts',(-19.0895746838927,21.7476269604994,
9.94905643646829));
#133671=CARTESIAN_POINT('Ctrl Pts',(-19.0045166631074,21.758107797425,9.95331001435372));
#133672=CARTESIAN_POINT('Ctrl Pts',(-18.9190822179584,21.7643007211442,
9.95756359223916));
#133673=CARTESIAN_POINT('Ctrl Pts',(-18.8353040862403,21.7703735829526,
9.96173470621711));
#133674=CARTESIAN_POINT('Ctrl Pts',(-18.7511644753126,21.7723232722254,
9.96590582019506));
#133675=CARTESIAN_POINT('Ctrl Pts',(-18.6671008395073,21.7701257300737,
9.97007693417301));
#133676=CARTESIAN_POINT('Ctrl Pts',(-18.5830654120668,21.7679289253285,
9.97424664849338));
#133677=CARTESIAN_POINT('Ctrl Pts',(-18.49910636861,21.7615876649968,9.97841636281376));
#133678=CARTESIAN_POINT('Ctrl Pts',(-18.4156612239222,21.7511300013277,
9.98258607713413));
#133679=CARTESIAN_POINT('Ctrl Pts',(-18.3322190485708,21.7406727097872,
9.98675564307818));
#133680=CARTESIAN_POINT('Ctrl Pts',(-18.2492911919861,21.7260993641991,
9.99092520902222));
#133681=CARTESIAN_POINT('Ctrl Pts',(-18.1673087413395,21.7074897390852,
9.99509477496626));
#133682=CARTESIAN_POINT('Ctrl Pts',(-18.0824438888645,21.6882258225098,
9.99941093770518));
#133683=CARTESIAN_POINT('Ctrl Pts',(-17.9985926745536,21.664636631037,10.0037271004441));
#133684=CARTESIAN_POINT('Ctrl Pts',(-17.9162183607824,21.6368675129855,
10.008043263183));
#133685=CARTESIAN_POINT('Ctrl Pts',(-17.8365273816181,21.6100029710338,
10.0122188273747));
#133686=CARTESIAN_POINT('Ctrl Pts',(-17.7582189816851,21.5792268589616,
10.0163943915664));
#133687=CARTESIAN_POINT('Ctrl Pts',(-17.6816923706303,21.5447199174645,
10.0205699557581));
#133688=CARTESIAN_POINT('Ctrl Pts',(-17.601300582376,21.5084701123847,10.0249564177706));
#133689=CARTESIAN_POINT('Ctrl Pts',(-17.5228758288489,21.4681029519008,
10.0293428797831));
#133690=CARTESIAN_POINT('Ctrl Pts',(-17.4468498189205,21.423881472503,10.0337293417957));
#133691=CARTESIAN_POINT('Ctrl Pts',(-17.3708238089921,21.3796599931052,
10.0381158038082));
#133692=CARTESIAN_POINT('Ctrl Pts',(-17.2971969868962,21.3315845757053,
10.0425022658208));
#133693=CARTESIAN_POINT('Ctrl Pts',(-17.2263622218889,21.2799679383722,
10.0468887278333));
#133694=CARTESIAN_POINT('Ctrl Pts',(-17.1587866694218,21.230726259037,10.0510733622264));
#133695=CARTESIAN_POINT('Ctrl Pts',(-17.0935003576728,21.1780787853436,
10.0552579966194));
#133696=CARTESIAN_POINT('Ctrl Pts',(-17.0308668782518,21.1222659599345,
10.0594426310125));
#133697=CARTESIAN_POINT('Ctrl Pts',(-16.9683225498363,21.0665325771741,
10.0636213090964));
#133698=CARTESIAN_POINT('Ctrl Pts',(-16.908423893985,21.0076430954477,10.0677999871803));
#133699=CARTESIAN_POINT('Ctrl Pts',(-16.8515040647698,20.9458801266491,
10.0719786652643));
#133700=CARTESIAN_POINT('Ctrl Pts',(-16.7935639885235,20.883010101023,10.0762322431497));
#133701=CARTESIAN_POINT('Ctrl Pts',(-16.7387109698993,20.8171628445092,
10.0804858210352));
#133702=CARTESIAN_POINT('Ctrl Pts',(-16.6872596563362,20.7486781085841,
10.0847393989206));
#133703=CARTESIAN_POINT('Ctrl Pts',(-16.6368058268854,20.6815210829019,
10.0889105128986));
#133704=CARTESIAN_POINT('Ctrl Pts',(-16.5896232711908,20.6118283153184,
10.0930816268765));
#133705=CARTESIAN_POINT('Ctrl Pts',(-16.5459690047033,20.5399546130779,
10.0972527408545));
#133706=CARTESIAN_POINT('Ctrl Pts',(-16.5023293868266,20.4681050287523,
10.1014224551748));
#133707=CARTESIAN_POINT('Ctrl Pts',(-16.4622159454254,20.3940763560657,
10.1055921694952));
#133708=CARTESIAN_POINT('Ctrl Pts',(-16.4258419114527,20.318251659865,10.1097618838156));
#133709=CARTESIAN_POINT('Ctrl Pts',(-16.3894691718243,20.2424296618324,
10.1139314497596));
#133710=CARTESIAN_POINT('Ctrl Pts',(-16.3568357732639,20.1648121825009,
10.1181010157037));
#133711=CARTESIAN_POINT('Ctrl Pts',(-16.3281079773328,20.0858048783966,
10.1222705816477));
#133712=CARTESIAN_POINT('Ctrl Pts',(-16.2983701475364,20.004019774946,10.1265867443866));
#133713=CARTESIAN_POINT('Ctrl Pts',(-16.2728178525521,19.920745791513,10.1309029071256));
#133714=CARTESIAN_POINT('Ctrl Pts',(-16.2515796325832,19.8364511327309,
10.1352190698645));
#133715=CARTESIAN_POINT('Ctrl Pts',(-16.231033245396,19.7549023635925,10.1393946340562));
#133716=CARTESIAN_POINT('Ctrl Pts',(-16.2145242335759,19.6723988660723,
10.1435701982478));
#133717=CARTESIAN_POINT('Ctrl Pts',(-16.2021167074112,19.5893741438175,
10.1477457624395));
#133718=CARTESIAN_POINT('Ctrl Pts',(-16.189082506596,19.5021560402142,10.1521322244521));
#133719=CARTESIAN_POINT('Ctrl Pts',(-16.1805750686802,19.414363255138,10.1565186864646));
#133720=CARTESIAN_POINT('Ctrl Pts',(-16.176606897426,19.3265011640937,10.1609051484772));
#133721=CARTESIAN_POINT('Ctrl Pts',(-16.1726387261718,19.2386390730495,
10.1652916104897));
#133722=CARTESIAN_POINT('Ctrl Pts',(-16.173209741748,19.1507082557479,10.1696780725022));
#133723=CARTESIAN_POINT('Ctrl Pts',(-16.1782696504243,19.0632083214198,
10.1740645345148));
#133724=CARTESIAN_POINT('Ctrl Pts',(-16.1830972264457,18.9797260667259,
10.1782495861008));
#133725=CARTESIAN_POINT('Ctrl Pts',(-16.1920284781124,18.8963252255056,
10.1824346376868));
#133726=CARTESIAN_POINT('Ctrl Pts',(-16.2050580322512,18.8134417982748,
10.1866196892728));
#133727=CARTESIAN_POINT('Ctrl Pts',(-16.2180651804963,18.7307008991188,
10.1907975441566));
#133728=CARTESIAN_POINT('Ctrl Pts',(-16.2351565463974,18.6484760952712,
10.1949753990404));
#133729=CARTESIAN_POINT('Ctrl Pts',(-16.2562748618428,18.5672002331905,
10.1991532539242));
#133730=CARTESIAN_POINT('Ctrl Pts',(-16.2773725113752,18.4860039058583,
10.2033270204522));
#133731=CARTESIAN_POINT('Ctrl Pts',(-16.3024891716603,18.4057551192321,
10.2075007869803));
#133732=CARTESIAN_POINT('Ctrl Pts',(-16.3315163412326,18.326877684166,10.2116745535083));
#133733=CARTESIAN_POINT('Ctrl Pts',(-16.3605238139034,18.2480537727846,
10.215845487853));
#133734=CARTESIAN_POINT('Ctrl Pts',(-16.3934363671985,18.1705997951908,
10.2200164221976));
#133735=CARTESIAN_POINT('Ctrl Pts',(-16.4300957454762,18.0949242024006,
10.2241873565423));
#133736=CARTESIAN_POINT('Ctrl Pts',(-16.4667412452109,18.0192772589498,
10.2283567118505));
#133737=CARTESIAN_POINT('Ctrl Pts',(-16.5071305503789,17.9454077756885,
10.2325260671588));
#133738=CARTESIAN_POINT('Ctrl Pts',(-16.5510579279904,17.8737027592003,
10.236695422467));
#133739=CARTESIAN_POINT('Ctrl Pts',(-16.5950001276849,17.8019735478304,
10.2408661846093));
#133740=CARTESIAN_POINT('Ctrl Pts',(-16.6424825512063,17.7324106591257,
10.2450369467516));
#133741=CARTESIAN_POINT('Ctrl Pts',(-16.6932547035781,17.6653743547897,
10.2492077088939));
#133742=CARTESIAN_POINT('Ctrl Pts',(-16.7440345633082,17.5983278741504,
10.2533791041699));
#133743=CARTESIAN_POINT('Ctrl Pts',(-16.7981048586349,17.5338091011393,
10.2575504994459));
#133744=CARTESIAN_POINT('Ctrl Pts',(-16.8551743954097,17.4721456796109,
10.2617218947218));
#133745=CARTESIAN_POINT('Ctrl Pts',(-16.9123064332965,17.4104147258642,
10.2658978584043));
#133746=CARTESIAN_POINT('Ctrl Pts',(-16.9724439505659,17.3515456983761,
10.2700738220868));
#133747=CARTESIAN_POINT('Ctrl Pts',(-17.0352588293081,17.2958293979397,
10.2742497857693));
#133748=CARTESIAN_POINT('Ctrl Pts',(-17.0803268546882,17.2558544160176,
10.2772459300109));
#133749=CARTESIAN_POINT('Ctrl Pts',(-17.126772332044,17.2175015725475,10.2802420742524));
#133750=CARTESIAN_POINT('Ctrl Pts',(-17.174464231106,17.180864983421,10.283238218494));
#133751=CARTESIAN_POINT('Origin',(-18.734,19.211,-1.76670989022852));
#133752=CARTESIAN_POINT('',(-17.1757181102512,17.1824653653531,11.1497835165008));
#133753=CARTESIAN_POINT('',(-17.1731949711369,17.1791828613964,11.0834063356124));
#133754=CARTESIAN_POINT('',(-17.174464231106,17.180864983421,-1.76670989022852));
#133755=CARTESIAN_POINT('',(-21.2939995125392,19.2125798097912,10.6332901097715));
#133756=CARTESIAN_POINT('Ctrl Pts',(-21.2907953051338,19.2125971079063,
10.6332910656997));
#133757=CARTESIAN_POINT('Ctrl Pts',(-21.292607272731,19.5356421908361,10.6493117789173));
#133758=CARTESIAN_POINT('Ctrl Pts',(-21.0857646549701,20.7112479426697,
10.7077244276952));
#133759=CARTESIAN_POINT('Ctrl Pts',(-19.318984802206,22.1810310672293,10.8085290120338));
#133760=CARTESIAN_POINT('Ctrl Pts',(-16.5533150683864,21.3105011284,10.9357048187152));
#133761=CARTESIAN_POINT('Ctrl Pts',(-15.8690423811832,18.8090198107934,
11.0494563202042));
#133762=CARTESIAN_POINT('Ctrl Pts',(-16.7160809400405,17.5418442729995,
11.1208158861327));
#133763=CARTESIAN_POINT('Ctrl Pts',(-17.175718110251,17.1824653653533,11.1497835165008));
#133764=CARTESIAN_POINT('Ctrl Pts',(-17.174464231106,17.180864983421,10.3499274761209));
#133765=CARTESIAN_POINT('Ctrl Pts',(-17.2411280860223,17.1296542681803,
10.354097206942));
#133766=CARTESIAN_POINT('Ctrl Pts',(-17.3103428504281,17.0817107249359,
10.3582669377631));
#133767=CARTESIAN_POINT('Ctrl Pts',(-17.3817510958368,17.0372882203039,
10.3624366685842));
#133768=CARTESIAN_POINT('Ctrl Pts',(-17.4531563510901,16.992867575824,10.3666062248017));
#133769=CARTESIAN_POINT('Ctrl Pts',(-17.5267545137001,16.9519679191462,
10.3707757810191));
#133770=CARTESIAN_POINT('Ctrl Pts',(-17.6021605539753,16.9147989050559,
10.3749453372365));
#133771=CARTESIAN_POINT('Ctrl Pts',(-17.6806132684811,16.8761281296082,
10.3792833584659));
#133772=CARTESIAN_POINT('Ctrl Pts',(-17.7610225775555,16.8414961150588,
10.3836213796953));
#133773=CARTESIAN_POINT('Ctrl Pts',(-17.842930188215,16.8110844617934,10.3879594009247));
#133774=CARTESIAN_POINT('Ctrl Pts',(-17.9217696726806,16.7818119797141,
10.3921349269177));
#133775=CARTESIAN_POINT('Ctrl Pts',(-18.0019967422928,16.7564494038124,
10.3963104529106));
#133776=CARTESIAN_POINT('Ctrl Pts',(-18.0831874283277,16.7351076363151,
10.4004859789035));
#133777=CARTESIAN_POINT('Ctrl Pts',(-18.1644361653549,16.7137506095455,
10.4046644903796));
#133778=CARTESIAN_POINT('Ctrl Pts',(-18.2466494404615,16.6964202058467,
10.4088430018557));
#133779=CARTESIAN_POINT('Ctrl Pts',(-18.329394229314,16.6831760009195,10.4130215133318));
#133780=CARTESIAN_POINT('Ctrl Pts',(-18.4122672488332,16.669911271277,10.4172065003011));
#133781=CARTESIAN_POINT('Ctrl Pts',(-18.4956729694358,16.660745419148,10.4213914872703));
#133782=CARTESIAN_POINT('Ctrl Pts',(-18.5791750874247,16.6556860767323,
10.4255764742396));
#133783=CARTESIAN_POINT('Ctrl Pts',(-18.5886534403544,16.6551117891074,
10.4260515134895));
#133784=CARTESIAN_POINT('Ctrl Pts',(-18.5981330383419,16.6545903570305,
10.4265265527395));
#133785=CARTESIAN_POINT('Ctrl Pts',(-18.6076132463769,16.6541217493771,
10.4270015919895));
#133786=CARTESIAN_POINT('Ctrl Pts',(-18.6911246711662,16.6499937711024,
10.4311862263825));
#133787=CARTESIAN_POINT('Ctrl Pts',(-18.7749939587051,16.6499538232249,
10.4353708607756));
#133788=CARTESIAN_POINT('Ctrl Pts',(-18.8587871646375,16.6540431830902,
10.4395554951686));
#133789=CARTESIAN_POINT('Ctrl Pts',(-18.9424611013131,16.6581267222578,
10.4437341732526));
#133790=CARTESIAN_POINT('Ctrl Pts',(-19.0260587159297,16.666327872255,10.4479128513366));
#133791=CARTESIAN_POINT('Ctrl Pts',(-19.1091432618604,16.6786359793504,
10.4520915294205));
#133792=CARTESIAN_POINT('Ctrl Pts',(-19.1937170385645,16.6911647004197,
10.456345107306));
#133793=CARTESIAN_POINT('Ctrl Pts',(-19.2777586906013,16.707949084993,10.4605986851914));
#133794=CARTESIAN_POINT('Ctrl Pts',(-19.3608099823644,16.7289223932342,
10.4648522630768));
#133795=CARTESIAN_POINT('Ctrl Pts',(-19.4422511627754,16.7494890929691,
10.4690233770548));
#133796=CARTESIAN_POINT('Ctrl Pts',(-19.5227395737981,16.774083627044,10.4731944910327));
#133797=CARTESIAN_POINT('Ctrl Pts',(-19.6018523684388,16.8025913414466,
10.4773656050107));
#133798=CARTESIAN_POINT('Ctrl Pts',(-19.6809386160173,16.8310894898103,
10.481535319331));
#133799=CARTESIAN_POINT('Ctrl Pts',(-19.7586497315296,16.8634980548298,
10.4857050336514));
#133800=CARTESIAN_POINT('Ctrl Pts',(-19.8345791893321,16.8996528932224,
10.4898747479718));
#133801=CARTESIAN_POINT('Ctrl Pts',(-19.9105059452388,16.9358064450708,
10.4940443139158));
#133802=CARTESIAN_POINT('Ctrl Pts',(-19.9846507545057,16.9757058066968,
10.4982138798599));
#133803=CARTESIAN_POINT('Ctrl Pts',(-20.0566294498852,17.0191397539313,
10.5023834458039));
#133804=CARTESIAN_POINT('Ctrl Pts',(-20.1311388273987,17.0641007851689,
10.5066996085429));
#133805=CARTESIAN_POINT('Ctrl Pts',(-20.2033264842393,17.112849306127,10.5110157712818));
#133806=CARTESIAN_POINT('Ctrl Pts',(-20.2727983186256,17.1651017291676,
10.5153319340207));
#133807=CARTESIAN_POINT('Ctrl Pts',(-20.340007115314,17.2156520350236,10.5195074982124));
#133808=CARTESIAN_POINT('Ctrl Pts',(-20.40467397639,17.2694811317362,10.523683062404));
#133809=CARTESIAN_POINT('Ctrl Pts',(-20.4664767307277,17.3262919649221,
10.5278586265957));
#133810=CARTESIAN_POINT('Ctrl Pts',(-20.5314009952648,17.3859721782373,
10.5322450886082));
#133811=CARTESIAN_POINT('Ctrl Pts',(-20.5931638083647,17.4489428422743,
10.5366315506208));
#133812=CARTESIAN_POINT('Ctrl Pts',(-20.6514380125592,17.5148185627731,
10.5410180126333));
#133813=CARTESIAN_POINT('Ctrl Pts',(-20.7097122167537,17.580694283272,10.5454044746458));
#133814=CARTESIAN_POINT('Ctrl Pts',(-20.7644975100435,17.649474559,10.5497909366584));
#133815=CARTESIAN_POINT('Ctrl Pts',(-20.8155192213964,17.7207390393097,
10.5541773986709));
#133816=CARTESIAN_POINT('Ctrl Pts',(-20.8646271615162,17.789330463214,10.5583993290636));
#133817=CARTESIAN_POINT('Ctrl Pts',(-20.91043082465,17.8604769154309,10.5626212594563));
#133818=CARTESIAN_POINT('Ctrl Pts',(-20.9526566798058,17.9338302629825,
10.5668431898491));
#133819=CARTESIAN_POINT('Ctrl Pts',(-20.9948201353165,18.0070752119515,
10.5710588812454));
#133820=CARTESIAN_POINT('Ctrl Pts',(-21.0334160638336,18.0825201920568,
10.5752745726417));
#133821=CARTESIAN_POINT('Ctrl Pts',(-21.0682129788551,18.1597865253222,
10.5794902640381));
#133822=CARTESIAN_POINT('Ctrl Pts',(-21.1029682787106,18.2369604523702,
10.583700913703));
#133823=CARTESIAN_POINT('Ctrl Pts',(-21.1339334100817,18.3159509969196,
10.587911563368));
#133824=CARTESIAN_POINT('Ctrl Pts',(-21.1609223976387,18.3963542635971,
10.592122213033));
#133825=CARTESIAN_POINT('Ctrl Pts',(-21.1878844462894,18.4766772762055,
10.5963286598616));
#133826=CARTESIAN_POINT('Ctrl Pts',(-21.2108781024617,18.5584097818782,
10.6005351066903));
#133827=CARTESIAN_POINT('Ctrl Pts',(-21.2297657078559,18.6411284956323,
10.6047415535189));
#133828=CARTESIAN_POINT('Ctrl Pts',(-21.24864245849,18.7237996707081,10.6089455828907));
#133829=CARTESIAN_POINT('Ctrl Pts',(-21.2634177498248,18.8074554899473,
10.6131496122625));
#133830=CARTESIAN_POINT('Ctrl Pts',(-21.2740042132099,18.8916591211951,
10.6173536416343));
#133831=CARTESIAN_POINT('Ctrl Pts',(-21.2845883389273,18.975844158876,10.6215567426862));
#133832=CARTESIAN_POINT('Ctrl Pts',(-21.2909854180498,19.0605763228041,
10.6257598437382));
#133833=CARTESIAN_POINT('Ctrl Pts',(-21.2931596531403,19.1454113596826,
10.6299629447901));
#133834=CARTESIAN_POINT('Ctrl Pts',(-21.2937333596144,19.1677964320698,
10.6310719997839));
#133835=CARTESIAN_POINT('Ctrl Pts',(-21.2940133304248,19.1901886456573,
10.6321810547777));
#133836=CARTESIAN_POINT('Ctrl Pts',(-21.2939995125392,19.2125798097912,
10.6332901097715));
#133837=CARTESIAN_POINT('',(-21.2940196853139,19.2096989556262,10.5667098967305));
#133838=CARTESIAN_POINT('Ctrl Pts',(-17.174464231106,17.180864983421,10.283238218494));
#133839=CARTESIAN_POINT('Ctrl Pts',(-17.2410686585138,17.1296999199839,
10.2874225029441));
#133840=CARTESIAN_POINT('Ctrl Pts',(-17.3101048654705,17.0818841653268,
10.2916067873942));
#133841=CARTESIAN_POINT('Ctrl Pts',(-17.3811936333275,17.0376351124834,
10.2957910718443));
#133842=CARTESIAN_POINT('Ctrl Pts',(-17.4120536962257,17.0184263317561,
10.2976074949616));
#133843=CARTESIAN_POINT('Ctrl Pts',(-17.4433002587604,16.9998890947577,
10.2994239180789));
#133844=CARTESIAN_POINT('Ctrl Pts',(-17.4749010481802,16.9820383965787,
10.3012403411962));
#133845=CARTESIAN_POINT('Ctrl Pts',(-17.5477022303472,16.9409143628506,
10.3054249755892));
#133846=CARTESIAN_POINT('Ctrl Pts',(-17.6226557687809,16.9032842410815,
10.3096096099823));
#133847=CARTESIAN_POINT('Ctrl Pts',(-17.6993922596291,16.8693794450073,
10.3137942443753));
#133848=CARTESIAN_POINT('Ctrl Pts',(-17.7760195255805,16.8355229082136,
10.3179729224593));
#133849=CARTESIAN_POINT('Ctrl Pts',(-17.8544242858621,16.8053813489309,
10.3221516005432));
#133850=CARTESIAN_POINT('Ctrl Pts',(-17.9342113535405,16.779141015397,10.3263302786272));
#133851=CARTESIAN_POINT('Ctrl Pts',(-18.0154285470652,16.752430342743,10.3305838565126));
#133852=CARTESIAN_POINT('Ctrl Pts',(-18.0980776713417,16.7297623675601,
10.334837434398));
#133853=CARTESIAN_POINT('Ctrl Pts',(-18.181719189663,16.7112828346924,10.3390910122835));
#133854=CARTESIAN_POINT('Ctrl Pts',(-18.2637391539387,16.6931615636292,
10.3432621262614));
#133855=CARTESIAN_POINT('Ctrl Pts',(-18.3467129067616,16.6790678856914,
10.3474332402394));
#133856=CARTESIAN_POINT('Ctrl Pts',(-18.4302110680641,16.6690888519004,
10.3516043542173));
#133857=CARTESIAN_POINT('Ctrl Pts',(-18.5136812107523,16.6591131666705,
10.3557740685377));
#133858=CARTESIAN_POINT('Ctrl Pts',(-18.5976749560381,16.6532494380237,
10.3599437828581));
#133859=CARTESIAN_POINT('Ctrl Pts',(-18.6817553300752,16.6515331620698,
10.3641134971784));
#133860=CARTESIAN_POINT('Ctrl Pts',(-18.7658327121718,16.6498169471884,
10.3682830631225));
#133861=CARTESIAN_POINT('Ctrl Pts',(-18.8499962569362,16.652247900101,10.3724526290665));
#133862=CARTESIAN_POINT('Ctrl Pts',(-18.9338078728663,16.6588094087744,
10.3766221950106));
#133863=CARTESIAN_POINT('Ctrl Pts',(-19.0205662018197,16.6656016119982,
10.3809383577495));
#133864=CARTESIAN_POINT('Ctrl Pts',(-19.106946868035,16.6768201947949,10.3852545204884));
#133865=CARTESIAN_POINT('Ctrl Pts',(-19.1924704625205,16.6923883119869,
10.3895706832273));
#133866=CARTESIAN_POINT('Ctrl Pts',(-19.2752081349112,16.7074492993989,
10.393746247419));
#133867=CARTESIAN_POINT('Ctrl Pts',(-19.357143268331,16.7265806476473,10.3979218116107));
#133868=CARTESIAN_POINT('Ctrl Pts',(-19.437854716723,16.749661230601,10.4020973758024));
#133869=CARTESIAN_POINT('Ctrl Pts',(-19.5226427085001,16.7739075589308,
10.4064838378149));
#133870=CARTESIAN_POINT('Ctrl Pts',(-19.6060795975567,16.8025123689437,
10.4108702998274));
#133871=CARTESIAN_POINT('Ctrl Pts',(-19.6877001821495,16.8352778018952,
10.41525676184));
#133872=CARTESIAN_POINT('Ctrl Pts',(-19.7693207667423,16.8680432348467,
10.4196432238525));
#133873=CARTESIAN_POINT('Ctrl Pts',(-19.8491245522344,16.9049689780518,
10.4240296858651));
#133874=CARTESIAN_POINT('Ctrl Pts',(-19.9266775857362,16.945802397917,10.4284161478776));
#133875=CARTESIAN_POINT('Ctrl Pts',(-20.0006622892055,16.9847570116046,
10.4326007822707));
#133876=CARTESIAN_POINT('Ctrl Pts',(-20.0728741952653,17.0274126045708,
10.4367854166637));
#133877=CARTESIAN_POINT('Ctrl Pts',(-20.1429187702869,17.0735838265015,
10.4409700510568));
#133878=CARTESIAN_POINT('Ctrl Pts',(-20.2128636455258,17.1196893294125,
10.4451487291407));
#133879=CARTESIAN_POINT('Ctrl Pts',(-20.2806469365539,17.1693002706272,
10.4493274072247));
#133880=CARTESIAN_POINT('Ctrl Pts',(-20.3458981308861,17.2221851731129,
10.4535060853086));
#133881=CARTESIAN_POINT('Ctrl Pts',(-20.4123189059815,17.276017999468,10.457759663194));
#133882=CARTESIAN_POINT('Ctrl Pts',(-20.4761154892317,17.3332430884428,
10.4620132410795));
#133883=CARTESIAN_POINT('Ctrl Pts',(-20.5369274194045,17.3935697481445,
10.4662668189649));
#133884=CARTESIAN_POINT('Ctrl Pts',(-20.5965603916461,17.4527268578301,
10.4704379329429));
#133885=CARTESIAN_POINT('Ctrl Pts',(-20.6533230631002,17.5148660125131,
10.4746090469208));
#133886=CARTESIAN_POINT('Ctrl Pts',(-20.7069098223473,17.5796732905743,
10.4787801608988));
#133887=CARTESIAN_POINT('Ctrl Pts',(-20.7604786000398,17.6444588219275,
10.4829498752191));
#133888=CARTESIAN_POINT('Ctrl Pts',(-20.8108732891324,17.7119103443124,
10.4871195895395));
#133889=CARTESIAN_POINT('Ctrl Pts',(-20.857827517359,17.7816796452479,10.4912893038599));
#133890=CARTESIAN_POINT('Ctrl Pts',(-20.9047800747525,17.8514464634921,
10.4954588698039));
#133891=CARTESIAN_POINT('Ctrl Pts',(-20.9482921585527,17.9235305141741,
10.499628435748));
#133892=CARTESIAN_POINT('Ctrl Pts',(-20.9881406062296,17.9975544398916,
10.503798001692));
#133893=CARTESIAN_POINT('Ctrl Pts',(-21.0293900761685,18.074180955519,10.5081141644309));
#133894=CARTESIAN_POINT('Ctrl Pts',(-21.0667132396991,18.1528858318598,
10.5124303271698));
#133895=CARTESIAN_POINT('Ctrl Pts',(-21.0999152164604,18.2332243669833,
10.5167464899088));
#133896=CARTESIAN_POINT('Ctrl Pts',(-21.1320356423208,18.3109458827751,
10.5209220541004));
#133897=CARTESIAN_POINT('Ctrl Pts',(-21.1602991397429,18.3901957994174,
10.5250976182921));
#133898=CARTESIAN_POINT('Ctrl Pts',(-21.1845795982611,18.4705544364463,
10.5292731824838));
#133899=CARTESIAN_POINT('Ctrl Pts',(-21.2100864050179,18.5549717971972,
10.5336596444963));
#133900=CARTESIAN_POINT('Ctrl Pts',(-21.2311970921469,18.6406122578467,
10.5380461065089));
#133901=CARTESIAN_POINT('Ctrl Pts',(-21.2478262226602,18.7269775601629,
10.5424325685214));
#133902=CARTESIAN_POINT('Ctrl Pts',(-21.2644553531735,18.813342862479,10.5468190305339));
#133903=CARTESIAN_POINT('Ctrl Pts',(-21.2766029222518,18.9004324212998,
10.5512054925465));
#133904=CARTESIAN_POINT('Ctrl Pts',(-21.2842464642989,18.9877446051473,
10.555591954559));
#133905=CARTESIAN_POINT('Ctrl Pts',(-21.2907042434478,19.0615118189368,
10.5592979331155));
#133906=CARTESIAN_POINT('Ctrl Pts',(-21.293961988618,19.1355632322755,10.563003911672));
#133907=CARTESIAN_POINT('Ctrl Pts',(-21.2939996693303,19.2096988355573,
10.5667098902285));
#133908=CARTESIAN_POINT('Ctrl Pts',(-21.2974135715529,19.2097193143547,
10.5667109992077));
#133909=CARTESIAN_POINT('Ctrl Pts',(-21.292595768045,19.9846331911651,10.6053965865519));
#133910=CARTESIAN_POINT('Ctrl Pts',(-20.5048168766745,21.6171665132323,
10.6864741094567));
#133911=CARTESIAN_POINT('Ctrl Pts',(-17.7257693111366,22.0652534087646,
10.8099435679219));
#133912=CARTESIAN_POINT('Ctrl Pts',(-15.7882884293495,19.9081907815984,
10.9371193746033));
#133913=CARTESIAN_POINT('Ctrl Pts',(-16.3366272769448,17.9036399517467,
11.0282736305002));
#133914=CARTESIAN_POINT('Ctrl Pts',(-17.0711420957025,17.2560799239325,
11.0770359508366));
#133915=CARTESIAN_POINT('Ctrl Pts',(-17.1731949711369,17.1791828613964,
11.0834063356124));
#133916=CARTESIAN_POINT('Origin',(-18.734,19.211,-1.76670989022852));
#133917=CARTESIAN_POINT('',(-17.174464231106,17.180864983421,11.9498687293772));
#133918=CARTESIAN_POINT('',(-17.174464231106,17.180864983421,11.8833305103542));
#133919=CARTESIAN_POINT('',(-17.174464231106,17.180864983421,-1.76670989022852));
#133920=CARTESIAN_POINT('',(-21.2940197026037,19.2123010442705,11.4332901032639));
#133921=CARTESIAN_POINT('Ctrl Pts',(-21.2939996693303,19.212301164443,11.4332901097715));
#133922=CARTESIAN_POINT('Ctrl Pts',(-21.293961988618,19.2864367677247,11.436996088328));
#133923=CARTESIAN_POINT('Ctrl Pts',(-21.2907042434478,19.3604881810636,
11.4407020668845));
#133924=CARTESIAN_POINT('Ctrl Pts',(-21.2842464642989,19.4342553948533,
11.444408045441));
#133925=CARTESIAN_POINT('Ctrl Pts',(-21.2769546129518,19.5175502156942,
11.4485926798341));
#133926=CARTESIAN_POINT('Ctrl Pts',(-21.2655641024497,19.6006424250678,
11.4527773142271));
#133927=CARTESIAN_POINT('Ctrl Pts',(-21.250093180474,19.6830965019697,11.4569619486202));
#133928=CARTESIAN_POINT('Ctrl Pts',(-21.2346442794409,19.7654332156989,
11.4611406267041));
#133929=CARTESIAN_POINT('Ctrl Pts',(-21.2151265874821,19.8471331528555,
11.465319304788));
#133930=CARTESIAN_POINT('Ctrl Pts',(-21.1916101807318,19.9277650937117,
11.469497982872));
#133931=CARTESIAN_POINT('Ctrl Pts',(-21.1676722592913,20.0098423041587,
11.4737515607574));
#133932=CARTESIAN_POINT('Ctrl Pts',(-21.1395909011584,20.0908123737399,
11.4780051386429));
#133933=CARTESIAN_POINT('Ctrl Pts',(-21.107494673889,20.170230437914,11.4822587165283));
#133934=CARTESIAN_POINT('Ctrl Pts',(-21.0760206946157,20.2481088279425,
11.4864298305062));
#133935=CARTESIAN_POINT('Ctrl Pts',(-21.0406863094725,20.3244944066984,
11.4906009444842));
#133936=CARTESIAN_POINT('Ctrl Pts',(-21.0016627302193,20.3989838980282,
11.4947720584621));
#133937=CARTESIAN_POINT('Ctrl Pts',(-20.962652245705,20.4734483936899,11.4989417727825));
#133938=CARTESIAN_POINT('Ctrl Pts',(-20.9199552389621,20.5460176583684,
11.5031114871029));
#133939=CARTESIAN_POINT('Ctrl Pts',(-20.873789724926,20.6163113295996,11.5072812014233));
#133940=CARTESIAN_POINT('Ctrl Pts',(-20.827625853657,20.6866024994803,11.5114507673673));
#133941=CARTESIAN_POINT('Ctrl Pts',(-20.7779939737414,20.7546178528605,
11.5156203333114));
#133942=CARTESIAN_POINT('Ctrl Pts',(-20.7251556946207,20.8200055934581,
11.5197898992554));
#133943=CARTESIAN_POINT('Ctrl Pts',(-20.6704596867893,20.8876922863505,
11.5241060619943));
#133944=CARTESIAN_POINT('Ctrl Pts',(-20.6123279420986,20.9525627446113,
11.5284222247332));
#133945=CARTESIAN_POINT('Ctrl Pts',(-20.5510951122121,21.0142651921375,
11.5327383874721));
#133946=CARTESIAN_POINT('Ctrl Pts',(-20.4918569353186,21.0739576889255,
11.5369139516638));
#133947=CARTESIAN_POINT('Ctrl Pts',(-20.4297169860235,21.1306851185865,
11.5410895158555));
#133948=CARTESIAN_POINT('Ctrl Pts',(-20.3650134540522,21.1841687998498,
11.5452650800472));
#133949=CARTESIAN_POINT('Ctrl Pts',(-20.2970419004992,21.2403538147082,
11.5496515420597));
#133950=CARTESIAN_POINT('Ctrl Pts',(-20.2262414538862,21.2929584378006,
11.5540380040723));
#133951=CARTESIAN_POINT('Ctrl Pts',(-20.1530384991425,21.3417110873958,
11.5584244660848));
#133952=CARTESIAN_POINT('Ctrl Pts',(-20.0798355443987,21.390463736991,11.5628109280973));
#133953=CARTESIAN_POINT('Ctrl Pts',(-20.0042306192381,21.4353641822177,
11.5671973901099));
#133954=CARTESIAN_POINT('Ctrl Pts',(-19.9266775857363,21.4761976020829,
11.5715838521224));
#133955=CARTESIAN_POINT('Ctrl Pts',(-19.852692882267,21.5151522157705,11.5757684865155));
#133956=CARTESIAN_POINT('Ctrl Pts',(-19.7766600165144,21.5505508359911,
11.5799531209085));
#133957=CARTESIAN_POINT('Ctrl Pts',(-19.6989550698443,21.5821730668978,
11.5841377553015));
#133958=CARTESIAN_POINT('Ctrl Pts',(-19.6213607265478,21.6137502874729,
11.5883164333855));
#133959=CARTESIAN_POINT('Ctrl Pts',(-19.5420994522194,21.6415616236984,
11.5924951114694));
#133960=CARTESIAN_POINT('Ctrl Pts',(-19.4615717652905,21.6654325874532,
11.5966737895534));
#133961=CARTESIAN_POINT('Ctrl Pts',(-19.3796006774476,21.6897314210775,
11.6009273674388));
#133962=CARTESIAN_POINT('Ctrl Pts',(-19.2963177561688,21.7099470058045,
11.6051809453242));
#133963=CARTESIAN_POINT('Ctrl Pts',(-19.2121666533116,21.7259466498637,
11.6094345232097));
#133964=CARTESIAN_POINT('Ctrl Pts',(-19.1296469837907,21.7416361096021,
11.6136056371876));
#133965=CARTESIAN_POINT('Ctrl Pts',(-19.0462929678286,21.7532715484977,
11.6177767511656));
#133966=CARTESIAN_POINT('Ctrl Pts',(-18.9625363705287,21.760778642813,11.6219478651435));
#133967=CARTESIAN_POINT('Ctrl Pts',(-18.878807878564,21.7682832180503,11.6261175794639));
#133968=CARTESIAN_POINT('Ctrl Pts',(-18.7946775313674,21.7716621589129,
11.6302872937843));
#133969=CARTESIAN_POINT('Ctrl Pts',(-18.7105831609272,21.7708928984721,
11.6344570081046));
#133970=CARTESIAN_POINT('Ctrl Pts',(-18.6264917829255,21.7701236654048,
11.6386265740487));
#133971=CARTESIAN_POINT('Ctrl Pts',(-18.5424368391406,21.7652065295826,
11.6427961399927));
#133972=CARTESIAN_POINT('Ctrl Pts',(-18.4588557388015,21.75617104249,11.6469657059368));
#133973=CARTESIAN_POINT('Ctrl Pts',(-18.3723360300829,21.7468178788176,
11.6512818686757));
#133974=CARTESIAN_POINT('Ctrl Pts',(-18.2863246298127,21.7330514297719,
11.6555980314146));
#133975=CARTESIAN_POINT('Ctrl Pts',(-18.201298466622,21.7149626747092,11.6599141941535));
#133976=CARTESIAN_POINT('Ctrl Pts',(-18.1190420217542,21.6974631589401,
11.6640897583452));
#133977=CARTESIAN_POINT('Ctrl Pts',(-18.0377080547437,21.6759187771978,
11.6682653225369));
#133978=CARTESIAN_POINT('Ctrl Pts',(-17.9577139481209,21.6504630486355,
11.6724408867286));
#133979=CARTESIAN_POINT('Ctrl Pts',(-17.8736795293404,21.6237216117387,
11.6768273487411));
#133980=CARTESIAN_POINT('Ctrl Pts',(-17.7911244272666,21.592663525305,11.6812138107537));
#133981=CARTESIAN_POINT('Ctrl Pts',(-17.710507793232,21.5575003095429,11.6856002727662));
#133982=CARTESIAN_POINT('Ctrl Pts',(-17.6298911591974,21.5223370937809,
11.6899867347788));
#133983=CARTESIAN_POINT('Ctrl Pts',(-17.5512134783825,21.4830690758564,
11.6943731967913));
#133984=CARTESIAN_POINT('Ctrl Pts',(-17.4749010481796,21.4399616034209,
11.6987596588039));
#133985=CARTESIAN_POINT('Ctrl Pts',(-17.4020998660126,21.3988375696928,
11.7029442931969));
#133986=CARTESIAN_POINT('Ctrl Pts',(-17.3311800802056,21.3540665637942,
11.70712892759));
#133987=CARTESIAN_POINT('Ctrl Pts',(-17.262530574498,21.3058455145458,11.711313561983));
#133988=CARTESIAN_POINT('Ctrl Pts',(-17.1939787828646,21.2576931019925,
11.7154922400669));
#133989=CARTESIAN_POINT('Ctrl Pts',(-17.1276912258534,21.206100662466,11.7196709181509));
#133990=CARTESIAN_POINT('Ctrl Pts',(-17.0640314133914,21.1513105214734,
11.7238495962348));
#133991=CARTESIAN_POINT('Ctrl Pts',(-16.9992305445425,21.0955383065804,
11.7281031741203));
#133992=CARTESIAN_POINT('Ctrl Pts',(-16.9371529712701,21.0364528621869,
11.7323567520057));
#133993=CARTESIAN_POINT('Ctrl Pts',(-16.8781504066902,20.9743554057568,
11.7366103298911));
#133994=CARTESIAN_POINT('Ctrl Pts',(-16.8202917219587,20.9134618296928,
11.7407814438691));
#133995=CARTESIAN_POINT('Ctrl Pts',(-16.7653902112892,20.8496723357183,
11.744952557847));
#133996=CARTESIAN_POINT('Ctrl Pts',(-16.7137420754446,20.7833097399275,
11.749123671825));
#133997=CARTESIAN_POINT('Ctrl Pts',(-16.6621112706308,20.7169694127468,
11.7532933861454));
#133998=CARTESIAN_POINT('Ctrl Pts',(-16.613731954815,20.6480580612727,11.7574631004657));
#133999=CARTESIAN_POINT('Ctrl Pts',(-16.5688600933643,20.5769316178687,
11.7616328147861));
#134000=CARTESIAN_POINT('Ctrl Pts',(-16.5239898286469,20.5058077054487,
11.7658023807301));
#134001=CARTESIAN_POINT('Ctrl Pts',(-16.4826270148771,20.4324692473491,
11.7699719466742));
#134002=CARTESIAN_POINT('Ctrl Pts',(-16.4449835652526,20.3573000311682,
11.7741415126182));
#134003=CARTESIAN_POINT('Ctrl Pts',(-16.4060166183775,20.2794879580777,
11.7784576753571));
#134004=CARTESIAN_POINT('Ctrl Pts',(-16.3710356838063,20.1997144642827,
11.7827738380961));
#134005=CARTESIAN_POINT('Ctrl Pts',(-16.3402224147201,20.1184298166865,
11.787090000835));
#134006=CARTESIAN_POINT('Ctrl Pts',(-16.3104128846334,20.039793007936,11.7912655650267));
#134007=CARTESIAN_POINT('Ctrl Pts',(-16.2845037664843,19.9597424478439,
11.7954411292183));
#134008=CARTESIAN_POINT('Ctrl Pts',(-16.2626087130421,19.8787013604513,
11.79961669341));
#134009=CARTESIAN_POINT('Ctrl Pts',(-16.2396077925011,19.7935670803915,
11.8040031554226));
#134010=CARTESIAN_POINT('Ctrl Pts',(-16.2210372171719,19.7073401510525,
11.8083896174351));
#134011=CARTESIAN_POINT('Ctrl Pts',(-16.2069676619408,19.6205211379197,
11.8127760794476));
#134012=CARTESIAN_POINT('Ctrl Pts',(-16.1928981067097,19.5337021247869,
11.8171625414602));
#134013=CARTESIAN_POINT('Ctrl Pts',(-16.1833295591006,19.4462916129091,
11.8215490034727));
#134014=CARTESIAN_POINT('Ctrl Pts',(-16.1782696504243,19.3587916785811,
11.8259354654852));
#134015=CARTESIAN_POINT('Ctrl Pts',(-16.1734424727603,19.2753163125975,
11.8301201717331));
#134016=CARTESIAN_POINT('Ctrl Pts',(-16.1727003261448,19.191448852862,11.834304877981));
#134017=CARTESIAN_POINT('Ctrl Pts',(-16.1760881218677,19.1076229052962,
11.8384895842288));
#134018=CARTESIAN_POINT('Ctrl Pts',(-16.1794710795838,19.0239166669836,
11.8426683144266));
#134019=CARTESIAN_POINT('Ctrl Pts',(-16.1869722459979,18.9402522788471,
11.8468470446244));
#134020=CARTESIAN_POINT('Ctrl Pts',(-16.1985846232539,18.8570665777874,
11.8510257748222));
#134021=CARTESIAN_POINT('Ctrl Pts',(-16.2101833131975,18.7739789263039,
11.8551995796215));
#134022=CARTESIAN_POINT('Ctrl Pts',(-16.2258835179279,18.6913692935071,
11.8593733844208));
#134023=CARTESIAN_POINT('Ctrl Pts',(-16.2456263033231,18.6096711833892,
11.8635471892201));
#134024=CARTESIAN_POINT('Ctrl Pts',(-16.2653562958445,18.5280260117797,
11.8677182894893));
#134025=CARTESIAN_POINT('Ctrl Pts',(-16.2891235604505,18.4472916360286,
11.8718893897585));
#134026=CARTESIAN_POINT('Ctrl Pts',(-16.3168179573514,18.3678920752969,
11.8760604900277));
#134027=CARTESIAN_POINT('Ctrl Pts',(-16.3445027167179,18.2885201452806,
11.8802301387714));
#134028=CARTESIAN_POINT('Ctrl Pts',(-16.3761117424971,18.2104825415902,
11.8843997875151));
#134029=CARTESIAN_POINT('Ctrl Pts',(-16.4114852391776,18.1341874881103,
11.8885694362588));
#134030=CARTESIAN_POINT('Ctrl Pts',(-16.4468570371505,18.0578960984751,
11.8927388847675));
#134031=CARTESIAN_POINT('Ctrl Pts',(-16.4859927520556,17.983347509486,11.8969083332761));
#134032=CARTESIAN_POINT('Ctrl Pts',(-16.528685277592,17.9109280884772,11.9010777817847));
#134033=CARTESIAN_POINT('Ctrl Pts',(-16.5714158514221,17.8384441260677,
11.9052509461757));
#134034=CARTESIAN_POINT('Ctrl Pts',(-16.617709334547,17.768093519667,11.9094241105667));
#134035=CARTESIAN_POINT('Ctrl Pts',(-16.6673139151783,17.7002357474429,
11.9135972749577));
#134036=CARTESIAN_POINT('Ctrl Pts',(-16.7169399758737,17.6323485910517,
11.9177722464365));
#134037=CARTESIAN_POINT('Ctrl Pts',(-16.7698797016504,17.5669567780992,
11.9219472179154));
#134038=CARTESIAN_POINT('Ctrl Pts',(-16.8258408816674,17.5043867517436,
11.9261221893943));
#134039=CARTESIAN_POINT('Ctrl Pts',(-16.8818951704667,17.4417126207399,
11.9303041072334));
#134040=CARTESIAN_POINT('Ctrl Pts',(-16.9409806348315,17.3818699858574,
11.9344860250724));
#134041=CARTESIAN_POINT('Ctrl Pts',(-17.0027682222049,17.3251483272663,
11.9386679429114));
#134042=CARTESIAN_POINT('Ctrl Pts',(-17.0579318735125,17.2745075120295,
11.9424015384));
#134043=CARTESIAN_POINT('Ctrl Pts',(-17.1152486738755,17.2263539675634,
11.9461351338886));
#134044=CARTESIAN_POINT('Ctrl Pts',(-17.174464231106,17.180864983421,11.9498687293772));
#134045=CARTESIAN_POINT('Ctrl Pts',(-17.175718110251,17.1824653653533,11.1497835165008));
#134046=CARTESIAN_POINT('Ctrl Pts',(-17.3887251657916,17.01592042969,11.1632078216932));
#134047=CARTESIAN_POINT('Ctrl Pts',(-18.377772028057,16.4618739124435,11.2190240624461));
#134048=CARTESIAN_POINT('Ctrl Pts',(-20.5048168878155,16.8048334715693,
11.3135258905415));
#134049=CARTESIAN_POINT('Ctrl Pts',(-21.2925957841654,18.43736680388,11.3946034134446));
#134050=CARTESIAN_POINT('Ctrl Pts',(-21.297413587737,19.2122806855485,11.4332890007871));
#134051=CARTESIAN_POINT('',(-21.2939995125392,19.2094201902091,11.3667098902285));
#134052=CARTESIAN_POINT('Ctrl Pts',(-17.1731949711369,17.1791828613964,
11.0834063356124));
#134053=CARTESIAN_POINT('Ctrl Pts',(-17.7502563205703,16.7443658855329,
11.119427886397));
#134054=CARTESIAN_POINT('Ctrl Pts',(-19.4306371353495,16.3338524651331,
11.1978413727421));
#134055=CARTESIAN_POINT('Ctrl Pts',(-21.0857646400936,17.7107520667789,
11.2922755723032));
#134056=CARTESIAN_POINT('Ctrl Pts',(-21.2926072565653,18.8863578111491,
11.3506882210795));
#134057=CARTESIAN_POINT('Ctrl Pts',(-21.2907952889915,19.209402892007,11.3667089342955));
#134058=CARTESIAN_POINT('Ctrl Pts',(-21.2939995125392,19.2094201902091,
11.3667098902285));
#134059=CARTESIAN_POINT('Ctrl Pts',(-21.2940518853803,19.2942876523606,
11.3709134538372));
#134060=CARTESIAN_POINT('Ctrl Pts',(-21.2898797137862,19.3791700299233,
11.3751170174459));
#134061=CARTESIAN_POINT('Ctrl Pts',(-21.2815050782104,19.4636220031829,
11.3793205810546));
#134062=CARTESIAN_POINT('Ctrl Pts',(-21.2731292177987,19.5480863280015,
11.3835247594572));
#134063=CARTESIAN_POINT('Ctrl Pts',(-21.2605497166712,19.6321196761629,
11.3877289378599));
#134064=CARTESIAN_POINT('Ctrl Pts',(-21.2438404672875,19.7152824890537,
11.3919331162626));
#134065=CARTESIAN_POINT('Ctrl Pts',(-21.2271240709727,19.7984808725961,
11.3961390928892));
#134066=CARTESIAN_POINT('Ctrl Pts',(-21.2062745049673,19.880807540606,11.4003450695159));
#134067=CARTESIAN_POINT('Ctrl Pts',(-21.1814163656275,19.9618349574033,
11.4045510461425));
#134068=CARTESIAN_POINT('Ctrl Pts',(-21.1565238219895,20.0429745182095,
11.408762843948));
#134069=CARTESIAN_POINT('Ctrl Pts',(-21.1276117659035,20.1228108093803,
11.4129746417534));
#134070=CARTESIAN_POINT('Ctrl Pts',(-21.0948539828414,20.2009335693377,
11.4171864395589));
#134071=CARTESIAN_POINT('Ctrl Pts',(-21.0620694457195,20.2791201340097,
11.4214016772397));
#134072=CARTESIAN_POINT('Ctrl Pts',(-21.0254331231615,20.3555899771933,
11.4256169149205));
#134073=CARTESIAN_POINT('Ctrl Pts',(-20.9851650013542,20.4299569872141,
11.4298321526013));
#134074=CARTESIAN_POINT('Ctrl Pts',(-20.9448260993909,20.5044547137502,
11.4340547994973));
#134075=CARTESIAN_POINT('Ctrl Pts',(-20.9008428915854,20.5768418481601,
11.4382774463933));
#134076=CARTESIAN_POINT('Ctrl Pts',(-20.8534787082554,20.6467611240217,
11.4425000932893));
#134077=CARTESIAN_POINT('Ctrl Pts',(-20.8410561777284,20.6650993339886,
11.4436075959693));
#134078=CARTESIAN_POINT('Ctrl Pts',(-20.8284012848672,20.6832679625288,
11.4447150986492));
#134079=CARTESIAN_POINT('Ctrl Pts',(-20.8155192213964,20.7012609606902,
11.4458226013291));
#134080=CARTESIAN_POINT('Ctrl Pts',(-20.7668450946151,20.7692464566218,
11.4500072357222));
#134081=CARTESIAN_POINT('Ctrl Pts',(-20.7147461245074,20.8349713096213,
11.4541918701152));
#134082=CARTESIAN_POINT('Ctrl Pts',(-20.6594597008472,20.8980699275411,
11.4583765045082));
#134083=CARTESIAN_POINT('Ctrl Pts',(-20.6042519705679,20.9610787323882,
11.4625551825922));
#134084=CARTESIAN_POINT('Ctrl Pts',(-20.5458660991118,21.0214683841929,
11.4667338606761));
#134085=CARTESIAN_POINT('Ctrl Pts',(-20.4845818988862,21.0789033741851,
11.4709125387601));
#134086=CARTESIAN_POINT('Ctrl Pts',(-20.4221992234157,21.1373678450951,
11.4751661166455));
#134087=CARTESIAN_POINT('Ctrl Pts',(-20.356813572753,21.1927702956727,11.4794196945309));
#134088=CARTESIAN_POINT('Ctrl Pts',(-20.2887620518457,21.2447932446885,
11.4836732724164));
#134089=CARTESIAN_POINT('Ctrl Pts',(-20.2220298424627,21.2958076273232,
11.4878443863943));
#134090=CARTESIAN_POINT('Ctrl Pts',(-20.1527345889113,21.3435720832561,
11.4920155003723));
#134091=CARTESIAN_POINT('Ctrl Pts',(-20.0812289339452,21.3878266351597,
11.4961866143502));
#134092=CARTESIAN_POINT('Ctrl Pts',(-20.0097472733923,21.4320663370211,
11.5003563286706));
#134093=CARTESIAN_POINT('Ctrl Pts',(-19.9360570753465,21.4727982320514,
11.504526042991));
#134094=CARTESIAN_POINT('Ctrl Pts',(-19.860539605792,21.5098058892786,11.5086957573113));
#134095=CARTESIAN_POINT('Ctrl Pts',(-19.7850248234731,21.5468122296146,
11.5128653232554));
#134096=CARTESIAN_POINT('Ctrl Pts',(-19.7076833123974,21.5800943939657,
11.5170348891994));
#134097=CARTESIAN_POINT('Ctrl Pts',(-19.6289193227221,21.6094827299396,
11.5212044551435));
#134098=CARTESIAN_POINT('Ctrl Pts',(-19.5473860883357,21.639904323552,11.5255206178824));
#134099=CARTESIAN_POINT('Ctrl Pts',(-19.4643289796732,21.6661529958306,
11.5298367806213));
#134100=CARTESIAN_POINT('Ctrl Pts',(-19.3802151086566,21.6880962906887,
11.5341529433602));
#134101=CARTESIAN_POINT('Ctrl Pts',(-19.2988412381411,21.7093247850249,
11.5383285075519));
#134102=CARTESIAN_POINT('Ctrl Pts',(-19.2164788667996,21.7265240396988,
11.5425040717436));
#134103=CARTESIAN_POINT('Ctrl Pts',(-19.1335609462714,21.7396263168398,
11.5466796359353));
#134104=CARTESIAN_POINT('Ctrl Pts',(-19.0464550386958,21.7533903588514,
11.5510660979478));
#134105=CARTESIAN_POINT('Ctrl Pts',(-18.9587365661208,21.7626326086006,
11.5554525599603));
#134106=CARTESIAN_POINT('Ctrl Pts',(-18.8709107816374,21.7673363311332,
11.5598390219729));
#134107=CARTESIAN_POINT('Ctrl Pts',(-18.7830849971541,21.7720400536657,
11.5642254839854));
#134108=CARTESIAN_POINT('Ctrl Pts',(-18.6951524811213,21.7722053239559,
11.568611945998));
#134109=CARTESIAN_POINT('Ctrl Pts',(-18.6076132463771,21.7678782506229,
11.5729984080105));
#134110=CARTESIAN_POINT('Ctrl Pts',(-18.5241018215878,21.7637502723483,
11.5771830424035));
#134111=CARTESIAN_POINT('Ctrl Pts',(-18.4406374370146,21.7555188996868,
11.5813676767966));
#134112=CARTESIAN_POINT('Ctrl Pts',(-18.3576559923796,21.7431858517747,
11.5855523111896));
#134113=CARTESIAN_POINT('Ctrl Pts',(-18.2747926615599,21.7308703584299,
11.5897309892736));
#134114=CARTESIAN_POINT('Ctrl Pts',(-18.192411356418,21.7144648534413,11.5939096673575));
#134115=CARTESIAN_POINT('Ctrl Pts',(-18.1109456438834,21.6940230102285,
11.5980883454415));
#134116=CARTESIAN_POINT('Ctrl Pts',(-18.028019717,21.6732147616674,11.6023419233269));
#134117=CARTESIAN_POINT('Ctrl Pts',(-17.9460430111254,21.6482240726707,
11.6065955012123));
#134118=CARTESIAN_POINT('Ctrl Pts',(-17.8654649462453,21.6191625485833,
11.6108490790978));
#134119=CARTESIAN_POINT('Ctrl Pts',(-17.786449044388,21.5906644388492,11.6150201930757));
#134120=CARTESIAN_POINT('Ctrl Pts',(-17.7087784893785,21.5582520908959,
11.6191913070537));
#134121=CARTESIAN_POINT('Ctrl Pts',(-17.632862759841,21.5220813006762,11.6233624210316));
#134122=CARTESIAN_POINT('Ctrl Pts',(-17.5569725045598,21.4859226479144,
11.627532135352));
#134123=CARTESIAN_POINT('Ctrl Pts',(-17.4828363202444,21.4460082553229,
11.6317018496724));
#134124=CARTESIAN_POINT('Ctrl Pts',(-17.4108425631371,21.4025415572775,
11.6358715639928));
#134125=CARTESIAN_POINT('Ctrl Pts',(-17.3388513678768,21.3590764059638,
11.6400411299368));
#134126=CARTESIAN_POINT('Ctrl Pts',(-17.2690028416267,21.3120594390257,
11.6442106958808));
#134127=CARTESIAN_POINT('Ctrl Pts',(-17.2016584481436,21.2617387372491,
11.6483802618249));
#134128=CARTESIAN_POINT('Ctrl Pts',(-17.1319463088639,21.2096488216754,
11.6526964245638));
#134129=CARTESIAN_POINT('Ctrl Pts',(-17.0649180918037,21.1540188458217,
11.6570125873027));
#134130=CARTESIAN_POINT('Ctrl Pts',(-17.0009380103942,21.0951698809246,
11.6613287500416));
#134131=CARTESIAN_POINT('Ctrl Pts',(-16.9390420734071,21.0382379148692,
11.6655043142333));
#134132=CARTESIAN_POINT('Ctrl Pts',(-16.8799990325861,20.9782938250442,
11.669679878425));
#134133=CARTESIAN_POINT('Ctrl Pts',(-16.8241001932717,20.9156649900374,
11.6738554426167));
#134134=CARTESIAN_POINT('Ctrl Pts',(-16.7653780364704,20.8498729214603,
11.6782419046292));
#134135=CARTESIAN_POINT('Ctrl Pts',(-16.7101264215567,20.7811182222701,
11.6826283666418));
#134136=CARTESIAN_POINT('Ctrl Pts',(-16.658632903894,20.7098166720451,11.6870148286543));
#134137=CARTESIAN_POINT('Ctrl Pts',(-16.6071393862313,20.6385151218201,
11.6914012906668));
#134138=CARTESIAN_POINT('Ctrl Pts',(-16.5594042169154,20.5646672491325,
11.6957877526794));
#134139=CARTESIAN_POINT('Ctrl Pts',(-16.5156592733602,20.4887184433712,
11.7001742146919));
#134140=CARTESIAN_POINT('Ctrl Pts',(-16.4739270995035,20.4162641547462,
11.704358849085));
#134141=CARTESIAN_POINT('Ctrl Pts',(-16.4356706929266,20.341628329944,11.708543483478));
#134142=CARTESIAN_POINT('Ctrl Pts',(-16.4011245523601,20.2651784221843,
11.712728117871));
#134143=CARTESIAN_POINT('Ctrl Pts',(-16.3666275839488,20.1888373314056,
11.716906795955));
#134144=CARTESIAN_POINT('Ctrl Pts',(-16.3358305794285,20.1106877022102,
11.7210854740389));
#134145=CARTESIAN_POINT('Ctrl Pts',(-16.3089230895031,20.0311231481764,
11.7252641521229));
#134146=CARTESIAN_POINT('Ctrl Pts',(-16.2815333021588,19.9501324566934,
11.7295177300083));
#134147=CARTESIAN_POINT('Ctrl Pts',(-16.258174080664,19.8676760341798,11.7337713078937));
#134148=CARTESIAN_POINT('Ctrl Pts',(-16.2389948450999,19.7841921815778,
11.7380248857792));
#134149=CARTESIAN_POINT('Ctrl Pts',(-16.2201874364424,19.7023268263638,
11.7421959997571));
#134150=CARTESIAN_POINT('Ctrl Pts',(-16.2053994934178,19.6194739920343,
11.7463671137351));
#134151=CARTESIAN_POINT('Ctrl Pts',(-16.194721659298,19.5360623147054,11.750538227713));
#134152=CARTESIAN_POINT('Ctrl Pts',(-16.1840474082286,19.4526786269704,
11.7547079420334));
#134153=CARTESIAN_POINT('Ctrl Pts',(-16.1774805853424,19.3687369245934,
11.7588776563538));
#134154=CARTESIAN_POINT('Ctrl Pts',(-16.1750603443919,19.2846738688846,
11.7630473706742));
#134155=CARTESIAN_POINT('Ctrl Pts',(-16.172640189564,19.2006138044999,11.7672169366182));
#134156=CARTESIAN_POINT('Ctrl Pts',(-16.1743663356855,19.1164328552362,
11.7713865025623));
#134157=CARTESIAN_POINT('Ctrl Pts',(-16.1802258395509,19.0325692363341,
11.7755560685063));
#134158=CARTESIAN_POINT('Ctrl Pts',(-16.1862913563437,18.9457570760484,
11.7798722312452));
#134159=CARTESIAN_POINT('Ctrl Pts',(-16.1967862597981,18.8592855021224,
11.7841883939841));
#134160=CARTESIAN_POINT('Ctrl Pts',(-16.2116377216372,18.7736345501844,
11.7885045567231));
#134161=CARTESIAN_POINT('Ctrl Pts',(-16.226005398669,18.690773668997,11.7926801209147));
#134162=CARTESIAN_POINT('Ctrl Pts',(-16.2444500136974,18.6086812165377,
11.7968556851064));
#134163=CARTESIAN_POINT('Ctrl Pts',(-16.2668539711945,18.527779338318,11.8010312492981));
#134164=CARTESIAN_POINT('Ctrl Pts',(-16.2903894993245,18.4427912985553,
11.8054177113106));
#134165=CARTESIAN_POINT('Ctrl Pts',(-16.3182946694534,18.3591178195347,
11.8098041733232));
#134166=CARTESIAN_POINT('Ctrl Pts',(-16.3503755250187,18.2772257434102,
11.8141906353357));
#134167=CARTESIAN_POINT('Ctrl Pts',(-16.382456380584,18.1953336672856,11.8185770973483));
#134168=CARTESIAN_POINT('Ctrl Pts',(-16.4187126130535,18.1152234912951,
11.8229635593608));
#134169=CARTESIAN_POINT('Ctrl Pts',(-16.4588952312817,18.0373312684769,
11.8273500213734));
#134170=CARTESIAN_POINT('Ctrl Pts',(-16.497232190989,17.9630167728226,11.8315350054498));
#134171=CARTESIAN_POINT('Ctrl Pts',(-16.5392854659847,17.8904443146189,
11.8357199895262));
#134172=CARTESIAN_POINT('Ctrl Pts',(-16.5848729683162,17.8200100641321,
11.8399049736025));
#134173=CARTESIAN_POINT('Ctrl Pts',(-16.6303841734332,17.7496936954514,
11.8440829535087));
#134174=CARTESIAN_POINT('Ctrl Pts',(-16.679417597685,17.6815088023829,11.8482609334148));
#134175=CARTESIAN_POINT('Ctrl Pts',(-16.7317449889595,17.6158276360332,
11.852438913321));
#134176=CARTESIAN_POINT('Ctrl Pts',(-16.784021729639,17.5502100461409,11.8566128491278));
#134177=CARTESIAN_POINT('Ctrl Pts',(-16.8395858226251,17.4870917295056,
11.8607867849346));
#134178=CARTESIAN_POINT('Ctrl Pts',(-16.8981658619793,17.4268158677766,
11.8649607207414));
#134179=CARTESIAN_POINT('Ctrl Pts',(-16.9567039826102,17.366583138268,11.8691316697619));
#134180=CARTESIAN_POINT('Ctrl Pts',(-17.018253441943,17.3091891512907,11.8733026187824));
#134181=CARTESIAN_POINT('Ctrl Pts',(-17.0825036449284,17.2549427950121,
11.8774735678028));
#134182=CARTESIAN_POINT('Ctrl Pts',(-17.1125775158831,17.2295514679395,
11.8794258819866));
#134183=CARTESIAN_POINT('Ctrl Pts',(-17.1432425623528,17.2048492548057,
11.8813781961704));
#134184=CARTESIAN_POINT('Ctrl Pts',(-17.174464231106,17.180864983421,11.8833305103542));
#134185=CARTESIAN_POINT('Origin',(-18.734,19.211,-1.76670989022852));
#134186=CARTESIAN_POINT('',(-17.174464231106,17.180864983421,12.7499597594996));
#134187=CARTESIAN_POINT('',(-17.175049467869,17.1816082633957,12.6831923912068));
#134188=CARTESIAN_POINT('',(-17.174464231106,17.180864983421,-1.76670989022852));
#134189=CARTESIAN_POINT('',(-21.2939989766127,19.2087109517328,12.2332901098107));
#134190=CARTESIAN_POINT('Ctrl Pts',(-21.2939989766127,19.2087109517328,
12.2332901098107));
#134191=CARTESIAN_POINT('Ctrl Pts',(-21.2940747905548,19.2934988599292,
12.2375129674107));
#134192=CARTESIAN_POINT('Ctrl Pts',(-21.2899336304853,19.3784221563149,
12.2417358250107));
#134193=CARTESIAN_POINT('Ctrl Pts',(-21.2815646644668,19.4630203967141,
12.2459586826108));
#134194=CARTESIAN_POINT('Ctrl Pts',(-21.2734134565487,19.5454174151129,
12.2500716626647));
#134195=CARTESIAN_POINT('Ctrl Pts',(-21.2612518149666,19.6275055813485,
12.2541846427187));
#134196=CARTESIAN_POINT('Ctrl Pts',(-21.2451224198776,19.7088596111236,
12.2582976227727));
#134197=CARTESIAN_POINT('Ctrl Pts',(-21.2290007459442,19.7901746966529,
12.2624086339395));
#134198=CARTESIAN_POINT('Ctrl Pts',(-21.20891517906,19.8707558783839,12.2665196451063));
#134199=CARTESIAN_POINT('Ctrl Pts',(-21.18495989447,19.9501857653523,12.2706306562731));
#134200=CARTESIAN_POINT('Ctrl Pts',(-21.1610084101081,20.0296030516903,
12.2747410152757));
#134201=CARTESIAN_POINT('Ctrl Pts',(-21.1331885645307,20.1078689519367,
12.2788513742782));
#134202=CARTESIAN_POINT('Ctrl Pts',(-21.1016446063279,20.184580514455,12.2829617332808));
#134203=CARTESIAN_POINT('Ctrl Pts',(-21.0685960771618,20.2649510340633,
12.2872681465249));
#134204=CARTESIAN_POINT('Ctrl Pts',(-21.0314595036716,20.3436147061448,
12.2915745597691));
#134205=CARTESIAN_POINT('Ctrl Pts',(-20.9904568914614,20.4201328698601,
12.2958809730133));
#134206=CARTESIAN_POINT('Ctrl Pts',(-20.9512718262788,20.4932591677037,
12.2999964933322));
#134207=CARTESIAN_POINT('Ctrl Pts',(-20.9085564982548,20.5644257408166,
12.304112013651));
#134208=CARTESIAN_POINT('Ctrl Pts',(-20.8625501361321,20.6332778624348,
12.3082275339699));
#134209=CARTESIAN_POINT('Ctrl Pts',(-20.8165130556112,20.70217595654,12.3123458022172));
#134210=CARTESIAN_POINT('Ctrl Pts',(-20.7671808550876,20.768756147345,12.3164640704645));
#134211=CARTESIAN_POINT('Ctrl Pts',(-20.7148334041511,20.8326963417974,
12.3205823387118));
#134212=CARTESIAN_POINT('Ctrl Pts',(-20.662405465351,20.8967348487665,12.3247069390843));
#134213=CARTESIAN_POINT('Ctrl Pts',(-20.6069533520093,20.9581249187391,
12.3288315394568));
#134214=CARTESIAN_POINT('Ctrl Pts',(-20.5487934990216,21.0165815007661,
12.3329561398293));
#134215=CARTESIAN_POINT('Ctrl Pts',(-20.5408850965646,21.0245302515484,
12.3335169906232));
#134216=CARTESIAN_POINT('Ctrl Pts',(-20.5329266770598,21.0324248251517,
12.3340778414171));
#134217=CARTESIAN_POINT('Ctrl Pts',(-20.5249190804941,21.040264564551,12.334638692211));
#134218=CARTESIAN_POINT('Ctrl Pts',(-20.4651725946906,21.0987586301398,
12.338823326604));
#134219=CARTESIAN_POINT('Ctrl Pts',(-20.4024461555817,21.154431359773,12.3430079609971));
#134220=CARTESIAN_POINT('Ctrl Pts',(-20.3370370650428,21.2069639696395,
12.3471925953901));
#134221=CARTESIAN_POINT('Ctrl Pts',(-20.2717210762482,21.2594218058381,
12.3513712734741));
#134222=CARTESIAN_POINT('Ctrl Pts',(-20.2037303762194,21.3087481146436,
12.355549951558));
#134223=CARTESIAN_POINT('Ctrl Pts',(-20.1333988170805,21.35466110912,12.3597286296419));
#134224=CARTESIAN_POINT('Ctrl Pts',(-20.0618066152904,21.4013970610254,
12.3639822075274));
#134225=CARTESIAN_POINT('Ctrl Pts',(-19.9877891536758,21.4445957903898,
12.3682357854128));
#134226=CARTESIAN_POINT('Ctrl Pts',(-19.9117335730787,21.484003218397,12.3724893632982));
#134227=CARTESIAN_POINT('Ctrl Pts',(-19.8371524783218,21.522646656515,12.3766604772762));
#134228=CARTESIAN_POINT('Ctrl Pts',(-19.7606120124672,21.5576442636059,
12.3808315912541));
#134229=CARTESIAN_POINT('Ctrl Pts',(-19.6825046263017,21.5888012898231,
12.3850027052321));
#134230=CARTESIAN_POINT('Ctrl Pts',(-19.604423449824,21.6199478609992,12.3891724195525));
#134231=CARTESIAN_POINT('Ctrl Pts',(-19.5247768242091,21.647256240463,12.3933421338728));
#134232=CARTESIAN_POINT('Ctrl Pts',(-19.4439778217473,21.6705795357392,
12.3975118481932));
#134233=CARTESIAN_POINT('Ctrl Pts',(-19.3631816944607,21.6939020010724,
12.4016814141372));
#134234=CARTESIAN_POINT('Ctrl Pts',(-19.2812337140823,21.7132395374009,
12.4058509800813));
#134235=CARTESIAN_POINT('Ctrl Pts',(-19.1985614595127,21.7284953128726,
12.4100205460253));
#134236=CARTESIAN_POINT('Ctrl Pts',(-19.1129825504594,21.7442874625898,
12.4143367087642));
#134237=CARTESIAN_POINT('Ctrl Pts',(-19.0266280073019,21.7557053858608,
12.4186528715032));
#134238=CARTESIAN_POINT('Ctrl Pts',(-18.9399808515258,21.762699803818,12.4229690342421));
#134239=CARTESIAN_POINT('Ctrl Pts',(-18.8561562177354,21.7694663793458,
12.4271445984338));
#134240=CARTESIAN_POINT('Ctrl Pts',(-18.7720582145672,21.7720932477196,
12.4313201626254));
#134241=CARTESIAN_POINT('Ctrl Pts',(-18.6881249777991,21.7705889283903,
12.4354957268171));
#134242=CARTESIAN_POINT('Ctrl Pts',(-18.599952472774,21.7690086294678,12.4398821888297));
#134243=CARTESIAN_POINT('Ctrl Pts',(-18.5119623987479,21.7628688832023,
12.4442686508422));
#134244=CARTESIAN_POINT('Ctrl Pts',(-18.4246552312348,21.7522409988109,
12.4486551128548));
#134245=CARTESIAN_POINT('Ctrl Pts',(-18.3373480637217,21.7416131144196,
12.4530415748673));
#134246=CARTESIAN_POINT('Ctrl Pts',(-18.2507243612258,21.7264972665759,
12.4574280368799));
#134247=CARTESIAN_POINT('Ctrl Pts',(-18.1652685194105,21.7070257416514,
12.4618144988924));
#134248=CARTESIAN_POINT('Ctrl Pts',(-18.0837446275532,21.6884501304525,
12.4659991332855));
#134249=CARTESIAN_POINT('Ctrl Pts',(-18.0029800405435,21.6658417144697,
12.4701837676785));
#134250=CARTESIAN_POINT('Ctrl Pts',(-17.9234037289843,21.6392779259005,
12.4743684020716));
#134251=CARTESIAN_POINT('Ctrl Pts',(-17.8439406844549,21.6127519475962,
12.4785470801555));
#134252=CARTESIAN_POINT('Ctrl Pts',(-17.7656629884269,21.5822819240424,
12.4827257582395));
#134253=CARTESIAN_POINT('Ctrl Pts',(-17.6889882869427,21.5479960461184,
12.4869044363234));
#134254=CARTESIAN_POINT('Ctrl Pts',(-17.6109392465396,21.5130956184734,
12.4911580142088));
#134255=CARTESIAN_POINT('Ctrl Pts',(-17.5345517033715,21.474241299649,12.4954115920943));
#134256=CARTESIAN_POINT('Ctrl Pts',(-17.4602488495091,21.4316210857828,
12.4996651699797));
#134257=CARTESIAN_POINT('Ctrl Pts',(-17.3873865014589,21.3898271479288,
12.5038362839577));
#134258=CARTESIAN_POINT('Ctrl Pts',(-17.3165291499246,21.3444122698725,
12.5080073979356));
#134259=CARTESIAN_POINT('Ctrl Pts',(-17.2480529748745,21.2956010262208,
12.5121785119136));
#134260=CARTESIAN_POINT('Ctrl Pts',(-17.1795997776663,21.2468061616532,
12.5163482262339));
#134261=CARTESIAN_POINT('Ctrl Pts',(-17.1135265443543,21.1946174617221,
12.5205179405543));
#134262=CARTESIAN_POINT('Ctrl Pts',(-17.0501803764602,21.1393027447427,
12.5246876548747));
#134263=CARTESIAN_POINT('Ctrl Pts',(-16.9868364626946,21.0839899960983,
12.5288572208187));
#134264=CARTESIAN_POINT('Ctrl Pts',(-16.9262197673613,21.0255517547983,
12.5330267867628));
#134265=CARTESIAN_POINT('Ctrl Pts',(-16.8686431510732,20.9642951337872,
12.5371963527068));
#134266=CARTESIAN_POINT('Ctrl Pts',(-16.8090422119848,20.9008848055495,
12.5415125154458));
#134267=CARTESIAN_POINT('Ctrl Pts',(-16.7526994690718,20.8344546059654,
12.5458286781847));
#134268=CARTESIAN_POINT('Ctrl Pts',(-16.6999178084323,20.765384005948,12.5501448409236));
#134269=CARTESIAN_POINT('Ctrl Pts',(-16.6488555048364,20.6985633734612,
12.5543204051153));
#134270=CARTESIAN_POINT('Ctrl Pts',(-16.6011260701748,20.6292721356224,
12.558495969307));
#134271=CARTESIAN_POINT('Ctrl Pts',(-16.5569594955243,20.5578833067018,
12.5626715334986));
#134272=CARTESIAN_POINT('Ctrl Pts',(-16.5105621721842,20.4828887977433,
12.5670579955112));
#134273=CARTESIAN_POINT('Ctrl Pts',(-16.4680973689511,20.4055797420145,
12.5714444575237));
#134274=CARTESIAN_POINT('Ctrl Pts',(-16.4297760239617,20.3264155585477,
12.5758309195363));
#134275=CARTESIAN_POINT('Ctrl Pts',(-16.3914546789723,20.2472513750809,
12.5802173815488));
#134276=CARTESIAN_POINT('Ctrl Pts',(-16.3572769476616,20.166232628037,12.5846038435613));
#134277=CARTESIAN_POINT('Ctrl Pts',(-16.3273937923111,20.0838382216157,
12.5889903055739));
#134278=CARTESIAN_POINT('Ctrl Pts',(-16.2988856052357,20.0052349039716,
12.5931749399669));
#134279=CARTESIAN_POINT('Ctrl Pts',(-16.274179366091,19.9250871608005,12.59735957436));
#134280=CARTESIAN_POINT('Ctrl Pts',(-16.2534421603042,19.8437976010731,
12.601544208753));
#134281=CARTESIAN_POINT('Ctrl Pts',(-16.2327344713631,19.7626237469723,
12.605722886837));
#134282=CARTESIAN_POINT('Ctrl Pts',(-16.2159847069801,19.6803117464869,
12.6099015649209));
#134283=CARTESIAN_POINT('Ctrl Pts',(-16.2033111427938,19.5972821611362,
12.6140802430049));
#134284=CARTESIAN_POINT('Ctrl Pts',(-16.1904104140777,19.5127643301403,
12.6183338208903));
#134285=CARTESIAN_POINT('Ctrl Pts',(-16.1817336190672,19.4275033890774,
12.6225873987757));
#134286=CARTESIAN_POINT('Ctrl Pts',(-16.177351748603,19.3419569342512,12.6268409766612));
#134287=CARTESIAN_POINT('Ctrl Pts',(-16.1730548292483,19.2580689643819,
12.6310120906391));
#134288=CARTESIAN_POINT('Ctrl Pts',(-16.1728878141637,19.17390693303,12.6351832046171));
#134289=CARTESIAN_POINT('Ctrl Pts',(-16.1768654907269,19.0899087059923,
12.639354318595));
#134290=CARTESIAN_POINT('Ctrl Pts',(-16.1808418325422,19.0059386653711,
12.6435240329154));
#134291=CARTESIAN_POINT('Ctrl Pts',(-16.1889600821296,18.922132779036,12.6476937472358));
#134292=CARTESIAN_POINT('Ctrl Pts',(-16.2011829261395,18.8389278694113,
12.6518634615561));
#134293=CARTESIAN_POINT('Ctrl Pts',(-16.2134053352083,18.7557259205741,
12.6560330275002));
#134294=CARTESIAN_POINT('Ctrl Pts',(-16.229731980592,18.673125360952,12.6602025934442));
#134295=CARTESIAN_POINT('Ctrl Pts',(-16.250073974422,18.5915554912211,12.6643721593883));
#134296=CARTESIAN_POINT('Ctrl Pts',(-16.2711311676606,18.5071177254978,
12.6686883221272));
#134297=CARTESIAN_POINT('Ctrl Pts',(-16.2964911945897,18.4237849880537,
12.6730044848661));
#134298=CARTESIAN_POINT('Ctrl Pts',(-16.3259989267241,18.3420173585728,
12.677320647605));
#134299=CARTESIAN_POINT('Ctrl Pts',(-16.3545454475878,18.2629133010218,
12.6814962117967));
#134300=CARTESIAN_POINT('Ctrl Pts',(-16.3869733753121,18.1852743669884,
12.6856717759884));
#134301=CARTESIAN_POINT('Ctrl Pts',(-16.4230935537342,18.1094958481208,
12.6898473401801));
#134302=CARTESIAN_POINT('Ctrl Pts',(-16.4610380765009,18.0298899364114,
12.6942338021926));
#134303=CARTESIAN_POINT('Ctrl Pts',(-16.5030573653642,17.9523378315092,
12.6986202642051));
#134304=CARTESIAN_POINT('Ctrl Pts',(-16.5488792984353,17.8772655738142,
12.7030067262177));
#134305=CARTESIAN_POINT('Ctrl Pts',(-16.5947012315064,17.8021933161192,
12.7073931882302));
#134306=CARTESIAN_POINT('Ctrl Pts',(-16.6443254185491,17.7296013416972,
12.7117796502428));
#134307=CARTESIAN_POINT('Ctrl Pts',(-16.6974308899397,17.6598758076968,
12.7161661122553));
#134308=CARTESIAN_POINT('Ctrl Pts',(-16.7480908287733,17.5933611681483,
12.7203505755777));
#134309=CARTESIAN_POINT('Ctrl Pts',(-16.8021070326387,17.5292072036809,
12.7245350389001));
#134310=CARTESIAN_POINT('Ctrl Pts',(-16.8592314426079,17.4677722879056,
12.7287195022225));
#134311=CARTESIAN_POINT('Ctrl Pts',(-16.916267765385,17.4064321062243,12.7328975130034));
#134312=CARTESIAN_POINT('Ctrl Pts',(-16.9764024587933,17.3478029746755,
12.7370755237843));
#134313=CARTESIAN_POINT('Ctrl Pts',(-17.0393460611034,17.2922118336351,
12.7412535345652));
#134314=CARTESIAN_POINT('Ctrl Pts',(-17.083067119491,17.2535978453334,12.7441556095433));
#134315=CARTESIAN_POINT('Ctrl Pts',(-17.1281425218688,17.2164490021399,
12.7470576845215));
#134316=CARTESIAN_POINT('Ctrl Pts',(-17.174464231106,17.180864983421,12.7499597594996));
#134317=CARTESIAN_POINT('Ctrl Pts',(-17.174464231106,17.180864983421,11.9498687293772));
#134318=CARTESIAN_POINT('Ctrl Pts',(-17.1916066861211,17.1676962672793,
11.9509495769737));
#134319=CARTESIAN_POINT('Ctrl Pts',(-17.2089081586167,17.1547506759101,
11.9520304245702));
#134320=CARTESIAN_POINT('Ctrl Pts',(-17.2263622218886,17.142032061628,11.9531112721667));
#134321=CARTESIAN_POINT('Ctrl Pts',(-17.2939377743557,17.0927903822928,
11.9572959065597));
#134322=CARTESIAN_POINT('Ctrl Pts',(-17.3640540780912,17.0467712239068,
11.9614805409528));
#134323=CARTESIAN_POINT('Ctrl Pts',(-17.436370866589,17.0042470387189,11.9656651753458));
#134324=CARTESIAN_POINT('Ctrl Pts',(-17.5085847210894,16.9617833814452,
11.9698438534298));
#134325=CARTESIAN_POINT('Ctrl Pts',(-17.5829924458182,16.9228050473159,
11.9740225315137));
#134326=CARTESIAN_POINT('Ctrl Pts',(-17.6592229568398,16.8875425961521,
11.9782012095977));
#134327=CARTESIAN_POINT('Ctrl Pts',(-17.7368198449856,16.8516480908938,
11.9824547874831));
#134328=CARTESIAN_POINT('Ctrl Pts',(-17.8163051194015,16.8196042772378,
11.9867083653685));
#134329=CARTESIAN_POINT('Ctrl Pts',(-17.8972589731899,16.7916065937817,
11.990961943254));
#134330=CARTESIAN_POINT('Ctrl Pts',(-17.9766433785542,16.7641517000523,
11.9951330572319));
#134331=CARTESIAN_POINT('Ctrl Pts',(-18.0574394740945,16.7405876095593,
11.9993041712099));
#134332=CARTESIAN_POINT('Ctrl Pts',(-18.1392307762334,16.721050287564,12.0034752851878));
#134333=CARTESIAN_POINT('Ctrl Pts',(-18.220994632511,16.7015195215058,12.0076449995082));
#134334=CARTESIAN_POINT('Ctrl Pts',(-18.3037525850822,16.6860129471901,
12.0118147138286));
#134335=CARTESIAN_POINT('Ctrl Pts',(-18.387074664491,16.6746161939521,12.015984428149));
#134336=CARTESIAN_POINT('Ctrl Pts',(-18.4703937789427,16.6632198462596,
12.020153994093));
#134337=CARTESIAN_POINT('Ctrl Pts',(-18.5542765244151,16.6559330903703,
12.024323560037));
#134338=CARTESIAN_POINT('Ctrl Pts',(-18.6382858147576,16.6527899236491,
12.0284931259811));
#134339=CARTESIAN_POINT('Ctrl Pts',(-18.7252487681119,16.6495362470634,
12.03280928872));
#134340=CARTESIAN_POINT('Ctrl Pts',(-18.8123468034839,16.6507229779045,
12.0371254514589));
#134341=CARTESIAN_POINT('Ctrl Pts',(-18.8990948495912,16.6563290445464,
12.0414416141978));
#134342=CARTESIAN_POINT('Ctrl Pts',(-18.9830170872209,16.6617524941571,
12.0456171783895));
#134343=CARTESIAN_POINT('Ctrl Pts',(-19.0666113245962,16.6713116809417,
12.0497927425812));
#134344=CARTESIAN_POINT('Ctrl Pts',(-19.1494452607508,16.6849348315375,
12.0539683067729));
#134345=CARTESIAN_POINT('Ctrl Pts',(-19.2364629421015,16.6992460550839,
12.0583547687854));
#134346=CARTESIAN_POINT('Ctrl Pts',(-19.3226409276425,16.7180424488712,
12.062741230798));
#134347=CARTESIAN_POINT('Ctrl Pts',(-19.4074943094425,16.7411810966898,
12.0671276928105));
#134348=CARTESIAN_POINT('Ctrl Pts',(-19.4923476912424,16.7643197445083,
12.071514154823));
#134349=CARTESIAN_POINT('Ctrl Pts',(-19.5758759419184,16.7918003927741,
12.0759006168356));
#134350=CARTESIAN_POINT('Ctrl Pts',(-19.6576188802165,16.8234221134992,
12.0802870788481));
#134351=CARTESIAN_POINT('Ctrl Pts',(-19.7356007047514,16.8535888719792,
12.0844717132412));
#134352=CARTESIAN_POINT('Ctrl Pts',(-19.8122481596155,16.8876362896631,
12.0886563476342));
#134353=CARTESIAN_POINT('Ctrl Pts',(-19.8871479757777,16.9254257295026,
12.0928409820273));
#134354=CARTESIAN_POINT('Ctrl Pts',(-19.9619411813225,16.9631613807519,
12.0970196601112));
#134355=CARTESIAN_POINT('Ctrl Pts',(-20.0349912820117,17.0046282689895,
12.1011983381951));
#134356=CARTESIAN_POINT('Ctrl Pts',(-20.1059035528266,17.0496391690091,
12.1053770162791));
#134357=CARTESIAN_POINT('Ctrl Pts',(-20.1780868751321,17.0954568570628,
12.1096305941645));
#134358=CARTESIAN_POINT('Ctrl Pts',(-20.2480545228571,17.1449466854561,
12.11388417205));
#134359=CARTESIAN_POINT('Ctrl Pts',(-20.3154149295587,17.1978614502303,
12.1181377499354));
#134360=CARTESIAN_POINT('Ctrl Pts',(-20.3814694233333,17.2497503590347,
12.1223088639133));
#134361=CARTESIAN_POINT('Ctrl Pts',(-20.4450164884365,17.3049322938692,
12.1264799778913));
#134362=CARTESIAN_POINT('Ctrl Pts',(-20.5057163649394,17.3631306533724,
12.1306510918693));
#134363=CARTESIAN_POINT('Ctrl Pts',(-20.5663958730124,17.4213094838539,
12.1348208061896));
#134364=CARTESIAN_POINT('Ctrl Pts',(-20.6242297581414,17.4825024106647,
12.13899052051));
#134365=CARTESIAN_POINT('Ctrl Pts',(-20.678913285295,17.5463942470714,12.1431602348304));
#134366=CARTESIAN_POINT('Ctrl Pts',(-20.733594866574,17.6102838099324,12.1473298007744));
#134367=CARTESIAN_POINT('Ctrl Pts',(-20.7851260142849,17.6768717413838,
12.1514993667185));
#134368=CARTESIAN_POINT('Ctrl Pts',(-20.8332415555807,17.7458089232721,
12.1556689326625));
#134369=CARTESIAN_POINT('Ctrl Pts',(-20.8830487799516,17.8171698514324,
12.1599850954014));
#134370=CARTESIAN_POINT('Ctrl Pts',(-20.9291954417205,17.8910478705134,
12.1643012581404));
#134371=CARTESIAN_POINT('Ctrl Pts',(-20.971436698905,17.9670237066595,12.1686174208793));
#134372=CARTESIAN_POINT('Ctrl Pts',(-21.0123019515797,18.0405246379345,
12.172792985071));
#134373=CARTESIAN_POINT('Ctrl Pts',(-21.0495121634691,18.1159883689943,
12.1769685492626));
#134374=CARTESIAN_POINT('Ctrl Pts',(-21.082893688299,18.1930125535797,12.1811441134543));
#134375=CARTESIAN_POINT('Ctrl Pts',(-21.117961234591,18.2739270466209,12.1855305754669));
#134376=CARTESIAN_POINT('Ctrl Pts',(-21.1488029510882,18.3565632259543,
12.1899170374794));
#134377=CARTESIAN_POINT('Ctrl Pts',(-21.1752765362398,18.4404360029143,
12.1943034994919));
#134378=CARTESIAN_POINT('Ctrl Pts',(-21.2017501213915,18.5243087798743,
12.1986899615045));
#134379=CARTESIAN_POINT('Ctrl Pts',(-21.2238555029592,18.6094175737551,
12.203076423517));
#134380=CARTESIAN_POINT('Ctrl Pts',(-21.2415125421985,18.6952666864385,
12.2074628855296));
#134381=CARTESIAN_POINT('Ctrl Pts',(-21.2654843862328,18.8118185902907,
12.2134181072291));
#134382=CARTESIAN_POINT('Ctrl Pts',(-21.2813366135111,18.9300931627089,
12.2193733289286));
#134383=CARTESIAN_POINT('Ctrl Pts',(-21.2888788651003,19.0491544419404,
12.2253285506281));
#134384=CARTESIAN_POINT('Ctrl Pts',(-21.2922399536336,19.1022122716411,
12.2279824036759));
#134385=CARTESIAN_POINT('Ctrl Pts',(-21.2939513313562,19.1554260264004,
12.2306362567237));
#134386=CARTESIAN_POINT('Ctrl Pts',(-21.293998976612,19.2087109509454,12.2332901097715));
#134387=CARTESIAN_POINT('',(-21.2939992159918,19.2130035272629,12.1667098902285));
#134388=CARTESIAN_POINT('Ctrl Pts',(-17.174464231106,17.180864983421,11.8833305103542));
#134389=CARTESIAN_POINT('Ctrl Pts',(-17.2411433188361,17.1296425664374,
11.8875000033358));
#134390=CARTESIAN_POINT('Ctrl Pts',(-17.3103631224993,17.0816975368105,
11.8916694963173));
#134391=CARTESIAN_POINT('Ctrl Pts',(-17.3817637625324,17.037280340504,11.8958389892988));
#134392=CARTESIAN_POINT('Ctrl Pts',(-17.4531714778517,16.9928587427751,
11.9000088954469));
#134393=CARTESIAN_POINT('Ctrl Pts',(-17.5267600673345,16.9519659143865,
11.904178801595));
#134394=CARTESIAN_POINT('Ctrl Pts',(-17.6021425997059,16.9148077551304,
11.9083487077431));
#134395=CARTESIAN_POINT('Ctrl Pts',(-17.677605069376,16.8776101925433,11.9125230357516));
#134396=CARTESIAN_POINT('Ctrl Pts',(-17.7548648666536,16.8441554099555,
11.91669736376));
#134397=CARTESIAN_POINT('Ctrl Pts',(-17.8335129580331,16.8146020599137,
11.9208716917685));
#134398=CARTESIAN_POINT('Ctrl Pts',(-17.9122052197822,16.7850321121088,
11.9250483641646));
#134399=CARTESIAN_POINT('Ctrl Pts',(-17.992286889851,16.7593680998778,11.9292250365607));
#134400=CARTESIAN_POINT('Ctrl Pts',(-18.073333887536,16.737718720436,11.9334017089567));
#134401=CARTESIAN_POINT('Ctrl Pts',(-18.1545199182313,16.7160322023157,
11.9375855462738));
#134402=CARTESIAN_POINT('Ctrl Pts',(-18.2366741336785,16.6983741672315,
11.9417693835909));
#134403=CARTESIAN_POINT('Ctrl Pts',(-18.3193626550843,16.6848020916403,
11.945953220908));
#134404=CARTESIAN_POINT('Ctrl Pts',(-18.3758384177107,16.6755324456675,
11.9488107566236));
#134405=CARTESIAN_POINT('Ctrl Pts',(-18.4325632674714,16.6681677378075,
11.9516682923392));
#134406=CARTESIAN_POINT('Ctrl Pts',(-18.4893986055749,16.662712308658,11.9545258280548));
#134407=CARTESIAN_POINT('Ctrl Pts',(-18.5726294499944,16.6547232653983,
11.9587104624479));
#134408=CARTESIAN_POINT('Ctrl Pts',(-18.6564069960725,16.6508013065455,
11.9628950968409));
#134409=CARTESIAN_POINT('Ctrl Pts',(-18.740299675164,16.6510077511655,11.967079731234));
#134410=CARTESIAN_POINT('Ctrl Pts',(-18.8240729434104,16.6512139019371,
11.9712584093179));
#134411=CARTESIAN_POINT('Ctrl Pts',(-18.907960563061,16.655536782935,11.9754370874018));
#134412=CARTESIAN_POINT('Ctrl Pts',(-18.9915257624718,16.6639859675174,
11.9796157654858));
#134413=CARTESIAN_POINT('Ctrl Pts',(-19.076588808025,16.6725865976611,11.9838693433712));
#134414=CARTESIAN_POINT('Ctrl Pts',(-19.1613172809479,16.6854629604527,
11.9881229212567));
#134415=CARTESIAN_POINT('Ctrl Pts',(-19.2452503475945,16.702569597919,11.9923764991421));
#134416=CARTESIAN_POINT('Ctrl Pts',(-19.3275562079622,16.7193445898371,
11.99654761312));
#134417=CARTESIAN_POINT('Ctrl Pts',(-19.4090967563144,16.7401871997923,
12.000718727098));
#134418=CARTESIAN_POINT('Ctrl Pts',(-19.4894442918863,16.7650024689595,
12.004889841076));
#134419=CARTESIAN_POINT('Ctrl Pts',(-19.5697648660668,16.7898094111234,
12.0090595553963));
#134420=CARTESIAN_POINT('Ctrl Pts',(-19.6488927833418,16.818586229372,12.0132292697167));
#134421=CARTESIAN_POINT('Ctrl Pts',(-19.7264143560957,16.8511877731872,
12.0173989840371));
#134422=CARTESIAN_POINT('Ctrl Pts',(-19.8039331702994,16.8837881568996,
12.0215685499811));
#134423=CARTESIAN_POINT('Ctrl Pts',(-19.8798453299034,16.9202128164538,
12.0257381159252));
#134424=CARTESIAN_POINT('Ctrl Pts',(-19.9537573024931,16.9602685360055,
12.0299076818692));
#134425=CARTESIAN_POINT('Ctrl Pts',(-20.0302679288587,17.0017325652425,
12.0342238446081));
#134426=CARTESIAN_POINT('Ctrl Pts',(-20.104634634367,17.0470874900865,12.0385400073471));
#134427=CARTESIAN_POINT('Ctrl Pts',(-20.1764506132334,17.0960682686236,
12.042856170086));
#134428=CARTESIAN_POINT('Ctrl Pts',(-20.2459271941418,17.1434535034518,
12.0470317342777));
#134429=CARTESIAN_POINT('Ctrl Pts',(-20.3130163291629,17.1942316733328,
12.0512072984693));
#134430=CARTESIAN_POINT('Ctrl Pts',(-20.3773824427361,17.2481209545907,
12.055382862661));
#134431=CARTESIAN_POINT('Ctrl Pts',(-20.44499953569,17.3047320553354,12.0597693246736));
#134432=CARTESIAN_POINT('Ctrl Pts',(-20.5096108706379,17.3647764140012,
12.0641557866861));
#134433=CARTESIAN_POINT('Ctrl Pts',(-20.5708718020377,17.4278841925218,
12.0685422486987));
#134434=CARTESIAN_POINT('Ctrl Pts',(-20.6321327334376,17.4909919710424,
12.0729287107112));
#134435=CARTESIAN_POINT('Ctrl Pts',(-20.6900429364134,17.5571626827011,
12.0773151727237));
#134436=CARTESIAN_POINT('Ctrl Pts',(-20.7443085775788,17.625989141074,12.0817016347363));
#134437=CARTESIAN_POINT('Ctrl Pts',(-20.796026764239,17.6915845997261,12.0858821780095));
#134438=CARTESIAN_POINT('Ctrl Pts',(-20.8446312405901,17.7598411080022,
12.0900627212828));
#134439=CARTESIAN_POINT('Ctrl Pts',(-20.8898359348525,17.8304307616065,
12.0942432645561));
#134440=CARTESIAN_POINT('Ctrl Pts',(-20.934977871844,17.9009224162288,12.0984180040186));
#134441=CARTESIAN_POINT('Ctrl Pts',(-20.9767291512529,17.9737404018926,
12.1025927434812));
#134442=CARTESIAN_POINT('Ctrl Pts',(-21.0148441174676,18.0485241457073,
12.1067674829438));
#134443=CARTESIAN_POINT('Ctrl Pts',(-21.0529176328928,18.1232265607022,
12.1109376822936));
#134444=CARTESIAN_POINT('Ctrl Pts',(-21.087362480976,18.199890080528,12.1151078816434));
#134445=CARTESIAN_POINT('Ctrl Pts',(-21.1179772351417,18.2781267276172,
12.1192780809931));
#134446=CARTESIAN_POINT('Ctrl Pts',(-21.1485693987601,18.3563056440885,
12.1234452031637));
#134447=CARTESIAN_POINT('Ctrl Pts',(-21.1753369141585,18.436054955007,12.1276123253342));
#134448=CARTESIAN_POINT('Ctrl Pts',(-21.198125670353,18.5169649283305,12.1317794475048));
#134449=CARTESIAN_POINT('Ctrl Pts',(-21.2209040463211,18.5978380473459,
12.1359446715607));
#134450=CARTESIAN_POINT('Ctrl Pts',(-21.2397071410263,18.6798703351908,
12.1401098956166));
#134451=CARTESIAN_POINT('Ctrl Pts',(-21.2544305326007,18.7626363860277,
12.1442751196726));
#134452=CARTESIAN_POINT('Ctrl Pts',(-21.2691564647158,18.8454167182569,
12.1484410624434));
#134453=CARTESIAN_POINT('Ctrl Pts',(-21.279801198365,18.9289306143289,12.1526070052143));
#134454=CARTESIAN_POINT('Ctrl Pts',(-21.2863115236392,19.0127428783158,
12.1567729479852));
#134455=CARTESIAN_POINT('Ctrl Pts',(-21.2914878410454,19.0793814658917,
12.1600852620663));
#134456=CARTESIAN_POINT('Ctrl Pts',(-21.2940514917317,19.1462084026767,
12.1633975761474));
#134457=CARTESIAN_POINT('Ctrl Pts',(-21.2939992159918,19.2130035272629,
12.1667098902285));
#134458=CARTESIAN_POINT('Ctrl Pts',(-21.2916489709697,19.2130199896839,
12.1667107986323));
#134459=CARTESIAN_POINT('Ctrl Pts',(-21.2937097175741,19.4962014444643,
12.1807663462274));
#134460=CARTESIAN_POINT('Ctrl Pts',(-21.1196060444512,20.6310006101477,
12.2372138293831));
#134461=CARTESIAN_POINT('Ctrl Pts',(-19.4558314911034,22.1507705593909,
12.3360532480991));
#134462=CARTESIAN_POINT('Ctrl Pts',(-16.6528318838468,21.4091880983477,
12.4632290547806));
#134463=CARTESIAN_POINT('Ctrl Pts',(-15.8397229951737,18.8995173453507,
12.5789421024831));
#134464=CARTESIAN_POINT('Ctrl Pts',(-16.6852502181462,17.565474461991,12.6522632146252));
#134465=CARTESIAN_POINT('Ctrl Pts',(-17.1750494678687,17.181608263396,12.6831923912067));
#134466=CARTESIAN_POINT('Origin',(-18.734,19.211,-1.76670989022852));
#134467=CARTESIAN_POINT('',(-17.174464231106,17.180864983421,13.5498657030158));
#134468=CARTESIAN_POINT('',(-17.174464231106,17.180864983421,13.4833228554268));
#134469=CARTESIAN_POINT('',(-17.174464231106,17.180864983421,-1.76670989022852));
#134470=CARTESIAN_POINT('',(-21.293999998394,19.2109093211998,13.0332901097364));
#134471=CARTESIAN_POINT('Ctrl Pts',(-21.293999998394,19.2109093219103,13.0332901097715));
#134472=CARTESIAN_POINT('Ctrl Pts',(-21.2940031178915,19.2989781543512,
13.0376462156856));
#134473=CARTESIAN_POINT('Ctrl Pts',(-21.2894573285641,19.3869643923453,
13.0420023215996));
#134474=CARTESIAN_POINT('Ctrl Pts',(-21.2804139262415,19.4743934627951,
13.0463584275137));
#134475=CARTESIAN_POINT('Ctrl Pts',(-21.2713470661107,19.5620493167382,
13.0507258327921));
#134476=CARTESIAN_POINT('Ctrl Pts',(-21.2577593163574,19.6491447181139,
13.0550932380704));
#134477=CARTESIAN_POINT('Ctrl Pts',(-21.2397536148681,19.7352125728896,
13.0594606433488));
#134478=CARTESIAN_POINT('Ctrl Pts',(-21.2217244341811,19.8213926590148,
13.0638337436661));
#134479=CARTESIAN_POINT('Ctrl Pts',(-21.1992659159006,19.9065421429604,
13.0682068439834));
#134480=CARTESIAN_POINT('Ctrl Pts',(-21.1725309633218,19.9902090482796,
13.0725799443008));
#134481=CARTESIAN_POINT('Ctrl Pts',(-21.1457232584227,20.0741036316349,
13.0769649448896));
#134482=CARTESIAN_POINT('Ctrl Pts',(-21.1146159900528,20.1565071961892,
13.0813499454785));
#134483=CARTESIAN_POINT('Ctrl Pts',(-21.0794107185111,20.2369866283209,
13.0857349460674));
#134484=CARTESIAN_POINT('Ctrl Pts',(-21.0474072811092,20.3101466511123,
13.0897211414781));
#134485=CARTESIAN_POINT('Ctrl Pts',(-21.0120180507083,20.3817167133685,
13.0937073368888));
#134486=CARTESIAN_POINT('Ctrl Pts',(-20.9734262024017,20.4513911818442,
13.0976935322996));
#134487=CARTESIAN_POINT('Ctrl Pts',(-20.9329131921061,20.524534153289,13.1018781666926));
#134488=CARTESIAN_POINT('Ctrl Pts',(-20.8887375841055,20.5958263313021,
13.1060628010856));
#134489=CARTESIAN_POINT('Ctrl Pts',(-20.8410930441,20.6648771968448,13.1102474354787));
#134490=CARTESIAN_POINT('Ctrl Pts',(-20.7935163202,20.7338297770271,13.1144261135626));
#134491=CARTESIAN_POINT('Ctrl Pts',(-20.742480730941,20.8005470061346,13.1186047916466));
#134492=CARTESIAN_POINT('Ctrl Pts',(-20.6882255495788,20.8646633579339,
13.1227834697305));
#134493=CARTESIAN_POINT('Ctrl Pts',(-20.6329978830832,20.9299289492597,
13.1270370476159));
#134494=CARTESIAN_POINT('Ctrl Pts',(-20.5744343004284,20.9924990829436,
13.1312906255014));
#134495=CARTESIAN_POINT('Ctrl Pts',(-20.5128330635404,21.0520195360331,
13.1355442033868));
#134496=CARTESIAN_POINT('Ctrl Pts',(-20.4524260868345,21.1103860689948,
13.1397153173648));
#134497=CARTESIAN_POINT('Ctrl Pts',(-20.3890985326093,21.1658197797779,
13.1438864313427));
#134498=CARTESIAN_POINT('Ctrl Pts',(-20.3231707254824,21.2180217749864,
13.1480575453207));
#134499=CARTESIAN_POINT('Ctrl Pts',(-20.2572650410679,21.2702062533114,
13.152227259641));
#134500=CARTESIAN_POINT('Ctrl Pts',(-20.1887611969922,21.3191608844268,
13.1563969739614));
#134501=CARTESIAN_POINT('Ctrl Pts',(-20.1180129698815,21.3646267316319,
13.1605666882818));
#134502=CARTESIAN_POINT('Ctrl Pts',(-20.0472672602965,21.410090960967,13.1647362542258));
#134503=CARTESIAN_POINT('Ctrl Pts',(-19.9742777139364,21.4520664052351,
13.1689058201699));
#134504=CARTESIAN_POINT('Ctrl Pts',(-19.8994263305452,21.4903379451218,
13.1730753861139));
#134505=CARTESIAN_POINT('Ctrl Pts',(-19.8219432648529,21.5299550651379,
13.1773915488528));
#134506=CARTESIAN_POINT('Ctrl Pts',(-19.7424654713779,21.5656027360311,
13.1817077115918));
#134507=CARTESIAN_POINT('Ctrl Pts',(-19.661441680213,21.5970955407954,13.1860238743307));
#134508=CARTESIAN_POINT('Ctrl Pts',(-19.5830572305233,21.6275624707569,
13.1901994385224));
#134509=CARTESIAN_POINT('Ctrl Pts',(-19.5032264199668,21.6541409631939,
13.194375002714));
#134510=CARTESIAN_POINT('Ctrl Pts',(-19.4223715061063,21.6767138255647,
13.1985505669057));
#134511=CARTESIAN_POINT('Ctrl Pts',(-19.3374328027607,21.700426789552,13.2029370289183));
#134512=CARTESIAN_POINT('Ctrl Pts',(-19.2513643920958,21.7197187126533,
13.2073234909308));
#134513=CARTESIAN_POINT('Ctrl Pts',(-19.1646662302712,21.734514731105,13.2117099529434));
#134514=CARTESIAN_POINT('Ctrl Pts',(-19.0779680684465,21.7493107495567,
13.2160964149559));
#134515=CARTESIAN_POINT('Ctrl Pts',(-18.9906407405948,21.7596108709354,
13.2204828769685));
#134516=CARTESIAN_POINT('Ctrl Pts',(-18.9031862415114,21.7654032601927,
13.224869338981));
#134517=CARTESIAN_POINT('Ctrl Pts',(-18.8197556535694,21.7709291330339,
13.2290539733741));
#134518=CARTESIAN_POINT('Ctrl Pts',(-18.735898795338,21.7723735414423,13.2332386077671));
#134519=CARTESIAN_POINT('Ctrl Pts',(-18.6520488590981,21.7696879470746,
13.2374232421602));
#134520=CARTESIAN_POINT('Ctrl Pts',(-18.568318272864,21.7670061753181,13.2416019202441));
#134521=CARTESIAN_POINT('Ctrl Pts',(-18.4845950449156,21.7602060920318,
13.2457805983281));
#134522=CARTESIAN_POINT('Ctrl Pts',(-18.4013160390446,21.749291035741,13.249959276412));
#134523=CARTESIAN_POINT('Ctrl Pts',(-18.3165443168449,21.7381803349106,
13.2542128542974));
#134524=CARTESIAN_POINT('Ctrl Pts',(-18.2322333798103,21.7228056564124,
13.2584664321829));
#134525=CARTESIAN_POINT('Ctrl Pts',(-18.1488425169103,21.7032260571594,
13.2627200100683));
#134526=CARTESIAN_POINT('Ctrl Pts',(-18.0670683486116,21.6840260466443,
13.2668911240463));
#134527=CARTESIAN_POINT('Ctrl Pts',(-17.9861793664179,21.660782811607,13.2710622380242));
#134528=CARTESIAN_POINT('Ctrl Pts',(-17.9066002780144,21.6336039090322,
13.2752333520022));
#134529=CARTESIAN_POINT('Ctrl Pts',(-17.8270478931424,21.6064341266006,
13.2794030663225));
#134530=CARTESIAN_POINT('Ctrl Pts',(-17.7488049640927,21.575331448026,13.2835727806429));
#134531=CARTESIAN_POINT('Ctrl Pts',(-17.6722807082307,21.5404531859398,
13.2877424949633));
#134532=CARTESIAN_POINT('Ctrl Pts',(-17.5957591754303,21.5055761649718,
13.2919120609073));
#134533=CARTESIAN_POINT('Ctrl Pts',(-17.5209566124703,21.466924019184,13.2960816268514));
#134534=CARTESIAN_POINT('Ctrl Pts',(-17.4482606698672,21.4247015099036,
13.3002511927954));
#134535=CARTESIAN_POINT('Ctrl Pts',(-17.3730088276023,21.3809945092841,
13.3045673555344));
#134536=CARTESIAN_POINT('Ctrl Pts',(-17.300014955555,21.3334616707481,13.3088835182733));
#134537=CARTESIAN_POINT('Ctrl Pts',(-17.2296778491729,21.282379942582,13.3131996810122));
#134538=CARTESIAN_POINT('Ctrl Pts',(-17.1616319666332,21.2329621963381,
13.3173752452039));
#134539=CARTESIAN_POINT('Ctrl Pts',(-17.0960727569881,21.180223552015,13.3215508093955));
#134540=CARTESIAN_POINT('Ctrl Pts',(-17.0333273206293,21.1244556272989,
13.3257263735872));
#134541=CARTESIAN_POINT('Ctrl Pts',(-16.9674127614429,21.065870997281,13.3301128355998));
#134542=CARTESIAN_POINT('Ctrl Pts',(-16.9046041088514,21.0039434366076,
13.3344992976123));
#134543=CARTESIAN_POINT('Ctrl Pts',(-16.8452349282194,20.939052806954,13.3388857596248));
#134544=CARTESIAN_POINT('Ctrl Pts',(-16.7858657475873,20.8741621773003,
13.3432722216374));
#134545=CARTESIAN_POINT('Ctrl Pts',(-16.7299363492651,20.8063089747714,
13.3476586836499));
#134546=CARTESIAN_POINT('Ctrl Pts',(-16.6777284049171,20.7359088914604,
13.3520451456625));
#134547=CARTESIAN_POINT('Ctrl Pts',(-16.6279226254793,20.6687480203406,
13.3562297800555));
#134548=CARTESIAN_POINT('Ctrl Pts',(-16.5813179797008,20.5990195040795,
13.3604144144486));
#134549=CARTESIAN_POINT('Ctrl Pts',(-16.5381897594128,20.527061315947,13.3645990488416));
#134550=CARTESIAN_POINT('Ctrl Pts',(-16.4951229268081,20.4552055513887,
13.3687777269256));
#134551=CARTESIAN_POINT('Ctrl Pts',(-16.4555229253635,20.3811268100632,
13.3729564050095));
#134552=CARTESIAN_POINT('Ctrl Pts',(-16.4196234139923,20.3051942323643,
13.3771350830935));
#134553=CARTESIAN_POINT('Ctrl Pts',(-16.3830804296802,20.2279006177819,
13.3813886609789));
#134554=CARTESIAN_POINT('Ctrl Pts',(-16.3503721900682,20.1486864403636,
13.3856422388643));
#134555=CARTESIAN_POINT('Ctrl Pts',(-16.3216976420463,20.0679698558357,
13.3898958167498));
#134556=CARTESIAN_POINT('Ctrl Pts',(-16.2935790060916,19.9888181198043,
13.3940669307277));
#134557=CARTESIAN_POINT('Ctrl Pts',(-16.2693392165557,19.9082221644555,
13.3982380447057));
#134558=CARTESIAN_POINT('Ctrl Pts',(-16.2491177212505,19.8265973202967,
13.4024091586836));
#134559=CARTESIAN_POINT('Ctrl Pts',(-16.2289030114633,19.7449998661427,
13.406578873004));
#134560=CARTESIAN_POINT('Ctrl Pts',(-16.2127040285388,19.6623746550205,
13.4107485873244));
#134561=CARTESIAN_POINT('Ctrl Pts',(-16.200609999048,19.579150924318,13.4149183016447));
#134562=CARTESIAN_POINT('Ctrl Pts',(-16.1885163999146,19.495930155073,13.4190878675888));
#134563=CARTESIAN_POINT('Ctrl Pts',(-16.1805275291,19.412111363967,13.4232574335328));
#134564=CARTESIAN_POINT('Ctrl Pts',(-16.1766810426044,19.3281313371599,
13.4274269994769));
#134565=CARTESIAN_POINT('Ctrl Pts',(-16.1726993183887,19.2411986762107,
13.4317431622158));
#134566=CARTESIAN_POINT('Ctrl Pts',(-16.1731567148618,19.1540937573817,
13.4360593249547));
#134567=CARTESIAN_POINT('Ctrl Pts',(-16.1780362227548,19.0673018113881,
13.4403754876936));
#134568=CARTESIAN_POINT('Ctrl Pts',(-16.1827567811914,18.9833371039063,
13.4445510518853));
#134569=CARTESIAN_POINT('Ctrl Pts',(-16.1916156782437,18.89966575566,13.448726616077));
#134570=CARTESIAN_POINT('Ctrl Pts',(-16.2045447628248,18.8167206534362,
13.4529021802687));
#134571=CARTESIAN_POINT('Ctrl Pts',(-16.218126864732,18.7295861912824,13.4572886422812));
#134572=CARTESIAN_POINT('Ctrl Pts',(-16.2362010106219,18.6432538400943,
13.4616751042937));
#134573=CARTESIAN_POINT('Ctrl Pts',(-16.2586283495453,18.5582096874759,
13.4660615663063));
#134574=CARTESIAN_POINT('Ctrl Pts',(-16.2810556884687,18.4731655348575,
13.4704480283188));
#134575=CARTESIAN_POINT('Ctrl Pts',(-16.3078359712665,18.3894101102965,
13.4748344903314));
#134576=CARTESIAN_POINT('Ctrl Pts',(-16.3387721302027,18.3074052613332,
13.4792209523439));
#134577=CARTESIAN_POINT('Ctrl Pts',(-16.3682827836177,18.2291791091759,
13.483405290821));
#134578=CARTESIAN_POINT('Ctrl Pts',(-16.4016845822185,18.1522546019467,
13.4875896292981));
#134579=CARTESIAN_POINT('Ctrl Pts',(-16.438842384669,18.0770460676078,13.4917739677752));
#134580=CARTESIAN_POINT('Ctrl Pts',(-16.4759497063905,18.0019397078159,
13.4959526216196));
#134581=CARTESIAN_POINT('Ctrl Pts',(-16.5168026975426,17.9285451005998,
13.5001312754641));
#134582=CARTESIAN_POINT('Ctrl Pts',(-16.5612174513678,17.857258519377,13.5043099293085));
#134583=CARTESIAN_POINT('Ctrl Pts',(-16.6055802939284,17.7860552567873,
13.5084836992082));
#134584=CARTESIAN_POINT('Ctrl Pts',(-16.653496382304,17.716955511052,13.5126574691079));
#134585=CARTESIAN_POINT('Ctrl Pts',(-16.7047357061378,17.6503314170985,
13.5168312390075));
#134586=CARTESIAN_POINT('Ctrl Pts',(-16.7559398356138,17.5837530847207,
13.5210021421022));
#134587=CARTESIAN_POINT('Ctrl Pts',(-16.8104623870111,17.5196473901113,
13.5251730451968));
#134588=CARTESIAN_POINT('Ctrl Pts',(-16.8680304516818,17.4583569545543,
13.5293439482914));
#134589=CARTESIAN_POINT('Ctrl Pts',(-16.9255842027832,17.397081758087,13.5335138143439));
#134590=CARTESIAN_POINT('Ctrl Pts',(-16.9861816530137,17.3386207695855,
13.5376836803963));
#134591=CARTESIAN_POINT('Ctrl Pts',(-17.0495108543087,17.2832820958324,
13.5418535464488));
#134592=CARTESIAN_POINT('Ctrl Pts',(-17.0900719874207,17.2478387416381,
13.5445242653045));
#134593=CARTESIAN_POINT('Ctrl Pts',(-17.1317529452028,17.2136754997451,
13.5471949841601));
#134594=CARTESIAN_POINT('Ctrl Pts',(-17.174464231106,17.180864983421,13.5498657030158));
#134595=CARTESIAN_POINT('Ctrl Pts',(-17.174464231106,17.180864983421,12.7499597594996));
#134596=CARTESIAN_POINT('Ctrl Pts',(-17.2410533408435,17.129711686913,12.7541315958235));
#134597=CARTESIAN_POINT('Ctrl Pts',(-17.3102192313192,17.0817939819445,
12.7583034321475));
#134598=CARTESIAN_POINT('Ctrl Pts',(-17.3816117456086,17.0373749151741,
12.7624752684715));
#134599=CARTESIAN_POINT('Ctrl Pts',(-17.4529733625773,16.9929750721301,
12.7666452993041));
#134600=CARTESIAN_POINT('Ctrl Pts',(-17.5265592997717,16.9520711033273,
12.7708153301367));
#134601=CARTESIAN_POINT('Ctrl Pts',(-17.6019903087145,16.9148828298984,
12.7749853609694));
#134602=CARTESIAN_POINT('Ctrl Pts',(-17.6774113001236,16.8776994952179,
12.7791548380056));
#134603=CARTESIAN_POINT('Ctrl Pts',(-17.7546764636973,16.844231078498,12.7833243150418));
#134604=CARTESIAN_POINT('Ctrl Pts',(-17.8333830590112,16.8146508756853,
12.787493792078));
#134605=CARTESIAN_POINT('Ctrl Pts',(-17.9121028115406,16.7850657280125,
12.7916639661169));
#134606=CARTESIAN_POINT('Ctrl Pts',(-17.9922640432294,16.7593702454841,
12.7958341401557));
#134607=CARTESIAN_POINT('Ctrl Pts',(-18.0734464975692,16.737688642644,12.8000043141946));
#134608=CARTESIAN_POINT('Ctrl Pts',(-18.1547182495494,16.7159831908578,
12.8041790752678));
#134609=CARTESIAN_POINT('Ctrl Pts',(-18.237013020941,16.6983005493885,12.808353836341));
#134610=CARTESIAN_POINT('Ctrl Pts',(-18.3198984700697,16.6847142040321,
12.8125285974141));
#134611=CARTESIAN_POINT('Ctrl Pts',(-18.4028355291097,16.6711193989268,
12.8167059579671));
#134612=CARTESIAN_POINT('Ctrl Pts',(-18.4863635411595,16.6616260185993,
12.82088331852));
#134613=CARTESIAN_POINT('Ctrl Pts',(-18.5700455072367,16.6562556048985,
12.825060679073));
#134614=CARTESIAN_POINT('Ctrl Pts',(-18.6538653038287,16.6508763457209,
12.8292449200541));
#134615=CARTESIAN_POINT('Ctrl Pts',(-18.7378391012384,16.6496336144523,
12.8334291610351));
#134616=CARTESIAN_POINT('Ctrl Pts',(-18.821530806815,16.6524968520914,12.8376134020162));
#134617=CARTESIAN_POINT('Ctrl Pts',(-18.859724062068,16.6538035092475,12.8395229076564));
#134618=CARTESIAN_POINT('Ctrl Pts',(-18.8978586532058,16.6559645670067,
12.8414324132965));
#134619=CARTESIAN_POINT('Ctrl Pts',(-18.9358937423124,16.6589735665916,
12.8433419189367));
#134620=CARTESIAN_POINT('Ctrl Pts',(-19.0192466995764,16.665567714777,12.8475265533297));
#134621=CARTESIAN_POINT('Ctrl Pts',(-19.1024313715334,16.6762620749485,
12.8517111877227));
#134622=CARTESIAN_POINT('Ctrl Pts',(-19.1850120996543,16.6910420467862,
12.8558958221158));
#134623=CARTESIAN_POINT('Ctrl Pts',(-19.2674752843302,16.7058009811635,
12.8600745001997));
#134624=CARTESIAN_POINT('Ctrl Pts',(-19.3493357837201,16.7246338957132,
12.8642531782837));
#134625=CARTESIAN_POINT('Ctrl Pts',(-19.4301618064486,16.7474743274644,
12.8684318563676));
#134626=CARTESIAN_POINT('Ctrl Pts',(-19.512436577546,16.7707241575396,12.872685434253));
#134627=CARTESIAN_POINT('Ctrl Pts',(-19.5936389405802,16.7981265494104,
12.8769390121385));
#134628=CARTESIAN_POINT('Ctrl Pts',(-19.6733229700782,16.8295566649858,
12.8811925900239));
#134629=CARTESIAN_POINT('Ctrl Pts',(-19.7514621691736,16.8603774464399,
12.8853637040019));
#134630=CARTESIAN_POINT('Ctrl Pts',(-19.8281409334341,16.8950709981003,
12.8895348179798));
#134631=CARTESIAN_POINT('Ctrl Pts',(-19.9029545672463,16.9334694909367,
12.8937059319578));
#134632=CARTESIAN_POINT('Ctrl Pts',(-19.9777430966213,16.9718550987881,
12.8978756462781));
#134633=CARTESIAN_POINT('Ctrl Pts',(-20.0506673295885,17.0139429688568,
12.9020453605985));
#134634=CARTESIAN_POINT('Ctrl Pts',(-20.1213450915266,17.0595182787165,
12.9062150749189));
#134635=CARTESIAN_POINT('Ctrl Pts',(-20.1920203384467,17.1050919668111,
12.910384640863));
#134636=CARTESIAN_POINT('Ctrl Pts',(-20.2604488871169,17.1541525979352,
12.914554206807));
#134637=CARTESIAN_POINT('Ctrl Pts',(-20.3262767630691,17.2064415174932,
12.9187237727511));
#134638=CARTESIAN_POINT('Ctrl Pts',(-20.3944190659323,17.2605688509573,
12.92303993549));
#134639=CARTESIAN_POINT('Ctrl Pts',(-20.45977400114,17.3181553818456,12.9273560982289));
#134640=CARTESIAN_POINT('Ctrl Pts',(-20.5219870028024,17.3788694157322,
12.9316722609678));
#134641=CARTESIAN_POINT('Ctrl Pts',(-20.5821734224794,17.4376056963509,
12.9358478251595));
#134642=CARTESIAN_POINT('Ctrl Pts',(-20.6394191762104,17.4992684748651,
12.9400233893512));
#134643=CARTESIAN_POINT('Ctrl Pts',(-20.6934427607506,17.5635219068703,
12.9441989535429));
#134644=CARTESIAN_POINT('Ctrl Pts',(-20.750194948117,17.6310206269781,12.9485854155554));
#134645=CARTESIAN_POINT('Ctrl Pts',(-20.8033905562332,17.7013781204558,
12.9529718775679));
#134646=CARTESIAN_POINT('Ctrl Pts',(-20.8527544426652,17.7741702913405,
12.9573583395805));
#134647=CARTESIAN_POINT('Ctrl Pts',(-20.9021183290971,17.8469624622252,
12.961744801593));
#134648=CARTESIAN_POINT('Ctrl Pts',(-20.9476502584794,17.922188774755,12.9661312636056));
#134649=CARTESIAN_POINT('Ctrl Pts',(-20.9891316170534,17.9993971815128,
12.9705177256181));
#134650=CARTESIAN_POINT('Ctrl Pts',(-21.030861876244,18.0770688619123,12.9749305077209));
#134651=CARTESIAN_POINT('Ctrl Pts',(-21.0686351706118,18.1570094498411,
12.9793432898236));
#134652=CARTESIAN_POINT('Ctrl Pts',(-21.1022126120114,18.2388019624017,
12.9837560719264));
#134653=CARTESIAN_POINT('Ctrl Pts',(-21.1356929152443,18.3203578525637,
12.9881560880307));
#134654=CARTESIAN_POINT('Ctrl Pts',(-21.1650014030465,18.4037546379829,
12.992556104135));
#134655=CARTESIAN_POINT('Ctrl Pts',(-21.1899457627446,18.4885524860192,
12.9969561202393));
#134656=CARTESIAN_POINT('Ctrl Pts',(-21.2148467487812,18.5732028861678,
13.0013484855235));
#134657=CARTESIAN_POINT('Ctrl Pts',(-21.2353985968836,18.6592491335648,
13.0057408508078));
#134658=CARTESIAN_POINT('Ctrl Pts',(-21.2514572537725,18.7462323425323,
13.010133216092));
#134659=CARTESIAN_POINT('Ctrl Pts',(-21.267478998332,18.8330156124333,13.0145154851125));
#134660=CARTESIAN_POINT('Ctrl Pts',(-21.2790280568695,18.9207311752703,
13.018897754133));
#134661=CARTESIAN_POINT('Ctrl Pts',(-21.28601069243,19.0089073833049,13.0232800231535));
#134662=CARTESIAN_POINT('Ctrl Pts',(-21.291327328341,19.0760454703582,13.0266167186811));
#134663=CARTESIAN_POINT('Ctrl Pts',(-21.2939976088987,19.1434502453364,
13.0299534142087));
#134664=CARTESIAN_POINT('Ctrl Pts',(-21.293999998394,19.2109093211998,13.0332901097364));
#134665=CARTESIAN_POINT('',(-21.2943302428071,19.2116425108278,12.9667098340901));
#134666=CARTESIAN_POINT('Ctrl Pts',(-17.1750494678687,17.181608263396,12.6831923912067));
#134667=CARTESIAN_POINT('Ctrl Pts',(-17.3565755014764,17.039342409566,12.6946551501856));
#134668=CARTESIAN_POINT('Ctrl Pts',(-18.295337787686,16.4863766829119,12.748509844725));
#134669=CARTESIAN_POINT('Ctrl Pts',(-20.4360629288883,16.7305239810473,
12.8430154491748));
#134670=CARTESIAN_POINT('Ctrl Pts',(-21.2952860172943,18.397872866616,12.9260582946456));
#134671=CARTESIAN_POINT('Ctrl Pts',(-21.2980344808449,19.2116308398979,
12.9667092045559));
#134672=CARTESIAN_POINT('Ctrl Pts',(-21.2939999191096,19.2116435515775,
12.9667098902285));
#134673=CARTESIAN_POINT('Ctrl Pts',(-21.2939911726516,19.2464363059257,
12.9684506873211));
#134674=CARTESIAN_POINT('Ctrl Pts',(-21.2932731600888,19.281219269613,12.9701914844137));
#134675=CARTESIAN_POINT('Ctrl Pts',(-21.2918468828523,19.3159729673895,
12.9719322815063));
#134676=CARTESIAN_POINT('Ctrl Pts',(-21.2884183105029,19.3995160291397,
12.9761169158993));
#134677=CARTESIAN_POINT('Ctrl Pts',(-21.2808860937369,19.4830464110296,
12.9803015502924));
#134678=CARTESIAN_POINT('Ctrl Pts',(-21.2692483017375,19.5661282142231,
12.9844861846854));
#134679=CARTESIAN_POINT('Ctrl Pts',(-21.2576270746945,19.6490917607532,
12.9886648627693));
#134680=CARTESIAN_POINT('Ctrl Pts',(-21.2419119432712,19.7316075451531,
12.9928435408533));
#134681=CARTESIAN_POINT('Ctrl Pts',(-21.2221529486456,19.8132415662722,
12.9970222189372));
#134682=CARTESIAN_POINT('Ctrl Pts',(-21.2020397882419,19.8963388185507,
13.0012757968227));
#134683=CARTESIAN_POINT('Ctrl Pts',(-21.1777363859676,19.9785219036746,
13.0055293747081));
#134684=CARTESIAN_POINT('Ctrl Pts',(-21.1493505801535,20.0593404829147,
13.0097829525936));
#134685=CARTESIAN_POINT('Ctrl Pts',(-21.1215150885756,20.1385922362917,
13.0139540665715));
#134686=CARTESIAN_POINT('Ctrl Pts',(-21.0897542310845,20.2165314648403,
13.0181251805494));
#134687=CARTESIAN_POINT('Ctrl Pts',(-21.0542203695085,20.292747399774,13.0222962945274));
#134688=CARTESIAN_POINT('Ctrl Pts',(-21.018698431663,20.3689377597145,13.0264660088478));
#134689=CARTESIAN_POINT('Ctrl Pts',(-20.9794061983923,20.4434055578918,
13.0306357231681));
#134690=CARTESIAN_POINT('Ctrl Pts',(-20.9365438451405,20.5157607482728,
13.0348054374885));
#134691=CARTESIAN_POINT('Ctrl Pts',(-20.8936830171152,20.5881133639457,
13.0389750034325));
#134692=CARTESIAN_POINT('Ctrl Pts',(-20.8472525568965,20.6583531259272,
13.0431445693766));
#134693=CARTESIAN_POINT('Ctrl Pts',(-20.7974975099507,20.7261165058923,
13.0473141353206));
#134694=CARTESIAN_POINT('Ctrl Pts',(-20.7459931369336,20.796262362702,13.0516302980595));
#134695=CARTESIAN_POINT('Ctrl Pts',(-20.6909263546122,20.8637540331552,
13.0559464607985));
#134696=CARTESIAN_POINT('Ctrl Pts',(-20.6326151733211,20.928224628182,13.0602626235374));
#134697=CARTESIAN_POINT('Ctrl Pts',(-20.5762034726275,20.9905951003567,
13.0644381877291));
#134698=CARTESIAN_POINT('Ctrl Pts',(-20.5167558657732,21.0501379976125,
13.0686137519207));
#134699=CARTESIAN_POINT('Ctrl Pts',(-20.4545972806998,21.1065592836016,
13.0727893161124));
#134700=CARTESIAN_POINT('Ctrl Pts',(-20.389299213262,21.1658302746175,13.077175778125));
#134701=CARTESIAN_POINT('Ctrl Pts',(-20.321009559389,21.2216556522273,13.0815622401375));
#134702=CARTESIAN_POINT('Ctrl Pts',(-20.2501416763133,21.2737443897259,
13.0859487021501));
#134703=CARTESIAN_POINT('Ctrl Pts',(-20.1792737932376,21.3258331272245,
13.0903351641626));
#134704=CARTESIAN_POINT('Ctrl Pts',(-20.1058282074104,21.3741849690991,
13.0947216261752));
#134705=CARTESIAN_POINT('Ctrl Pts',(-20.0302483510418,21.4185643167123,
13.0991080881878));
#134706=CARTESIAN_POINT('Ctrl Pts',(-19.9581460359011,21.4609017047557,
13.1032927225808));
#134707=CARTESIAN_POINT('Ctrl Pts',(-19.8838331576255,21.4997817138927,
13.1074773569739));
#134708=CARTESIAN_POINT('Ctrl Pts',(-19.8076751930389,21.5349667768393,
13.1116619913669));
#134709=CARTESIAN_POINT('Ctrl Pts',(-19.7316256298885,21.5701017582038,
13.1158406694508));
#134710=CARTESIAN_POINT('Ctrl Pts',(-19.6537366110357,21.6015520487103,
13.1200193475348));
#134711=CARTESIAN_POINT('Ctrl Pts',(-19.5744001491066,21.629124808479,13.1241980256187));
#134712=CARTESIAN_POINT('Ctrl Pts',(-19.4936416381155,21.6571917901503,
13.1284516035042));
#134713=CARTESIAN_POINT('Ctrl Pts',(-19.4113836985809,21.6812406201864,
13.1327051813896));
#134714=CARTESIAN_POINT('Ctrl Pts',(-19.3280633649498,21.701118213745,13.136958759275));
#134715=CARTESIAN_POINT('Ctrl Pts',(-19.2463583585722,21.7206104413645,
13.141129873253));
#134716=CARTESIAN_POINT('Ctrl Pts',(-19.1636322517455,21.7360916126581,
13.1453009872309));
#134717=CARTESIAN_POINT('Ctrl Pts',(-19.0803129065814,21.7474674984583,
13.1494721012089));
#134718=CARTESIAN_POINT('Ctrl Pts',(-18.9970215200283,21.7588395669701,
13.1536418155293));
#134719=CARTESIAN_POINT('Ctrl Pts',(-18.9131377459124,21.76610902368,13.1578115298496));
#134720=CARTESIAN_POINT('Ctrl Pts',(-18.8290979023926,21.7692330599381,
13.16198124417));
#134721=CARTESIAN_POINT('Ctrl Pts',(-18.7450610493711,21.7723569850297,
13.166150810114));
#134722=CARTESIAN_POINT('Ctrl Pts',(-18.6608685977348,21.7713357667235,
13.1703203760581));
#134723=CARTESIAN_POINT('Ctrl Pts',(-18.5769588557388,21.7661786784898,
13.1744899420021));
#134724=CARTESIAN_POINT('Ctrl Pts',(-18.4900989507281,21.7608402733958,
13.1788061047411));
#134725=CARTESIAN_POINT('Ctrl Pts',(-18.4035425318193,21.7510697851063,
13.18312226748));
#134726=CARTESIAN_POINT('Ctrl Pts',(-18.3177702276211,21.7369360198915,
13.1874384302189));
#134727=CARTESIAN_POINT('Ctrl Pts',(-18.2347919472104,21.7232626605919,
13.1916139944106));
#134728=CARTESIAN_POINT('Ctrl Pts',(-18.1525479314088,21.7055060719794,
13.1957895586022));
#134729=CARTESIAN_POINT('Ctrl Pts',(-18.0714612955845,21.6837803107335,
13.1999651227939));
#134730=CARTESIAN_POINT('Ctrl Pts',(-17.98627916655,21.6609572329353,13.2043515848065));
#134731=CARTESIAN_POINT('Ctrl Pts',(-17.9023749641124,21.6337536591884,
13.208738046819));
#134732=CARTESIAN_POINT('Ctrl Pts',(-17.8202171381048,21.6023596302745,
13.2131245088315));
#134733=CARTESIAN_POINT('Ctrl Pts',(-17.7380593120971,21.5709656013606,
13.2175109708441));
#134734=CARTESIAN_POINT('Ctrl Pts',(-17.6576483623233,21.5353814216376,
13.2218974328566));
#134735=CARTESIAN_POINT('Ctrl Pts',(-17.579422411398,21.4958524223455,13.2262838948691));
#134736=CARTESIAN_POINT('Ctrl Pts',(-17.5047957524334,21.4581422109068,
13.2304685292622));
#134737=CARTESIAN_POINT('Ctrl Pts',(-17.4318796660886,21.4167018520732,
13.2346531636552));
#134738=CARTESIAN_POINT('Ctrl Pts',(-17.3610717345268,21.3717100633506,
13.2388377980483));
#134739=CARTESIAN_POINT('Ctrl Pts',(-17.2903645892912,21.3267823148704,
13.2430164761322));
#134740=CARTESIAN_POINT('Ctrl Pts',(-17.2217600234686,21.2783134219689,
13.2471951542162));
#134741=CARTESIAN_POINT('Ctrl Pts',(-17.1556323738797,21.2265286246579,
13.2513738323001));
#134742=CARTESIAN_POINT('Ctrl Pts',(-17.0883194336969,21.173815622072,13.2556274101856));
#134743=CARTESIAN_POINT('Ctrl Pts',(-17.0235735109216,21.117666888101,13.259880988071));
#134744=CARTESIAN_POINT('Ctrl Pts',(-16.9617598841366,21.0583670376307,
13.2641345659564));
#134745=CARTESIAN_POINT('Ctrl Pts',(-16.9011446351263,21.000216830476,13.2683056799344));
#134746=CARTESIAN_POINT('Ctrl Pts',(-16.8433493474163,20.9390369307226,
13.2724767939123));
#134747=CARTESIAN_POINT('Ctrl Pts',(-16.7886848464703,20.8751360982347,
13.2766479078903));
#134748=CARTESIAN_POINT('Ctrl Pts',(-16.7340386887256,20.8112567082883,
13.2808176222107));
#134749=CARTESIAN_POINT('Ctrl Pts',(-16.6825215301017,20.7446585481929,
13.284987336531));
#134750=CARTESIAN_POINT('Ctrl Pts',(-16.6344055366424,20.6756853209608,
13.2891570508514));
#134751=CARTESIAN_POINT('Ctrl Pts',(-16.5862912553567,20.6067145480922,
13.2933266167954));
#134752=CARTESIAN_POINT('Ctrl Pts',(-16.5415781611063,20.5353692539102,
13.2974961827395));
#134753=CARTESIAN_POINT('Ctrl Pts',(-16.5004957043155,20.4620230058472,
13.3016657486835));
#134754=CARTESIAN_POINT('Ctrl Pts',(-16.4579688390247,20.3860979941846,
13.3059819114225));
#134755=CARTESIAN_POINT('Ctrl Pts',(-16.4193329255797,20.3080291637333,
13.3102980741614));
#134756=CARTESIAN_POINT('Ctrl Pts',(-16.3847902639464,20.2282578906211,
13.3146142369003));
#134757=CARTESIAN_POINT('Ctrl Pts',(-16.3513728258826,20.1510851583402,
13.318789801092));
#134758=CARTESIAN_POINT('Ctrl Pts',(-16.3217861809924,20.0723196518131,
13.3229653652837));
#134759=CARTESIAN_POINT('Ctrl Pts',(-16.2961634499818,19.9923788808225,
13.3271409294753));
#134760=CARTESIAN_POINT('Ctrl Pts',(-16.2692465757402,19.9084004915302,
13.3315273914879));
#134761=CARTESIAN_POINT('Ctrl Pts',(-16.246704722792,19.8231255568952,13.3359138535004));
#134762=CARTESIAN_POINT('Ctrl Pts',(-16.2286316599242,19.7370508345642,
13.340300315513));
#134763=CARTESIAN_POINT('Ctrl Pts',(-16.2105585970564,19.6509761122332,
13.3446867775255));
#134764=CARTESIAN_POINT('Ctrl Pts',(-16.1969543388866,19.5641021872051,
13.3490732395381));
#134765=CARTESIAN_POINT('Ctrl Pts',(-16.1878497481282,19.4769302444118,
13.3534597015506));
#134766=CARTESIAN_POINT('Ctrl Pts',(-16.1791640730867,19.3937692119263,
13.3576443359437));
#134767=CARTESIAN_POINT('Ctrl Pts',(-16.1745407622114,19.3100274422731,
13.3618289703367));
#134768=CARTESIAN_POINT('Ctrl Pts',(-16.1740447460464,19.2261359755289,
13.3660136047298));
#134769=CARTESIAN_POINT('Ctrl Pts',(-16.173549435899,19.1423639179039,13.3701922828137));
#134770=CARTESIAN_POINT('Ctrl Pts',(-16.1771697541693,19.0584430425126,
13.3743709608977));
#134771=CARTESIAN_POINT('Ctrl Pts',(-16.1849189310737,18.9748100255276,
13.3785496389816));
#134772=CARTESIAN_POINT('Ctrl Pts',(-16.1928070064048,18.8896779468192,
13.382803216867));
#134773=CARTESIAN_POINT('Ctrl Pts',(-16.2049734659499,18.804844627276,13.3870567947525));
#134774=CARTESIAN_POINT('Ctrl Pts',(-16.2213767120001,18.7207712650195,
13.3913103726379));
#134775=CARTESIAN_POINT('Ctrl Pts',(-16.2374619491174,18.6383278289459,
13.3954814866159));
#134776=CARTESIAN_POINT('Ctrl Pts',(-16.2576210698179,18.5566156189164,
13.3996526005938));
#134777=CARTESIAN_POINT('Ctrl Pts',(-16.2817626998464,18.4760631158151,
13.4038237145718));
#134778=CARTESIAN_POINT('Ctrl Pts',(-16.3058962289179,18.3955376428842,
13.4079934288921));
#134779=CARTESIAN_POINT('Ctrl Pts',(-16.3340094813079,18.3161715443229,
13.4121631432125));
#134780=CARTESIAN_POINT('Ctrl Pts',(-16.3659607754927,18.2383797086247,
13.4163328575329));
#134781=CARTESIAN_POINT('Ctrl Pts',(-16.3979109327134,18.1605906410939,
13.4205024234769));
#134782=CARTESIAN_POINT('Ctrl Pts',(-16.4336986846161,18.0843761502596,
13.424671989421));
#134783=CARTESIAN_POINT('Ctrl Pts',(-16.4731341172713,18.0101313725834,
13.428841555365));
#134784=CARTESIAN_POINT('Ctrl Pts',(-16.5139560510898,17.933276240115,13.433157718104));
#134785=CARTESIAN_POINT('Ctrl Pts',(-16.5586866956794,17.8585323739429,
13.4374738808429));
#134786=CARTESIAN_POINT('Ctrl Pts',(-16.6070644247003,17.7863087848504,
13.4417900435818));
#134787=CARTESIAN_POINT('Ctrl Pts',(-16.6538662542868,17.7164378715759,
13.4459656077735));
#134788=CARTESIAN_POINT('Ctrl Pts',(-16.7040808906405,17.6489259106341,
13.4501411719652));
#134789=CARTESIAN_POINT('Ctrl Pts',(-16.7574293298199,17.5841108255988,
13.4543167361568));
#134790=CARTESIAN_POINT('Ctrl Pts',(-16.8134722718384,17.5160220847016,
13.4587031981694));
#134791=CARTESIAN_POINT('Ctrl Pts',(-16.8729735193545,17.450910248947,13.4630896601819));
#134792=CARTESIAN_POINT('Ctrl Pts',(-16.9355661330671,17.3891230485379,
13.4674761221945));
#134793=CARTESIAN_POINT('Ctrl Pts',(-16.9981587467797,17.3273358481289,
13.471862584207));
#134794=CARTESIAN_POINT('Ctrl Pts',(-17.0638422427094,17.2688736120054,
13.4762490462195));
#134795=CARTESIAN_POINT('Ctrl Pts',(-17.1322119090441,17.2140335727229,
13.4806355082321));
#134796=CARTESIAN_POINT('Ctrl Pts',(-17.1461740369508,17.2028344008691,
13.4815312906303));
#134797=CARTESIAN_POINT('Ctrl Pts',(-17.1602591664528,17.1917772164721,
13.4824270730286));
#134798=CARTESIAN_POINT('Ctrl Pts',(-17.174464231106,17.180864983421,13.4833228554268));
#134799=CARTESIAN_POINT('Origin',(-18.734,19.211,-1.76670989022852));
#134800=CARTESIAN_POINT('',(-17.1732300624786,17.1792869614928,14.3497865218036));
#134801=CARTESIAN_POINT('',(-17.1756294966408,17.182412846113,14.2834124313123));
#134802=CARTESIAN_POINT('',(-17.174464231106,17.180864983421,-1.76670989022852));
#134803=CARTESIAN_POINT('',(-21.2939989424941,19.2133268925441,13.8332901097715));
#134804=CARTESIAN_POINT('Ctrl Pts',(-21.2944497455462,19.2133273022983,
13.8332901097715));
#134805=CARTESIAN_POINT('Ctrl Pts',(-21.2961552640167,19.3972186594194,
13.8424428639771));
#134806=CARTESIAN_POINT('Ctrl Pts',(-21.1940977855363,20.4309438993384,
13.8939875537431));
#134807=CARTESIAN_POINT('Ctrl Pts',(-19.7898863418736,22.047969473252,13.9879241790696));
#134808=CARTESIAN_POINT('Ctrl Pts',(-16.9200888835355,21.634431084369,14.1150999857511));
#134809=CARTESIAN_POINT('Ctrl Pts',(-15.7765849628929,19.1334581710982,
14.2357207666624));
#134810=CARTESIAN_POINT('Ctrl Pts',(-16.6072658097655,17.6225945609841,
14.3139496120132));
#134811=CARTESIAN_POINT('Ctrl Pts',(-17.1732300624786,17.1792869614928,
14.3497865218036));
#134812=CARTESIAN_POINT('Ctrl Pts',(-17.174464231106,17.180864983421,13.5498657030158));
#134813=CARTESIAN_POINT('Ctrl Pts',(-17.2411543251493,17.1296341114632,
13.5540358067222));
#134814=CARTESIAN_POINT('Ctrl Pts',(-17.3103576653337,17.0817034418445,
13.5582059104285));
#134815=CARTESIAN_POINT('Ctrl Pts',(-17.3817086482351,17.0373146271961,
13.5623760141349));
#134816=CARTESIAN_POINT('Ctrl Pts',(-17.4531374462619,16.9928774022659,
13.5665506657413));
#134817=CARTESIAN_POINT('Ctrl Pts',(-17.5267181707769,16.9519899856981,
13.5707253173478));
#134818=CARTESIAN_POINT('Ctrl Pts',(-17.6020588076407,16.914849060484,13.5748999689542));
#134819=CARTESIAN_POINT('Ctrl Pts',(-17.677445250084,16.8776855543405,13.5790771586642));
#134820=CARTESIAN_POINT('Ctrl Pts',(-17.7545933127803,16.8442732563227,
13.5832543483742));
#134821=CARTESIAN_POINT('Ctrl Pts',(-17.8330913235602,16.8147605385281,
13.5874315380842));
#134822=CARTESIAN_POINT('Ctrl Pts',(-17.9117198950076,16.7851987341374,
13.5916156754438));
#134823=CARTESIAN_POINT('Ctrl Pts',(-17.9917024590505,16.7595495978572,
13.5957998128035));
#134824=CARTESIAN_POINT('Ctrl Pts',(-18.0726129198988,16.7379114188377,
13.5999839501631));
#134825=CARTESIAN_POINT('Ctrl Pts',(-18.1139486661373,16.7268568497791,
13.6021215531172));
#134826=CARTESIAN_POINT('Ctrl Pts',(-18.1555264377626,16.7168483177079,
13.6042591560712));
#134827=CARTESIAN_POINT('Ctrl Pts',(-18.1972887614196,16.7078937205182,
13.6063967590253));
#134828=CARTESIAN_POINT('Ctrl Pts',(-18.2790439141133,16.6903639377749,
13.6105813934184));
#134829=CARTESIAN_POINT('Ctrl Pts',(-18.3618109357873,16.6768111110841,
13.6147660278114));
#134830=CARTESIAN_POINT('Ctrl Pts',(-18.4451682027609,16.6673458975514,
13.6189506622045));
#134831=CARTESIAN_POINT('Ctrl Pts',(-18.5284068209824,16.6578941565787,
13.6231293402884));
#134832=CARTESIAN_POINT('Ctrl Pts',(-18.6122335625328,16.6525185234246,
13.6273080183723));
#134833=CARTESIAN_POINT('Ctrl Pts',(-18.6962156707035,16.6512788541602,
13.6314866964563));
#134834=CARTESIAN_POINT('Ctrl Pts',(-18.7817030978064,16.6500169647151,
13.6357402743417));
#134835=CARTESIAN_POINT('Ctrl Pts',(-18.867351044784,16.6530408729659,13.6399938522271));
#134836=CARTESIAN_POINT('Ctrl Pts',(-18.9526965098734,16.6603585440974,
13.6442474301126));
#134837=CARTESIAN_POINT('Ctrl Pts',(-19.036387386584,16.6675343478947,13.6484185440905));
#134838=CARTESIAN_POINT('Ctrl Pts',(-19.1197869256877,16.6788388732103,
13.6525896580685));
#134839=CARTESIAN_POINT('Ctrl Pts',(-19.2024593314997,16.6942270951214,
13.6567607720464));
#134840=CARTESIAN_POINT('Ctrl Pts',(-19.2851039957874,16.7096101533661,
13.6609304863668));
#134841=CARTESIAN_POINT('Ctrl Pts',(-19.3670215594759,16.729074102609,13.6651002006872));
#134842=CARTESIAN_POINT('Ctrl Pts',(-19.4477843610407,16.7525224455095,
13.6692699150076));
#134843=CARTESIAN_POINT('Ctrl Pts',(-19.5285442887184,16.7759699540173,
13.6734394809516));
#134844=CARTESIAN_POINT('Ctrl Pts',(-19.6081490944211,16.8034014451982,
13.6776090468957));
#134845=CARTESIAN_POINT('Ctrl Pts',(-19.6861855970009,16.8346703534938,
13.6817786128397));
#134846=CARTESIAN_POINT('Ctrl Pts',(-19.766965766743,16.8670386380308,13.6860947755786));
#134847=CARTESIAN_POINT('Ctrl Pts',(-19.8460648087822,16.9035190114424,
13.6904109383175));
#134848=CARTESIAN_POINT('Ctrl Pts',(-19.9230480777099,16.9438950908936,
13.6947271010565));
#134849=CARTESIAN_POINT('Ctrl Pts',(-19.9975236247495,16.9829559238035,
13.6989026652482));
#134850=CARTESIAN_POINT('Ctrl Pts',(-20.0700187425844,17.0256622753738,
13.7030782294398));
#134851=CARTESIAN_POINT('Ctrl Pts',(-20.140167606798,17.0717728821857,13.7072537936315));
#134852=CARTESIAN_POINT('Ctrl Pts',(-20.21385952338,17.1202124261301,13.7116402556441));
#134853=CARTESIAN_POINT('Ctrl Pts',(-20.2849614681662,17.1724088154587,
13.7160267176566));
#134854=CARTESIAN_POINT('Ctrl Pts',(-20.3530884618266,17.2280344045395,
13.7204131796692));
#134855=CARTESIAN_POINT('Ctrl Pts',(-20.421215455487,17.2836599936203,13.7247996416817));
#134856=CARTESIAN_POINT('Ctrl Pts',(-20.4863671192073,17.3427143364292,
13.7291861036942));
#134857=CARTESIAN_POINT('Ctrl Pts',(-20.548204641978,17.4048268308311,13.7335725657068));
#134858=CARTESIAN_POINT('Ctrl Pts',(-20.6067777194386,17.4636603639817,
13.7377274633762));
#134859=CARTESIAN_POINT('Ctrl Pts',(-20.6626103382647,17.5254713783546,
13.7418823610455));
#134860=CARTESIAN_POINT('Ctrl Pts',(-20.7153787245625,17.5899699725634,
13.7460372587149));
#134861=CARTESIAN_POINT('Ctrl Pts',(-20.7677053791601,17.6539286398258,
13.7501573751423));
#134862=CARTESIAN_POINT('Ctrl Pts',(-20.8170185699061,17.7205297194409,
13.7542774915697));
#134863=CARTESIAN_POINT('Ctrl Pts',(-20.8630375889925,17.7894519196816,
13.7583976079971));
#134864=CARTESIAN_POINT('Ctrl Pts',(-20.9090125260321,17.8583080987051,
13.7625137777266));
#134865=CARTESIAN_POINT('Ctrl Pts',(-20.951699290088,17.9294805955782,13.7666299474561));
#134866=CARTESIAN_POINT('Ctrl Pts',(-20.9908578231797,18.0026156381546,
13.7707461171856));
#134867=CARTESIAN_POINT('Ctrl Pts',(-21.0299913601116,18.0757039962649,
13.7748596594307));
#134868=CARTESIAN_POINT('Ctrl Pts',(-21.0656009133711,18.1507519968574,
13.7789732016758));
#134869=CARTESIAN_POINT('Ctrl Pts',(-21.0974909394082,18.2273788435911,
13.7830867439209));
#134870=CARTESIAN_POINT('Ctrl Pts',(-21.1299241917558,18.3053109799219,
13.7872703577417));
#134871=CARTESIAN_POINT('Ctrl Pts',(-21.1585097661409,18.3848758167557,
13.7914539715626));
#134872=CARTESIAN_POINT('Ctrl Pts',(-21.1830923574767,18.4656499986255,
13.7956375853835));
#134873=CARTESIAN_POINT('Ctrl Pts',(-21.2072638620762,18.5450734199364,
13.7997512379815));
#134874=CARTESIAN_POINT('Ctrl Pts',(-21.2275651518659,18.6256655681997,
13.8038648905795));
#134875=CARTESIAN_POINT('Ctrl Pts',(-21.2438990336338,18.7070090864272,
13.8079785431775));
#134876=CARTESIAN_POINT('Ctrl Pts',(-21.260649602877,18.7904277283589,13.8121971376098));
#134877=CARTESIAN_POINT('Ctrl Pts',(-21.2732274574716,18.8746360871023,
13.8164157320421));
#134878=CARTESIAN_POINT('Ctrl Pts',(-21.2815840465261,18.9591756050627,
13.8206343264745));
#134879=CARTESIAN_POINT('Ctrl Pts',(-21.2899406355806,19.043715123023,13.8248529209068));
#134880=CARTESIAN_POINT('Ctrl Pts',(-21.2940759677847,19.1285852645553,
13.8290715153392));
#134881=CARTESIAN_POINT('Ctrl Pts',(-21.2939989424941,19.2133268925441,
13.8332901097715));
#134882=CARTESIAN_POINT('',(-21.2939989173812,19.2086456408557,13.7667098774912));
#134883=CARTESIAN_POINT('Ctrl Pts',(-17.174464231106,17.180864983421,13.4833228554268));
#134884=CARTESIAN_POINT('Ctrl Pts',(-17.2408009142214,17.1299055993094,
13.4875060981324));
#134885=CARTESIAN_POINT('Ctrl Pts',(-17.3097560410181,17.0821103414713,
13.4916893408381));
#134886=CARTESIAN_POINT('Ctrl Pts',(-17.3809949048231,17.0377588232262,
13.4958725835437));
#134887=CARTESIAN_POINT('Ctrl Pts',(-17.4521374194886,16.993467289523,13.5000501684971));
#134888=CARTESIAN_POINT('Ctrl Pts',(-17.5255571481475,16.9526104846787,
13.5042277534506));
#134889=CARTESIAN_POINT('Ctrl Pts',(-17.6008877396761,16.9154267370647,
13.508405338404));
#134890=CARTESIAN_POINT('Ctrl Pts',(-17.6761383840039,16.8782824519914,
13.5125784897507));
#134891=CARTESIAN_POINT('Ctrl Pts',(-17.7532954499436,16.8448036790587,
13.5167516410973));
#134892=CARTESIAN_POINT('Ctrl Pts',(-17.8319663255885,16.8151838029123,
13.520924792444));
#134893=CARTESIAN_POINT('Ctrl Pts',(-17.9105918009404,16.7855810201445,
13.5250955355005));
#134894=CARTESIAN_POINT('Ctrl Pts',(-17.9907289220234,16.7598328745479,
13.529266278557));
#134895=CARTESIAN_POINT('Ctrl Pts',(-18.0719643826269,16.7380849506444,
13.5334370216135));
#134896=CARTESIAN_POINT('Ctrl Pts',(-18.1531773319184,16.7163430533492,
13.5376066089076));
#134897=CARTESIAN_POINT('Ctrl Pts',(-18.2354875720585,16.6985992948508,
13.5417761962016));
#134898=CARTESIAN_POINT('Ctrl Pts',(-18.3184672066022,16.6849492290116,
13.5459457834956));
#134899=CARTESIAN_POINT('Ctrl Pts',(-18.4014487382646,16.6712988510983,
13.5501154661167));
#134900=CARTESIAN_POINT('Ctrl Pts',(-18.4850992405653,16.6617424250825,
13.5542851487377));
#134901=CARTESIAN_POINT('Ctrl Pts',(-18.5689825669994,16.6563240427002,
13.5584548313588));
#134902=CARTESIAN_POINT('Ctrl Pts',(-18.6529509714077,16.650900164768,13.5626287430462));
#134903=CARTESIAN_POINT('Ctrl Pts',(-18.7371522114986,16.6496227435834,
13.5668026547335));
#134904=CARTESIAN_POINT('Ctrl Pts',(-18.8211474534948,16.6524837656663,
13.5709765664209));
#134905=CARTESIAN_POINT('Ctrl Pts',(-18.9051841270904,16.6553461989804,
13.5751525369372));
#134906=CARTESIAN_POINT('Ctrl Pts',(-18.9890141412379,16.6623511034493,
13.5793285074536));
#134907=CARTESIAN_POINT('Ctrl Pts',(-19.0722035617808,16.6734385030509,
13.5835044779699));
#134908=CARTESIAN_POINT('Ctrl Pts',(-19.1555423768616,16.6845458138013,
13.5876879478435));
#134909=CARTESIAN_POINT('Ctrl Pts',(-19.2382378461903,16.6997501856857,
13.5918714177171));
#134910=CARTESIAN_POINT('Ctrl Pts',(-19.3198660896852,16.7189404250787,
13.5960548875907));
#134911=CARTESIAN_POINT('Ctrl Pts',(-19.3963302483165,16.736916623589,13.5999736966983));
#134912=CARTESIAN_POINT('Ctrl Pts',(-19.471857774533,16.7583897384897,13.6038925058059));
#134913=CARTESIAN_POINT('Ctrl Pts',(-19.5461152252309,16.783229652346,13.6078113149135));
#134914=CARTESIAN_POINT('Ctrl Pts',(-19.6254097949838,16.809754536562,13.6119959493065));
#134915=CARTESIAN_POINT('Ctrl Pts',(-19.7035510491552,16.8402176845382,
13.6161805836996));
#134916=CARTESIAN_POINT('Ctrl Pts',(-19.7801197445754,16.8744997367838,
13.6203652180926));
#134917=CARTESIAN_POINT('Ctrl Pts',(-19.856579453935,16.9087329927713,13.6245438961766));
#134918=CARTESIAN_POINT('Ctrl Pts',(-19.9314706343179,16.9467741695628,
13.6287225742605));
#134919=CARTESIAN_POINT('Ctrl Pts',(-20.0043903176931,16.9884545132413,
13.6329012523445));
#134920=CARTESIAN_POINT('Ctrl Pts',(-20.0786170339864,17.0308819471251,
13.6371548302299));
#134921=CARTESIAN_POINT('Ctrl Pts',(-20.1508004226817,17.0770801423177,
13.6414084081153));
#134922=CARTESIAN_POINT('Ctrl Pts',(-20.2205378947047,17.1268202842349,
13.6456619860008));
#134923=CARTESIAN_POINT('Ctrl Pts',(-20.288923369751,17.1755961164411,13.6498330999787));
#134924=CARTESIAN_POINT('Ctrl Pts',(-20.3549565277687,17.2277775063951,
13.6540042139567));
#134925=CARTESIAN_POINT('Ctrl Pts',(-20.4182851699542,17.283103875653,13.6581753279346));
#134926=CARTESIAN_POINT('Ctrl Pts',(-20.4815925616022,17.3384116796133,
13.662345042255));
#134927=CARTESIAN_POINT('Ctrl Pts',(-20.5421968936246,17.3968620645641,
13.6665147565753));
#134928=CARTESIAN_POINT('Ctrl Pts',(-20.5997791685761,17.4581542868503,
13.6706844708957));
#134929=CARTESIAN_POINT('Ctrl Pts',(-20.6573593945032,17.5194443280962,
13.6748540368398));
#134930=CARTESIAN_POINT('Ctrl Pts',(-20.7119174628062,17.5835756697508,
13.6790236027838));
#134931=CARTESIAN_POINT('Ctrl Pts',(-20.763172325239,17.6502118418939,13.6831931687278));
#134932=CARTESIAN_POINT('Ctrl Pts',(-20.8162292454052,17.719190859645,13.6875093314668));
#134933=CARTESIAN_POINT('Ctrl Pts',(-20.8657460348867,17.79085370675,13.6918254942057));
#134934=CARTESIAN_POINT('Ctrl Pts',(-20.911458707217,17.864792891727,13.6961416569446));
#134935=CARTESIAN_POINT('Ctrl Pts',(-20.9556822940543,17.9363235155303,
13.7003172211363));
#134936=CARTESIAN_POINT('Ctrl Pts',(-20.9963456096572,18.0099840160616,
13.704492785328));
#134937=CARTESIAN_POINT('Ctrl Pts',(-21.0332565704859,18.0853805158591,
13.7086683495196));
#134938=CARTESIAN_POINT('Ctrl Pts',(-21.0720318161985,18.1645851136233,
13.7130548115322));
#134939=CARTESIAN_POINT('Ctrl Pts',(-21.1066654530387,18.245705153136,13.7174412735447));
#134940=CARTESIAN_POINT('Ctrl Pts',(-21.1369928787006,18.3282626523623,
13.7218277355573));
#134941=CARTESIAN_POINT('Ctrl Pts',(-21.1673203043624,18.4108201515887,
13.7262141975698));
#134942=CARTESIAN_POINT('Ctrl Pts',(-21.1933414198056,18.494814533789,13.7306006595824));
#134943=CARTESIAN_POINT('Ctrl Pts',(-21.214953227824,18.5797543415201,13.7349871215949));
#134944=CARTESIAN_POINT('Ctrl Pts',(-21.2416966549181,18.6848626949492,
13.740415127754));
#134945=CARTESIAN_POINT('Ctrl Pts',(-21.2617718479477,18.7917315462695,
13.7458431339131));
#134946=CARTESIAN_POINT('Ctrl Pts',(-21.2749934581325,18.8996284442541,
13.7512711400722));
#134947=CARTESIAN_POINT('Ctrl Pts',(-21.2875287526721,19.0019245622934,
13.7564173858785));
#134948=CARTESIAN_POINT('Ctrl Pts',(-21.2939037306914,19.1051449394058,
13.7615636316849));
#134949=CARTESIAN_POINT('Ctrl Pts',(-21.2939989173812,19.2086456408557,
13.7667098774912));
#134950=CARTESIAN_POINT('Ctrl Pts',(-21.2935817003363,19.2086462806877,
13.7667098902285));
#134951=CARTESIAN_POINT('Ctrl Pts',(-21.2877698482561,19.8484613719781,
13.7985275695778));
#134952=CARTESIAN_POINT('Ctrl Pts',(-20.7208250258792,21.3499116215441,
13.8727371844875));
#134953=CARTESIAN_POINT('Ctrl Pts',(-18.1988330521628,22.1904106768542,
13.9893387349578));
#134954=CARTESIAN_POINT('Ctrl Pts',(-15.9391114041072,20.373707779263,14.1165145416392));
#134955=CARTESIAN_POINT('Ctrl Pts',(-16.1737485207935,18.1512291376149,
14.2145391070908));
#134956=CARTESIAN_POINT('Ctrl Pts',(-16.9627571498223,17.3430212960427,
14.2701717369818));
#134957=CARTESIAN_POINT('Ctrl Pts',(-17.1756294966411,17.1824128461128,
14.2834124313123));
#134958=CARTESIAN_POINT('Origin',(-18.734,19.211,-1.76670989022852));
#134959=CARTESIAN_POINT('',(-17.174464231106,17.180864983421,15.149955384767));
#134960=CARTESIAN_POINT('',(-17.174464231106,17.180864983421,15.0832685841393));
#134961=CARTESIAN_POINT('',(-17.174464231106,17.180864983421,-1.76670989022852));
#134962=CARTESIAN_POINT('',(-21.2941234937244,19.2098698166564,14.6332901097715));
#134963=CARTESIAN_POINT('Ctrl Pts',(-21.2939997505486,19.2098698712836,
14.6332901097715));
#134964=CARTESIAN_POINT('Ctrl Pts',(-21.2940362985033,19.2926593390013,
14.6374299052976));
#134965=CARTESIAN_POINT('Ctrl Pts',(-21.2900525381051,19.3756125071059,
14.6415697008237));
#134966=CARTESIAN_POINT('Ctrl Pts',(-21.2820270867845,19.4583013647603,
14.6457094963498));
#134967=CARTESIAN_POINT('Ctrl Pts',(-21.2740124509524,19.5408787868902,
14.6498437128862));
#134968=CARTESIAN_POINT('Ctrl Pts',(-21.2619669829652,19.623192141297,14.6539779294226));
#134969=CARTESIAN_POINT('Ctrl Pts',(-21.2459213201026,19.7048130026779,
14.658112145959));
#134970=CARTESIAN_POINT('Ctrl Pts',(-21.2298921267197,19.7863500873319,
14.6622421190811));
#134971=CARTESIAN_POINT('Ctrl Pts',(-21.209870984755,19.8671956313595,14.6663720922032));
#134972=CARTESIAN_POINT('Ctrl Pts',(-21.1859402178855,19.9469274202771,
14.6705020653253));
#134973=CARTESIAN_POINT('Ctrl Pts',(-21.1620224032908,20.026616055206,14.6746298031431));
#134974=CARTESIAN_POINT('Ctrl Pts',(-21.1341992976676,20.105191681447,14.6787575409609));
#134975=CARTESIAN_POINT('Ctrl Pts',(-21.1026037847566,20.1822446194635,
14.6828852787786));
#134976=CARTESIAN_POINT('Ctrl Pts',(-21.0710154147152,20.2592801379466,
14.6870120834293));
#134977=CARTESIAN_POINT('Ctrl Pts',(-21.0356565094082,20.3347932165768,
14.69113888808));
#134978=CARTESIAN_POINT('Ctrl Pts',(-20.9967085276621,20.4083930511094,
14.6952656927306));
#134979=CARTESIAN_POINT('Ctrl Pts',(-20.9577570758468,20.481999443017,14.6993928650588));
#134980=CARTESIAN_POINT('Ctrl Pts',(-20.915216134864,20.5536918375766,14.703520037387));
#134981=CARTESIAN_POINT('Ctrl Pts',(-20.8693129406042,20.6231043324372,
14.7076472097152));
#134982=CARTESIAN_POINT('Ctrl Pts',(-20.82336222789,20.6925886823078,14.7117786544443));
#134983=CARTESIAN_POINT('Ctrl Pts',(-20.7740425759679,20.7597880294049,
14.7159100991735));
#134984=CARTESIAN_POINT('Ctrl Pts',(-20.7216239583874,20.8243663564251,
14.7200415439026));
#134985=CARTESIAN_POINT('Ctrl Pts',(-20.6691749218121,20.8889821588287,
14.7241753861462));
#134986=CARTESIAN_POINT('Ctrl Pts',(-20.6136236562298,20.9509735655346,
14.7283092283899));
#134987=CARTESIAN_POINT('Ctrl Pts',(-20.5552780488243,21.0100403744415,
14.7324430706335));
#134988=CARTESIAN_POINT('Ctrl Pts',(-20.496836459412,21.0692043517748,14.7365837132944));
#134989=CARTESIAN_POINT('Ctrl Pts',(-20.4355917013479,21.1254338132407,
14.7407243559553));
#134990=CARTESIAN_POINT('Ctrl Pts',(-20.3718854170609,21.1784682616447,
14.7448649986162));
#134991=CARTESIAN_POINT('Ctrl Pts',(-20.340529452726,21.2045715933849,14.7469030054635));
#134992=CARTESIAN_POINT('Ctrl Pts',(-20.3085776248467,21.2299015689541,
14.7489410123109));
#134993=CARTESIAN_POINT('Ctrl Pts',(-20.2760730898184,21.2544310817001,
14.7509790191583));
#134994=CARTESIAN_POINT('Ctrl Pts',(-20.2093316088543,21.3047974692387,
14.7551636535513));
#134995=CARTESIAN_POINT('Ctrl Pts',(-20.1399957689001,21.3519843348468,
14.7593482879444));
#134996=CARTESIAN_POINT('Ctrl Pts',(-20.0684012262927,21.3957135664129,
14.7635329223374));
#134997=CARTESIAN_POINT('Ctrl Pts',(-19.9969085896549,21.4393805548305,
14.7677116004214));
#134998=CARTESIAN_POINT('Ctrl Pts',(-19.9231640255691,21.4795994471402,
14.7718902785053));
#134999=CARTESIAN_POINT('Ctrl Pts',(-19.8475347050064,21.5161335017188,
14.7760689565893));
#135000=CARTESIAN_POINT('Ctrl Pts',(-19.7705497832267,21.553322402969,14.7803225344747));
#135001=CARTESIAN_POINT('Ctrl Pts',(-19.6916122567004,21.5866927752846,
14.7845761123602));
#135002=CARTESIAN_POINT('Ctrl Pts',(-19.6111386006649,21.6160421774313,
14.7888296902456));
#135003=CARTESIAN_POINT('Ctrl Pts',(-19.532225083483,21.6448225841468,14.7930008042235));
#135004=CARTESIAN_POINT('Ctrl Pts',(-19.4518349191,21.6697363732163,14.7971719182015));
#135005=CARTESIAN_POINT('Ctrl Pts',(-19.3703822558334,21.6906406240543,
14.8013430321794));
#135006=CARTESIAN_POINT('Ctrl Pts',(-19.2889569247947,21.711537860269,14.8055127464998));
#135007=CARTESIAN_POINT('Ctrl Pts',(-19.2064702481715,21.728428116053,14.8096824608202));
#135008=CARTESIAN_POINT('Ctrl Pts',(-19.1233507011891,21.7412185738555,
14.8138521751405));
#135009=CARTESIAN_POINT('Ctrl Pts',(-19.0402341119568,21.7540085765187,
14.8180217410846));
#135010=CARTESIAN_POINT('Ctrl Pts',(-18.9564851519519,21.7626990021399,
14.8221913070286));
#135011=CARTESIAN_POINT('Ctrl Pts',(-18.8725402767196,21.7672485387236,
14.8263608729727));
#135012=CARTESIAN_POINT('Ctrl Pts',(-18.7856440032315,21.7719580314011,
14.8306770357116));
#135013=CARTESIAN_POINT('Ctrl Pts',(-18.6985383080786,21.7722300013651,
14.8349931984505));
#135014=CARTESIAN_POINT('Ctrl Pts',(-18.6117085473887,21.7680773943348,
14.8393093611894));
#135015=CARTESIAN_POINT('Ctrl Pts',(-18.5277072570202,21.7640600580418,
14.8434849253811));
#135016=CARTESIAN_POINT('Ctrl Pts',(-18.4439646643002,21.7559020718402,
14.8476604895728));
#135017=CARTESIAN_POINT('Ctrl Pts',(-18.3609142114856,21.7436679597627,
14.8518360537645));
#135018=CARTESIAN_POINT('Ctrl Pts',(-18.2736690777334,21.7308159317681,
14.856222515777));
#135019=CARTESIAN_POINT('Ctrl Pts',(-18.187188413865,21.713465300997,14.8606089777895));
#135020=CARTESIAN_POINT('Ctrl Pts',(-18.1019594530762,21.6917508434029,
14.8649954398021));
#135021=CARTESIAN_POINT('Ctrl Pts',(-18.0167304922875,21.6700363858088,
14.8693819018146));
#135022=CARTESIAN_POINT('Ctrl Pts',(-17.932753766134,21.6439583461084,14.8737683638271));
#135023=CARTESIAN_POINT('Ctrl Pts',(-17.8504927560607,21.613709917969,14.8781548258396));
#135024=CARTESIAN_POINT('Ctrl Pts',(-17.7720166970008,21.5848532648472,
14.8823394602327));
#135025=CARTESIAN_POINT('Ctrl Pts',(-17.6948098353987,21.5520941514643,
14.8865240946257));
#135026=CARTESIAN_POINT('Ctrl Pts',(-17.6192877039371,21.5155642748698,
14.8907087290188));
#135027=CARTESIAN_POINT('Ctrl Pts',(-17.543873068882,21.4790863940332,14.8948874071027));
#135028=CARTESIAN_POINT('Ctrl Pts',(-17.4701388113641,21.4388486095631,
14.8990660851867));
#135029=CARTESIAN_POINT('Ctrl Pts',(-17.3984827363062,21.3950315103898,
14.9032447632706));
#135030=CARTESIAN_POINT('Ctrl Pts',(-17.3255422776009,21.3504290212045,
14.907498341156));
#135031=CARTESIAN_POINT('Ctrl Pts',(-17.2547556895192,21.3021178031456,
14.9117519190415));
#135032=CARTESIAN_POINT('Ctrl Pts',(-17.1865186232488,21.2503384683785,
14.9160054969269));
#135033=CARTESIAN_POINT('Ctrl Pts',(-17.1196044656618,21.1995629770549,
14.9201766109048));
#135034=CARTESIAN_POINT('Ctrl Pts',(-17.0551422404864,21.1454529323241,
14.9243477248828));
#135035=CARTESIAN_POINT('Ctrl Pts',(-16.9934762919468,21.0882792071785,
14.9285188388608));
#135036=CARTESIAN_POINT('Ctrl Pts',(-16.9318310360118,21.0311246672285,
14.9326885531811));
#135037=CARTESIAN_POINT('Ctrl Pts',(-16.8729805302658,20.970908801095,14.9368582675015));
#135038=CARTESIAN_POINT('Ctrl Pts',(-16.8172347450929,20.9079416482545,
14.9410279818219));
#135039=CARTESIAN_POINT('Ctrl Pts',(-16.7614909435942,20.8449767360556,
14.9451975477659));
#135040=CARTESIAN_POINT('Ctrl Pts',(-16.7088519473105,20.7792610768136,
14.9493671137099));
#135041=CARTESIAN_POINT('Ctrl Pts',(-16.6595887382006,20.7111392991718,
14.953536679654));
#135042=CARTESIAN_POINT('Ctrl Pts',(-16.608593495431,20.6406224438653,14.9578528423929));
#135043=CARTESIAN_POINT('Ctrl Pts',(-16.5612161510352,20.5675275511998,
14.9621690051318));
#135044=CARTESIAN_POINT('Ctrl Pts',(-16.5177085337784,20.4922697361419,
14.9664851678708));
#135045=CARTESIAN_POINT('Ctrl Pts',(-16.4756181725776,20.4194634364939,
14.9706607320624));
#135046=CARTESIAN_POINT('Ctrl Pts',(-16.4371494708084,20.3446334053666,
14.9748362962541));
#135047=CARTESIAN_POINT('Ctrl Pts',(-16.4024827880432,20.2681790247396,
14.9790118604458));
#135048=CARTESIAN_POINT('Ctrl Pts',(-16.3660651735437,20.1878631150998,
14.9833983224583));
#135049=CARTESIAN_POINT('Ctrl Pts',(-16.3338439651087,20.1057549952923,
14.9877847844709));
#135050=CARTESIAN_POINT('Ctrl Pts',(-16.3059695675779,20.0223373029956,
14.9921712464834));
#135051=CARTESIAN_POINT('Ctrl Pts',(-16.2780951700472,19.9389196106989,
14.996557708496));
#135052=CARTESIAN_POINT('Ctrl Pts',(-16.2545676653735,19.8541929253278,
15.0009441705085));
#135053=CARTESIAN_POINT('Ctrl Pts',(-16.2354754819719,19.7686515334978,
15.0053306325211));
#135054=CARTESIAN_POINT('Ctrl Pts',(-16.2172617582301,19.6870460279088,
15.0095152669141));
#135055=CARTESIAN_POINT('Ctrl Pts',(-16.2030163785017,19.6043953888036,
15.0136999013072));
#135056=CARTESIAN_POINT('Ctrl Pts',(-16.1928535263698,19.5211202985239,
15.0178845357002));
#135057=CARTESIAN_POINT('Ctrl Pts',(-16.1827051397999,19.4379637400279,
15.0220632137842));
#135058=CARTESIAN_POINT('Ctrl Pts',(-16.1766277936582,19.3541849485907,
15.0262418918681));
#135059=CARTESIAN_POINT('Ctrl Pts',(-16.1746849654928,19.270216164561,15.0304205699521));
#135060=CARTESIAN_POINT('Ctrl Pts',(-16.1727073135288,19.1847423004249,
15.0346741478375));
#135061=CARTESIAN_POINT('Ctrl Pts',(-16.1750139649457,19.0990720360281,
15.0389277257229));
#135062=CARTESIAN_POINT('Ctrl Pts',(-16.1816167614736,19.0136682902079,
15.0431813036084));
#135063=CARTESIAN_POINT('Ctrl Pts',(-16.1880915499066,18.9299202626522,
15.0473524175863));
#135064=CARTESIAN_POINT('Ctrl Pts',(-16.1986973545604,18.8464289917134,
15.0515235315643));
#135065=CARTESIAN_POINT('Ctrl Pts',(-16.2133928011124,18.7636306348037,
15.0556946455422));
#135066=CARTESIAN_POINT('Ctrl Pts',(-16.2280833164655,18.6808600616822,
15.0598643598626));
#135067=CARTESIAN_POINT('Ctrl Pts',(-16.2468606679443,18.5987823933903,
15.064034074183));
#135068=CARTESIAN_POINT('Ctrl Pts',(-16.2696319425036,18.5178260844556,
15.0682037885034));
#135069=CARTESIAN_POINT('Ctrl Pts',(-16.2924024067631,18.4368726562939,
15.0723733544474));
#135070=CARTESIAN_POINT('Ctrl Pts',(-16.3191663861463,18.3570409507694,
15.0765429203914));
#135071=CARTESIAN_POINT('Ctrl Pts',(-16.3497807798975,18.278745361774,15.0807124863355));
#135072=CARTESIAN_POINT('Ctrl Pts',(-16.3814715379661,18.1976969964576,
15.0850286490744));
#135073=CARTESIAN_POINT('Ctrl Pts',(-16.4172883172411,18.1182952684027,
15.0893448118133));
#135074=CARTESIAN_POINT('Ctrl Pts',(-16.4570183818635,18.0409766196061,
15.0936609745522));
#135075=CARTESIAN_POINT('Ctrl Pts',(-16.4954542438097,17.9661766176615,
15.0978365387439));
#135076=CARTESIAN_POINT('Ctrl Pts',(-16.5375520792275,17.8933264506922,
15.1020121029356));
#135077=CARTESIAN_POINT('Ctrl Pts',(-16.5830736962918,17.8227939504468,
15.1061876671273));
#135078=CARTESIAN_POINT('Ctrl Pts',(-16.6308945020166,17.7486990212891,
15.1105741291398));
#135079=CARTESIAN_POINT('Ctrl Pts',(-16.6824937078806,17.677162516164,15.1149605911524));
#135080=CARTESIAN_POINT('Ctrl Pts',(-16.7375469032623,17.6085721443614,
15.1193470531649));
#135081=CARTESIAN_POINT('Ctrl Pts',(-16.7926000986441,17.5399817725587,
15.1237335151774));
#135082=CARTESIAN_POINT('Ctrl Pts',(-16.851106840707,17.474337916614,15.12811997719));
#135083=CARTESIAN_POINT('Ctrl Pts',(-16.9126993772537,17.4119824788001,
15.1325064392025));
#135084=CARTESIAN_POINT('Ctrl Pts',(-16.9714542743061,17.3524998282257,
15.1366908118298));
#135085=CARTESIAN_POINT('Ctrl Pts',(-17.0332355735151,17.295787869,15.1408751844571));
#135086=CARTESIAN_POINT('Ctrl Pts',(-17.0977514090542,17.2421702591062,
15.1450595570844));
#135087=CARTESIAN_POINT('Ctrl Pts',(-17.1229131590333,17.2212589141108,
15.1466914996452));
#135088=CARTESIAN_POINT('Ctrl Pts',(-17.1484904128431,17.2008178921216,
15.1483234422061));
#135089=CARTESIAN_POINT('Ctrl Pts',(-17.174464231106,17.180864983421,15.149955384767));
#135090=CARTESIAN_POINT('Ctrl Pts',(-17.1732300624786,17.1792869614928,
14.3497865218036));
#135091=CARTESIAN_POINT('Ctrl Pts',(-17.2767521095298,17.0982003735101,
14.3563415475737));
#135092=CARTESIAN_POINT('Ctrl Pts',(-18.0960849484291,16.5548825890784,
14.4052885089043));
#135093=CARTESIAN_POINT('Ctrl Pts',(-20.1784867160069,16.5507838647211,
14.4966274057954));
#135094=CARTESIAN_POINT('Ctrl Pts',(-21.2671018326456,18.2345793421635,
14.5845735760146));
#135095=CARTESIAN_POINT('Ctrl Pts',(-21.2979709281649,19.1465375840163,
14.6301278106733));
#135096=CARTESIAN_POINT('Ctrl Pts',(-21.2976211493107,19.2098682725933,
14.6332901097715));
#135097=CARTESIAN_POINT('',(-21.2936354898062,19.2115601738724,14.5667099150531));
#135098=CARTESIAN_POINT('Ctrl Pts',(-17.1756294966411,17.1824128461128,
14.2834124313123));
#135099=CARTESIAN_POINT('Ctrl Pts',(-17.6442977536355,16.8288108709757,
14.3125636725423));
#135100=CARTESIAN_POINT('Ctrl Pts',(-19.0929372054435,16.3386618105897,
14.3841068493327));
#135101=CARTESIAN_POINT('Ctrl Pts',(-20.9482576099774,17.4308694729993,
14.4785393356381));
#135102=CARTESIAN_POINT('Ctrl Pts',(-21.2889976010488,18.7496082874005,
14.5438205807135));
#135103=CARTESIAN_POINT('Ctrl Pts',(-21.2898971100035,19.211558854651,14.5667098902285));
#135104=CARTESIAN_POINT('Ctrl Pts',(-21.2939999386838,19.2115603024813,
14.5667099174733));
#135105=CARTESIAN_POINT('Ctrl Pts',(-21.2939802627011,19.301459091566,14.5711571992722));
#135106=CARTESIAN_POINT('Ctrl Pts',(-21.2892209204019,19.3912344818061,
14.5756044810712));
#135107=CARTESIAN_POINT('Ctrl Pts',(-21.2797861099485,19.4803939167712,
14.5800517628701));
#135108=CARTESIAN_POINT('Ctrl Pts',(-21.270316767046,19.5698796851229,14.584515322212));
#135109=CARTESIAN_POINT('Ctrl Pts',(-21.2561377674645,19.6587446305213,
14.5889788815539));
#135110=CARTESIAN_POINT('Ctrl Pts',(-21.2373647797492,19.7465042292186,
14.5934424408958));
#135111=CARTESIAN_POINT('Ctrl Pts',(-21.2185553401057,19.8344342326829,
14.5979146672303));
#135112=CARTESIAN_POINT('Ctrl Pts',(-21.1951342035234,19.9212542602487,
14.6023868935647));
#135113=CARTESIAN_POINT('Ctrl Pts',(-21.1672666877215,20.0064955854214,
14.6068591198992));
#135114=CARTESIAN_POINT('Ctrl Pts',(-21.1393161596827,20.0919908289243,
14.6113446681786));
#135115=CARTESIAN_POINT('Ctrl Pts',(-21.1068928974848,20.1758976314735,
14.615830216458));
#135116=CARTESIAN_POINT('Ctrl Pts',(-21.0702104967872,20.2577666954491,
14.6203157647375));
#135117=CARTESIAN_POINT('Ctrl Pts',(-21.0568477853949,20.2875900617789,
14.6219497659466));
#135118=CARTESIAN_POINT('Ctrl Pts',(-21.0429203172376,20.3171432681498,
14.6235837671558));
#135119=CARTESIAN_POINT('Ctrl Pts',(-21.0284398795323,20.3464054955,14.6252177683649));
#135120=CARTESIAN_POINT('Ctrl Pts',(-20.9913558570061,20.4213452949944,
14.6294024027579));
#135121=CARTESIAN_POINT('Ctrl Pts',(-20.9505274948145,20.4946058152548,
14.633587037151));
#135122=CARTESIAN_POINT('Ctrl Pts',(-20.9061301751472,20.5657879916116,
14.637771671544));
#135123=CARTESIAN_POINT('Ctrl Pts',(-20.8617960495691,20.636868848951,14.641950349628));
#135124=CARTESIAN_POINT('Ctrl Pts',(-20.8139032983065,20.7058768514385,
14.6461290277119));
#135125=CARTESIAN_POINT('Ctrl Pts',(-20.7626740190628,20.7724357893874,
14.6503077057959));
#135126=CARTESIAN_POINT('Ctrl Pts',(-20.7105264918065,20.8401877484639,
14.6545612836813));
#135127=CARTESIAN_POINT('Ctrl Pts',(-20.6549218593555,20.9054015483268,
14.6588148615668));
#135128=CARTESIAN_POINT('Ctrl Pts',(-20.5961416680528,20.9677095400496,
14.6630684394522));
#135129=CARTESIAN_POINT('Ctrl Pts',(-20.5385010454587,21.0288095697688,
14.6672395534301));
#135130=CARTESIAN_POINT('Ctrl Pts',(-20.4778072242622,21.0871151053885,
14.6714106674081));
#135131=CARTESIAN_POINT('Ctrl Pts',(-20.4143663508875,21.1423127470208,
14.6755817813861));
#135132=CARTESIAN_POINT('Ctrl Pts',(-20.3509467657105,21.1974918665513,
14.6797514957064));
#135133=CARTESIAN_POINT('Ctrl Pts',(-20.2847823058331,21.2495648615671,
14.6839212100268));
#135134=CARTESIAN_POINT('Ctrl Pts',(-20.2162143833073,21.2982566976577,
14.6880909243472));
#135135=CARTESIAN_POINT('Ctrl Pts',(-20.1476489007224,21.3469468010838,
14.6922604902912));
#135136=CARTESIAN_POINT('Ctrl Pts',(-20.0766805011099,21.3922557191444,
14.6964300562353));
#135137=CARTESIAN_POINT('Ctrl Pts',(-20.0036808175629,21.433950881489,14.7005996221793));
#135138=CARTESIAN_POINT('Ctrl Pts',(-19.9281145551974,21.477111994305,14.7049157849182));
#135139=CARTESIAN_POINT('Ctrl Pts',(-19.850371969323,21.5164002423867,14.7092319476572));
#135140=CARTESIAN_POINT('Ctrl Pts',(-19.7708927266886,21.5516096371117,
14.7135481103961));
#135141=CARTESIAN_POINT('Ctrl Pts',(-19.6940025120233,21.5856720895069,
14.7177236745878));
#135142=CARTESIAN_POINT('Ctrl Pts',(-19.6154875027973,21.6159172197028,
14.7218992387794));
#135143=CARTESIAN_POINT('Ctrl Pts',(-19.5357640795052,21.6422084157503,
14.7260748029711));
#135144=CARTESIAN_POINT('Ctrl Pts',(-19.4520140156271,21.6698275176088,
14.7304612649837));
#135145=CARTESIAN_POINT('Ctrl Pts',(-19.3669308187544,21.6930826078309,
14.7348477269962));
#135146=CARTESIAN_POINT('Ctrl Pts',(-19.2810104439706,21.7118757614458,
14.7392341890088));
#135147=CARTESIAN_POINT('Ctrl Pts',(-19.1950900691869,21.7306689150607,
14.7436206510213));
#135148=CARTESIAN_POINT('Ctrl Pts',(-19.1083331013483,21.7450001125529,
14.7480071130338));
#135149=CARTESIAN_POINT('Ctrl Pts',(-19.021240449396,21.7548342957494,14.7523935750464));
#135150=CARTESIAN_POINT('Ctrl Pts',(-18.9381550594623,21.7642159935992,
14.7565782094394));
#135151=CARTESIAN_POINT('Ctrl Pts',(-18.8544549375686,21.7695403323457,
14.7607628438325));
#135152=CARTESIAN_POINT('Ctrl Pts',(-18.770570565002,21.7707387745189,14.7649474782255));
#135153=CARTESIAN_POINT('Ctrl Pts',(-18.6868055914569,21.7719355108579,
14.7691261563095));
#135154=CARTESIAN_POINT('Ctrl Pts',(-18.6028573442174,21.7690180091444,
14.7733048343934));
#135155=CARTESIAN_POINT('Ctrl Pts',(-18.5191623733682,21.7619693832312,
14.7774835124774));
#135156=CARTESIAN_POINT('Ctrl Pts',(-18.4339672303171,21.7547944157644,
14.7817370903628));
#135157=CARTESIAN_POINT('Ctrl Pts',(-18.3490350120195,21.7433387124852,
14.7859906682482));
#135158=CARTESIAN_POINT('Ctrl Pts',(-18.2648272487365,21.7276400079216,
14.7902442461337));
#135159=CARTESIAN_POINT('Ctrl Pts',(-18.1822520172626,21.7122456533795,
14.7944153601116));
#135160=CARTESIAN_POINT('Ctrl Pts',(-18.1003738745931,21.6927714353377,
14.7985864740896));
#135161=CARTESIAN_POINT('Ctrl Pts',(-18.0196220516901,21.6693051370748,
14.8027575880676));
#135162=CARTESIAN_POINT('Ctrl Pts',(-17.9388973258412,21.645846713155,14.8069273023879));
#135163=CARTESIAN_POINT('Ctrl Pts',(-17.8592986105396,21.6183989977105,
14.8110970167083));
#135164=CARTESIAN_POINT('Ctrl Pts',(-17.7812419660678,21.5871001933373,
14.8152667310287));
#135165=CARTESIAN_POINT('Ctrl Pts',(-17.7031880991865,21.5558025027099,
14.8194362969727));
#135166=CARTESIAN_POINT('Ctrl Pts',(-17.6266766207012,21.5206541676232,
14.8236058629168));
#135167=CARTESIAN_POINT('Ctrl Pts',(-17.5521042434164,21.4818417867764,
14.8277754288608));
#135168=CARTESIAN_POINT('Ctrl Pts',(-17.4749099933414,21.4416648104993,
14.8320915915997));
#135169=CARTESIAN_POINT('Ctrl Pts',(-17.3997942069759,21.3975615823359,
14.8364077543386));
#135170=CARTESIAN_POINT('Ctrl Pts',(-17.3271680714248,21.349790294709,14.8407239170776));
#135171=CARTESIAN_POINT('Ctrl Pts',(-17.2569077246003,21.3035751517518,
14.8448994812692));
#135172=CARTESIAN_POINT('Ctrl Pts',(-17.188977671162,21.253927569593,14.8490750454609));
#135173=CARTESIAN_POINT('Ctrl Pts',(-17.1237181590043,21.2011237128781,
14.8532506096526));
#135174=CARTESIAN_POINT('Ctrl Pts',(-17.0551625440275,21.1456528588898,
14.8576370716651));
#135175=CARTESIAN_POINT('Ctrl Pts',(-16.9895547726119,21.0866988942974,
14.8620235336777));
#135176=CARTESIAN_POINT('Ctrl Pts',(-16.9272456352412,21.0246258339098,
14.8664099956902));
#135177=CARTESIAN_POINT('Ctrl Pts',(-16.8649364978706,20.9625527735222,
14.8707964577027));
#135178=CARTESIAN_POINT('Ctrl Pts',(-16.8059263275258,20.8973610985477,
14.8751829197153));
#135179=CARTESIAN_POINT('Ctrl Pts',(-16.7505157350919,20.8294530178111,
14.8795693817278));
#135180=CARTESIAN_POINT('Ctrl Pts',(-16.697654666154,20.764669488533,14.8837540161209));
#135181=CARTESIAN_POINT('Ctrl Pts',(-16.6478724513804,20.6971728954314,
14.8879386505139));
#135182=CARTESIAN_POINT('Ctrl Pts',(-16.6014597312931,20.6272881071108,
14.892123284907));
#135183=CARTESIAN_POINT('Ctrl Pts',(-16.5551130739681,20.5575027911364,
14.8963019629909));
#135184=CARTESIAN_POINT('Ctrl Pts',(-16.5121266371783,20.4853364119635,
14.9004806410748));
#135185=CARTESIAN_POINT('Ctrl Pts',(-16.4727509157821,20.4111468989768,
14.9046593191588));
#135186=CARTESIAN_POINT('Ctrl Pts',(-16.4326694128786,20.3356275922887,
14.9089128970442));
#135187=CARTESIAN_POINT('Ctrl Pts',(-16.3963296475344,20.2580122826049,
14.9131664749297));
#135188=CARTESIAN_POINT('Ctrl Pts',(-16.3639497085599,20.1787094688205,
14.9174200528151));
#135189=CARTESIAN_POINT('Ctrl Pts',(-16.3321975178868,20.1009440948281,
14.9215911667931));
#135190=CARTESIAN_POINT('Ctrl Pts',(-16.3042531677129,20.0215565094719,
14.925762280771));
#135191=CARTESIAN_POINT('Ctrl Pts',(-16.2802751807719,19.9409551434874,
14.929933394749));
#135192=CARTESIAN_POINT('Ctrl Pts',(-16.2563052398759,19.8603808240697,
14.9341031090693));
#135193=CARTESIAN_POINT('Ctrl Pts',(-16.2362991499858,19.7785939734879,
14.9382728233897));
#135194=CARTESIAN_POINT('Ctrl Pts',(-16.2203659101292,19.6960192390406,
14.9424425377101));
#135195=CARTESIAN_POINT('Ctrl Pts',(-16.2044332372457,19.6134474429567,
14.9466121036541));
#135196=CARTESIAN_POINT('Ctrl Pts',(-16.1925732125599,19.530088270613,14.9507816695982));
#135197=CARTESIAN_POINT('Ctrl Pts',(-16.1848436692124,19.4463762970338,
14.9549512355422));
#135198=CARTESIAN_POINT('Ctrl Pts',(-16.1768423646562,19.3597211137334,
14.9592673982811));
#135199=CARTESIAN_POINT('Ctrl Pts',(-16.1732674495782,19.2726883838098,
14.9635835610201));
#135200=CARTESIAN_POINT('Ctrl Pts',(-16.1741243927921,19.185763605208,14.967899723759));
#135201=CARTESIAN_POINT('Ctrl Pts',(-16.174953421171,19.1016703921263,14.9720752879507));
#135202=CARTESIAN_POINT('Ctrl Pts',(-16.1799299313355,19.0176786727672,
14.9762508521424));
#135203=CARTESIAN_POINT('Ctrl Pts',(-16.1890058822548,18.9342240244489,
14.980426416334));
#135204=CARTESIAN_POINT('Ctrl Pts',(-16.198540237879,18.8465542802385,14.9848128783466));
#135205=CARTESIAN_POINT('Ctrl Pts',(-16.2125989501167,18.7594778642492,
14.9891993403591));
#135206=CARTESIAN_POINT('Ctrl Pts',(-16.2310658163554,18.6734867700759,
14.9935858023717));
#135207=CARTESIAN_POINT('Ctrl Pts',(-16.2495326825942,18.5874956759026,
14.9979722643842));
#135208=CARTESIAN_POINT('Ctrl Pts',(-16.2724074784504,18.5025904439986,
15.0023587263968));
#135209=CARTESIAN_POINT('Ctrl Pts',(-16.2995147249237,18.4192415485537,
15.0067451884093));
#135210=CARTESIAN_POINT('Ctrl Pts',(-16.3253715040259,18.3397375686843,
15.0109293012963));
#135211=CARTESIAN_POINT('Ctrl Pts',(-16.3551750808439,18.2613536084849,
15.0151134141832));
#135212=CARTESIAN_POINT('Ctrl Pts',(-16.3888096569691,18.1845097394741,
15.0192975270702));
#135213=CARTESIAN_POINT('Ctrl Pts',(-16.4223989481496,18.1077693315666,
15.0234760065482));
#135214=CARTESIAN_POINT('Ctrl Pts',(-16.4598088142964,18.0325653152782,
15.0276544860263));
#135215=CARTESIAN_POINT('Ctrl Pts',(-16.5008739124279,17.9593020024763,
15.0318329655043));
#135216=CARTESIAN_POINT('Ctrl Pts',(-16.5429986601539,17.884148192799,15.0361192670572));
#135217=CARTESIAN_POINT('Ctrl Pts',(-16.5889697495617,17.8110370999845,
15.0404055686101));
#135218=CARTESIAN_POINT('Ctrl Pts',(-16.6385563150878,17.7403825231007,
15.0446918701631));
#135219=CARTESIAN_POINT('Ctrl Pts',(-16.686808182088,17.6716297226077,15.0488627993302));
#135220=CARTESIAN_POINT('Ctrl Pts',(-16.7384830670581,17.6052032663847,
15.0530337284974));
#135221=CARTESIAN_POINT('Ctrl Pts',(-16.7933230566453,17.5414572477676,
15.0572046576646));
#135222=CARTESIAN_POINT('Ctrl Pts',(-16.8504384458537,17.4750663040202,
15.0615486454104));
#135223=CARTESIAN_POINT('Ctrl Pts',(-16.9109870226805,17.4115835115971,
15.0658926331562));
#135224=CARTESIAN_POINT('Ctrl Pts',(-16.9746305398746,17.35137124598,15.0702366209019));
#135225=CARTESIAN_POINT('Ctrl Pts',(-17.0382740570687,17.2911589803629,
15.0745806086477));
#135226=CARTESIAN_POINT('Ctrl Pts',(-17.1050121046529,17.2342176296957,
15.0789245963935));
#135227=CARTESIAN_POINT('Ctrl Pts',(-17.174464231106,17.180864983421,15.0832685841393));
#135228=CARTESIAN_POINT('Origin',(-18.734,19.211,-1.76670989022852));
#135229=CARTESIAN_POINT('',(-17.174464231106,17.180864983421,15.9499155238083));
#135230=CARTESIAN_POINT('',(-17.172599350298,17.1784745189047,15.8832287057516));
#135231=CARTESIAN_POINT('',(-17.174464231106,17.180864983421,-1.76670989022852));
#135232=CARTESIAN_POINT('',(-21.293999428374,19.2092892327452,15.4332901097416));
#135233=CARTESIAN_POINT('Ctrl Pts',(-21.2939994283744,19.2092892333484,
15.4332901097715));
#135234=CARTESIAN_POINT('Ctrl Pts',(-21.2940559692553,19.2938972788889,
15.437482057942));
#135235=CARTESIAN_POINT('Ctrl Pts',(-21.2899137324165,19.3785303101354,
15.4416740061124));
#135236=CARTESIAN_POINT('Ctrl Pts',(-21.2815918669692,19.4627452667924,
15.4458659542829));
#135237=CARTESIAN_POINT('Ctrl Pts',(-21.2732695913204,19.546964374574,15.4500581090829));
#135238=CARTESIAN_POINT('Ctrl Pts',(-21.2607673227297,19.6307649161162,
15.4542502638829));
#135239=CARTESIAN_POINT('Ctrl Pts',(-21.2441560631152,19.7137091990464,
15.4584424186829));
#135240=CARTESIAN_POINT('Ctrl Pts',(-21.2275392030058,19.7966814466854,
15.4626359868702));
#135241=CARTESIAN_POINT('Ctrl Pts',(-21.2068106889623,19.878796418332,15.4668295550574));
#135242=CARTESIAN_POINT('Ctrl Pts',(-21.1820923104738,19.9596281048684,
15.4710231232446));
#135243=CARTESIAN_POINT('Ctrl Pts',(-21.157341575289,20.0405656011908,15.4752221808701));
#135244=CARTESIAN_POINT('Ctrl Pts',(-21.1285906849039,20.1202160261787,
15.4794212384956));
#135245=CARTESIAN_POINT('Ctrl Pts',(-21.0960107310932,20.1981703531815,
15.483620296121));
#135246=CARTESIAN_POINT('Ctrl Pts',(-21.0634063961448,20.2761830171356,
15.4878224961022));
#135247=CARTESIAN_POINT('Ctrl Pts',(-21.0269674888695,20.3524966484648,
15.4920246960833));
#135248=CARTESIAN_POINT('Ctrl Pts',(-20.9869114421225,20.4267261344371,
15.4962268960644));
#135249=CARTESIAN_POINT('Ctrl Pts',(-20.9467843119665,20.5010873479597,
15.5004365532642));
#135250=CARTESIAN_POINT('Ctrl Pts',(-20.903027463882,20.5733566470828,15.504646210464));
#135251=CARTESIAN_POINT('Ctrl Pts',(-20.8559018807143,20.6431775059751,
15.5088558676638));
#135252=CARTESIAN_POINT('Ctrl Pts',(-20.8365799691026,20.6718046841124,
15.5105818648582));
#135253=CARTESIAN_POINT('Ctrl Pts',(-20.8166922183619,20.7000206489315,
15.5123078620525));
#135254=CARTESIAN_POINT('Ctrl Pts',(-20.7962584977301,20.7278025212729,
15.5140338592469));
#135255=CARTESIAN_POINT('Ctrl Pts',(-20.7467174843304,20.7951589334867,
15.5182184936399));
#135256=CARTESIAN_POINT('Ctrl Pts',(-20.6937808669813,20.8602110167103,
15.522403128033));
#135257=CARTESIAN_POINT('Ctrl Pts',(-20.6376906991395,20.9225962497066,
15.526587762426));
#135258=CARTESIAN_POINT('Ctrl Pts',(-20.5816803687091,20.9848926850455,
15.53076644051));
#135259=CARTESIAN_POINT('Ctrl Pts',(-20.5225257086781,21.0445294709031,
15.5349451185939));
#135260=CARTESIAN_POINT('Ctrl Pts',(-20.4605108062945,21.1011747103769,
15.5391237966779));
#135261=CARTESIAN_POINT('Ctrl Pts',(-20.3973843313549,21.1588352750581,
15.5433773745633));
#135262=CARTESIAN_POINT('Ctrl Pts',(-20.3312943514667,21.213395603145,15.5476309524487));
#135263=CARTESIAN_POINT('Ctrl Pts',(-20.2625820107878,21.2645425577026,
15.5518845303342));
#135264=CARTESIAN_POINT('Ctrl Pts',(-20.195201792914,21.3146979287411,15.5560556443121));
#135265=CARTESIAN_POINT('Ctrl Pts',(-20.1253003720614,21.3615708076597,
15.5602267582901));
#135266=CARTESIAN_POINT('Ctrl Pts',(-20.0532336923064,21.4049057557433,
15.564397872268));
#135267=CARTESIAN_POINT('Ctrl Pts',(-19.9811911952217,21.4482261623666,
15.5685675865884));
#135268=CARTESIAN_POINT('Ctrl Pts',(-19.9069852761388,21.4880107590574,
15.5727373009088));
#135269=CARTESIAN_POINT('Ctrl Pts',(-19.8309999421956,21.5240480165407,
15.5769070152291));
#135270=CARTESIAN_POINT('Ctrl Pts',(-19.7550173121366,21.5600839916638,
15.5810765811732));
#135271=CARTESIAN_POINT('Ctrl Pts',(-19.677255809133,21.592372696345,15.5852461471172));
#135272=CARTESIAN_POINT('Ctrl Pts',(-19.5981218233861,21.6207496704736,
15.5894157130613));
#135273=CARTESIAN_POINT('Ctrl Pts',(-19.5162055843226,21.6501243440058,
15.5937318758002));
#135274=CARTESIAN_POINT('Ctrl Pts',(-19.4328190502825,21.6753069180703,
15.5980480385391));
#135275=CARTESIAN_POINT('Ctrl Pts',(-19.3484309915966,21.696170931056,15.602364201278));
#135276=CARTESIAN_POINT('Ctrl Pts',(-19.2667918650464,21.7163553010132,
15.6065397654697));
#135277=CARTESIAN_POINT('Ctrl Pts',(-19.1842159325099,21.7324980994094,
15.6107153296614));
#135278=CARTESIAN_POINT('Ctrl Pts',(-19.1011369778114,21.7445371399534,
15.6148908938531));
#135279=CARTESIAN_POINT('Ctrl Pts',(-19.0138619026126,21.7571842438153,
15.6192773558656));
#135280=CARTESIAN_POINT('Ctrl Pts',(-18.9260322359069,21.7653020795901,
15.6236638178782));
#135281=CARTESIAN_POINT('Ctrl Pts',(-18.8381534037013,21.7688803858854,
15.6280502798907));
#135282=CARTESIAN_POINT('Ctrl Pts',(-18.7502745714957,21.7724586921808,
15.6324367419032));
#135283=CARTESIAN_POINT('Ctrl Pts',(-18.6623471531412,21.771497551399,15.6368232039158));
#135284=CARTESIAN_POINT('Ctrl Pts',(-18.5748705298081,21.7660494734381,
15.6412096659283));
#135285=CARTESIAN_POINT('Ctrl Pts',(-18.4914188355861,21.7608520696202,
15.6453943003213));
#135286=CARTESIAN_POINT('Ctrl Pts',(-18.4080667413617,21.7515522106695,
15.6495789347144));
#135287=CARTESIAN_POINT('Ctrl Pts',(-18.3252500890704,21.7381571993675,
15.6537635691074));
#135288=CARTESIAN_POINT('Ctrl Pts',(-18.2425513160331,21.7247812542061,
15.6579422471914));
#135289=CARTESIAN_POINT('Ctrl Pts',(-18.1603869213351,21.7073218076316,
15.6621209252753));
#135290=CARTESIAN_POINT('Ctrl Pts',(-18.0791897487866,21.6858380825634,
15.6662996033592));
#135291=CARTESIAN_POINT('Ctrl Pts',(-17.9965371752754,21.6639692771633,
15.6705531812447));
#135292=CARTESIAN_POINT('Ctrl Pts',(-17.9148873210955,21.6379305338184,
15.6748067591301));
#135293=CARTESIAN_POINT('Ctrl Pts',(-17.8346881397166,21.6078392056943,
15.6790603370156));
#135294=CARTESIAN_POINT('Ctrl Pts',(-17.7560437759646,21.5783312566844,
15.6832314509935));
#135295=CARTESIAN_POINT('Ctrl Pts',(-17.6787947892658,21.5449266242313,
15.6874025649715));
#135296=CARTESIAN_POINT('Ctrl Pts',(-17.6033486289331,21.5077863368421,
15.6915736789494));
#135297=CARTESIAN_POINT('Ctrl Pts',(-17.5279277852881,21.470658512235,15.6957433932698));
#135298=CARTESIAN_POINT('Ctrl Pts',(-17.4543089789471,21.4297977252417,
15.6999131075901));
#135299=CARTESIAN_POINT('Ctrl Pts',(-17.3828779283357,21.3854123683104,
15.7040828219105));
#135300=CARTESIAN_POINT('Ctrl Pts',(-17.3114494195476,21.3410285908007,
15.7082523878546));
#135301=CARTESIAN_POINT('Ctrl Pts',(-17.2422089019967,21.2931207362396,
15.7124219537986));
#135302=CARTESIAN_POINT('Ctrl Pts',(-17.1755146319181,21.2419414953352,
15.7165915197426));
#135303=CARTESIAN_POINT('Ctrl Pts',(-17.1064754735796,21.1889628554569,
15.7209076824816));
#135304=CARTESIAN_POINT('Ctrl Pts',(-17.0401653646947,21.13247882625,15.7252238452205));
#135305=CARTESIAN_POINT('Ctrl Pts',(-16.9769443759548,21.0728151181068,
15.7295400079594));
#135306=CARTESIAN_POINT('Ctrl Pts',(-16.9157828042734,21.0150949489809,
15.7337155721511));
#135307=CARTESIAN_POINT('Ctrl Pts',(-16.8575124793698,20.9543994482419,
15.7378911363428));
#135308=CARTESIAN_POINT('Ctrl Pts',(-16.8024204890304,20.8910596991781,
15.7420667005344));
#135309=CARTESIAN_POINT('Ctrl Pts',(-16.7445459332276,20.8245208099649,
15.746453162547));
#135310=CARTESIAN_POINT('Ctrl Pts',(-16.6901795852498,20.7550639901493,
15.7508396245595));
#135311=CARTESIAN_POINT('Ctrl Pts',(-16.6396036508155,20.6831086687207,
15.7552260865721));
#135312=CARTESIAN_POINT('Ctrl Pts',(-16.5890277163812,20.611153347292,15.7596125485846));
#135313=CARTESIAN_POINT('Ctrl Pts',(-16.5422424397948,20.5367000559955,
15.7639990105972));
#135314=CARTESIAN_POINT('Ctrl Pts',(-16.499473974098,20.4601971179787,15.7683854726097));
#135315=CARTESIAN_POINT('Ctrl Pts',(-16.458673348906,20.3872141935448,15.7725701070028));
#135316=CARTESIAN_POINT('Ctrl Pts',(-16.4213761508428,20.3120944357928,
15.7767547413958));
#135317=CARTESIAN_POINT('Ctrl Pts',(-16.3878121523981,20.2352082716739,
15.7809393757889));
#135318=CARTESIAN_POINT('Ctrl Pts',(-16.3542959281508,20.158431545493,15.7851180538728));
#135319=CARTESIAN_POINT('Ctrl Pts',(-16.3245025312236,20.0798938250632,
15.7892967319567));
#135320=CARTESIAN_POINT('Ctrl Pts',(-16.2986164546586,19.9999911197726,
15.7934754100407));
#135321=CARTESIAN_POINT('Ctrl Pts',(-16.272266388775,19.9186562159147,15.7977289879261));
#135322=CARTESIAN_POINT('Ctrl Pts',(-16.249965333752,19.8359073320103,15.8019825658115));
#135323=CARTESIAN_POINT('Ctrl Pts',(-16.2318570828658,19.75218464708,15.806236143697));
#135324=CARTESIAN_POINT('Ctrl Pts',(-16.2140998957584,19.6700850897684,
15.8104072576749));
#135325=CARTESIAN_POINT('Ctrl Pts',(-16.2003744938966,19.587049622894,15.8145783716529));
#135326=CARTESIAN_POINT('Ctrl Pts',(-16.1907660223746,19.5035080085253,
15.8187494856308));
#135327=CARTESIAN_POINT('Ctrl Pts',(-16.1811607750679,19.4199944273522,
15.8229191999512));
#135328=CARTESIAN_POINT('Ctrl Pts',(-16.1756697669882,19.3359754926348,
15.8270889142716));
#135329=CARTESIAN_POINT('Ctrl Pts',(-16.1743265551335,19.2518883314074,
15.8312586285919));
#135330=CARTESIAN_POINT('Ctrl Pts',(-16.172983391076,19.1678041623621,15.835428194536));
#135331=CARTESIAN_POINT('Ctrl Pts',(-16.1757877362795,19.0836522316217,
15.83959776048));
#135332=CARTESIAN_POINT('Ctrl Pts',(-16.182721035153,18.9998705526721,15.8437673264241));
#135333=CARTESIAN_POINT('Ctrl Pts',(-16.1898981002617,18.9131432132465,
15.848083489163));
#135334=CARTESIAN_POINT('Ctrl Pts',(-16.2014998257646,18.8268131717714,
15.8523996519019));
#135335=CARTESIAN_POINT('Ctrl Pts',(-16.2174472402024,18.7413594915735,
15.8567158146408));
#135336=CARTESIAN_POINT('Ctrl Pts',(-16.2328751692923,18.6586894560197,
15.8608913788325));
#135337=CARTESIAN_POINT('Ctrl Pts',(-16.2523698584564,18.5768400108858,
15.8650669430242));
#135338=CARTESIAN_POINT('Ctrl Pts',(-16.275808314218,18.4962317606719,15.8692425072159));
#135339=CARTESIAN_POINT('Ctrl Pts',(-16.3004305906604,18.4115521793678,
15.8736289692284));
#135340=CARTESIAN_POINT('Ctrl Pts',(-16.3294053113241,18.3282430251664,
15.8780154312409));
#135341=CARTESIAN_POINT('Ctrl Pts',(-16.3625325554082,18.2467686173739,
15.8824018932535));
#135342=CARTESIAN_POINT('Ctrl Pts',(-16.3956597994922,18.1652942095814,
15.886788355266));
#135343=CARTESIAN_POINT('Ctrl Pts',(-16.4329392521203,18.0856550414426,
15.8911748172785));
#135344=CARTESIAN_POINT('Ctrl Pts',(-16.4741163568262,18.0082839406928,
15.8955612792911));
#135345=CARTESIAN_POINT('Ctrl Pts',(-16.5134028649731,17.9344652397022,
15.8997463422483));
#135346=CARTESIAN_POINT('Ctrl Pts',(-16.5563832077405,17.8624361059901,
15.9039314052056));
#135347=CARTESIAN_POINT('Ctrl Pts',(-16.6028702262198,17.7925903668871,
15.9081164681628));
#135348=CARTESIAN_POINT('Ctrl Pts',(-16.6492791580825,17.7228619512356,
15.9122945012563));
#135349=CARTESIAN_POINT('Ctrl Pts',(-16.6991828014219,17.6553100178988,
15.9164725343498));
#135350=CARTESIAN_POINT('Ctrl Pts',(-16.7523481443525,17.5903038770304,
15.9206505674433));
#135351=CARTESIAN_POINT('Ctrl Pts',(-16.8054619536389,17.525360747198,15.9248245507318));
#135352=CARTESIAN_POINT('Ctrl Pts',(-16.8618308964002,17.4629588649887,
15.9289985340203));
#135353=CARTESIAN_POINT('Ctrl Pts',(-16.9211791819185,17.4034379176553,
15.9331725173088));
#135354=CARTESIAN_POINT('Ctrl Pts',(-16.9804837256409,17.3439608393757,
15.9373434242233));
#135355=CARTESIAN_POINT('Ctrl Pts',(-17.0427629244188,17.2873608011024,
15.9415143311377));
#135356=CARTESIAN_POINT('Ctrl Pts',(-17.1077022600073,17.2339426763762,
15.9456852380522));
#135357=CARTESIAN_POINT('Ctrl Pts',(-17.1296568733952,17.2158831402623,
15.9470953333042));
#135358=CARTESIAN_POINT('Ctrl Pts',(-17.1519152216166,17.1981869775567,
15.9485054285563));
#135359=CARTESIAN_POINT('Ctrl Pts',(-17.174464231106,17.180864983421,15.9499155238083));
#135360=CARTESIAN_POINT('Ctrl Pts',(-17.174464231106,17.180864983421,15.149955384767));
#135361=CARTESIAN_POINT('Ctrl Pts',(-17.240940630191,17.1297982704617,15.1541321162688));
#135362=CARTESIAN_POINT('Ctrl Pts',(-17.3100170700777,17.0819316454899,
15.1583088477706));
#135363=CARTESIAN_POINT('Ctrl Pts',(-17.3813512206993,17.0375370304842,
15.1624855792724));
#135364=CARTESIAN_POINT('Ctrl Pts',(-17.4526154142036,16.9931859531006,
15.1666582146703));
#135365=CARTESIAN_POINT('Ctrl Pts',(-17.5261325291112,16.9523003606111,
15.1708308500681));
#135366=CARTESIAN_POINT('Ctrl Pts',(-17.6015298591648,16.9151098937195,
15.175003485466));
#135367=CARTESIAN_POINT('Ctrl Pts',(-17.6768876681862,16.8779389209617,
15.1791739336928));
#135368=CARTESIAN_POINT('Ctrl Pts',(-17.7541233237704,16.8444594312558,
15.1833443819196));
#135369=CARTESIAN_POINT('Ctrl Pts',(-17.8328390496217,16.8148554005417,
15.1875148301464));
#135370=CARTESIAN_POINT('Ctrl Pts',(-17.9115371280723,16.7852580068011,
15.1916843433939));
#135371=CARTESIAN_POINT('Ctrl Pts',(-17.9917141871842,16.7595345078961,
15.1958538566414));
#135372=CARTESIAN_POINT('Ctrl Pts',(-18.0729532517235,16.7378204277503,
15.200023369889));
#135373=CARTESIAN_POINT('Ctrl Pts',(-18.1541984727113,16.7161047020709,
15.20419319911));
#135374=CARTESIAN_POINT('Ctrl Pts',(-18.236505414156,16.6983991159896,15.2083630283311));
#135375=CARTESIAN_POINT('Ctrl Pts',(-18.3194440819341,16.6847887279967,
15.2125328575522));
#135376=CARTESIAN_POINT('Ctrl Pts',(-18.4024695461715,16.6711640965452,
15.216707050557));
#135377=CARTESIAN_POINT('Ctrl Pts',(-18.4861276019741,16.6616432956659,
15.2208812435618));
#135378=CARTESIAN_POINT('Ctrl Pts',(-18.5699807426584,16.6562597620852,
15.2250554365667));
#135379=CARTESIAN_POINT('Ctrl Pts',(-18.6538792241245,16.6508733175387,
15.2292318866268));
#135380=CARTESIAN_POINT('Ctrl Pts',(-18.7379725403117,16.6496286017922,
15.2334083366869));
#135381=CARTESIAN_POINT('Ctrl Pts',(-18.8218232182444,16.6525068727204,
15.237584786747));
#135382=CARTESIAN_POINT('Ctrl Pts',(-18.9058197639797,16.6553901507285,
15.2417685022176));
#135383=CARTESIAN_POINT('Ctrl Pts',(-18.989572369497,16.6624107030258,15.2459522176882));
#135384=CARTESIAN_POINT('Ctrl Pts',(-19.0726489290364,16.6734979009147,
15.2501359331588));
#135385=CARTESIAN_POINT('Ctrl Pts',(-19.135836369568,16.6819307448017,15.2533180374005));
#135386=CARTESIAN_POINT('Ctrl Pts',(-19.1986328257473,16.6927150716866,
15.2565001416423));
#135387=CARTESIAN_POINT('Ctrl Pts',(-19.2608535512399,16.7058003401833,
15.259682245884));
#135388=CARTESIAN_POINT('Ctrl Pts',(-19.3426770768309,16.7230081562804,
15.263866880277));
#135389=CARTESIAN_POINT('Ctrl Pts',(-19.4238089369641,16.74426092691,15.2680515146701));
#135390=CARTESIAN_POINT('Ctrl Pts',(-19.5038189245164,16.7694884142285,
15.2722361490631));
#135391=CARTESIAN_POINT('Ctrl Pts',(-19.5837150277547,16.7946799933414,
15.2764148271471));
#135392=CARTESIAN_POINT('Ctrl Pts',(-19.6624919952645,16.8238349143801,
15.280593505231));
#135393=CARTESIAN_POINT('Ctrl Pts',(-19.7397300928959,16.8568319982967,
15.284772183315));
#135394=CARTESIAN_POINT('Ctrl Pts',(-19.8183526279172,16.8904205312279,
15.2890257612004));
#135395=CARTESIAN_POINT('Ctrl Pts',(-19.895380110122,16.92799022417,15.2932793390859));
#135396=CARTESIAN_POINT('Ctrl Pts',(-19.9703862586171,16.9693601940761,
15.2975329169713));
#135397=CARTESIAN_POINT('Ctrl Pts',(-20.0439382665611,17.0099281263885,
15.3017040309492));
#135398=CARTESIAN_POINT('Ctrl Pts',(-20.1155461950125,17.0541500666243,
15.3058751449272));
#135399=CARTESIAN_POINT('Ctrl Pts',(-20.1848301560492,17.1018077711365,
15.3100462589051));
#135400=CARTESIAN_POINT('Ctrl Pts',(-20.2540908681836,17.1494494836456,
15.3142159732255));
#135401=CARTESIAN_POINT('Ctrl Pts',(-20.3210287829504,17.2005244102481,
15.3183856875459));
#135402=CARTESIAN_POINT('Ctrl Pts',(-20.3852923626423,17.2547705827079,
15.3225554018662));
#135403=CARTESIAN_POINT('Ctrl Pts',(-20.4495536555603,17.3090148248561,
15.3267249678103));
#135404=CARTESIAN_POINT('Ctrl Pts',(-20.5111404516292,17.3664297911047,
15.3308945337543));
#135405=CARTESIAN_POINT('Ctrl Pts',(-20.5697347912254,17.4267136507039,
15.3350640996984));
#135406=CARTESIAN_POINT('Ctrl Pts',(-20.6303892355179,17.4891170164384,
15.3393802624373));
#135407=CARTESIAN_POINT('Ctrl Pts',(-20.68783651095,17.5545943914713,15.3436964251762));
#135408=CARTESIAN_POINT('Ctrl Pts',(-20.7417674193154,17.6227714301979,
15.3480125879151));
#135409=CARTESIAN_POINT('Ctrl Pts',(-20.7939415340132,17.6887276090589,
15.3521881521068));
#135410=CARTESIAN_POINT('Ctrl Pts',(-20.8428246196127,17.7572098587051,
15.3563637162985));
#135411=CARTESIAN_POINT('Ctrl Pts',(-20.8881804708299,17.8278490685774,
15.3605392804902));
#135412=CARTESIAN_POINT('Ctrl Pts',(-20.9358271382688,17.9020560970117,
15.3649257425027));
#135413=CARTESIAN_POINT('Ctrl Pts',(-20.9795805961808,17.9786432012269,
15.3693122045153));
#135414=CARTESIAN_POINT('Ctrl Pts',(-21.0192222426253,18.0571545589591,
15.3736986665278));
#135415=CARTESIAN_POINT('Ctrl Pts',(-21.0588638890698,18.1356659166914,
15.3780851285404));
#135416=CARTESIAN_POINT('Ctrl Pts',(-21.0943935591862,18.2161009664617,
15.3824715905529));
#135417=CARTESIAN_POINT('Ctrl Pts',(-21.1256522921828,18.2979833992217,
15.3868580525655));
#135418=CARTESIAN_POINT('Ctrl Pts',(-21.1596866697224,18.3871366489942,
15.3916340140292));
#135419=CARTESIAN_POINT('Ctrl Pts',(-21.188765023978,18.4782809296074,15.396409975493));
#135420=CARTESIAN_POINT('Ctrl Pts',(-21.2126811308611,18.5708907503299,
15.4011859369568));
#135421=CARTESIAN_POINT('Ctrl Pts',(-21.236499376369,18.6631216245769,15.4059423558521));
#135422=CARTESIAN_POINT('Ctrl Pts',(-21.2551974088383,18.7568058878157,
15.4106987747474));
#135423=CARTESIAN_POINT('Ctrl Pts',(-21.2686182636666,18.8514026453274,
15.4154551936427));
#135424=CARTESIAN_POINT('Ctrl Pts',(-21.2819450244393,18.9453361818536,
15.4201782651283));
#135425=CARTESIAN_POINT('Ctrl Pts',(-21.2900682365864,19.0401692636774,
15.4249013366139));
#135426=CARTESIAN_POINT('Ctrl Pts',(-21.2928821031966,19.1353535728531,
15.4296244080995));
#135427=CARTESIAN_POINT('Ctrl Pts',(-21.2936100754836,19.1599785991387,
15.4308463086469));
#135428=CARTESIAN_POINT('Ctrl Pts',(-21.2939829474075,19.1846270439602,
15.4320682091942));
#135429=CARTESIAN_POINT('Ctrl Pts',(-21.293999428374,19.2092892327452,15.4332901097416));
#135430=CARTESIAN_POINT('',(-21.2939991231355,19.2131188547121,15.3667098902285));
#135431=CARTESIAN_POINT('Ctrl Pts',(-17.174464231106,17.180864983421,15.0832685841393));
#135432=CARTESIAN_POINT('Ctrl Pts',(-17.2419505642565,17.1290224460527,
15.0874896183852));
#135433=CARTESIAN_POINT('Ctrl Pts',(-17.3119989353086,17.0805684098818,
15.0917106526312));
#135434=CARTESIAN_POINT('Ctrl Pts',(-17.3842279949674,17.0357493168762,
15.0959316868771));
#135435=CARTESIAN_POINT('Ctrl Pts',(-17.4556818847612,16.9914112270907,
15.1001074205396));
#135436=CARTESIAN_POINT('Ctrl Pts',(-17.5292694432467,16.9506306039143,
15.104283154202));
#135437=CARTESIAN_POINT('Ctrl Pts',(-17.6045968973434,16.9135995926462,
15.1084588878645));
#135438=CARTESIAN_POINT('Ctrl Pts',(-17.6811501399716,16.8759659831692,
15.1127025724022));
#135439=CARTESIAN_POINT('Ctrl Pts',(-17.7594999534078,16.8422053023395,
15.1169462569399));
#135440=CARTESIAN_POINT('Ctrl Pts',(-17.8392139784633,16.8124675370839,
15.1211899414776));
#135441=CARTESIAN_POINT('Ctrl Pts',(-17.9189280035187,16.7827297718283,
15.1254336260153));
#135442=CARTESIAN_POINT('Ctrl Pts',(-18.0000057517656,16.7570150077627,
15.129677310553));
#135443=CARTESIAN_POINT('Ctrl Pts',(-18.0820028534396,16.7354193164275,
15.1339209950906));
#135444=CARTESIAN_POINT('Ctrl Pts',(-18.1628589794658,16.7141241254443,
15.1381056294837));
#135445=CARTESIAN_POINT('Ctrl Pts',(-18.2449099711144,16.6967547916185,
15.1422902638767));
#135446=CARTESIAN_POINT('Ctrl Pts',(-18.3277397785879,16.6834413691275,
15.1464748982698));
#135447=CARTESIAN_POINT('Ctrl Pts',(-18.4104516880828,16.6701468966455,
15.1506535763537));
#135448=CARTESIAN_POINT('Ctrl Pts',(-18.4939397611591,16.66089694071,15.1548322544377));
#135449=CARTESIAN_POINT('Ctrl Pts',(-18.5777744754985,16.6557713242267,
15.1590109325216));
#135450=CARTESIAN_POINT('Ctrl Pts',(-18.6631118668416,16.6505538347517,
15.163264510407));
#135451=CARTESIAN_POINT('Ctrl Pts',(-18.7488079825292,16.6496101194126,
15.1675180882925));
#135452=CARTESIAN_POINT('Ctrl Pts',(-18.8344006857351,16.652969565798,15.1717716661779));
#135453=CARTESIAN_POINT('Ctrl Pts',(-18.9183340073688,16.6562638827597,
15.1759427801559));
#135454=CARTESIAN_POINT('Ctrl Pts',(-19.0021674095958,16.6636959811426,
15.1801138941338));
#135455=CARTESIAN_POINT('Ctrl Pts',(-19.085463479757,16.6752410559367,15.1842850081118));
#135456=CARTESIAN_POINT('Ctrl Pts',(-19.1687315991175,16.6867822566694,
15.1884547224321));
#135457=CARTESIAN_POINT('Ctrl Pts',(-19.2514622892072,16.70243362971,15.1926244367525));
#135458=CARTESIAN_POINT('Ctrl Pts',(-19.3332238803081,16.7221185762941,
15.1967941510729));
#135459=CARTESIAN_POINT('Ctrl Pts',(-19.4149825619807,16.7418028224032,
15.2009637170169));
#135460=CARTESIAN_POINT('Ctrl Pts',(-19.4957717661756,16.7655202481684,
15.205133282961));
#135461=CARTESIAN_POINT('Ctrl Pts',(-19.5751719705258,16.7931435700187,
15.209302848905));
#135462=CARTESIAN_POINT('Ctrl Pts',(-19.6573637881102,16.8217380937883,
15.2136190116439));
#135463=CARTESIAN_POINT('Ctrl Pts',(-19.7380666159158,16.8545181133117,
15.2179351743828));
#135464=CARTESIAN_POINT('Ctrl Pts',(-19.8168362586915,16.891287596088,15.2222513371218));
#135465=CARTESIAN_POINT('Ctrl Pts',(-19.8930399886387,16.9268593168303,
15.2264269013134));
#135466=CARTESIAN_POINT('Ctrl Pts',(-19.9674341519877,16.966164316944,15.2306024655051));
#135467=CARTESIAN_POINT('Ctrl Pts',(-20.0396421490695,17.0089785244977,
15.2347780296968));
#135468=CARTESIAN_POINT('Ctrl Pts',(-20.1154972004258,17.0539551758939,
15.2391644917093));
#135469=CARTESIAN_POINT('Ctrl Pts',(-20.1889389488847,17.1028045279329,
15.2435509537219));
#135470=CARTESIAN_POINT('Ctrl Pts',(-20.2595676620249,17.1552171056787,
15.2479374157344));
#135471=CARTESIAN_POINT('Ctrl Pts',(-20.3301963751651,17.2076296834245,
15.252323877747));
#135472=CARTESIAN_POINT('Ctrl Pts',(-20.3980116539333,17.2636050588652,
15.2567103397595));
#135473=CARTESIAN_POINT('Ctrl Pts',(-20.4626578964189,17.3227887096121,
15.2610968017721));
#135474=CARTESIAN_POINT('Ctrl Pts',(-20.5234100187947,17.3784072924496,
15.2652190348167));
#135475=CARTESIAN_POINT('Ctrl Pts',(-20.5816044022757,17.4370795204071,
15.2693412678613));
#135476=CARTESIAN_POINT('Ctrl Pts',(-20.6369112461388,17.498537215202,15.2734635009059));
#135477=CARTESIAN_POINT('Ctrl Pts',(-20.6921256485485,17.5598921878337,
15.2775788439313));
#135478=CARTESIAN_POINT('Ctrl Pts',(-20.7444617859859,17.6240230272318,
15.2816941869567));
#135479=CARTESIAN_POINT('Ctrl Pts',(-20.793624524071,17.6906228034315,15.2858095299821));
#135480=CARTESIAN_POINT('Ctrl Pts',(-20.8427410076366,17.7571599195604,
15.2899210011074));
#135481=CARTESIAN_POINT('Ctrl Pts',(-20.8886897335868,17.8261609852054,
15.2940324722326));
#135482=CARTESIAN_POINT('Ctrl Pts',(-20.9312146121396,17.8972846776412,
15.2981439433579));
#135483=CARTESIAN_POINT('Ctrl Pts',(-20.9737131282073,17.9683642783043,
15.3022528656552));
#135484=CARTESIAN_POINT('Ctrl Pts',(-21.0127917657825,18.0415634879279,
15.3063617879526));
#135485=CARTESIAN_POINT('Ctrl Pts',(-21.0482376124066,18.1165118669796,
15.3104707102499));
#135486=CARTESIAN_POINT('Ctrl Pts',(-21.0836728562224,18.1914378269505,
15.3145784034579));
#135487=CARTESIAN_POINT('Ctrl Pts',(-21.1154772648512,18.2681114878987,
15.3186860966658));
#135488=CARTESIAN_POINT('Ctrl Pts',(-21.1434845038954,18.3461390715913,
15.3227937898737));
#135489=CARTESIAN_POINT('Ctrl Pts',(-21.1715053065244,18.4242044431482,
15.3269034723903));
#135490=CARTESIAN_POINT('Ctrl Pts',(-21.1957251016689,18.5036246009545,
15.331013154907));
#135491=CARTESIAN_POINT('Ctrl Pts',(-21.2160265895475,18.5839880313906,
15.3351228374236));
#135492=CARTESIAN_POINT('Ctrl Pts',(-21.2363332616047,18.6643719833958,
15.339233569387));
#135493=CARTESIAN_POINT('Ctrl Pts',(-21.2527195357628,18.7456992225568,
15.3433443013503));
#135494=CARTESIAN_POINT('Ctrl Pts',(-21.2651191757883,18.827547632741,15.3474550333136));
#135495=CARTESIAN_POINT('Ctrl Pts',(-21.2775338661873,18.9094953884813,
15.3515707547807));
#135496=CARTESIAN_POINT('Ctrl Pts',(-21.2859522113273,18.9919651056503,
15.3556864762478));
#135497=CARTESIAN_POINT('Ctrl Pts',(-21.2903598951031,19.0745299054426,
15.3598021977149));
#135498=CARTESIAN_POINT('Ctrl Pts',(-21.292825799276,19.1207212600627,15.3621047618861));
#135499=CARTESIAN_POINT('Ctrl Pts',(-21.294037342402,19.1669423575626,15.3644073260573));
#135500=CARTESIAN_POINT('Ctrl Pts',(-21.2939991231355,19.2131188547121,
15.3667098902285));
#135501=CARTESIAN_POINT('Ctrl Pts',(-21.2956374879243,19.2131202107504,
15.3667098902285));
#135502=CARTESIAN_POINT('Ctrl Pts',(-21.2969229026965,19.3573559385303,
15.3738974629702));
#135503=CARTESIAN_POINT('Ctrl Pts',(-21.2201492855026,20.3509180416766,
15.4234769712724));
#135504=CARTESIAN_POINT('Ctrl Pts',(-19.9200692925299,21.9960549863024,
15.515448415135));
#135505=CARTESIAN_POINT('Ctrl Pts',(-17.0342063134898,21.7157940168225,
15.6426242218164));
#135506=CARTESIAN_POINT('Ctrl Pts',(-15.7555914341564,19.2304392007512,
15.7652176520219));
#135507=CARTESIAN_POINT('Ctrl Pts',(-16.5753465329547,17.6447069007991,
15.845419146667));
#135508=CARTESIAN_POINT('Ctrl Pts',(-17.172599350298,17.1784745189047,15.8832287057516));
#135509=CARTESIAN_POINT('Origin',(-18.734,19.211,-1.76670989022852));
#135510=CARTESIAN_POINT('',(-17.174464231106,17.180864983421,16.749817664185));
#135511=CARTESIAN_POINT('',(-17.174464231106,17.180864983421,16.6833822560226));
#135512=CARTESIAN_POINT('',(-17.174464231106,17.180864983421,-1.76670989022852));
#135513=CARTESIAN_POINT('',(-21.2939992944986,19.2129005700935,16.2332901098004));
#135514=CARTESIAN_POINT('Ctrl Pts',(-21.2939992944986,19.2129005700935,
16.2332901098004));
#135515=CARTESIAN_POINT('Ctrl Pts',(-21.2939272486892,19.3099436741152,
16.2381006886061));
#135516=CARTESIAN_POINT('Ctrl Pts',(-21.2883332378637,19.4067618611679,
16.2429112674118));
#135517=CARTESIAN_POINT('Ctrl Pts',(-21.2773175036261,19.5027808694022,
16.2477218462175));
#135518=CARTESIAN_POINT('Ctrl Pts',(-21.2661096544807,19.6004744535223,
16.2526163217372));
#135519=CARTESIAN_POINT('Ctrl Pts',(-21.2492893600036,19.6973405506026,
16.2575107972568));
#135520=CARTESIAN_POINT('Ctrl Pts',(-21.2270132516536,19.792794574639,16.2624052727765));
#135521=CARTESIAN_POINT('Ctrl Pts',(-21.2047371433036,19.8882485986755,
16.2672997482961));
#135522=CARTESIAN_POINT('Ctrl Pts',(-21.1770053785922,19.9822904288902,
16.2721942238158));
#135523=CARTESIAN_POINT('Ctrl Pts',(-21.1440235064311,20.074357804418,16.2770886993354));
#135524=CARTESIAN_POINT('Ctrl Pts',(-21.1158249638011,20.1530727360925,
16.2812733337285));
#135525=CARTESIAN_POINT('Ctrl Pts',(-21.0837134704203,20.2305511910393,
16.2854579681215));
#135526=CARTESIAN_POINT('Ctrl Pts',(-21.0478172393665,20.3063765484118,
16.2896426025146));
#135527=CARTESIAN_POINT('Ctrl Pts',(-21.0119721021545,20.3820939777732,
16.2938212805985));
#135528=CARTESIAN_POINT('Ctrl Pts',(-20.9723531229123,20.4561625710811,
16.2979999586825));
#135529=CARTESIAN_POINT('Ctrl Pts',(-20.9291375533232,20.5281830252437,
16.3021786367664));
#135530=CARTESIAN_POINT('Ctrl Pts',(-20.8851473757077,20.601494394287,16.3064322146518));
#135531=CARTESIAN_POINT('Ctrl Pts',(-20.8374305643565,20.6726830222908,
16.3106857925373));
#135532=CARTESIAN_POINT('Ctrl Pts',(-20.7862244101177,20.7413512572338,
16.3149393704227));
#135533=CARTESIAN_POINT('Ctrl Pts',(-20.7360109870995,20.8086882244473,
16.3191104844007));
#135534=CARTESIAN_POINT('Ctrl Pts',(-20.6824425969519,20.873601266221,16.3232815983786));
#135535=CARTESIAN_POINT('Ctrl Pts',(-20.6257872198946,20.9357437823176,
16.3274527123566));
#135536=CARTESIAN_POINT('Ctrl Pts',(-20.5691508540963,20.9978654458928,
16.331622426677));
#135537=CARTESIAN_POINT('Ctrl Pts',(-20.5094298683183,21.0572180904716,
16.3357921409973));
#135538=CARTESIAN_POINT('Ctrl Pts',(-20.4469316957122,21.1134891605011,
16.3399618553177));
#135539=CARTESIAN_POINT('Ctrl Pts',(-20.3844357470594,21.1697582281645,
16.3441314212617));
#135540=CARTESIAN_POINT('Ctrl Pts',(-20.3191631505145,21.2229456321213,
16.3483009872058));
#135541=CARTESIAN_POINT('Ctrl Pts',(-20.2514562536424,21.2727775142535,
16.3524705531498));
#135542=CARTESIAN_POINT('Ctrl Pts',(-20.1813688658018,21.3243614238873,
16.3567867158888));
#135543=CARTESIAN_POINT('Ctrl Pts',(-20.1086732374466,21.372349148503,16.3611028786277));
#135544=CARTESIAN_POINT('Ctrl Pts',(-20.0337823603681,21.4164853923062,
16.3654190413666));
#135545=CARTESIAN_POINT('Ctrl Pts',(-19.9613310457333,21.4591839026097,
16.3695946055583));
#135546=CARTESIAN_POINT('Ctrl Pts',(-19.8868257455395,21.498277825633,16.37377016975));
#135547=CARTESIAN_POINT('Ctrl Pts',(-19.8106643175712,21.5335834640049,
16.3779457339416));
#135548=CARTESIAN_POINT('Ctrl Pts',(-19.7306561569328,21.5706723062398,
16.3823321959542));
#135549=CARTESIAN_POINT('Ctrl Pts',(-19.6488207114389,21.6035798961264,
16.3867186579667));
#135550=CARTESIAN_POINT('Ctrl Pts',(-19.565639342473,21.6321517928562,16.3911051199793));
#135551=CARTESIAN_POINT('Ctrl Pts',(-19.4824579735071,21.6607236895861,
16.3954915819918));
#135552=CARTESIAN_POINT('Ctrl Pts',(-19.3979312597773,21.6849598063577,
16.3998780440043));
#135553=CARTESIAN_POINT('Ctrl Pts',(-19.3125527301391,21.7047675790756,
16.4042645060169));
#135554=CARTESIAN_POINT('Ctrl Pts',(-19.2311025932108,21.7236639668085,
16.4084491404099));
#135555=CARTESIAN_POINT('Ctrl Pts',(-19.1485741315075,21.7386009007969,
16.412633774803));
#135556=CARTESIAN_POINT('Ctrl Pts',(-19.0653870565367,21.7494606789864,
16.416818409196));
#135557=CARTESIAN_POINT('Ctrl Pts',(-18.9823183880706,21.7603049996257,
16.42099708728));
#135558=CARTESIAN_POINT('Ctrl Pts',(-18.8985934206773,21.7670836326581,
16.4251757653639));
#135559=CARTESIAN_POINT('Ctrl Pts',(-18.81464384804,21.769729483508,16.4293544434479));
#135560=CARTESIAN_POINT('Ctrl Pts',(-18.7291895396467,21.7724227593329,
16.4336080213333));
#135561=CARTESIAN_POINT('Ctrl Pts',(-18.6435029643767,21.770833526475,16.4378615992187));
#135562=CARTESIAN_POINT('Ctrl Pts',(-18.5580469256855,21.7649460674884,
16.4421151771042));
#135563=CARTESIAN_POINT('Ctrl Pts',(-18.4742476190581,21.7591727483826,
16.4462862910821));
#135564=CARTESIAN_POINT('Ctrl Pts',(-18.390670470056,21.7492664079889,16.4504574050601));
#135565=CARTESIAN_POINT('Ctrl Pts',(-18.3077519672383,21.7352647671286,
16.454628519038));
#135566=CARTESIAN_POINT('Ctrl Pts',(-18.224861288525,21.7212678246541,16.4587982333584));
#135567=CARTESIAN_POINT('Ctrl Pts',(-18.1426292702904,21.7031783874643,
16.4629679476788));
#135568=CARTESIAN_POINT('Ctrl Pts',(-18.0614851300253,21.6810857777945,
16.4671376619991));
#135569=CARTESIAN_POINT('Ctrl Pts',(-17.980343877217,21.6589939542747,16.4713072279432));
#135570=CARTESIAN_POINT('Ctrl Pts',(-17.9002908690615,21.6328993631756,
16.4754767938872));
#135571=CARTESIAN_POINT('Ctrl Pts',(-17.8217416831406,21.6029416304168,
16.4796463598313));
#135572=CARTESIAN_POINT('Ctrl Pts',(-17.7404308047436,21.5719306207309,
16.4839625225702));
#135573=CARTESIAN_POINT('Ctrl Pts',(-17.6607319577168,21.5367799467921,
16.4882786853091));
#135574=CARTESIAN_POINT('Ctrl Pts',(-17.5830833500456,21.4976986825679,
16.492594848048));
#135575=CARTESIAN_POINT('Ctrl Pts',(-17.5079641376021,21.4598904864152,
16.4967704122397));
#135576=CARTESIAN_POINT('Ctrl Pts',(-17.4347640291968,21.4184041187291,
16.5009459764314));
#135577=CARTESIAN_POINT('Ctrl Pts',(-17.363852838121,21.3734746830413,16.5051215406231));
#135578=CARTESIAN_POINT('Ctrl Pts',(-17.2893600913592,21.3262759683666,
16.5095080026356));
#135579=CARTESIAN_POINT('Ctrl Pts',(-17.2173940414898,21.2752775637101,
16.5138944646481));
#135580=CARTESIAN_POINT('Ctrl Pts',(-17.1483451005789,21.2208006219378,
16.5182809266607));
#135581=CARTESIAN_POINT('Ctrl Pts',(-17.079296159668,21.1663236801655,16.5226673886732));
#135582=CARTESIAN_POINT('Ctrl Pts',(-17.0131647139457,21.1083686408955,
16.5270538506858));
#135583=CARTESIAN_POINT('Ctrl Pts',(-16.9502957329767,21.047300380603,16.5314403126983));
#135584=CARTESIAN_POINT('Ctrl Pts',(-16.8903194470162,20.9890419614914,
16.5356249470914));
#135585=CARTESIAN_POINT('Ctrl Pts',(-16.8330887583091,20.9277336646776,
16.5398095814844));
#135586=CARTESIAN_POINT('Ctrl Pts',(-16.7789298175348,20.8636646912291,
16.5439942158775));
#135587=CARTESIAN_POINT('Ctrl Pts',(-16.7248479653092,20.7996869120342,
16.5481728939614));
#135588=CARTESIAN_POINT('Ctrl Pts',(-16.6738294707905,20.7329566097131,
16.5523515720454));
#135589=CARTESIAN_POINT('Ctrl Pts',(-16.6261644175017,20.6638004533156,
16.5565302501293));
#135590=CARTESIAN_POINT('Ctrl Pts',(-16.5776450023889,20.5934047225163,
16.5607838280147));
#135591=CARTESIAN_POINT('Ctrl Pts',(-16.5326007777017,20.520495651305,16.5650374059002));
#135592=CARTESIAN_POINT('Ctrl Pts',(-16.4912954660574,20.445453876592,16.5692909837856));
#135593=CARTESIAN_POINT('Ctrl Pts',(-16.4507909384799,20.3718669331139,
16.5734620977636));
#135594=CARTESIAN_POINT('Ctrl Pts',(-16.4138818774498,20.2962296630071,
16.5776332117415));
#135595=CARTESIAN_POINT('Ctrl Pts',(-16.3807728287042,20.2189295016393,
16.5818043257195));
#135596=CARTESIAN_POINT('Ctrl Pts',(-16.3476748900196,20.1416552790873,
16.5859740400399));
#135597=CARTESIAN_POINT('Ctrl Pts',(-16.3183746121639,20.0627196959934,
16.5901437543602));
#135598=CARTESIAN_POINT('Ctrl Pts',(-16.2930292165598,19.9825320047743,
16.5943134686806));
#135599=CARTESIAN_POINT('Ctrl Pts',(-16.2676847228535,19.9023471669774,
16.5984830346247));
#135600=CARTESIAN_POINT('Ctrl Pts',(-16.2462949694201,19.8209107485429,
16.6026526005687));
#135601=CARTESIAN_POINT('Ctrl Pts',(-16.2289674972205,19.7386477613125,
16.6068221665128));
#135602=CARTESIAN_POINT('Ctrl Pts',(-16.2110308124741,19.6534925089336,
16.6111383292517));
#135603=CARTESIAN_POINT('Ctrl Pts',(-16.1974474922546,19.5674519980822,
16.6154544919906));
#135604=CARTESIAN_POINT('Ctrl Pts',(-16.1882789321129,19.4810078600996,
16.6197706547295));
#135605=CARTESIAN_POINT('Ctrl Pts',(-16.1794090368535,19.3973796308195,
16.6239462189212));
#135606=CARTESIAN_POINT('Ctrl Pts',(-16.1746706763875,19.3133741398416,
16.6281217831129));
#135607=CARTESIAN_POINT('Ctrl Pts',(-16.1740663387713,19.2294295987024,
16.6322973473046));
#135608=CARTESIAN_POINT('Ctrl Pts',(-16.1734314774988,19.1412452183496,
16.6366838093171));
#135609=CARTESIAN_POINT('Ctrl Pts',(-16.1773592072922,19.0531286901045,
16.6410702713296));
#135610=CARTESIAN_POINT('Ctrl Pts',(-16.1857908120614,18.965582122686,16.6454567333422));
#135611=CARTESIAN_POINT('Ctrl Pts',(-16.1942224168306,18.8780355552674,
16.6498431953547));
#135612=CARTESIAN_POINT('Ctrl Pts',(-16.2071577359856,18.7910595113906,
16.6542296573673));
#135613=CARTESIAN_POINT('Ctrl Pts',(-16.2244766916358,18.7051415565825,
16.6586161193798));
#135614=CARTESIAN_POINT('Ctrl Pts',(-16.240994821372,18.6231964351303,16.6627997520462));
#135615=CARTESIAN_POINT('Ctrl Pts',(-16.2615616142013,18.5419087704143,
16.6669833847125));
#135616=CARTESIAN_POINT('Ctrl Pts',(-16.2861104910119,18.4617090339621,
16.6711670173789));
#135617=CARTESIAN_POINT('Ctrl Pts',(-16.3106270618205,18.3816148393183,
16.6753451444392));
#135618=CARTESIAN_POINT('Ctrl Pts',(-16.339115179776,18.3026061663184,16.6795232714995));
#135619=CARTESIAN_POINT('Ctrl Pts',(-16.3714572466673,18.2251035862349,
16.6837013985598));
#135620=CARTESIAN_POINT('Ctrl Pts',(-16.4037664575567,18.1476797402942,
16.6878752811));
#135621=CARTESIAN_POINT('Ctrl Pts',(-16.4399216659457,18.0717593708794,
16.6920491636403));
#135622=CARTESIAN_POINT('Ctrl Pts',(-16.4797558270827,17.9977468488117,
16.6962230461805));
#135623=CARTESIAN_POINT('Ctrl Pts',(-16.5195614728604,17.9237873087472,
16.7003939408391));
#135624=CARTESIAN_POINT('Ctrl Pts',(-16.5630406213955,17.85173330636,16.7045648354977));
#135625=CARTESIAN_POINT('Ctrl Pts',(-16.6099791482389,17.7819669628438,
16.7087357301563));
#135626=CARTESIAN_POINT('Ctrl Pts',(-16.6569061252189,17.7122177862859,
16.7129055985095));
#135627=CARTESIAN_POINT('Ctrl Pts',(-16.7072905385225,17.6447555353964,
16.7170754668627));
#135628=CARTESIAN_POINT('Ctrl Pts',(-16.7608741705703,17.579934562552,16.7212453352159));
#135629=CARTESIAN_POINT('Ctrl Pts',(-16.814450725419,17.5151221511081,16.7254146528227));
#135630=CARTESIAN_POINT('Ctrl Pts',(-16.8712253612617,17.4529506748475,
16.7295839704296));
#135631=CARTESIAN_POINT('Ctrl Pts',(-16.9308997149285,17.3937412506814,
16.7337532880365));
#135632=CARTESIAN_POINT('Ctrl Pts',(-16.9906010256115,17.3345050795242,
16.7379244890716));
#135633=CARTESIAN_POINT('Ctrl Pts',(-17.0532043372424,17.2782339503866,
16.7420956901067));
#135634=CARTESIAN_POINT('Ctrl Pts',(-17.1183753223192,17.2252112647946,
16.7462668911418));
#135635=CARTESIAN_POINT('Ctrl Pts',(-17.1368677880835,17.2101659160572,
16.7474504821562));
#135636=CARTESIAN_POINT('Ctrl Pts',(-17.155566790538,17.1953818674044,16.7486340731706));
#135637=CARTESIAN_POINT('Ctrl Pts',(-17.174464231106,17.180864983421,16.749817664185));
#135638=CARTESIAN_POINT('Ctrl Pts',(-17.174464231106,17.180864983421,15.9499155238083));
#135639=CARTESIAN_POINT('Ctrl Pts',(-17.2411397248561,17.1296453273081,
15.9540850549449));
#135640=CARTESIAN_POINT('Ctrl Pts',(-17.3103588008463,17.0817002942196,
15.9582545860814));
#135641=CARTESIAN_POINT('Ctrl Pts',(-17.3817622485653,17.0372812823194,
15.962424117218));
#135642=CARTESIAN_POINT('Ctrl Pts',(-17.453169987322,16.9928596010292,15.9665938989253));
#135643=CARTESIAN_POINT('Ctrl Pts',(-17.5267619671467,16.95196460357,15.9707636806326));
#135644=CARTESIAN_POINT('Ctrl Pts',(-17.6021517731608,16.9148032333006,
15.9749334623399));
#135645=CARTESIAN_POINT('Ctrl Pts',(-17.6776197620901,16.8776033248731,
15.9791075683147));
#135646=CARTESIAN_POINT('Ctrl Pts',(-17.7548888870243,16.8441449798714,
15.9832816742895));
#135647=CARTESIAN_POINT('Ctrl Pts',(-17.8335504480885,16.8145879727262,
15.9874557802643));
#135648=CARTESIAN_POINT('Ctrl Pts',(-17.9122534362687,16.7850153993814,
15.9916320845323));
#135649=CARTESIAN_POINT('Ctrl Pts',(-17.992349882587,16.7593483961333,15.9958083888003));
#135650=CARTESIAN_POINT('Ctrl Pts',(-18.0734158610802,16.7376968250116,
15.9999846930683));
#135651=CARTESIAN_POINT('Ctrl Pts',(-18.1546241977047,16.7160072320557,
16.0041683312497));
#135652=CARTESIAN_POINT('Ctrl Pts',(-18.2368050172129,16.6983472540206,
16.0083519694312));
#135653=CARTESIAN_POINT('Ctrl Pts',(-18.3195243135909,16.6847755631426,
16.0125356076127));
#135654=CARTESIAN_POINT('Ctrl Pts',(-18.3867591839236,16.6737443900507,
16.0159361003993));
#135655=CARTESIAN_POINT('Ctrl Pts',(-18.4543495507435,16.6654131903478,
16.0193365931859));
#135656=CARTESIAN_POINT('Ctrl Pts',(-18.5220617179684,16.6597880988421,
16.0227370859726));
#135657=CARTESIAN_POINT('Ctrl Pts',(-18.6053880714047,16.6528658811356,
16.0269217203656));
#135658=CARTESIAN_POINT('Ctrl Pts',(-18.6892089831255,16.6500174172729,
16.0311063547587));
#135659=CARTESIAN_POINT('Ctrl Pts',(-18.7730921344107,16.6512984929826,
16.0352909891517));
#135660=CARTESIAN_POINT('Ctrl Pts',(-18.856855888413,16.6525777452396,16.0394696672357));
#135661=CARTESIAN_POINT('Ctrl Pts',(-18.9406812499664,16.6579748547684,
16.0436483453196));
#135662=CARTESIAN_POINT('Ctrl Pts',(-19.0241313606307,16.6674937991861,
16.0478270234036));
#135663=CARTESIAN_POINT('Ctrl Pts',(-19.1090772545541,16.6771833638415,
16.052080601289));
#135664=CARTESIAN_POINT('Ctrl Pts',(-19.1936338320393,16.6911440245191,
16.0563341791744));
#135665=CARTESIAN_POINT('Ctrl Pts',(-19.2773408795587,16.7093244237911,
16.0605877570599));
#135666=CARTESIAN_POINT('Ctrl Pts',(-19.359425102621,16.727152360547,16.0647588710378));
#135667=CARTESIAN_POINT('Ctrl Pts',(-19.4406919711072,16.7490377781069,
16.0689299850158));
#135668=CARTESIAN_POINT('Ctrl Pts',(-19.5207150357479,16.7748802466775,
16.0731010989937));
#135669=CARTESIAN_POINT('Ctrl Pts',(-19.6007112478765,16.8007140435582,
16.0772708133141));
#135670=CARTESIAN_POINT('Ctrl Pts',(-19.6794640476566,16.8305021131095,
16.0814405276345));
#135671=CARTESIAN_POINT('Ctrl Pts',(-19.7565616407634,16.8640940174691,
16.0856102419549));
#135672=CARTESIAN_POINT('Ctrl Pts',(-19.8336564904069,16.8976847264846,
16.0897798078989));
#135673=CARTESIAN_POINT('Ctrl Pts',(-19.9090958290849,16.9350788166485,
16.0939493738429));
#135674=CARTESIAN_POINT('Ctrl Pts',(-19.982488631727,16.9760780469,16.098118939787));
#135675=CARTESIAN_POINT('Ctrl Pts',(-20.0584618347703,17.0185187595092,
16.1024351025259));
#135676=CARTESIAN_POINT('Ctrl Pts',(-20.1322414512869,17.0648225852951,
16.1067512652648));
#135677=CARTESIAN_POINT('Ctrl Pts',(-20.2034241040029,17.1147192929917,
16.1110674280037));
#135678=CARTESIAN_POINT('Ctrl Pts',(-20.2722879892937,17.1629906206833,
16.1152429921954));
#135679=CARTESIAN_POINT('Ctrl Pts',(-20.3387211617813,17.2146240223489,
16.1194185563871));
#135680=CARTESIAN_POINT('Ctrl Pts',(-20.4023916835425,17.2693333987818,
16.1235941205788));
#135681=CARTESIAN_POINT('Ctrl Pts',(-20.4692780519956,17.3268060157591,
16.1279805825913));
#135682=CARTESIAN_POINT('Ctrl Pts',(-20.5331149297309,17.3876731058187,
16.1323670446039));
#135683=CARTESIAN_POINT('Ctrl Pts',(-20.5935624370342,17.4515604464003,
16.1367535066164));
#135684=CARTESIAN_POINT('Ctrl Pts',(-20.6540099443375,17.5154477869819,
16.141139968629));
#135685=CARTESIAN_POINT('Ctrl Pts',(-20.7110677625942,17.5823548872471,
16.1455264306415));
#135686=CARTESIAN_POINT('Ctrl Pts',(-20.764447298501,17.6518708302357,16.149912892654));
#135687=CARTESIAN_POINT('Ctrl Pts',(-20.8154455601759,17.7182856499018,
16.1541036735168));
#135688=CARTESIAN_POINT('Ctrl Pts',(-20.8632791399794,17.7873320135741,
16.1582944543796));
#135689=CARTESIAN_POINT('Ctrl Pts',(-20.9076654294934,17.8586765917041,
16.1624852352424));
#135690=CARTESIAN_POINT('Ctrl Pts',(-20.9519891627481,17.929920619642,16.1666701097864));
#135691=CARTESIAN_POINT('Ctrl Pts',(-20.9928750133147,18.0034560458724,
16.1708549843304));
#135692=CARTESIAN_POINT('Ctrl Pts',(-21.0300812471761,18.0789174471947,
16.1750398588744));
#135693=CARTESIAN_POINT('Ctrl Pts',(-21.0672460755937,18.1542948703099,
16.1792200762261));
#135694=CARTESIAN_POINT('Ctrl Pts',(-21.1007392197539,18.2315936031769,
16.1834002935778));
#135695=CARTESIAN_POINT('Ctrl Pts',(-21.1303635397438,18.310421416318,16.1875805109295));
#135696=CARTESIAN_POINT('Ctrl Pts',(-21.1599640139561,18.3891857778594,
16.1917573634602));
#135697=CARTESIAN_POINT('Ctrl Pts',(-21.1857016914127,18.4694763469324,
16.1959342159909));
#135698=CARTESIAN_POINT('Ctrl Pts',(-21.2074270380287,18.550879793107,16.2001110685216));
#135699=CARTESIAN_POINT('Ctrl Pts',(-21.2291418983469,18.6322439478127,
16.2042859049869));
#135700=CARTESIAN_POINT('Ctrl Pts',(-21.2468481598048,18.7147194701813,
16.2084607414522));
#135701=CARTESIAN_POINT('Ctrl Pts',(-21.2604461548154,18.7978779516678,
16.2126355779175));
#135702=CARTESIAN_POINT('Ctrl Pts',(-21.2740449836496,18.881041532398,16.2168106703821));
#135703=CARTESIAN_POINT('Ctrl Pts',(-21.2835349604935,18.9648877054714,
16.2209857628466));
#135704=CARTESIAN_POINT('Ctrl Pts',(-21.2888677421723,19.0489789519614,
16.2251608553112));
#135705=CARTESIAN_POINT('Ctrl Pts',(-21.2923288662564,19.1035565169218,
16.227870606798));
#135706=CARTESIAN_POINT('Ctrl Pts',(-21.2940398771788,19.1582371483247,
16.2305803582847));
#135707=CARTESIAN_POINT('Ctrl Pts',(-21.293999294499,19.2129005695107,16.2332901097715));
#135708=CARTESIAN_POINT('',(-21.2939994369002,19.2093020392337,16.1667098902285));
#135709=CARTESIAN_POINT('Ctrl Pts',(-17.172599350298,17.1784745189047,15.8832287057516));
#135710=CARTESIAN_POINT('Ctrl Pts',(-17.2449841473338,17.1219689062814,
15.8878110822275));
#135711=CARTESIAN_POINT('Ctrl Pts',(-18.0187464993596,16.585086496338,15.9347853942639));
#135712=CARTESIAN_POINT('Ctrl Pts',(-20.0538051846353,16.4867742534768,
16.0241516418607));
#135713=CARTESIAN_POINT('Ctrl Pts',(-21.2452321357866,18.1548349245933,
16.1140629935438));
#135714=CARTESIAN_POINT('Ctrl Pts',(-21.2975540665632,19.1065231701483,
16.1615824096664));
#135715=CARTESIAN_POINT('Ctrl Pts',(-21.2967674646518,19.2093002032948,
16.1667098902285));
#135716=CARTESIAN_POINT('Ctrl Pts',(-21.2939994369002,19.2093020392337,
16.1667098902285));
#135717=CARTESIAN_POINT('Ctrl Pts',(-21.2940542005915,19.2918687402816,
16.1708335669039));
#135718=CARTESIAN_POINT('Ctrl Pts',(-21.2901102644712,19.37459277435,16.1749572435793));
#135719=CARTESIAN_POINT('Ctrl Pts',(-21.282148407848,19.4570481489096,16.1790809202548));
#135720=CARTESIAN_POINT('Ctrl Pts',(-21.2741500199359,19.5398818524497,
16.1832235175451));
#135721=CARTESIAN_POINT('Ctrl Pts',(-21.2620966823448,19.6224439445467,
16.1873661148355));
#135722=CARTESIAN_POINT('Ctrl Pts',(-21.2460219433305,19.7043008779902,
16.1915087121259));
#135723=CARTESIAN_POINT('Ctrl Pts',(-21.23005430851,19.7856124078128,16.1956237077524));
#135724=CARTESIAN_POINT('Ctrl Pts',(-21.2101187777554,19.8662276743518,
16.1997387033789));
#135725=CARTESIAN_POINT('Ctrl Pts',(-21.1863001253011,19.9457272251988,
16.2038536990054));
#135726=CARTESIAN_POINT('Ctrl Pts',(-21.1624916905597,20.0251926723701,
16.2079669293832));
#135727=CARTESIAN_POINT('Ctrl Pts',(-21.13480357533,20.1035429002386,16.2120801597611));
#135728=CARTESIAN_POINT('Ctrl Pts',(-21.1033710027996,20.1803714721883,
16.2161933901389));
#135729=CARTESIAN_POINT('Ctrl Pts',(-21.0719418753925,20.2571916234494,
16.2203061696919));
#135730=CARTESIAN_POINT('Ctrl Pts',(-21.0367692860285,20.3324900117991,
16.2244189492448));
#135731=CARTESIAN_POINT('Ctrl Pts',(-20.998036835518,20.405879578626,16.2285317287978));
#135732=CARTESIAN_POINT('Ctrl Pts',(-20.9588192445656,20.48018838104,16.2326960226666));
#135733=CARTESIAN_POINT('Ctrl Pts',(-20.9159522062818,20.5525397612551,
16.2368603165354));
#135734=CARTESIAN_POINT('Ctrl Pts',(-20.8696736494983,20.6225587351713,
16.2410246104042));
#135735=CARTESIAN_POINT('Ctrl Pts',(-20.8239074514183,20.6918025157111,
16.2451428005837));
#135736=CARTESIAN_POINT('Ctrl Pts',(-20.7748052350545,20.7587649302322,
16.2492609907631));
#135737=CARTESIAN_POINT('Ctrl Pts',(-20.7226388747276,20.823115202435,16.2533791809425));
#135738=CARTESIAN_POINT('Ctrl Pts',(-20.6695965003383,20.8885460894827,
16.257566526656));
#135739=CARTESIAN_POINT('Ctrl Pts',(-20.6133864683218,20.9512759179512,
16.2617538723695));
#135740=CARTESIAN_POINT('Ctrl Pts',(-20.5543334369044,21.0109961606869,
16.265941218083));
#135741=CARTESIAN_POINT('Ctrl Pts',(-20.495280405487,21.0707164034227,16.2701285637965));
#135742=CARTESIAN_POINT('Ctrl Pts',(-20.4333847973435,21.1274267716985,
16.2743159095101));
#135743=CARTESIAN_POINT('Ctrl Pts',(-20.369004471075,21.1808630357374,16.2785032552236));
#135744=CARTESIAN_POINT('Ctrl Pts',(-20.3046658312848,21.2342646996153,
16.2826878896166));
#135745=CARTESIAN_POINT('Ctrl Pts',(-20.2375884427955,21.2846103343966,
16.2868725240096));
#135746=CARTESIAN_POINT('Ctrl Pts',(-20.16809472922,21.3316065895454,16.2910571584027));
#135747=CARTESIAN_POINT('Ctrl Pts',(-20.0986999313442,21.378535951342,16.2952358364866));
#135748=CARTESIAN_POINT('Ctrl Pts',(-20.0268960178075,21.4221251476138,
16.2994145145706));
#135749=CARTESIAN_POINT('Ctrl Pts',(-19.9530388079931,21.4621206952553,
16.3035931926545));
#135750=CARTESIAN_POINT('Ctrl Pts',(-19.8778577607731,21.502833134344,16.30784677054));
#135751=CARTESIAN_POINT('Ctrl Pts',(-19.8005494535681,21.5398215173808,
16.3121003484254));
#135752=CARTESIAN_POINT('Ctrl Pts',(-19.7215205448428,21.5728643427414,
16.3163539263108));
#135753=CARTESIAN_POINT('Ctrl Pts',(-19.6440237657255,21.6052665684546,
16.3205250402888));
#135754=CARTESIAN_POINT('Ctrl Pts',(-19.56487294815,21.6338746703222,16.3246961542667));
#135755=CARTESIAN_POINT('Ctrl Pts',(-19.4844751811849,21.6585267112792,
16.3288672682447));
#135756=CARTESIAN_POINT('Ctrl Pts',(-19.404104392467,21.6831704800059,16.3330369825651));
#135757=CARTESIAN_POINT('Ctrl Pts',(-19.3224879248154,21.7038606894987,
16.3372066968854));
#135758=CARTESIAN_POINT('Ctrl Pts',(-19.2400494979671,21.7204847888774,
16.3413764112058));
#135759=CARTESIAN_POINT('Ctrl Pts',(-19.1576140046318,21.7371082966994,
16.3455459771499));
#135760=CARTESIAN_POINT('Ctrl Pts',(-19.0743570613777,21.7496658919856,
16.3497155430939));
#135761=CARTESIAN_POINT('Ctrl Pts',(-18.9907127437439,21.758096104822,16.3538851090379));
#135762=CARTESIAN_POINT('Ctrl Pts',(-18.9041275950885,21.7668227135419,
16.3582012717769));
#135763=CARTESIAN_POINT('Ctrl Pts',(-18.8171278498233,21.7711262492444,
16.3625174345158));
#135764=CARTESIAN_POINT('Ctrl Pts',(-18.7301989430817,21.7709971781169,
16.3668335972547));
#135765=CARTESIAN_POINT('Ctrl Pts',(-18.646101736334,21.7708723114677,16.3710091614464));
#135766=CARTESIAN_POINT('Ctrl Pts',(-18.5620712918898,21.7665992585964,
16.3751847256381));
#135767=CARTESIAN_POINT('Ctrl Pts',(-18.478543574057,21.7582224116563,16.3793602898297));
#135768=CARTESIAN_POINT('Ctrl Pts',(-18.3907970697647,21.7494224700914,
16.3837467518423));
#135769=CARTESIAN_POINT('Ctrl Pts',(-18.3036059893692,21.7360933624401,
16.3881332138548));
#135770=CARTESIAN_POINT('Ctrl Pts',(-18.2174632822105,21.7183471676605,
16.3925196758674));
#135771=CARTESIAN_POINT('Ctrl Pts',(-18.1313205750519,21.700600972881,16.3969061378799));
#135772=CARTESIAN_POINT('Ctrl Pts',(-18.0462267834431,21.6784379108237,
16.4012925998925));
#135773=CARTESIAN_POINT('Ctrl Pts',(-17.9626538344088,21.652029514944,16.405679061905));
#135774=CARTESIAN_POINT('Ctrl Pts',(-17.8829262006443,21.6268362085053,
16.409863696298));
#135775=CARTESIAN_POINT('Ctrl Pts',(-17.8042857709966,21.5976858772392,
16.4140483306911));
#135776=CARTESIAN_POINT('Ctrl Pts',(-17.7271537286291,21.5646908432984,
16.4182329650841));
#135777=CARTESIAN_POINT('Ctrl Pts',(-17.6501314741772,21.5317427737044,
16.4224116431681));
#135778=CARTESIAN_POINT('Ctrl Pts',(-17.5746137617241,21.4949610508433,
16.426590321252));
#135779=CARTESIAN_POINT('Ctrl Pts',(-17.5010063287307,21.4545076569091,
16.4307689993359));
#135780=CARTESIAN_POINT('Ctrl Pts',(-17.4260795354015,21.4133291649619,
16.4350225772214));
#135781=CARTESIAN_POINT('Ctrl Pts',(-17.353132638384,21.3683462231051,16.4392761551068));
#135782=CARTESIAN_POINT('Ctrl Pts',(-17.2825720020051,21.3197808721241,
16.4435297329923));
#135783=CARTESIAN_POINT('Ctrl Pts',(-17.2133793212501,21.2721570552393,
16.4477008469702));
#135784=CARTESIAN_POINT('Ctrl Pts',(-17.1464815985702,21.2210887664921,
16.4518719609482));
#135785=CARTESIAN_POINT('Ctrl Pts',(-17.0822353470014,21.1668306499041,
16.4560430749261));
#135786=CARTESIAN_POINT('Ctrl Pts',(-17.0180106538829,21.1125907401512,
16.4602127892465));
#135787=CARTESIAN_POINT('Ctrl Pts',(-16.956436016035,21.0551634249198,16.4643825035668));
#135788=CARTESIAN_POINT('Ctrl Pts',(-16.8978354223938,20.9948440637971,
16.4685522178872));
#135789=CARTESIAN_POINT('Ctrl Pts',(-16.8392369140131,20.9345268490961,
16.4727217838313));
#135790=CARTESIAN_POINT('Ctrl Pts',(-16.7836125593694,20.8713181236712,
16.4768913497753));
#135791=CARTESIAN_POINT('Ctrl Pts',(-16.7312490017889,20.8055496038582,
16.4810609157193));
#135792=CARTESIAN_POINT('Ctrl Pts',(-16.6770444061212,20.7374687440227,
16.4853770784583));
#135793=CARTESIAN_POINT('Ctrl Pts',(-16.6263345016133,20.6666451485156,
16.4896932411972));
#135794=CARTESIAN_POINT('Ctrl Pts',(-16.5793900615235,20.5934818309903,
16.4940094039361));
#135795=CARTESIAN_POINT('Ctrl Pts',(-16.5339748316321,20.5227018008381,
16.4981849681278));
#135796=CARTESIAN_POINT('Ctrl Pts',(-16.4920837070573,20.4497325726924,
16.5023605323195));
#135797=CARTESIAN_POINT('Ctrl Pts',(-16.4539153402347,20.3749647521738,
16.5065360965111));
#135798=CARTESIAN_POINT('Ctrl Pts',(-16.4138191799405,20.2964205867842,
16.5109225585237));
#135799=CARTESIAN_POINT('Ctrl Pts',(-16.3778319719898,20.215891893294,16.5153090205362));
#135800=CARTESIAN_POINT('Ctrl Pts',(-16.3461262998438,20.1338538303015,
16.5196954825488));
#135801=CARTESIAN_POINT('Ctrl Pts',(-16.3144206276978,20.051815767309,16.5240819445613));
#135802=CARTESIAN_POINT('Ctrl Pts',(-16.2869966000409,19.9682689098145,
16.5284684065739));
#135803=CARTESIAN_POINT('Ctrl Pts',(-16.2639654295305,19.8837029215676,
16.5328548685864));
#135804=CARTESIAN_POINT('Ctrl Pts',(-16.2419939573158,19.803027939797,16.5370395029795));
#135805=CARTESIAN_POINT('Ctrl Pts',(-16.223938199736,19.7211252621465,16.5412241373725));
#135806=CARTESIAN_POINT('Ctrl Pts',(-16.2099316900943,19.638409834854,16.5454087717656));
#135807=CARTESIAN_POINT('Ctrl Pts',(-16.1959451169855,19.5558121427342,
16.5495874498495));
#135808=CARTESIAN_POINT('Ctrl Pts',(-16.1859964196337,19.4724044485339,
16.5537661279335));
#135809=CARTESIAN_POINT('Ctrl Pts',(-16.18016901464,19.3886155911379,16.5579448060174));
#135810=CARTESIAN_POINT('Ctrl Pts',(-16.1742371575999,19.3033248786909,
16.5621983839028));
#135811=CARTESIAN_POINT('Ctrl Pts',(-16.1725759211884,19.2176396691378,
16.5664519617883));
#135812=CARTESIAN_POINT('Ctrl Pts',(-16.1752185615464,19.1320218370347,
16.5707055396737));
#135813=CARTESIAN_POINT('Ctrl Pts',(-16.1778099691644,19.0480638736762,
16.5748766536517));
#135814=CARTESIAN_POINT('Ctrl Pts',(-16.1845398497979,18.9641711795844,
16.5790477676296));
#135815=CARTESIAN_POINT('Ctrl Pts',(-16.1953870618677,18.8807813597822,
16.5832188816076));
#135816=CARTESIAN_POINT('Ctrl Pts',(-16.2062306340507,18.7974195222395,
16.587388595928));
#135817=CARTESIAN_POINT('Ctrl Pts',(-16.221188734479,18.7145606796676,16.5915583102483));
#135818=CARTESIAN_POINT('Ctrl Pts',(-16.2401883815475,18.6326371280316,
16.5957280245687));
#135819=CARTESIAN_POINT('Ctrl Pts',(-16.2591873525271,18.5507164915872,
16.5998975905127));
#135820=CARTESIAN_POINT('Ctrl Pts',(-16.2822274794425,18.4697315278526,
16.6040671564568));
#135821=CARTESIAN_POINT('Ctrl Pts',(-16.3091849959464,18.3901028102639,
16.6082367224008));
#135822=CARTESIAN_POINT('Ctrl Pts',(-16.337090305475,18.3076744451974,16.6125528851398));
#135823=CARTESIAN_POINT('Ctrl Pts',(-16.3691934316988,18.2266999715503,
16.6168690478787));
#135824=CARTESIAN_POINT('Ctrl Pts',(-16.4053020683426,18.1476252104292,
16.6211852106176));
#135825=CARTESIAN_POINT('Ctrl Pts',(-16.4402344699458,18.0711263013345,
16.6253607748093));
#135826=CARTESIAN_POINT('Ctrl Pts',(-16.4789151719814,17.9964056357569,
16.629536339001));
#135827=CARTESIAN_POINT('Ctrl Pts',(-16.5211232637327,17.9238416763712,
16.6337119031926));
#135828=CARTESIAN_POINT('Ctrl Pts',(-16.5654631858581,17.8476126839014,
16.6380983652052));
#135829=CARTESIAN_POINT('Ctrl Pts',(-16.613695880029,17.7737644826753,16.6424848272177));
#135830=CARTESIAN_POINT('Ctrl Pts',(-16.6655152292137,17.7026993824091,
16.6468712892303));
#135831=CARTESIAN_POINT('Ctrl Pts',(-16.7173345783984,17.6316342821429,
16.6512577512428));
#135832=CARTESIAN_POINT('Ctrl Pts',(-16.7727401579415,17.5633526854597,
16.6556442132553));
#135833=CARTESIAN_POINT('Ctrl Pts',(-16.8313804354227,17.4982131503051,
16.6600306752679));
#135834=CARTESIAN_POINT('Ctrl Pts',(-16.8873083679597,17.4360865764876,
16.6642142460498));
#135835=CARTESIAN_POINT('Ctrl Pts',(-16.9463864967517,17.3765866334562,
16.6683978168317));
#135836=CARTESIAN_POINT('Ctrl Pts',(-17.0083384129123,17.3200499512547,
16.6725813876136));
#135837=CARTESIAN_POINT('Ctrl Pts',(-17.0616528763228,17.2713957196927,
16.6761816770833));
#135838=CARTESIAN_POINT('Ctrl Pts',(-17.1170948413747,17.2249357543771,
16.6797819665529));
#135839=CARTESIAN_POINT('Ctrl Pts',(-17.174464231106,17.180864983421,16.6833822560226));
#135840=CARTESIAN_POINT('Origin',(-18.734,19.211,-1.76670989022852));
#135841=CARTESIAN_POINT('',(-17.1718943031603,17.177514077948,17.549894074293));
#135842=CARTESIAN_POINT('',(-17.1769969530062,17.1841723796816,17.4833253039094));
#135843=CARTESIAN_POINT('',(-17.174464231106,17.180864983421,-1.76670989022852));
#135844=CARTESIAN_POINT('',(-21.2942631180427,19.2118355653576,17.0332901097715));
#135845=CARTESIAN_POINT('Ctrl Pts',(-21.2979002849781,19.2118367523804,
17.0332901097715));
#135846=CARTESIAN_POINT('Ctrl Pts',(-21.2980949927007,19.2575742464713,
17.0355745863224));
#135847=CARTESIAN_POINT('Ctrl Pts',(-21.2762381497003,20.1518505805258,
17.0802509984337));
#135848=CARTESIAN_POINT('Ctrl Pts',(-20.2331956316243,21.8407726550478,
17.1673193461055));
#135849=CARTESIAN_POINT('Ctrl Pts',(-17.334263528554,21.895032333938,17.2944951527869));
#135850=CARTESIAN_POINT('Ctrl Pts',(-15.7195027605925,19.4868589362738,
17.4216709594684));
#135851=CARTESIAN_POINT('Ctrl Pts',(-16.4898974650082,17.7053824456698,
17.5068039333037));
#135852=CARTESIAN_POINT('Ctrl Pts',(-17.1663500536343,17.1817661252999,
17.5495449715786));
#135853=CARTESIAN_POINT('Ctrl Pts',(-17.1718943031603,17.177514077948,17.549894074293));
#135854=CARTESIAN_POINT('Ctrl Pts',(-17.174464231106,17.180864983421,16.749817664185));
#135855=CARTESIAN_POINT('Ctrl Pts',(-17.2411414928805,17.1296439691239,
16.7539938174381));
#135856=CARTESIAN_POINT('Ctrl Pts',(-17.3102911901789,17.0817524742227,
16.7581699706911));
#135857=CARTESIAN_POINT('Ctrl Pts',(-17.3815400031077,17.0374195536383,
16.7623461239442));
#135858=CARTESIAN_POINT('Ctrl Pts',(-17.452915189634,16.9930080000153,16.7665296844155));
#135859=CARTESIAN_POINT('Ctrl Pts',(-17.5263965273637,16.9521678546901,
16.7707132448868));
#135860=CARTESIAN_POINT('Ctrl Pts',(-17.6015860289866,16.9150821882625,
16.7748968053582));
#135861=CARTESIAN_POINT('Ctrl Pts',(-17.6668572814998,16.8828884930554,
16.7785285122592));
#135862=CARTESIAN_POINT('Ctrl Pts',(-17.7334152454288,16.853523409711,16.7821602191602));
#135863=CARTESIAN_POINT('Ctrl Pts',(-17.800989527137,16.8270764572814,16.7857919260613));
#135864=CARTESIAN_POINT('Ctrl Pts',(-17.8788519953999,16.7966029554973,
16.7899765604543));
#135865=CARTESIAN_POINT('Ctrl Pts',(-17.9583538968787,16.7698914102529,
16.7941611948473));
#135866=CARTESIAN_POINT('Ctrl Pts',(-18.0390969463691,16.7471189667408,
16.7983458292404));
#135867=CARTESIAN_POINT('Ctrl Pts',(-18.1197250681226,16.7243789369834,
16.8025245073243));
#135868=CARTESIAN_POINT('Ctrl Pts',(-18.20159038985,16.7055669958483,16.8067031854083));
#135869=CARTESIAN_POINT('Ctrl Pts',(-18.2842754534885,16.6908119450595,
16.8108818634922));
#135870=CARTESIAN_POINT('Ctrl Pts',(-18.3684425874681,16.6757924205895,
16.8151354413777));
#135871=CARTESIAN_POINT('Ctrl Pts',(-18.4534586911851,16.66497683224,16.8193890192631));
#135872=CARTESIAN_POINT('Ctrl Pts',(-18.5388680958069,16.6584476420716,
16.8236425971485));
#135873=CARTESIAN_POINT('Ctrl Pts',(-18.6226216724573,16.6520450329952,
16.8278137111265));
#135874=CARTESIAN_POINT('Ctrl Pts',(-18.7067529564691,16.6497641415373,
16.8319848251044));
#135875=CARTESIAN_POINT('Ctrl Pts',(-18.7908245916081,16.6516307484483,
16.8361559390824));
#135876=CARTESIAN_POINT('Ctrl Pts',(-18.8748680156981,16.6534967290012,
16.8403256534027));
#135877=CARTESIAN_POINT('Ctrl Pts',(-18.95885137113,16.659507433716,16.8444953677231));
#135878=CARTESIAN_POINT('Ctrl Pts',(-19.0423370360802,16.6696365328467,
16.8486650820435));
#135879=CARTESIAN_POINT('Ctrl Pts',(-19.1258197302521,16.6797652715406,
16.8528346479875));
#135880=CARTESIAN_POINT('Ctrl Pts',(-19.208804312573,16.6940120570168,16.8570042139316));
#135881=CARTESIAN_POINT('Ctrl Pts',(-19.2908593851773,16.7122988123547,
16.8611737798756));
#135882=CARTESIAN_POINT('Ctrl Pts',(-19.3757994129084,16.7312285074512,
16.8654899426145));
#135883=CARTESIAN_POINT('Ctrl Pts',(-19.4597428368619,16.7544874341396,
16.8698061053535));
#135884=CARTESIAN_POINT('Ctrl Pts',(-19.5422258260851,16.781932068869,16.8741222680924));
#135885=CARTESIAN_POINT('Ctrl Pts',(-19.62202194061,16.8084826975088,16.878297832284));
#135886=CARTESIAN_POINT('Ctrl Pts',(-19.7004508845914,16.838950308513,16.8824733964757));
#135887=CARTESIAN_POINT('Ctrl Pts',(-19.777112739986,16.8731557340835,16.8866489606674));
#135888=CARTESIAN_POINT('Ctrl Pts',(-19.8576466034504,16.9090887943838,
16.8910354226799));
#135889=CARTESIAN_POINT('Ctrl Pts',(-19.9362296554815,16.9491469214588,
16.8954218846925));
#135890=CARTESIAN_POINT('Ctrl Pts',(-20.0124291551048,16.9930687802869,
16.899808346705));
#135891=CARTESIAN_POINT('Ctrl Pts',(-20.088628654728,17.036990639115,16.9041948087175));
#135892=CARTESIAN_POINT('Ctrl Pts',(-20.1624441562133,17.0847758505362,
16.9085812707301));
#135893=CARTESIAN_POINT('Ctrl Pts',(-20.2334815623277,17.1361132454422,
16.9129677327426));
#135894=CARTESIAN_POINT('Ctrl Pts',(-20.3007008312569,17.1846913445463,
16.9171184300414));
#135895=CARTESIAN_POINT('Ctrl Pts',(-20.3656920487853,17.2366370916662,
16.9212691273401));
#135896=CARTESIAN_POINT('Ctrl Pts',(-20.4280939407347,17.2917173944502,
16.9254198246388));
#135897=CARTESIAN_POINT('Ctrl Pts',(-20.4904067758308,17.3467190893862,
16.9295645982704));
#135898=CARTESIAN_POINT('Ctrl Pts',(-20.5501372744549,17.4048461509353,
16.9337093719019));
#135899=CARTESIAN_POINT('Ctrl Pts',(-20.6069541187605,17.4658229691467,
16.9378541455335));
#135900=CARTESIAN_POINT('Ctrl Pts',(-20.6637057912848,17.5267298438773,
16.9419941649009));
#135901=CARTESIAN_POINT('Ctrl Pts',(-20.7175501324578,17.5904796396565,
16.9461341842684));
#135902=CARTESIAN_POINT('Ctrl Pts',(-20.7681909845745,17.6567583719782,
16.9502742036359));
#135903=CARTESIAN_POINT('Ctrl Pts',(-20.8188004163149,17.7229959813208,
16.9544116543072));
#135904=CARTESIAN_POINT('Ctrl Pts',(-20.8662100198437,17.7917590422704,
16.9585491049784));
#135905=CARTESIAN_POINT('Ctrl Pts',(-20.9101632231195,17.8626997269368,
16.9626865556497));
#135906=CARTESIAN_POINT('Ctrl Pts',(-20.9541028768145,17.9336185425138,
16.9668227308571));
#135907=CARTESIAN_POINT('Ctrl Pts',(-20.994587999437,18.0067132510727,16.9709589060645));
#135908=CARTESIAN_POINT('Ctrl Pts',(-21.031405596239,18.0816074524906,16.9750950812719));
#135909=CARTESIAN_POINT('Ctrl Pts',(-21.0682233367814,18.1565019463047,
16.9792312726275));
#135910=CARTESIAN_POINT('Ctrl Pts',(-21.1013733182381,18.2331955257884,
16.983367463983));
#135911=CARTESIAN_POINT('Ctrl Pts',(-21.1306893947115,18.3112889656799,
16.9875036553386));
#135912=CARTESIAN_POINT('Ctrl Pts',(-21.1600333335746,18.3894566266172,
16.9916437777855));
#135913=CARTESIAN_POINT('Ctrl Pts',(-21.1855359272154,18.4690263650883,
16.9957839002324));
#135914=CARTESIAN_POINT('Ctrl Pts',(-21.2070801670876,18.549581458411,16.9999240226793));
#135915=CARTESIAN_POINT('Ctrl Pts',(-21.2286351815299,18.6301768384412,
17.0040662156583));
#135916=CARTESIAN_POINT('Ctrl Pts',(-21.2462278030767,18.7117580962757,
17.0082084086373));
#135917=CARTESIAN_POINT('Ctrl Pts',(-21.2597921942375,18.7938983438909,
17.0123506016163));
#135918=CARTESIAN_POINT('Ctrl Pts',(-21.2733789861849,18.8761742412481,
17.016499635181));
#135919=CARTESIAN_POINT('Ctrl Pts',(-21.2829242114339,18.95901050629,17.0206486687457));
#135920=CARTESIAN_POINT('Ctrl Pts',(-21.2884139728529,19.0419755778182,
17.0247977023105));
#135921=CARTESIAN_POINT('Ctrl Pts',(-21.2921595270972,19.0985809841503,
17.0276285047975));
#135922=CARTESIAN_POINT('Ctrl Pts',(-21.2940183320645,19.1552463005707,
17.0304593072845));
#135923=CARTESIAN_POINT('Ctrl Pts',(-21.2939998636668,19.2118354794421,
17.0332901097715));
#135924=CARTESIAN_POINT('',(-21.2938494856171,19.209803254918,16.9667098397541));
#135925=CARTESIAN_POINT('Ctrl Pts',(-17.174464231106,17.180864983421,16.6833822560226));
#135926=CARTESIAN_POINT('Ctrl Pts',(-17.2433977216274,17.127910749705,16.6877082654362));
#135927=CARTESIAN_POINT('Ctrl Pts',(-17.3151147415225,17.0784073959019,
16.6920342748498));
#135928=CARTESIAN_POINT('Ctrl Pts',(-17.3892304768158,17.0326531659273,
16.6963602842634));
#135929=CARTESIAN_POINT('Ctrl Pts',(-17.4606968284318,16.9885344929579,
16.7005316536578));
#135930=CARTESIAN_POINT('Ctrl Pts',(-17.5343928910415,16.947901727856,16.7047030230523));
#135931=CARTESIAN_POINT('Ctrl Pts',(-17.6099425209296,16.9109793949301,
16.7088743924467));
#135932=CARTESIAN_POINT('Ctrl Pts',(-17.6854640454202,16.8740707975692,
16.7130442100401));
#135933=CARTESIAN_POINT('Ctrl Pts',(-17.7628373549223,16.8408700929972,
16.7172140276334));
#135934=CARTESIAN_POINT('Ctrl Pts',(-17.8416620090713,16.8115557080971,
16.7213838452268));
#135935=CARTESIAN_POINT('Ctrl Pts',(-17.920480984977,16.7822434348995,16.7255533624416));
#135936=CARTESIAN_POINT('Ctrl Pts',(-18.0007506663518,16.7568170847122,
16.7297228796563));
#135937=CARTESIAN_POINT('Ctrl Pts',(-18.0820522390349,16.735406310201,16.7338923968711));
#135938=CARTESIAN_POINT('Ctrl Pts',(-18.1633723431405,16.7139906554385,
16.7380628644621));
#135939=CARTESIAN_POINT('Ctrl Pts',(-18.245724360498,16.6965925096898,16.7422333320532));
#135940=CARTESIAN_POINT('Ctrl Pts',(-18.3286773196109,16.6832908543976,
16.7464037996442));
#135941=CARTESIAN_POINT('Ctrl Pts',(-18.4117243393771,16.6699741163114,
16.7505789961432));
#135942=CARTESIAN_POINT('Ctrl Pts',(-18.4953732056763,16.6607632092122,
16.7547541926422));
#135943=CARTESIAN_POINT('Ctrl Pts',(-18.5791864016643,16.6556853912345,
16.7589293891411));
#135944=CARTESIAN_POINT('Ctrl Pts',(-18.6630563522702,16.6506041347814,
16.7631074128999));
#135945=CARTESIAN_POINT('Ctrl Pts',(-18.7470903946914,16.6496615419162,
16.7672854366587));
#135946=CARTESIAN_POINT('Ctrl Pts',(-18.8308519536333,16.6528327460705,
16.7714634604175));
#135947=CARTESIAN_POINT('Ctrl Pts',(-18.9147465871835,16.6560089884159,
16.7756481219333));
#135948=CARTESIAN_POINT('Ctrl Pts',(-18.9983674167173,16.6633120266781,
16.7798327834491));
#135949=CARTESIAN_POINT('Ctrl Pts',(-19.0812844992108,16.6746653460933,
16.7840174449649));
#135950=CARTESIAN_POINT('Ctrl Pts',(-19.102347584139,16.6775493830598,16.7850804572931));
#135951=CARTESIAN_POINT('Ctrl Pts',(-19.1233653199158,16.6806945264327,
16.7861434696212));
#135952=CARTESIAN_POINT('Ctrl Pts',(-19.1443308019264,16.6840990060965,
16.7872064819493));
#135953=CARTESIAN_POINT('Ctrl Pts',(-19.2268631251808,16.6975010168866,
16.7913911163424));
#135954=CARTESIAN_POINT('Ctrl Pts',(-19.3088917529363,16.7149756618514,
16.7955757507354));
#135955=CARTESIAN_POINT('Ctrl Pts',(-19.389983688077,16.7364726914061,16.7997603851285));
#135956=CARTESIAN_POINT('Ctrl Pts',(-19.4709601988852,16.7579391226001,
16.8039390632124));
#135957=CARTESIAN_POINT('Ctrl Pts',(-19.5510022244943,16.7834164491322,
16.8081177412964));
#135958=CARTESIAN_POINT('Ctrl Pts',(-19.6296848716229,16.8128030500508,
16.8122964193803));
#135959=CARTESIAN_POINT('Ctrl Pts',(-19.709777848653,16.842716384671,16.8165499972657));
#135960=CARTESIAN_POINT('Ctrl Pts',(-19.7884617582361,16.8766804423688,
16.8208035751512));
#135961=CARTESIAN_POINT('Ctrl Pts',(-19.8653024038484,16.9145342652139,
16.8250571530366));
#135962=CARTESIAN_POINT('Ctrl Pts',(-19.9406533436033,16.9516542178375,
16.8292282670146));
#135963=CARTESIAN_POINT('Ctrl Pts',(-20.0142314204538,16.9925142474789,
16.8333993809925));
#135964=CARTESIAN_POINT('Ctrl Pts',(-20.0856470518142,17.0369139282627,
16.8375704949705));
#135965=CARTESIAN_POINT('Ctrl Pts',(-20.1570387189699,17.081298710305,16.8417402092909));
#135966=CARTESIAN_POINT('Ctrl Pts',(-20.2262689913883,17.1292205418819,
16.8459099236112));
#135967=CARTESIAN_POINT('Ctrl Pts',(-20.2929745824341,17.1804340071486,
16.8500796379316));
#135968=CARTESIAN_POINT('Ctrl Pts',(-20.3596777998086,17.2316456500204,
16.8542492038757));
#135969=CARTESIAN_POINT('Ctrl Pts',(-20.4238561500592,17.2861484128723,
16.8584187698197));
#135970=CARTESIAN_POINT('Ctrl Pts',(-20.4851780435305,17.3436555058435,
16.8625883357638));
#135971=CARTESIAN_POINT('Ctrl Pts',(-20.5486559391275,17.4031844772608,
16.8669044985027));
#135972=CARTESIAN_POINT('Ctrl Pts',(-20.6090723898817,17.4659326132811,
16.8712206612416));
#135973=CARTESIAN_POINT('Ctrl Pts',(-20.6661012016728,17.5315402813719,
16.8755368239805));
#135974=CARTESIAN_POINT('Ctrl Pts',(-20.7212723059183,17.5950107865754,
16.8797123881722));
#135975=CARTESIAN_POINT('Ctrl Pts',(-20.7732728325614,17.6611569867926,
16.8838879523639));
#135976=CARTESIAN_POINT('Ctrl Pts',(-20.8218497444836,17.7296211003056,
16.8880635165556));
#135977=CARTESIAN_POINT('Ctrl Pts',(-20.8728801607463,17.8015431734342,
16.8924499785681));
#135978=CARTESIAN_POINT('Ctrl Pts',(-20.9201317067405,17.8760229761492,
16.8968364405806));
#135979=CARTESIAN_POINT('Ctrl Pts',(-20.9633649162028,17.9526152931618,
16.9012229025932));
#135980=CARTESIAN_POINT('Ctrl Pts',(-21.006598125665,18.0292076101744,16.9056093646057));
#135981=CARTESIAN_POINT('Ctrl Pts',(-21.0458128079223,18.1079118882384,
16.9099958266183));
#135982=CARTESIAN_POINT('Ctrl Pts',(-21.0808281256647,18.1882596866315,
16.9143822886308));
#135983=CARTESIAN_POINT('Ctrl Pts',(-21.117652895614,18.2727595393394,16.9189954255354));
#135984=CARTESIAN_POINT('Ctrl Pts',(-21.1499518315869,18.3593459986734,
16.92360856244));
#135985=CARTESIAN_POINT('Ctrl Pts',(-21.1775079602936,18.4475415217695,
16.9282216993445));
#135986=CARTESIAN_POINT('Ctrl Pts',(-21.204985218715,18.5354846144123,16.9328216326737));
#135987=CARTESIAN_POINT('Ctrl Pts',(-21.2277466226995,18.6250273148932,
16.9374215660029));
#135988=CARTESIAN_POINT('Ctrl Pts',(-21.2456232056939,18.7156729639725,
16.942021499332));
#135989=CARTESIAN_POINT('Ctrl Pts',(-21.263411741867,18.8058721596512,16.946598776793));
#135990=CARTESIAN_POINT('Ctrl Pts',(-21.2763633328307,18.897163189666,16.951176054254));
#135991=CARTESIAN_POINT('Ctrl Pts',(-21.2843593339857,18.9890376888929,
16.955753331715));
#135992=CARTESIAN_POINT('Ctrl Pts',(-21.2907392715853,19.0623435277363,
16.9594055003441));
#135993=CARTESIAN_POINT('Ctrl Pts',(-21.2939652250926,19.136020399912,16.9630576689733));
#135994=CARTESIAN_POINT('Ctrl Pts',(-21.2939997202205,19.2098031412724,
16.9667098376024));
#135995=CARTESIAN_POINT('Ctrl Pts',(-21.2903253208441,19.2098059207881,
16.9667098902285));
#135996=CARTESIAN_POINT('Ctrl Pts',(-21.2882103114883,19.7131225250721,
16.9916592919231));
#135997=CARTESIAN_POINT('Ctrl Pts',(-20.9008595718265,21.0746360886269,
17.0590006291781));
#135998=CARTESIAN_POINT('Ctrl Pts',(-18.685881688709,22.2377104703834,17.1687339019936));
#135999=CARTESIAN_POINT('Ctrl Pts',(-16.1629699524582,20.8088410866063,
17.2959097086751));
#136000=CARTESIAN_POINT('Ctrl Pts',(-16.0276177675682,18.4219199634484,
17.4007735093137));
#136001=CARTESIAN_POINT('Ctrl Pts',(-16.8552506581505,17.430604537599,17.4632453743918));
#136002=CARTESIAN_POINT('Ctrl Pts',(-17.1769969530062,17.1841723796816,
17.4833253039094));
#136003=CARTESIAN_POINT('Origin',(-18.734,19.211,-1.76670989022852));
#136004=CARTESIAN_POINT('',(-17.174464231106,17.180864983421,18.3499540467144));
#136005=CARTESIAN_POINT('',(-17.174464231106,17.180864983421,18.2832318539276));
#136006=CARTESIAN_POINT('',(-17.174464231106,17.180864983421,-1.76670989022852));
#136007=CARTESIAN_POINT('',(-21.2939989159607,19.2086440968075,17.8332901097715));
#136008=CARTESIAN_POINT('Ctrl Pts',(-21.2939989159607,19.2086440968075,
17.8332901097715));
#136009=CARTESIAN_POINT('Ctrl Pts',(-21.2940751741219,19.2915086264566,
17.837412174938));
#136010=CARTESIAN_POINT('Ctrl Pts',(-21.290123839502,19.3744847533444,17.8415342401044));
#136011=CARTESIAN_POINT('Ctrl Pts',(-21.2821391268744,19.457144246514,17.8456563052709));
#136012=CARTESIAN_POINT('Ctrl Pts',(-21.2741597741335,19.5397482529613,
17.8497756034244));
#136013=CARTESIAN_POINT('Ctrl Pts',(-21.262152459652,19.6220355783688,17.8538949015779));
#136014=CARTESIAN_POINT('Ctrl Pts',(-21.2461634417033,19.7035797825424,
17.8580141997315));
#136015=CARTESIAN_POINT('Ctrl Pts',(-21.2301800733889,19.7850951735057,
17.862132042353));
#136016=CARTESIAN_POINT('Ctrl Pts',(-21.2102178848107,19.8658675009386,
17.8662498849744));
#136017=CARTESIAN_POINT('Ctrl Pts',(-21.1863745538874,19.9454787590158,
17.8703677275959));
#136018=CARTESIAN_POINT('Ctrl Pts',(-21.1625320679642,20.0250871956953,
17.8744854242823));
#136019=CARTESIAN_POINT('Ctrl Pts',(-21.1348088500427,20.1035341923717,
17.8786031209688));
#136020=CARTESIAN_POINT('Ctrl Pts',(-21.1033525053491,20.1804166830605,
17.8827208176552));
#136021=CARTESIAN_POINT('Ctrl Pts',(-21.0718661219911,20.2573725912857,
17.8868424464612));
#136022=CARTESIAN_POINT('Ctrl Pts',(-21.0366396717685,20.3327605713694,
17.8909640752672));
#136023=CARTESIAN_POINT('Ctrl Pts',(-20.9978687619912,20.4061979871471,
17.8950857040732));
#136024=CARTESIAN_POINT('Ctrl Pts',(-20.9590794967267,20.4796701707327,
17.8992092842006));
#136025=CARTESIAN_POINT('Ctrl Pts',(-20.9167426732501,20.551189545137,17.9033328643279));
#136026=CARTESIAN_POINT('Ctrl Pts',(-20.8710983794445,20.6204007650685,
17.9074564444553));
#136027=CARTESIAN_POINT('Ctrl Pts',(-20.8253741239694,20.6897332322411,
17.9115872484506));
#136028=CARTESIAN_POINT('Ctrl Pts',(-20.7763311058832,20.7567490876314,
17.9157180524459));
#136029=CARTESIAN_POINT('Ctrl Pts',(-20.7242507920073,20.8211247730888,
17.9198488564413));
#136030=CARTESIAN_POINT('Ctrl Pts',(-20.6800170723896,20.8758014024867,
17.9233572996922));
#136031=CARTESIAN_POINT('Ctrl Pts',(-20.6335931281538,20.9285739549631,
17.9268657429431));
#136032=CARTESIAN_POINT('Ctrl Pts',(-20.5851713910723,20.9792659530951,
17.9303741861941));
#136033=CARTESIAN_POINT('Ctrl Pts',(-20.5274172101246,21.0397279482481,
17.9345588205871));
#136034=CARTESIAN_POINT('Ctrl Pts',(-20.4665902688467,21.0974699797564,
17.9387434549801));
#136035=CARTESIAN_POINT('Ctrl Pts',(-20.4029770272298,21.1521634868241,
17.9429280893731));
#136036=CARTESIAN_POINT('Ctrl Pts',(-20.3394543311886,21.2067791444542,
17.947106767457));
#136037=CARTESIAN_POINT('Ctrl Pts',(-20.2731535582846,21.2583545993042,
17.9512854455408));
#136038=CARTESIAN_POINT('Ctrl Pts',(-20.2043989371767,21.3065970427421,
17.9554641236247));
#136039=CARTESIAN_POINT('Ctrl Pts',(-20.1344119388974,21.3557041973082,
17.9597177015102));
#136040=CARTESIAN_POINT('Ctrl Pts',(-20.0618825897101,21.4013573280785,
17.9639712793956));
#136041=CARTESIAN_POINT('Ctrl Pts',(-19.9871893049689,21.4432895345164,
17.9682248572811));
#136042=CARTESIAN_POINT('Ctrl Pts',(-19.9139440953056,21.4844088033079,
17.972395971259));
#136043=CARTESIAN_POINT('Ctrl Pts',(-19.8386185251855,21.5219498994727,
17.9765670852369));
#136044=CARTESIAN_POINT('Ctrl Pts',(-19.7615983036838,21.555705040355,17.9807381992148));
#136045=CARTESIAN_POINT('Ctrl Pts',(-19.6846039270611,21.5894488543738,
17.9849079135351));
#136046=CARTESIAN_POINT('Ctrl Pts',(-19.6059164494116,21.619409051666,17.9890776278554));
#136047=CARTESIAN_POINT('Ctrl Pts',(-19.5259437923521,21.6454249895519,
17.9932473421757));
#136048=CARTESIAN_POINT('Ctrl Pts',(-19.4459739810632,21.6714400016791,
17.9974169081197));
#136049=CARTESIAN_POINT('Ctrl Pts',(-19.3647195190224,21.6935108919569,
18.0015864740637));
#136050=CARTESIAN_POINT('Ctrl Pts',(-19.2826045027058,21.7115265644681,
18.0057560400077));
#136051=CARTESIAN_POINT('Ctrl Pts',(-19.1976024237129,21.7301756458007,
18.0100722027467));
#136052=CARTESIAN_POINT('Ctrl Pts',(-19.1116786655147,21.7444789277004,
18.0143883654857));
#136053=CARTESIAN_POINT('Ctrl Pts',(-19.0253143284886,21.7543709839536,
18.0187045282247));
#136054=CARTESIAN_POINT('Ctrl Pts',(-18.9417633006594,21.7639408075146,
18.0228800924163));
#136055=CARTESIAN_POINT('Ctrl Pts',(-18.857800430025,21.7693824000208,18.0270556566079));
#136056=CARTESIAN_POINT('Ctrl Pts',(-18.7738638919265,21.7706896042529,
18.0312312207996));
#136057=CARTESIAN_POINT('Ctrl Pts',(-18.6856879188254,21.7720628322632,
18.0356176828122));
#136058=CARTESIAN_POINT('Ctrl Pts',(-18.5975415917828,21.7688730610124,
18.0400041448249));
#136059=CARTESIAN_POINT('Ctrl Pts',(-18.5099274935594,21.7611748002553,
18.0443906068375));
#136060=CARTESIAN_POINT('Ctrl Pts',(-18.4223133953359,21.7534765394983,
18.0487770688502));
#136061=CARTESIAN_POINT('Ctrl Pts',(-18.3352320899719,21.7412699451077,
18.0531635308629));
#136062=CARTESIAN_POINT('Ctrl Pts',(-18.2491721313432,21.7246710082613,
18.0575499928755));
#136063=CARTESIAN_POINT('Ctrl Pts',(-18.1670719189868,21.7088358131057,
18.0617346272685));
#136064=CARTESIAN_POINT('Ctrl Pts',(-18.0855955387247,21.6889446480546,
18.0659192616614));
#136065=CARTESIAN_POINT('Ctrl Pts',(-18.0051743135506,21.6650605369003,
18.0701038960543));
#136066=CARTESIAN_POINT('Ctrl Pts',(-17.9248675580363,21.641210421822,18.0742825741382));
#136067=CARTESIAN_POINT('Ctrl Pts',(-17.8456134116221,21.6133787796396,
18.078461252222));
#136068=CARTESIAN_POINT('Ctrl Pts',(-17.767833578853,21.5816797435858,18.0826399303058));
#136069=CARTESIAN_POINT('Ctrl Pts',(-17.6886595984782,21.5494125250913,
18.0868935081913));
#136070=CARTESIAN_POINT('Ctrl Pts',(-17.6110137791776,21.5131379942491,
18.0911470860768));
#136071=CARTESIAN_POINT('Ctrl Pts',(-17.5353253711183,21.473029870288,18.0954006639622));
#136072=CARTESIAN_POINT('Ctrl Pts',(-17.4611043305455,21.4336993205758,
18.0995717779401));
#136073=CARTESIAN_POINT('Ctrl Pts',(-17.3887659072355,21.3906827199664,
18.1037428919179));
#136074=CARTESIAN_POINT('Ctrl Pts',(-17.3186935905263,21.3441919199413,
18.1079140058957));
#136075=CARTESIAN_POINT('Ctrl Pts',(-17.2486447872598,21.2977167203531,
18.112083720216));
#136076=CARTESIAN_POINT('Ctrl Pts',(-17.1808609634163,21.2477698907684,
18.1162534345363));
#136077=CARTESIAN_POINT('Ctrl Pts',(-17.1156979943015,21.1946074758762,
18.1204231488565));
#136078=CARTESIAN_POINT('Ctrl Pts',(-17.0505373439648,21.1414469527309,
18.1245927148005));
#136079=CARTESIAN_POINT('Ctrl Pts',(-16.9879977188458,21.0850713632529,
18.1287622807444));
#136080=CARTESIAN_POINT('Ctrl Pts',(-16.9284020884085,21.0257771713509,
18.1329318466883));
#136081=CARTESIAN_POINT('Ctrl Pts',(-16.8667111491206,20.9643982688052,
18.1372480094274));
#136082=CARTESIAN_POINT('Ctrl Pts',(-16.8081754519453,20.8998920810984,
18.1415641721664));
#136083=CARTESIAN_POINT('Ctrl Pts',(-16.7531104204839,20.8326277235434,
18.1458803349055));
#136084=CARTESIAN_POINT('Ctrl Pts',(-16.6998391266337,20.7675544953646,
18.1500558990971));
#136085=CARTESIAN_POINT('Ctrl Pts',(-16.6498160990945,20.6999004393904,
18.1542314632886));
#136086=CARTESIAN_POINT('Ctrl Pts',(-16.6032836911149,20.6300306589538,
18.1584070274802));
#136087=CARTESIAN_POINT('Ctrl Pts',(-16.5544010418242,20.5566319220006,
18.162793489493));
#136088=CARTESIAN_POINT('Ctrl Pts',(-16.5093711996513,20.4807882477349,
18.1671799515058));
#136089=CARTESIAN_POINT('Ctrl Pts',(-16.4684203690348,20.4029517338195,
18.1715664135186));
#136090=CARTESIAN_POINT('Ctrl Pts',(-16.4274695384182,20.3251152199041,
18.1759528755314));
#136091=CARTESIAN_POINT('Ctrl Pts',(-16.3905978935981,20.2452864249786,
18.1803393375442));
#136092=CARTESIAN_POINT('Ctrl Pts',(-16.3579723492966,20.1639389293617,
18.184725799557));
#136093=CARTESIAN_POINT('Ctrl Pts',(-16.3268479546498,20.0863343526005,
18.1889104339505));
#136094=CARTESIAN_POINT('Ctrl Pts',(-16.2994716572956,20.00705890033,18.193095068344));
#136095=CARTESIAN_POINT('Ctrl Pts',(-16.2760239311543,19.926509360513,18.1972797027374));
#136096=CARTESIAN_POINT('Ctrl Pts',(-16.252609579949,19.8460744729961,18.2014583808218));
#136097=CARTESIAN_POINT('Ctrl Pts',(-16.2331128202905,19.7643695380473,
18.2056370589062));
#136098=CARTESIAN_POINT('Ctrl Pts',(-16.2176659448641,19.6818109206073,
18.2098157369906));
#136099=CARTESIAN_POINT('Ctrl Pts',(-16.2019421952991,19.5977724992944,
18.2140693148759));
#136100=CARTESIAN_POINT('Ctrl Pts',(-16.190415125853,19.5128499374393,18.2183228927612));
#136101=CARTESIAN_POINT('Ctrl Pts',(-16.1831710111199,19.4274981974259,
18.2225764706466));
#136102=CARTESIAN_POINT('Ctrl Pts',(-16.1760673376856,19.343801167432,18.2267475846249));
#136103=CARTESIAN_POINT('Ctrl Pts',(-16.1730820747445,19.2596919311863,
18.2309186986033));
#136104=CARTESIAN_POINT('Ctrl Pts',(-16.1742446642318,19.1756076137227,
18.2350898125817));
#136105=CARTESIAN_POINT('Ctrl Pts',(-16.1754068636011,19.0915515115639,
18.2392595269025));
#136106=CARTESIAN_POINT('Ctrl Pts',(-16.180714144804,19.0075207711868,18.2434292412233));
#136107=CARTESIAN_POINT('Ctrl Pts',(-16.1901438433302,18.9239532195391,
18.2475989555441));
#136108=CARTESIAN_POINT('Ctrl Pts',(-16.1995732063072,18.8403886415836,
18.2517685214886));
#136109=CARTESIAN_POINT('Ctrl Pts',(-16.2131246425144,18.757287676623,18.2559380874331));
#136110=CARTESIAN_POINT('Ctrl Pts',(-16.2307236899663,18.6750823611562,
18.2601076533775));
#136111=CARTESIAN_POINT('Ctrl Pts',(-16.2489414982117,18.5899868082277,
18.2644238161159));
#136112=CARTESIAN_POINT('Ctrl Pts',(-16.2714967310844,18.5058515744437,
18.2687399788543));
#136113=CARTESIAN_POINT('Ctrl Pts',(-16.2982497538327,18.4231416762539,
18.2730561415928));
#136114=CARTESIAN_POINT('Ctrl Pts',(-16.3241312996846,18.3431260442806,
18.2772317057848));
#136115=CARTESIAN_POINT('Ctrl Pts',(-16.3539411382345,18.2644447370894,
18.281407269977));
#136116=CARTESIAN_POINT('Ctrl Pts',(-16.3875034565749,18.1874991589187,
18.285582834169));
#136117=CARTESIAN_POINT('Ctrl Pts',(-16.4227609278164,18.1066672425416,
18.2899692961806));
#136118=CARTESIAN_POINT('Ctrl Pts',(-16.4621596558343,18.0277515290341,
18.2943557581922));
#136119=CARTESIAN_POINT('Ctrl Pts',(-16.5054419382126,17.9511869324212,
18.2987422202037));
#136120=CARTESIAN_POINT('Ctrl Pts',(-16.5487242205909,17.8746223358083,
18.3031286822153));
#136121=CARTESIAN_POINT('Ctrl Pts',(-16.5958896819152,17.8004093049793,
18.3075151442268));
#136122=CARTESIAN_POINT('Ctrl Pts',(-16.6466304638567,17.7289445288449,
18.3119016062384));
#136123=CARTESIAN_POINT('Ctrl Pts',(-16.6950307331482,17.6607761980189,
18.3160857345564));
#136124=CARTESIAN_POINT('Ctrl Pts',(-16.7468638869145,17.5948544666272,
18.3202698628743));
#136125=CARTESIAN_POINT('Ctrl Pts',(-16.8018940647046,17.5315457270898,
18.3244539911923));
#136126=CARTESIAN_POINT('Ctrl Pts',(-16.8577907167831,17.467240163678,18.3287040004459));
#136127=CARTESIAN_POINT('Ctrl Pts',(-16.9169857342869,17.4056310236911,
18.3329540096996));
#136128=CARTESIAN_POINT('Ctrl Pts',(-16.9791857557851,17.3470721665525,
18.3372040189533));
#136129=CARTESIAN_POINT('Ctrl Pts',(-17.0413857772832,17.2885133094139,
18.341454028207));
#136130=CARTESIAN_POINT('Ctrl Pts',(-17.1065904878517,17.2330051265689,
18.3457040374607));
#136131=CARTESIAN_POINT('Ctrl Pts',(-17.174464231106,17.180864983421,18.3499540467144));
#136132=CARTESIAN_POINT('Ctrl Pts',(-17.1718943031603,17.177514077948,17.549894074293));
#136133=CARTESIAN_POINT('Ctrl Pts',(-17.8395945142173,16.6654352292226,
17.5919369071391));
#136134=CARTESIAN_POINT('Ctrl Pts',(-19.7363287875448,16.3587000094287,
17.6763716755457));
#136135=CARTESIAN_POINT('Ctrl Pts',(-21.1817726888933,17.9552739588088,
17.7708370080137));
#136136=CARTESIAN_POINT('Ctrl Pts',(-21.2957665006941,19.0070072439541,
17.8232595076358));
#136137=CARTESIAN_POINT('Ctrl Pts',(-21.2939118038754,19.2086434116094,
17.8332900716974));
#136138=CARTESIAN_POINT('',(-21.2939990418858,19.2132148462352,17.7667099127482));
#136139=CARTESIAN_POINT('Ctrl Pts',(-17.1769969530062,17.1841723796816,
17.4833253039094));
#136140=CARTESIAN_POINT('Ctrl Pts',(-17.5345084307618,16.9103469266704,
17.5056373099522));
#136141=CARTESIAN_POINT('Ctrl Pts',(-18.7708037278702,16.3747766682838,
17.5703412515555));
#136142=CARTESIAN_POINT('Ctrl Pts',(-20.7784813956588,17.1540155580924,
17.6648027803286));
#136143=CARTESIAN_POINT('Ctrl Pts',(-21.2874613721703,18.6141143669069,
17.7369523030588));
#136144=CARTESIAN_POINT('Ctrl Pts',(-21.2923873719166,19.2132129984815,
17.7667098902285));
#136145=CARTESIAN_POINT('Ctrl Pts',(-21.2939990418858,19.2132148462352,
17.7667099127482));
#136146=CARTESIAN_POINT('Ctrl Pts',(-21.2939112972768,19.3146332252686,
17.7717442924635));
#136147=CARTESIAN_POINT('Ctrl Pts',(-21.2877929815477,19.415787678657,17.7767786721789));
#136148=CARTESIAN_POINT('Ctrl Pts',(-21.2757605528227,19.5160463769891,
17.7818130518942));
#136149=CARTESIAN_POINT('Ctrl Pts',(-21.2635573150943,19.6177283198494,
17.7869188982603));
#136150=CARTESIAN_POINT('Ctrl Pts',(-21.245270932932,19.7184889031551,17.7920247446265));
#136151=CARTESIAN_POINT('Ctrl Pts',(-21.2210717431444,19.8176911442014,
17.7971305909926));
#136152=CARTESIAN_POINT('Ctrl Pts',(-21.2092508709255,19.866149668042,17.7996247057953));
#136153=CARTESIAN_POINT('Ctrl Pts',(-21.1960198419246,19.9142366801055,
17.8021188205981));
#136154=CARTESIAN_POINT('Ctrl Pts',(-21.1814026084241,19.9618797988219,
17.8046129354008));
#136155=CARTESIAN_POINT('Ctrl Pts',(-21.1568777637899,20.0418155872439,
17.8087975697939));
#136156=CARTESIAN_POINT('Ctrl Pts',(-21.1283869296254,20.1206973427815,
17.8129822041869));
#136157=CARTESIAN_POINT('Ctrl Pts',(-21.0960388974778,20.1981029565359,
17.81716683858));
#136158=CARTESIAN_POINT('Ctrl Pts',(-21.0637369087501,20.27539839298,17.8213455166639));
#136159=CARTESIAN_POINT('Ctrl Pts',(-21.0275888032569,20.3512214402681,
17.8255241947478));
#136160=CARTESIAN_POINT('Ctrl Pts',(-20.987753160177,20.4251650188472,17.8297028728318));
#136161=CARTESIAN_POINT('Ctrl Pts',(-20.9472034918241,20.5004339829302,
17.8339564507172));
#136162=CARTESIAN_POINT('Ctrl Pts',(-20.9028329287838,20.5737549756817,
17.8382100286026));
#136163=CARTESIAN_POINT('Ctrl Pts',(-20.8548601014716,20.6447197878197,
17.8424636064881));
#136164=CARTESIAN_POINT('Ctrl Pts',(-20.8078173210282,20.7143088085979,
17.846634720466));
#136165=CARTESIAN_POINT('Ctrl Pts',(-20.7573109732373,20.7816317931437,
17.850805834444));
#136166=CARTESIAN_POINT('Ctrl Pts',(-20.7035927080245,20.8463301087232,
17.8549769484219));
#136167=CARTESIAN_POINT('Ctrl Pts',(-20.6498924684944,20.9110067141581,
17.8591466627423));
#136168=CARTESIAN_POINT('Ctrl Pts',(-20.592982745675,20.9730600461347,17.8633163770627));
#136169=CARTESIAN_POINT('Ctrl Pts',(-20.533156175962,21.032163653958,17.867486091383));
#136170=CARTESIAN_POINT('Ctrl Pts',(-20.4733317351351,21.0912651586214,
17.8716556573271));
#136171=CARTESIAN_POINT('Ctrl Pts',(-20.4105909816463,21.147416825124,17.8758252232711));
#136172=CARTESIAN_POINT('Ctrl Pts',(-20.3452632200691,21.2003292426475,
17.8799947892152));
#136173=CARTESIAN_POINT('Ctrl Pts',(-20.2776386149852,21.2551019954968,
17.8843109519541));
#136174=CARTESIAN_POINT('Ctrl Pts',(-20.2072421084912,21.3064031452814,
17.888627114693));
#136175=CARTESIAN_POINT('Ctrl Pts',(-20.134474432863,21.3539585537049,17.8929432774319));
#136176=CARTESIAN_POINT('Ctrl Pts',(-20.0640771566148,21.3999648497008,
17.8971188416236));
#136177=CARTESIAN_POINT('Ctrl Pts',(-19.9914612509379,21.4424654946023,
17.9012944058153));
#136178=CARTESIAN_POINT('Ctrl Pts',(-19.9170156443953,21.4812585723032,
17.905469970007));
#136179=CARTESIAN_POINT('Ctrl Pts',(-19.8388099672435,21.522010996137,17.9098564320195));
#136180=CARTESIAN_POINT('Ctrl Pts',(-19.7585854263164,21.558671228602,17.9142428940321));
#136181=CARTESIAN_POINT('Ctrl Pts',(-19.6768157184724,21.5910627136698,
17.9186293560446));
#136182=CARTESIAN_POINT('Ctrl Pts',(-19.5950460106283,21.6234541987376,
17.9230158180572));
#136183=CARTESIAN_POINT('Ctrl Pts',(-19.5117317099373,21.6515768229132,
17.9274022800697));
#136184=CARTESIAN_POINT('Ctrl Pts',(-19.427361531773,21.6753152773656,17.9317887420823));
#136185=CARTESIAN_POINT('Ctrl Pts',(-19.3468733505733,21.6979614903395,
17.9359733764753));
#136186=CARTESIAN_POINT('Ctrl Pts',(-19.2651247293132,21.716702405741,17.9401580108683));
#136187=CARTESIAN_POINT('Ctrl Pts',(-19.1825294815775,21.7314010205036,
17.9443426452614));
#136188=CARTESIAN_POINT('Ctrl Pts',(-19.1000517979537,21.7460787136074,
17.9485213233453));
#136189=CARTESIAN_POINT('Ctrl Pts',(-19.0167303305417,21.7567254548486,
17.9527000014292));
#136190=CARTESIAN_POINT('Ctrl Pts',(-18.9329932047255,21.7632542397796,
17.9568786795131));
#136191=CARTESIAN_POINT('Ctrl Pts',(-18.8477551511093,21.7699000484884,
17.9611322573986));
#136192=CARTESIAN_POINT('Ctrl Pts',(-18.7620868552843,21.7722786894991,
17.965385835284));
#136193=CARTESIAN_POINT('Ctrl Pts',(-18.6764498971537,21.7703530404503,
17.9696394131695));
#136194=CARTESIAN_POINT('Ctrl Pts',(-18.5924731785638,21.768464723866,17.9738105271474));
#136195=CARTESIAN_POINT('Ctrl Pts',(-18.5085270745239,21.76243753283,17.9779816411253));
#136196=CARTESIAN_POINT('Ctrl Pts',(-18.42504935174,21.7522889440085,17.9821527551033));
#136197=CARTESIAN_POINT('Ctrl Pts',(-18.3415996407122,21.742143760644,17.9863224694236));
#136198=CARTESIAN_POINT('Ctrl Pts',(-18.258618455089,21.7278799815763,17.990492183744));
#136199=CARTESIAN_POINT('Ctrl Pts',(-18.1765386867735,21.7095669661339,
17.9946618980643));
#136200=CARTESIAN_POINT('Ctrl Pts',(-18.0944618392085,21.6912546023473,
17.9988314640083));
#136201=CARTESIAN_POINT('Ctrl Pts',(-18.013286793983,21.6688933896802,18.0030010299524));
#136202=CARTESIAN_POINT('Ctrl Pts',(-17.9334351461148,21.6426035685785,
18.0071705958964));
#136203=CARTESIAN_POINT('Ctrl Pts',(-17.8507760128143,21.6153894297986,
18.0114867586353));
#136204=CARTESIAN_POINT('Ctrl Pts',(-17.7695355706381,21.5839654477009,
18.0158029213743));
#136205=CARTESIAN_POINT('Ctrl Pts',(-17.6901612352907,21.5485201888519,
18.0201190841132));
#136206=CARTESIAN_POINT('Ctrl Pts',(-17.6133725105693,21.514229555582,18.0242946483049));
#136207=CARTESIAN_POINT('Ctrl Pts',(-17.5383305816069,21.4761758636208,
18.0284702124965));
#136208=CARTESIAN_POINT('Ctrl Pts',(-17.4654157475494,21.434576846982,18.0326457766882));
#136209=CARTESIAN_POINT('Ctrl Pts',(-17.388818158561,21.3908767629043,18.0370322387008));
#136210=CARTESIAN_POINT('Ctrl Pts',(-17.3145686822397,21.34326410831,18.0414187007134));
#136211=CARTESIAN_POINT('Ctrl Pts',(-17.2430721773898,21.2920416208636,
18.045805162726));
#136212=CARTESIAN_POINT('Ctrl Pts',(-17.1715756725399,21.2408191334172,
18.0501916247386));
#136213=CARTESIAN_POINT('Ctrl Pts',(-17.102832545326,21.185987234388,18.0545780867511));
#136214=CARTESIAN_POINT('Ctrl Pts',(-17.0372042845896,21.1278944415811,
18.0589645487637));
#136215=CARTESIAN_POINT('Ctrl Pts',(-16.9745956774138,21.0724745842853,
18.0631491831568));
#136216=CARTESIAN_POINT('Ctrl Pts',(-16.9145885551714,21.0138810328614,
18.06733381755));
#136217=CARTESIAN_POINT('Ctrl Pts',(-16.8575221052049,20.9523875818855,
18.0715184519431));
#136218=CARTESIAN_POINT('Ctrl Pts',(-16.8005368822664,20.8909816592257,
18.0756971300271));
#136219=CARTESIAN_POINT('Ctrl Pts',(-16.7464843277716,20.8266843701415,
18.0798758081111));
#136220=CARTESIAN_POINT('Ctrl Pts',(-16.6956693348425,20.759808606471,18.0840544861951));
#136221=CARTESIAN_POINT('Ctrl Pts',(-16.6439435196863,20.6917341428008,
18.0883080640805));
#136222=CARTESIAN_POINT('Ctrl Pts',(-16.5955728353227,20.6209881765788,
18.0925616419659));
#136223=CARTESIAN_POINT('Ctrl Pts',(-16.55083834023,20.5479387298265,18.0968152198513));
#136224=CARTESIAN_POINT('Ctrl Pts',(-16.506971110616,20.4763054891424,18.1009863338293));
#136225=CARTESIAN_POINT('Ctrl Pts',(-16.4666005905002,20.4024576962094,
18.1051574478073));
#136226=CARTESIAN_POINT('Ctrl Pts',(-16.4299490395872,20.3267729033368,
18.1093285617853));
#136227=CARTESIAN_POINT('Ctrl Pts',(-16.393309787456,20.2511135072275,18.1134982761058));
#136228=CARTESIAN_POINT('Ctrl Pts',(-16.3603872264447,20.1736187490988,
18.1176679904262));
#136229=CARTESIAN_POINT('Ctrl Pts',(-16.3313573525109,20.0946901654238,
18.1218377047466));
#136230=CARTESIAN_POINT('Ctrl Pts',(-16.3023285115847,20.0157643903665,
18.1260072706907));
#136231=CARTESIAN_POINT('Ctrl Pts',(-16.2771922403253,19.9354053232569,
18.1301768366348));
#136232=CARTESIAN_POINT('Ctrl Pts',(-16.2560756369329,19.854032542659,18.1343464025789));
#136233=CARTESIAN_POINT('Ctrl Pts',(-16.2342165998161,19.7697987954821,
18.1386625653178));
#136234=CARTESIAN_POINT('Ctrl Pts',(-16.2166652853052,19.6844792346862,
18.1429787280566));
#136235=CARTESIAN_POINT('Ctrl Pts',(-16.203505316394,19.5985521335794,18.1472948907955));
#136236=CARTESIAN_POINT('Ctrl Pts',(-16.1907740320855,19.5154240987507,
18.1514704549872));
#136237=CARTESIAN_POINT('Ctrl Pts',(-16.1821523920334,19.4317279704213,
18.1556460191789));
#136238=CARTESIAN_POINT('Ctrl Pts',(-16.177663165104,19.3479013752812,18.1598215833707));
#136239=CARTESIAN_POINT('Ctrl Pts',(-16.1729471979947,19.2598408981034,
18.1642080453831));
#136240=CARTESIAN_POINT('Ctrl Pts',(-16.172792072363,19.1716370118691,18.1685945073955));
#136241=CARTESIAN_POINT('Ctrl Pts',(-16.1771623761343,19.0837940049179,
18.1729809694079));
#136242=CARTESIAN_POINT('Ctrl Pts',(-16.1815326799056,18.9959509979667,
18.1773674314203));
#136243=CARTESIAN_POINT('Ctrl Pts',(-16.1904282787084,18.9084694398441,
18.1817538934327));
#136244=CARTESIAN_POINT('Ctrl Pts',(-16.2037517912763,18.8218419315364,
18.1861403554451));
#136245=CARTESIAN_POINT('Ctrl Pts',(-16.2164587426285,18.7392232130701,
18.1903238287683));
#136246=CARTESIAN_POINT('Ctrl Pts',(-16.2332401386069,18.6570738106168,
18.1945073020916));
#136247=CARTESIAN_POINT('Ctrl Pts',(-16.2540494029882,18.5758267666371,
18.1986907754148));
#136248=CARTESIAN_POINT('Ctrl Pts',(-16.2748315365047,18.494685651561,18.2028687943767));
#136249=CARTESIAN_POINT('Ctrl Pts',(-16.2996310005467,18.4144450007917,
18.2070468133385));
#136250=CARTESIAN_POINT('Ctrl Pts',(-16.3283498001328,18.3355303455408,
18.2112248323003));
#136251=CARTESIAN_POINT('Ctrl Pts',(-16.3570397744324,18.2566948975543,
18.2153986577514));
#136252=CARTESIAN_POINT('Ctrl Pts',(-16.3896411161687,18.1791832320051,
18.2195724832026));
#136253=CARTESIAN_POINT('Ctrl Pts',(-16.4260056863206,18.1034070025396,
18.2237463086537));
#136254=CARTESIAN_POINT('Ctrl Pts',(-16.462344667467,18.0276840952595,18.2279171970691));
#136255=CARTESIAN_POINT('Ctrl Pts',(-16.5024414177568,17.953694611493,18.2320880854844));
#136256=CARTESIAN_POINT('Ctrl Pts',(-16.5460997340485,17.8818301740374,
18.2362589738998));
#136257=CARTESIAN_POINT('Ctrl Pts',(-16.5897512956067,17.809976855314,18.2404292170031));
#136258=CARTESIAN_POINT('Ctrl Pts',(-16.6369631004847,17.7402483290546,
18.2445994601063));
#136259=CARTESIAN_POINT('Ctrl Pts',(-16.6874935461503,17.6730106195583,
18.2487697032096));
#136260=CARTESIAN_POINT('Ctrl Pts',(-16.7380175638304,17.6057814633809,
18.2529394158156));
#136261=CARTESIAN_POINT('Ctrl Pts',(-16.7918591019478,17.5410428584573,
18.2571091284217));
#136262=CARTESIAN_POINT('Ctrl Pts',(-16.8487348978804,17.4791294809571,
18.2612788410277));
#136263=CARTESIAN_POINT('Ctrl Pts',(-16.9056490538859,17.4171743457701,
18.2654513659105));
#136264=CARTESIAN_POINT('Ctrl Pts',(-16.9656012405693,17.3580485804858,
18.2696238907933));
#136265=CARTESIAN_POINT('Ctrl Pts',(-17.0282702918587,17.302051031912,18.2737964156761));
#136266=CARTESIAN_POINT('Ctrl Pts',(-17.0755086731215,17.259841464432,18.2769415617599));
#136267=CARTESIAN_POINT('Ctrl Pts',(-17.1242899094492,17.2194085525259,
18.2800867078438));
#136268=CARTESIAN_POINT('Ctrl Pts',(-17.174464231106,17.180864983421,18.2832318539276));
#136269=CARTESIAN_POINT('Origin',(-18.734,19.211,-1.76670989022852));
#136270=CARTESIAN_POINT('',(-17.1767158295569,17.1837658568561,19.1498287197874));
#136271=CARTESIAN_POINT('',(-17.174464231106,17.180864983421,19.083343695997));
#136272=CARTESIAN_POINT('',(-17.174464231106,17.180864983421,-1.76670989022852));
#136273=CARTESIAN_POINT('',(-21.2936055415609,19.2113823947434,18.6332901348857));
#136274=CARTESIAN_POINT('Ctrl Pts',(-21.2898372017813,19.2113866752102,
18.6332903748237));
#136275=CARTESIAN_POINT('Ctrl Pts',(-21.2903732285223,19.6159817978459,
18.6533365919766));
#136276=CARTESIAN_POINT('Ctrl Pts',(-21.0089154443045,20.8754716727687,
18.7157747446901));
#136277=CARTESIAN_POINT('Ctrl Pts',(-19.0350903746839,22.2230817299851,
18.8206048329641));
#136278=CARTESIAN_POINT('Ctrl Pts',(-16.3642904476992,21.0945520673855,
18.9477806396456));
#136279=CARTESIAN_POINT('Ctrl Pts',(-15.9356497533123,18.6295872620917,
19.0575219352533));
#136280=CARTESIAN_POINT('Ctrl Pts',(-16.7788810677115,17.4923455496799,
19.1248712953006));
#136281=CARTESIAN_POINT('Ctrl Pts',(-17.1767158295569,17.1837658568561,
19.1498287197874));
#136282=CARTESIAN_POINT('Ctrl Pts',(-17.174464231106,17.180864983421,18.3499540467144));
#136283=CARTESIAN_POINT('Ctrl Pts',(-17.2410774775475,17.1296931452628,
18.3541251281992));
#136284=CARTESIAN_POINT('Ctrl Pts',(-17.3102610867351,17.0817656086938,
18.358296209684));
#136285=CARTESIAN_POINT('Ctrl Pts',(-17.3816629355787,17.0373430665829,
18.3624672911689));
#136286=CARTESIAN_POINT('Ctrl Pts',(-17.4530411701186,16.992935216072,18.366636993177));
#136287=CARTESIAN_POINT('Ctrl Pts',(-17.5266357970195,16.9520303006554,
18.3708066951852));
#136288=CARTESIAN_POINT('Ctrl Pts',(-17.6020659860245,16.9148455217461,
18.3749763971933));
#136289=CARTESIAN_POINT('Ctrl Pts',(-17.6774938556494,16.8776618862204,
18.3791459709886));
#136290=CARTESIAN_POINT('Ctrl Pts',(-17.7547567621351,16.8441983623599,
18.3833155447838));
#136291=CARTESIAN_POINT('Ctrl Pts',(-17.8334508010709,16.8146254173631,
18.3874851185791));
#136292=CARTESIAN_POINT('Ctrl Pts',(-17.9145943067586,16.7841319713156,
18.3917844764408));
#136293=CARTESIAN_POINT('Ctrl Pts',(-17.9972590302591,16.7577755082822,
18.3960838343025));
#136294=CARTESIAN_POINT('Ctrl Pts',(-18.0809836050741,16.7356879816965,
18.4003831921643));
#136295=CARTESIAN_POINT('Ctrl Pts',(-18.1622980297666,16.7142362810318,
18.4045587859113));
#136296=CARTESIAN_POINT('Ctrl Pts',(-18.2446116391388,16.6968111018946,
18.4087343796584));
#136297=CARTESIAN_POINT('Ctrl Pts',(-18.3274916636507,16.6834812616959,
18.4129099734055));
#136298=CARTESIAN_POINT('Ctrl Pts',(-18.4140565196421,16.6695587791195,
18.4172712133245));
#136299=CARTESIAN_POINT('Ctrl Pts',(-18.5012387641433,16.6601043283044,
18.4216324532436));
#136300=CARTESIAN_POINT('Ctrl Pts',(-18.5885418813438,16.6551357751796,
18.4259936931626));
#136301=CARTESIAN_POINT('Ctrl Pts',(-18.6758449985444,16.6501672220548,
18.4303549330817));
#136302=CARTESIAN_POINT('Ctrl Pts',(-18.7632684243732,16.6496844955093,
18.4347161730007));
#136303=CARTESIAN_POINT('Ctrl Pts',(-18.8503205710793,16.6536440363642,
18.4390774129198));
#136304=CARTESIAN_POINT('Ctrl Pts',(-18.933847598669,16.6574432382305,18.4432620473123));
#136305=CARTESIAN_POINT('Ctrl Pts',(-19.0173437395032,16.6653459878635,
18.4474466817047));
#136306=CARTESIAN_POINT('Ctrl Pts',(-19.1003730904697,16.6773522820685,
18.4516313160972));
#136307=CARTESIAN_POINT('Ctrl Pts',(-19.1832842594319,16.6893414867997,
18.4558099941806));
#136308=CARTESIAN_POINT('Ctrl Pts',(-19.2657295068657,16.7054225689875,
18.4599886722639));
#136309=CARTESIAN_POINT('Ctrl Pts',(-19.3472750579147,16.7255435623734,
18.4641673503473));
#136310=CARTESIAN_POINT('Ctrl Pts',(-19.4302822543748,16.7460252101085,
18.4684209282329));
#136311=CARTESIAN_POINT('Ctrl Pts',(-19.5123567014431,16.7706930025013,
18.4726745061185));
#136312=CARTESIAN_POINT('Ctrl Pts',(-19.5930485432792,16.7994371042227,
18.476928084004));
#136313=CARTESIAN_POINT('Ctrl Pts',(-19.6721760162898,16.8276239454376,
18.4810991979814));
#136314=CARTESIAN_POINT('Ctrl Pts',(-19.7499735613558,16.8597302905281,
18.4852703119587));
#136315=CARTESIAN_POINT('Ctrl Pts',(-19.8260310897316,16.8956019566693,
18.4894414259361));
#136316=CARTESIAN_POINT('Ctrl Pts',(-19.9020630962693,16.9314615857266,
18.4936111402559));
#136317=CARTESIAN_POINT('Ctrl Pts',(-19.976355829979,16.9710838304488,18.4977808545756));
#136318=CARTESIAN_POINT('Ctrl Pts',(-20.0485201368038,17.0142667868088,
18.5019505688954));
#136319=CARTESIAN_POINT('Ctrl Pts',(-20.1206818757128,17.0574482065338,
18.5061201348388));
#136320=CARTESIAN_POINT('Ctrl Pts',(-20.1907149440086,17.1041898490227,
18.5102897007823));
#136321=CARTESIAN_POINT('Ctrl Pts',(-20.25825690416,17.1542450583211,18.5144592667257));
#136322=CARTESIAN_POINT('Ctrl Pts',(-20.3281735563298,17.2060601470446,
18.5187754294653));
#136323=CARTESIAN_POINT('Ctrl Pts',(-20.3954202425942,17.2614258339352,
18.523091592205));
#136324=CARTESIAN_POINT('Ctrl Pts',(-20.4596314884403,17.3200224839773,
18.5274077549446));
#136325=CARTESIAN_POINT('Ctrl Pts',(-20.5217510596875,17.37671035429,18.5315833191357));
#136326=CARTESIAN_POINT('Ctrl Pts',(-20.5810296141605,17.4364215555172,
18.5357588833267));
#136327=CARTESIAN_POINT('Ctrl Pts',(-20.6371745600437,17.4988298583369,
18.5399344475178));
#136328=CARTESIAN_POINT('Ctrl Pts',(-20.6961552536984,17.5643902562004,
18.5443209095317));
#136329=CARTESIAN_POINT('Ctrl Pts',(-20.7516770948093,17.6329269235829,
18.5487073715456));
#136330=CARTESIAN_POINT('Ctrl Pts',(-20.8034508935159,17.7040252160948,
18.5530938335595));
#136331=CARTESIAN_POINT('Ctrl Pts',(-20.8552246922225,17.7751235086066,
18.5574802955734));
#136332=CARTESIAN_POINT('Ctrl Pts',(-20.9032501953502,17.8487828986681,
18.5618667575873));
#136333=CARTESIAN_POINT('Ctrl Pts',(-20.9472937739972,17.9245589131308,
18.5662532196012));
#136334=CARTESIAN_POINT('Ctrl Pts',(-20.9909726387699,17.9997074453438,
18.5706033584188));
#136335=CARTESIAN_POINT('Ctrl Pts',(-21.0308877830075,18.0771985084606,
18.5749534972363));
#136336=CARTESIAN_POINT('Ctrl Pts',(-21.0667913726612,18.1566355413627,
18.5793036360538));
#136337=CARTESIAN_POINT('Ctrl Pts',(-21.1039225287098,18.2387885765656,
18.5838025088636));
#136338=CARTESIAN_POINT('Ctrl Pts',(-21.1367625751612,18.3230227236645,
18.5883013816734));
#136339=CARTESIAN_POINT('Ctrl Pts',(-21.1650869626505,18.4088677290927,
18.5928002544832));
#136340=CARTESIAN_POINT('Ctrl Pts',(-21.1923645588302,18.4915401396792,
18.5971328613513));
#136341=CARTESIAN_POINT('Ctrl Pts',(-21.2154541944225,18.5757060184776,
18.6014654682194));
#136342=CARTESIAN_POINT('Ctrl Pts',(-21.234202937817,18.6609224875245,18.6057980750875));
#136343=CARTESIAN_POINT('Ctrl Pts',(-21.2529274817652,18.7460289656604,
18.6101250897574));
#136344=CARTESIAN_POINT('Ctrl Pts',(-21.2673221897251,18.8321829392873,
18.6144521044274));
#136345=CARTESIAN_POINT('Ctrl Pts',(-21.2772839154183,18.9189265065526,
18.6187791190974));
#136346=CARTESIAN_POINT('Ctrl Pts',(-21.2872318317724,19.0055498264465,
18.6231001354881));
#136347=CARTESIAN_POINT('Ctrl Pts',(-21.2927589555479,19.0927607071587,
18.6274211518788));
#136348=CARTESIAN_POINT('Ctrl Pts',(-21.2938134141941,19.1800923227686,
18.6317421682696));
#136349=CARTESIAN_POINT('Ctrl Pts',(-21.2939393290371,19.1905207513303,
18.6322581487702));
#136350=CARTESIAN_POINT('Ctrl Pts',(-21.2940015277988,19.2009508929668,
18.6327741292709));
#136351=CARTESIAN_POINT('Ctrl Pts',(-21.2939999715072,19.2113819467094,
18.6332901097715));
#136352=CARTESIAN_POINT('',(-21.2939999971965,19.2111198080496,18.5667098901964));
#136353=CARTESIAN_POINT('Ctrl Pts',(-17.174464231106,17.180864983421,18.2832318539276));
#136354=CARTESIAN_POINT('Ctrl Pts',(-17.2411083724626,17.1296694120014,
18.2874094003952));
#136355=CARTESIAN_POINT('Ctrl Pts',(-17.3102109927058,17.0818088780222,
18.2915869468627));
#136356=CARTESIAN_POINT('Ctrl Pts',(-17.3813970185547,17.0375085289826,
18.2957644933303));
#136357=CARTESIAN_POINT('Ctrl Pts',(-17.4526990807105,16.9931359684545,
18.2999488493796));
#136358=CARTESIAN_POINT('Ctrl Pts',(-17.5260909246801,16.9523353976319,
18.3041332054289));
#136359=CARTESIAN_POINT('Ctrl Pts',(-17.6011737540801,16.9152855803574,
18.3083175614783));
#136360=CARTESIAN_POINT('Ctrl Pts',(-17.6310715508009,16.9005324348744,
18.3099837616943));
#136361=CARTESIAN_POINT('Ctrl Pts',(-17.6612372642791,16.8863734711475,
18.3116499619104));
#136362=CARTESIAN_POINT('Ctrl Pts',(-17.6916449845519,16.8728177954295,
18.3133161621265));
#136363=CARTESIAN_POINT('Ctrl Pts',(-17.7680134730662,16.8387729391863,
18.3175007965194));
#136364=CARTESIAN_POINT('Ctrl Pts',(-17.8461937671331,16.8084101229908,
18.3216854309124));
#136365=CARTESIAN_POINT('Ctrl Pts',(-17.9257962079479,16.7819247375776,
18.3258700653053));
#136366=CARTESIAN_POINT('Ctrl Pts',(-18.0052853445408,16.7554770508323,
18.3300487433892));
#136367=CARTESIAN_POINT('Ctrl Pts',(-18.0861921743122,16.7328959763057,
18.334227421473));
#136368=CARTESIAN_POINT('Ctrl Pts',(-18.1681056484765,16.714329500532,18.3384060995568));
#136369=CARTESIAN_POINT('Ctrl Pts',(-18.2514873627979,16.6954302340229,
18.3426596774423));
#136370=CARTESIAN_POINT('Ctrl Pts',(-18.3359117243126,16.6806911015683,
18.3469132553277));
#136371=CARTESIAN_POINT('Ctrl Pts',(-18.4209273694984,16.6702155683666,
18.3511668332132));
#136372=CARTESIAN_POINT('Ctrl Pts',(-18.5042948205052,16.6599431238176,
18.355337947191));
#136373=CARTESIAN_POINT('Ctrl Pts',(-18.5882303557915,16.6537704962434,
18.3595090611689));
#136374=CARTESIAN_POINT('Ctrl Pts',(-18.6722982812007,16.6517436826497,
18.3636801751467));
#136375=CARTESIAN_POINT('Ctrl Pts',(-18.7563379968057,16.649717549173,18.367849889467));
#136376=CARTESIAN_POINT('Ctrl Pts',(-18.8405095547889,16.6518344778738,
18.3720196037873));
#136377=CARTESIAN_POINT('Ctrl Pts',(-18.9243745836524,16.6580884234077,
18.3761893181075));
#136378=CARTESIAN_POINT('Ctrl Pts',(-19.0082366282384,16.6643421463994,
18.3803588840514));
#136379=CARTESIAN_POINT('Ctrl Pts',(-19.0917917066962,16.6747325584671,
18.3845284499954));
#136380=CARTESIAN_POINT('Ctrl Pts',(-19.1746052695965,16.6892016344672,
18.3886980159393));
#136381=CARTESIAN_POINT('Ctrl Pts',(-19.2603304552117,16.7041794253309,
18.3930141786784));
#136382=CARTESIAN_POINT('Ctrl Pts',(-19.3452604921649,16.723527937402,18.3973303414174));
#136383=CARTESIAN_POINT('Ctrl Pts',(-19.4289254033766,16.7471252702822,
18.4016465041565));
#136384=CARTESIAN_POINT('Ctrl Pts',(-19.5098649389009,16.7699539225245,
18.405822068348));
#136385=CARTESIAN_POINT('Ctrl Pts',(-19.5896200744158,16.796758641008,18.4099976325396));
#136386=CARTESIAN_POINT('Ctrl Pts',(-19.667783027385,16.8273789609571,18.4141731967312));
#136387=CARTESIAN_POINT('Ctrl Pts',(-19.7498938053008,16.8595458404767,
18.418559658744));
#136388=CARTESIAN_POINT('Ctrl Pts',(-19.8302467994661,16.8959236625789,
18.4229461207568));
#136389=CARTESIAN_POINT('Ctrl Pts',(-19.9083976363224,16.9362714026064,
18.4273325827696));
#136390=CARTESIAN_POINT('Ctrl Pts',(-19.9865484731787,16.9766191426339,
18.4317190447824));
#136391=CARTESIAN_POINT('Ctrl Pts',(-20.0624966899236,17.0209364424643,
18.4361055067951));
#136392=CARTESIAN_POINT('Ctrl Pts',(-20.1358342086536,17.0689307080656,
18.4404919688079));
#136393=CARTESIAN_POINT('Ctrl Pts',(-20.2057039471168,17.1146555545475,
18.4446710160258));
#136394=CARTESIAN_POINT('Ctrl Pts',(-20.2734659150699,17.1638887348098,
18.4488500632436));
#136395=CARTESIAN_POINT('Ctrl Pts',(-20.3387454860834,17.2164093339998,
18.4530291104615));
#136396=CARTESIAN_POINT('Ctrl Pts',(-20.4039320790894,17.2688551278475,
18.4572022054423));
#136397=CARTESIAN_POINT('Ctrl Pts',(-20.4666429412498,17.3245787540421,
18.461375300423));
#136398=CARTESIAN_POINT('Ctrl Pts',(-20.5265316718114,17.3833156165374,
18.4655483954038));
#136399=CARTESIAN_POINT('Ctrl Pts',(-20.5870226816091,17.4426431743496,
18.4697634576868));
#136400=CARTESIAN_POINT('Ctrl Pts',(-20.6446340707896,17.5050446643085,
18.4739785199699));
#136401=CARTESIAN_POINT('Ctrl Pts',(-20.6990425114803,17.5702050926228,
18.4781935822529));
#136402=CARTESIAN_POINT('Ctrl Pts',(-20.7528122887529,17.6346006473008,
18.4823591668069));
#136403=CARTESIAN_POINT('Ctrl Pts',(-20.8034536124378,17.701690347722,18.4865247513609));
#136404=CARTESIAN_POINT('Ctrl Pts',(-20.8506921231952,17.7711338758054,
18.4906903359149));
#136405=CARTESIAN_POINT('Ctrl Pts',(-20.8979149500342,17.84055434756,18.4948545374302));
#136406=CARTESIAN_POINT('Ctrl Pts',(-20.9417369482813,17.9123267137653,
18.4990187389455));
#136407=CARTESIAN_POINT('Ctrl Pts',(-20.9819260328715,17.9860801859964,
18.5031829404608));
#136408=CARTESIAN_POINT('Ctrl Pts',(-21.0221139173364,18.0598314558035,
18.5073470176248));
#136409=CARTESIAN_POINT('Ctrl Pts',(-21.0586688839109,18.1355633083682,
18.5115110947889));
#136410=CARTESIAN_POINT('Ctrl Pts',(-21.0914046022626,18.2128799965779,
18.5156751719529));
#136411=CARTESIAN_POINT('Ctrl Pts',(-21.1248385440613,18.2918457802491,
18.5199280651399));
#136412=CARTESIAN_POINT('Ctrl Pts',(-21.1542882228968,18.3724643312946,
18.5241809583268));
#136413=CARTESIAN_POINT('Ctrl Pts',(-21.1796074785073,18.4542939401135,
18.5284338515138));
#136414=CARTESIAN_POINT('Ctrl Pts',(-21.2044336791702,18.5345300386761,
18.5326039259141));
#136415=CARTESIAN_POINT('Ctrl Pts',(-21.2252888283686,18.6159299801768,
18.5367740003144));
#136416=CARTESIAN_POINT('Ctrl Pts',(-21.2420864983912,18.6980651926534,
18.5409440747148));
#136417=CARTESIAN_POINT('Ctrl Pts',(-21.2593845777047,18.7826472458753,
18.545238377295));
#136418=CARTESIAN_POINT('Ctrl Pts',(-21.2723795196075,18.8680085473307,
18.5495326798753));
#136419=CARTESIAN_POINT('Ctrl Pts',(-21.2810343673868,18.9536754357808,
18.5538269824556));
#136420=CARTESIAN_POINT('Ctrl Pts',(-21.2896892151661,19.0393423242309,
18.5581212850358));
#136421=CARTESIAN_POINT('Ctrl Pts',(-21.2940040128973,19.125314270194,18.5624155876161));
#136422=CARTESIAN_POINT('Ctrl Pts',(-21.2939999971965,19.2111198080496,
18.5667098901964));
#136423=CARTESIAN_POINT('Ctrl Pts',(-21.2939999971965,19.2111198086917,
18.5667098902285));
#136424=CARTESIAN_POINT('Ctrl Pts',(-21.2939996986147,19.2174997239769,
18.5670291853155));
#136425=CARTESIAN_POINT('Ctrl Pts',(-21.2939755504833,19.223879573923,18.5673484804024));
#136426=CARTESIAN_POINT('Ctrl Pts',(-21.2939275539577,19.2302592442234,
18.5676677754894));
#136427=CARTESIAN_POINT('Ctrl Pts',(-21.2932985185608,19.31387026376,18.5718524098819));
#136428=CARTESIAN_POINT('Ctrl Pts',(-21.2885677156651,19.3976060296583,
18.5760370442745));
#136429=CARTESIAN_POINT('Ctrl Pts',(-21.2797186185528,19.4810309522135,
18.580221678667));
#136430=CARTESIAN_POINT('Ctrl Pts',(-21.2708821170351,19.5643371297175,
18.5844003567505));
#136431=CARTESIAN_POINT('Ctrl Pts',(-21.2579390129528,19.6473328891638,
18.5885790348339));
#136432=CARTESIAN_POINT('Ctrl Pts',(-21.2409247859828,19.7295827970778,
18.5927577129174));
#136433=CARTESIAN_POINT('Ctrl Pts',(-21.2236055912197,19.8133069754917,
18.5970112908029));
#136434=CARTESIAN_POINT('Ctrl Pts',(-21.2020678918843,19.8962578184688,
18.6012648686885));
#136435=CARTESIAN_POINT('Ctrl Pts',(-21.1764043852928,19.9779816286603,
18.605518446574));
#136436=CARTESIAN_POINT('Ctrl Pts',(-21.1512384158585,20.0581210633086,
18.6096895605515));
#136437=CARTESIAN_POINT('Ctrl Pts',(-21.1221053294156,20.1370801583403,
18.613860674529));
#136438=CARTESIAN_POINT('Ctrl Pts',(-21.0891436468889,20.2144432731942,
18.6180317885065));
#136439=CARTESIAN_POINT('Ctrl Pts',(-21.0561930249731,20.2917804281078,
18.6222015028263));
#136440=CARTESIAN_POINT('Ctrl Pts',(-21.0194165386216,20.3675222435798,
18.6263712171462));
#136441=CARTESIAN_POINT('Ctrl Pts',(-20.9790011895033,20.4412721890413,
18.6305409314661));
#136442=CARTESIAN_POINT('Ctrl Pts',(-20.9385872785366,20.5150195101634,
18.6347104974097));
#136443=CARTESIAN_POINT('Ctrl Pts',(-20.8945349840829,20.5867746991834,
18.6388800633533));
#136444=CARTESIAN_POINT('Ctrl Pts',(-20.8470770406692,20.6561662258013,
18.6430496292968));
#136445=CARTESIAN_POINT('Ctrl Pts',(-20.7979505344985,20.7279974729093,
18.6473657920363));
#136446=CARTESIAN_POINT('Ctrl Pts',(-20.7451747360215,20.7972953169815,
18.6516819547758));
#136447=CARTESIAN_POINT('Ctrl Pts',(-20.6890551911697,20.863682425477,18.6559981175153));
#136448=CARTESIAN_POINT('Ctrl Pts',(-20.634763734602,20.9279069808801,18.6601736817066));
#136449=CARTESIAN_POINT('Ctrl Pts',(-20.5773433873057,20.9894072108732,
18.6643492458978));
#136450=CARTESIAN_POINT('Ctrl Pts',(-20.517109048565,21.0478783631274,18.668524810089));
#136451=CARTESIAN_POINT('Ctrl Pts',(-20.4538324165451,21.1093027543023,
18.6729112721026));
#136452=CARTESIAN_POINT('Ctrl Pts',(-20.3874504923528,21.1673836440657,
18.6772977341163));
#136453=CARTESIAN_POINT('Ctrl Pts',(-20.3183666557521,21.2218163268038,
18.6816841961299));
#136454=CARTESIAN_POINT('Ctrl Pts',(-20.2492828191514,21.276249009542,18.6860706581436));
#136455=CARTESIAN_POINT('Ctrl Pts',(-20.1774975877418,21.327033212256,18.6904571201572));
#136456=CARTESIAN_POINT('Ctrl Pts',(-20.1034462555222,21.3739186191894,
18.6948435821709));
#136457=CARTESIAN_POINT('Ctrl Pts',(-20.032802134896,21.4186467590315,18.6990282165633));
#136458=CARTESIAN_POINT('Ctrl Pts',(-19.9598329133702,21.459993484366,18.7032128509558));
#136459=CARTESIAN_POINT('Ctrl Pts',(-19.8848959073541,21.497709122393,18.7073974853483));
#136460=CARTESIAN_POINT('Ctrl Pts',(-19.8100655648908,21.5353710768775,
18.7115761634316));
#136461=CARTESIAN_POINT('Ctrl Pts',(-19.733273408809,21.5694120050826,18.715754841515));
#136462=CARTESIAN_POINT('Ctrl Pts',(-19.654904774228,21.5996260479204,18.7199335195984));
#136463=CARTESIAN_POINT('Ctrl Pts',(-19.5751314381808,21.630381655767,18.7241870974839));
#136464=CARTESIAN_POINT('Ctrl Pts',(-19.493724958338,21.6571715770569,18.7284406753695));
#136465=CARTESIAN_POINT('Ctrl Pts',(-19.41111699767,21.6798281777933,18.7326942532551));
#136466=CARTESIAN_POINT('Ctrl Pts',(-19.3301105535301,21.7020455361098,
18.7368653672325));
#136467=CARTESIAN_POINT('Ctrl Pts',(-19.2479492630204,21.7202882813848,
18.7410364812098));
#136468=CARTESIAN_POINT('Ctrl Pts',(-19.1650575928257,21.734447909442,18.7452075951871));
#136469=CARTESIAN_POINT('Ctrl Pts',(-19.0821937377315,21.7486027860993,
18.7493773095069));
#136470=CARTESIAN_POINT('Ctrl Pts',(-18.9986004427839,21.7586771892408,
18.7535470238267));
#136471=CARTESIAN_POINT('Ctrl Pts',(-18.9147123478954,21.7646137232005,
18.7577167381465));
#136472=CARTESIAN_POINT('Ctrl Pts',(-18.8308272381054,21.7705500459129,
18.7618863040899));
#136473=CARTESIAN_POINT('Ctrl Pts',(-18.7466478081773,21.7723487605766,
18.7660558700333));
#136474=CARTESIAN_POINT('Ctrl Pts',(-18.6626124310825,21.7700044577929,
18.7702254359768));
#136475=CARTESIAN_POINT('Ctrl Pts',(-18.5756224737711,21.7675777322146,
18.7745415987164));
#136476=CARTESIAN_POINT('Ctrl Pts',(-18.4887874147817,21.7607112463061,
18.778857761456));
#136477=CARTESIAN_POINT('Ctrl Pts',(-18.4025899172848,21.749457672894,18.7831739241957));
#136478=CARTESIAN_POINT('Ctrl Pts',(-18.3192002942283,21.7385706834556,
18.7873494883867));
#136479=CARTESIAN_POINT('Ctrl Pts',(-18.2364077885004,21.7235781663988,
18.7915250525778));
#136480=CARTESIAN_POINT('Ctrl Pts',(-18.1546390975914,21.7045799455322,
18.7957006167689));
#136481=CARTESIAN_POINT('Ctrl Pts',(-18.0687404644519,21.6846221696844,
18.8000870787828));
#136482=CARTESIAN_POINT('Ctrl Pts',(-17.9839723511224,21.6602435606427,
18.8044735407967));
#136483=CARTESIAN_POINT('Ctrl Pts',(-17.9008093086191,21.6316183655827,
18.8088600028106));
#136484=CARTESIAN_POINT('Ctrl Pts',(-17.8176462661158,21.6029931705227,
18.8132464648245));
#136485=CARTESIAN_POINT('Ctrl Pts',(-17.7360888041544,21.5701216768946,
18.8176329268384));
#136486=CARTESIAN_POINT('Ctrl Pts',(-17.6565830150584,21.5332344068933,
18.8220193888523));
#136487=CARTESIAN_POINT('Ctrl Pts',(-17.5807354051426,21.4980443748501,
18.8262040232484));
#136488=CARTESIAN_POINT('Ctrl Pts',(-17.5064724966939,21.4590690053602,
18.8303886576445));
#136489=CARTESIAN_POINT('Ctrl Pts',(-17.4341976336211,21.416473601827,18.8345732920406));
#136490=CARTESIAN_POINT('Ctrl Pts',(-17.3620256448697,21.3739388275783,
18.8387519701277));
#136491=CARTESIAN_POINT('Ctrl Pts',(-17.2918364736816,21.327794485688,18.8429306482147));
#136492=CARTESIAN_POINT('Ctrl Pts',(-17.2240117895636,21.2782531543918,
18.8471093263017));
#136493=CARTESIAN_POINT('Ctrl Pts',(-17.1549713967908,21.2278238303831,
18.8513629041864));
#136494=CARTESIAN_POINT('Ctrl Pts',(-17.0883815290674,21.173874739978,18.855616482071));
#136495=CARTESIAN_POINT('Ctrl Pts',(-17.0246167910337,21.1166781063191,
18.8598700599557));
#136496=CARTESIAN_POINT('Ctrl Pts',(-16.9620882568161,21.0605903409623,
18.8640411739367));
#136497=CARTESIAN_POINT('Ctrl Pts',(-16.9022766467391,21.0013801499079,
18.8682122879177));
#136498=CARTESIAN_POINT('Ctrl Pts',(-16.8455029514096,20.9393457112121,
18.8723834018988));
#136499=CARTESIAN_POINT('Ctrl Pts',(-16.788748307042,20.8773320887715,18.8765531162222));
#136500=CARTESIAN_POINT('Ctrl Pts',(-16.7350298632001,20.8124964399251,
18.8807228305456));
#136501=CARTESIAN_POINT('Ctrl Pts',(-16.6846311428973,20.7451731608712,
18.8848925448691));
#136502=CARTESIAN_POINT('Ctrl Pts',(-16.6342342159975,20.6778522774687,
18.8890621108162));
#136503=CARTESIAN_POINT('Ctrl Pts',(-16.5871570527732,20.6080443086434,
18.8932316767633));
#136504=CARTESIAN_POINT('Ctrl Pts',(-16.5436414846482,20.5361149286858,
18.8974012427104));
#136505=CARTESIAN_POINT('Ctrl Pts',(-16.4985959629012,20.4616566005807,
18.9017174054456));
#136506=CARTESIAN_POINT('Ctrl Pts',(-16.4573674205007,20.384925359397,18.9060335681809));
#136507=CARTESIAN_POINT('Ctrl Pts',(-16.420172824354,20.3063555592783,18.9103497309162));
#136508=CARTESIAN_POINT('Ctrl Pts',(-16.3841898382084,20.2303451620158,
18.9145252951109));
#136509=CARTESIAN_POINT('Ctrl Pts',(-16.3519821593669,20.1526146016957,
18.9187008593055));
#136510=CARTESIAN_POINT('Ctrl Pts',(-16.3236968150629,20.0735766961158,
18.9228764235002));
#136511=CARTESIAN_POINT('Ctrl Pts',(-16.2939828453285,19.990546774011,18.9272628855058));
#136512=CARTESIAN_POINT('Ctrl Pts',(-16.2685980256127,19.9060745270031,
18.9316493475114));
#136513=CARTESIAN_POINT('Ctrl Pts',(-16.24765270708,19.8206532940854,18.936035809517));
#136514=CARTESIAN_POINT('Ctrl Pts',(-16.2267073885473,19.7352320611677,
18.9404222715225));
#136515=CARTESIAN_POINT('Ctrl Pts',(-16.210201605397,19.6488624265218,18.9448087335281));
#136516=CARTESIAN_POINT('Ctrl Pts',(-16.1981829862585,19.5620442604845,
18.9491951955337));
#136517=CARTESIAN_POINT('Ctrl Pts',(-16.1867173615958,19.4792207269146,
18.9533798299225));
#136518=CARTESIAN_POINT('Ctrl Pts',(-16.1792923755172,19.3956807451282,
18.9575644643113));
#136519=CARTESIAN_POINT('Ctrl Pts',(-16.1759873564286,19.3118529391174,
18.9617490987001));
#136520=CARTESIAN_POINT('Ctrl Pts',(-16.1726870416255,19.2281444516125,
18.9659277767798));
#136521=CARTESIAN_POINT('Ctrl Pts',(-16.173495063509,19.1441494093851,18.9701064548596));
#136522=CARTESIAN_POINT('Ctrl Pts',(-16.1784392678899,19.0603038006557,
18.9742851329393));
#136523=CARTESIAN_POINT('Ctrl Pts',(-16.1834720935873,18.974955319541,18.9785387108258));
#136524=CARTESIAN_POINT('Ctrl Pts',(-16.1927909085457,18.8897621593934,
18.9827922887123));
#136525=CARTESIAN_POINT('Ctrl Pts',(-16.2063695825696,18.8051866526586,
18.9870458665988));
#136526=CARTESIAN_POINT('Ctrl Pts',(-16.2196850074843,18.7222508072609,
18.9912169805725));
#136527=CARTESIAN_POINT('Ctrl Pts',(-16.2370965177706,18.6399093552906,
18.9953880945463));
#136528=CARTESIAN_POINT('Ctrl Pts',(-16.2585271389987,18.5585935971758,
18.9995592085201));
#136529=CARTESIAN_POINT('Ctrl Pts',(-16.279950568975,18.4773051253485,19.0037289228363));
#136530=CARTESIAN_POINT('Ctrl Pts',(-16.3053903143098,18.3970421082999,
19.0078986371526));
#136531=CARTESIAN_POINT('Ctrl Pts',(-16.3347186663499,18.3182239463347,
19.0120683514688));
#136532=CARTESIAN_POINT('Ctrl Pts',(-16.3640459747616,18.2394085890572,
19.0162379174088));
#136533=CARTESIAN_POINT('Ctrl Pts',(-16.3972614535261,18.162038415493,19.0204074833487));
#136534=CARTESIAN_POINT('Ctrl Pts',(-16.4341885271975,18.0865147001556,
19.0245770492886));
#136535=CARTESIAN_POINT('Ctrl Pts',(-16.4724139113062,18.008335663989,19.0288932120325));
#136536=CARTESIAN_POINT('Ctrl Pts',(-16.5146165141609,17.9321358186697,
19.0332093747764));
#136537=CARTESIAN_POINT('Ctrl Pts',(-16.5605485527345,17.8583327066941,
19.0375255375203));
#136538=CARTESIAN_POINT('Ctrl Pts',(-16.6049843598895,17.7869337234782,
19.041701101708));
#136539=CARTESIAN_POINT('Ctrl Pts',(-16.6529100541823,17.7177780846056,
19.0458766658957));
#136540=CARTESIAN_POINT('Ctrl Pts',(-16.704058104228,17.6512128671548,19.0500522300834));
#136541=CARTESIAN_POINT('Ctrl Pts',(-16.757789520855,17.5812855985977,19.0544386921054));
#136542=CARTESIAN_POINT('Ctrl Pts',(-16.8150769912952,17.5142177570114,
19.0588251541273));
#136543=CARTESIAN_POINT('Ctrl Pts',(-16.8755654265149,17.450369165306,19.0632116161493));
#136544=CARTESIAN_POINT('Ctrl Pts',(-16.9360538617346,17.3865205736007,
19.0675980781712));
#136545=CARTESIAN_POINT('Ctrl Pts',(-16.9997427890409,17.3258915767388,
19.0719845401932));
#136546=CARTESIAN_POINT('Ctrl Pts',(-17.0662376770542,17.2687927931957,
19.0763710022152));
#136547=CARTESIAN_POINT('Ctrl Pts',(-17.1014709690828,17.2385381649806,
19.0786952334758));
#136548=CARTESIAN_POINT('Ctrl Pts',(-17.1375641351115,17.209211383591,19.0810194647364));
#136549=CARTESIAN_POINT('Ctrl Pts',(-17.174464231106,17.180864983421,19.083343695997));
#136550=CARTESIAN_POINT('Origin',(-18.734,19.211,-1.76670989022852));
#136551=CARTESIAN_POINT('',(-17.174464231106,17.180864983421,19.9498236312054));
#136552=CARTESIAN_POINT('',(-17.174464231106,17.180864983421,19.8833624896767));
#136553=CARTESIAN_POINT('',(-17.174464231106,17.180864983421,-1.76670989022852));
#136554=CARTESIAN_POINT('',(-21.2939990581246,19.2131959965571,19.4332901097715));
#136555=CARTESIAN_POINT('Ctrl Pts',(-21.2939990581246,19.2131959965571,
19.4332901097715));
#136556=CARTESIAN_POINT('Ctrl Pts',(-21.293890587382,19.3396465586196,19.4395926510263));
#136557=CARTESIAN_POINT('Ctrl Pts',(-21.2844099378551,19.465708927393,19.4458951922812));
#136558=CARTESIAN_POINT('Ctrl Pts',(-21.2657470116552,19.5902849443033,
19.452197733536));
#136559=CARTESIAN_POINT('Ctrl Pts',(-21.2615163488398,19.618524841776,19.4536264444811));
#136560=CARTESIAN_POINT('Ctrl Pts',(-21.2568139996567,19.6466884925667,
19.4550551554262));
#136561=CARTESIAN_POINT('Ctrl Pts',(-21.2516424693627,19.6747632978808,
19.4564838663713));
#136562=CARTESIAN_POINT('Ctrl Pts',(-21.2364952751686,19.7569932189831,
19.4606685004935));
#136563=CARTESIAN_POINT('Ctrl Pts',(-21.2172870302474,19.8386332916553,
19.4648531346158));
#136564=CARTESIAN_POINT('Ctrl Pts',(-21.1940771445785,19.9192516803528,
19.469037768738));
#136565=CARTESIAN_POINT('Ctrl Pts',(-21.1709002953099,19.9997553187496,
19.4732164465514));
#136566=CARTESIAN_POINT('Ctrl Pts',(-21.1437332452095,20.0792397234556,
19.4773951243647));
#136567=CARTESIAN_POINT('Ctrl Pts',(-21.1126865924437,20.1572822490824,
19.4815738021781));
#136568=CARTESIAN_POINT('Ctrl Pts',(-21.0810834481907,20.2367236373009,
19.4858273801312));
#136569=CARTESIAN_POINT('Ctrl Pts',(-21.0454603361894,20.3146704722382,
19.4900809580843));
#136570=CARTESIAN_POINT('Ctrl Pts',(-21.0059873753743,20.3906920641166,
19.4943345360374));
#136571=CARTESIAN_POINT('Ctrl Pts',(-20.9672796780334,20.4652398231152,
19.4985056497473));
#136572=CARTESIAN_POINT('Ctrl Pts',(-20.9248702957982,20.5379358953033,
19.5026767634572));
#136573=CARTESIAN_POINT('Ctrl Pts',(-20.8789678616489,20.6083950309391,
19.506847877167));
#136574=CARTESIAN_POINT('Ctrl Pts',(-20.8330808304891,20.6788305233554,
19.5110175912208));
#136575=CARTESIAN_POINT('Ctrl Pts',(-20.7837033261796,20.7470301848417,
19.5151873052746));
#136576=CARTESIAN_POINT('Ctrl Pts',(-20.7310884045781,20.8126360086797,
19.5193570193284));
#136577=CARTESIAN_POINT('Ctrl Pts',(-20.6784753552182,20.8782394980099,
19.5235265850078));
#136578=CARTESIAN_POINT('Ctrl Pts',(-20.6226254060923,20.9412489748611,
19.5276961506871));
#136579=CARTESIAN_POINT('Ctrl Pts',(-20.5638323063888,21.0013389987641,
19.5318657163664));
#136580=CARTESIAN_POINT('Ctrl Pts',(-20.502972105477,21.0635417223146,19.5361818794236));
#136581=CARTESIAN_POINT('Ctrl Pts',(-20.4389583088965,21.122615499409,19.5404980424808));
#136582=CARTESIAN_POINT('Ctrl Pts',(-20.3721573780251,21.1782418267264,
19.544814205538));
#136583=CARTESIAN_POINT('Ctrl Pts',(-20.3075324892011,21.2320561249956,
19.5489897694722));
#136584=CARTESIAN_POINT('Ctrl Pts',(-20.2402996648593,21.2826438810762,
19.5531653334064));
#136585=CARTESIAN_POINT('Ctrl Pts',(-20.1708219662268,21.329759693162,19.5573408973406));
#136586=CARTESIAN_POINT('Ctrl Pts',(-20.0978350996175,21.3792552228008,
19.5617273599593));
#136587=CARTESIAN_POINT('Ctrl Pts',(-20.0223711202591,21.4249185513468,
19.566113822578));
#136588=CARTESIAN_POINT('Ctrl Pts',(-19.9448802161397,21.4665196966911,
19.5705002851967));
#136589=CARTESIAN_POINT('Ctrl Pts',(-19.8673893120203,21.5081208420354,
19.5748867478154));
#136590=CARTESIAN_POINT('Ctrl Pts',(-19.7878720403016,21.5456596252664,
19.579273210434));
#136591=CARTESIAN_POINT('Ctrl Pts',(-19.7068005673304,21.5789651720837,
19.5836596730527));
#136592=CARTESIAN_POINT('Ctrl Pts',(-19.629459322931,21.6107382772446,19.5878443074871));
#136593=CARTESIAN_POINT('Ctrl Pts',(-19.5504158778411,21.6387774071505,
19.5920289419215));
#136594=CARTESIAN_POINT('Ctrl Pts',(-19.4700654949587,21.6628987717953,
19.5962135763559));
#136595=CARTESIAN_POINT('Ctrl Pts',(-19.3898294809474,21.6869858026491,
19.6003922544787));
#136596=CARTESIAN_POINT('Ctrl Pts',(-19.3082906610537,21.7071660136986,
19.6045709326015));
#136597=CARTESIAN_POINT('Ctrl Pts',(-19.2258642779018,21.7233036305598,
19.6087496107243));
#136598=CARTESIAN_POINT('Ctrl Pts',(-19.1419604620487,21.7397305024139,
19.6130031885997));
#136599=CARTESIAN_POINT('Ctrl Pts',(-19.0571373968166,21.7519682444677,
19.6172567664751));
#136600=CARTESIAN_POINT('Ctrl Pts',(-18.9718493062277,21.7599267756307,
19.6215103443505));
#136601=CARTESIAN_POINT('Ctrl Pts',(-18.8882146908505,21.7677310152166,
19.6256814583611));
#136602=CARTESIAN_POINT('Ctrl Pts',(-18.8041333991885,21.7714204401683,
19.6298525723716));
#136603=CARTESIAN_POINT('Ctrl Pts',(-18.7200422944287,21.7709619494155,
19.6340236863821));
#136604=CARTESIAN_POINT('Ctrl Pts',(-18.6359794072993,21.7705036125139,
19.6381934007327));
#136605=CARTESIAN_POINT('Ctrl Pts',(-18.551907173255,21.7659001267009,19.6423631150832));
#136606=CARTESIAN_POINT('Ctrl Pts',(-18.4682635936743,21.7571704896477,
19.6465328294338));
#136607=CARTESIAN_POINT('Ctrl Pts',(-18.3846229905396,21.7484411632376,
19.6507023954056));
#136608=CARTESIAN_POINT('Ctrl Pts',(-18.3014114689995,21.7355860261208,
19.6548719613774));
#136609=CARTESIAN_POINT('Ctrl Pts',(-18.2190616739018,21.7186759201131,
19.6590415273492));
#136610=CARTESIAN_POINT('Ctrl Pts',(-18.1338165629591,21.7011712759185,
19.663357690048));
#136611=CARTESIAN_POINT('Ctrl Pts',(-18.0494954191338,21.679321318249,19.6676738527467));
#136612=CARTESIAN_POINT('Ctrl Pts',(-17.966564411757,21.6532617832448,19.6719900154455));
#136613=CARTESIAN_POINT('Ctrl Pts',(-17.8863348720621,21.6280511344877,
19.6761655796587));
#136614=CARTESIAN_POINT('Ctrl Pts',(-17.8074067178008,21.5989011580654,
19.6803411438719));
#136615=CARTESIAN_POINT('Ctrl Pts',(-17.7301828112741,21.5659842996543,
19.6845167080851));
#136616=CARTESIAN_POINT('Ctrl Pts',(-17.6490585105433,21.5314048897156,
19.6889031700266));
#136617=CARTESIAN_POINT('Ctrl Pts',(-17.5698156696645,21.4926683234483,
19.6932896319682));
#136618=CARTESIAN_POINT('Ctrl Pts',(-17.492891345209,21.4500286525641,19.6976760939097));
#136619=CARTESIAN_POINT('Ctrl Pts',(-17.4159670207535,21.4073889816798,
19.7020625558512));
#136620=CARTESIAN_POINT('Ctrl Pts',(-17.341361664738,21.3608465778214,19.7064490177927));
#136621=CARTESIAN_POINT('Ctrl Pts',(-17.2694745299336,21.3107059669218,
19.7108354797342));
#136622=CARTESIAN_POINT('Ctrl Pts',(-17.2008950125853,21.2628723885714,
19.7150201150467));
#136623=CARTESIAN_POINT('Ctrl Pts',(-17.1345338099885,21.2115863975994,
19.7192047503592));
#136624=CARTESIAN_POINT('Ctrl Pts',(-17.0707594088287,21.1570808657093,
19.7233893856716));
#136625=CARTESIAN_POINT('Ctrl Pts',(-17.0070757825499,21.1026529156246,
19.7275680646793));
#136626=CARTESIAN_POINT('Ctrl Pts',(-16.945971990841,21.0450148234629,19.731746743687));
#136627=CARTESIAN_POINT('Ctrl Pts',(-16.8877869614792,20.9844422506514,
19.7359254226946));
#136628=CARTESIAN_POINT('Ctrl Pts',(-16.8285590235835,20.9227839749746,
19.7401790003497));
#136629=CARTESIAN_POINT('Ctrl Pts',(-16.7723559086582,20.8580852602608,
19.7444325780047));
#136630=CARTESIAN_POINT('Ctrl Pts',(-16.719499223283,20.790679277767,19.7486861556597));
#136631=CARTESIAN_POINT('Ctrl Pts',(-16.6676672535619,20.7245800734972,
19.7528572705652));
#136632=CARTESIAN_POINT('Ctrl Pts',(-16.6190534158838,20.6558780132752,
19.7570283854707));
#136633=CARTESIAN_POINT('Ctrl Pts',(-16.5739220088091,20.5849225130889,
19.7611995003762));
#136634=CARTESIAN_POINT('Ctrl Pts',(-16.528805746017,20.5139908227108,19.7653692156234));
#136635=CARTESIAN_POINT('Ctrl Pts',(-16.4871698397316,20.440807581965,19.7695389308707));
#136636=CARTESIAN_POINT('Ctrl Pts',(-16.4492353977934,20.3657513639325,
19.773708646118));
#136637=CARTESIAN_POINT('Ctrl Pts',(-16.4113023057417,20.2906978167542,
19.7778782129872));
#136638=CARTESIAN_POINT('Ctrl Pts',(-16.3770706229015,20.2137718357625,
19.7820477798563));
#136639=CARTESIAN_POINT('Ctrl Pts',(-16.3467149650018,20.1353755522913,
19.7862173467255));
#136640=CARTESIAN_POINT('Ctrl Pts',(-16.3152920545844,20.054222990857,19.7905335083663));
#136641=CARTESIAN_POINT('Ctrl Pts',(-16.2880229889401,19.9714953049146,
19.7948496700072));
#136642=CARTESIAN_POINT('Ctrl Pts',(-16.2650459639335,19.8876579400192,
19.799165831648));
#136643=CARTESIAN_POINT('Ctrl Pts',(-16.242817402594,19.806551530134,19.8033413967509));
#136644=CARTESIAN_POINT('Ctrl Pts',(-16.224605609274,19.7244070957626,19.8075169618538));
#136645=CARTESIAN_POINT('Ctrl Pts',(-16.2104836462314,19.6416567220678,
19.8116925269566));
#136646=CARTESIAN_POINT('Ctrl Pts',(-16.195648426756,19.5547268843585,19.8160789868665));
#136647=CARTESIAN_POINT('Ctrl Pts',(-16.185327112135,19.4671288674576,19.8204654467763));
#136648=CARTESIAN_POINT('Ctrl Pts',(-16.1795426555597,19.3793676793066,
19.8248519066861));
#136649=CARTESIAN_POINT('Ctrl Pts',(-16.1737581989845,19.2916064911556,
19.829238366596));
#136650=CARTESIAN_POINT('Ctrl Pts',(-16.172510532631,19.20368271299,19.8336248265058));
#136651=CARTESIAN_POINT('Ctrl Pts',(-16.1757597065464,19.1160968865085,
19.8380112864156));
#136652=CARTESIAN_POINT('Ctrl Pts',(-16.1788596427718,19.0325339614677,
19.8421962719934));
#136653=CARTESIAN_POINT('Ctrl Pts',(-16.1860639312761,18.9489675605742,
19.8463812575711));
#136654=CARTESIAN_POINT('Ctrl Pts',(-16.1973762177222,18.8658336818538,
19.8505662431489));
#136655=CARTESIAN_POINT('Ctrl Pts',(-16.2086691571991,18.7828419838145,
19.8547440713065));
#136656=CARTESIAN_POINT('Ctrl Pts',(-16.2240560628308,18.7002817889827,
19.858921899464));
#136657=CARTESIAN_POINT('Ctrl Pts',(-16.2434886327822,18.6185870276919,
19.8630997276216));
#136658=CARTESIAN_POINT('Ctrl Pts',(-16.262902292549,18.5369717650481,19.8672734902592));
#136659=CARTESIAN_POINT('Ctrl Pts',(-16.2863536948447,18.4562207088556,
19.8714472528968));
#136660=CARTESIAN_POINT('Ctrl Pts',(-16.3137431279862,18.3767598226709,
19.8756210155344));
#136661=CARTESIAN_POINT('Ctrl Pts',(-16.3411141250046,18.2973524224668,
19.8797919687673));
#136662=CARTESIAN_POINT('Ctrl Pts',(-16.3724177390461,18.2192339011836,
19.8839629220001));
#136663=CARTESIAN_POINT('Ctrl Pts',(-16.4075041946845,18.1428159017055,
19.888133875233));
#136664=CARTESIAN_POINT('Ctrl Pts',(-16.4425775587027,18.0664264156637,
19.8923032721806));
#136665=CARTESIAN_POINT('Ctrl Pts',(-16.4814307675656,17.991736608042,19.8964726691282));
#136666=CARTESIAN_POINT('Ctrl Pts',(-16.5238661307731,17.9191376698363,
19.9006420660758));
#136667=CARTESIAN_POINT('Ctrl Pts',(-16.566318136594,17.8465102592441,19.9048130982082));
#136668=CARTESIAN_POINT('Ctrl Pts',(-16.6123548789664,17.775975758528,19.9089841303406));
#136669=CARTESIAN_POINT('Ctrl Pts',(-16.6617333188454,17.7078996034276,
19.913155162473));
#136670=CARTESIAN_POINT('Ctrl Pts',(-16.7111193623267,17.6398129655331,
19.9173268368871));
#136671=CARTESIAN_POINT('Ctrl Pts',(-16.7638478477789,17.5741857926268,
19.9214985113013));
#136672=CARTESIAN_POINT('Ctrl Pts',(-16.8196343586719,17.51135174483,19.9256701857154));
#136673=CARTESIAN_POINT('Ctrl Pts',(-16.875489508745,17.4484403866323,19.9298469929171));
#136674=CARTESIAN_POINT('Ctrl Pts',(-16.9344098861507,17.3883293561259,
19.9340238001189));
#136675=CARTESIAN_POINT('Ctrl Pts',(-16.9960732542543,17.3313163493764,
19.9382006073206));
#136676=CARTESIAN_POINT('Ctrl Pts',(-17.0532712339288,17.2784319724516,
19.9420749486156));
#136677=CARTESIAN_POINT('Ctrl Pts',(-17.1128287126708,17.2282129651311,
19.9459492899105));
#136678=CARTESIAN_POINT('Ctrl Pts',(-17.174464231106,17.180864983421,19.9498236312055));
#136679=CARTESIAN_POINT('Ctrl Pts',(-17.1767158295569,17.1837658568561,
19.1498287197874));
#136680=CARTESIAN_POINT('Ctrl Pts',(-17.4546313077574,16.9682013031296,
19.1672632308611));
#136681=CARTESIAN_POINT('Ctrl Pts',(-18.5512406904231,16.4174579447905,
19.2270896774953));
#136682=CARTESIAN_POINT('Ctrl Pts',(-20.635918474416,16.9602241188658,19.3215765970806));
#136683=CARTESIAN_POINT('Ctrl Pts',(-21.2889869220882,18.5174131978834,
19.3986290055925));
#136684=CARTESIAN_POINT('Ctrl Pts',(-21.2953149015357,19.2131844541912,
19.4332894785437));
#136685=CARTESIAN_POINT('',(-21.2939989850552,19.2087204131754,19.3667098901939));
#136686=CARTESIAN_POINT('Ctrl Pts',(-17.174464231106,17.180864983421,19.083343695997));
#136687=CARTESIAN_POINT('Ctrl Pts',(-17.2408453266491,17.1298714819877,
19.0875248509024));
#136688=CARTESIAN_POINT('Ctrl Pts',(-17.3098397832821,17.0820529442478,
19.0917060058077));
#136689=CARTESIAN_POINT('Ctrl Pts',(-17.3811106246903,17.037686783233,19.0958871607131));
#136690=CARTESIAN_POINT('Ctrl Pts',(-17.452293133591,16.9933756092813,19.1000631335287));
#136691=CARTESIAN_POINT('Ctrl Pts',(-17.5257460343461,16.9525085530914,
19.1042391063443));
#136692=CARTESIAN_POINT('Ctrl Pts',(-17.6011010651429,16.9153214503334,
19.1084150791599));
#136693=CARTESIAN_POINT('Ctrl Pts',(-17.6763878065308,16.8781680478504,
19.1125872675604));
#136694=CARTESIAN_POINT('Ctrl Pts',(-17.7535728413456,16.8446881742378,
19.1167594559609));
#136695=CARTESIAN_POINT('Ctrl Pts',(-17.832261991049,16.8150725046001,19.1209316443614));
#136696=CARTESIAN_POINT('Ctrl Pts',(-17.9109137869838,16.7854708935318,
19.1251018522225));
#136697=CARTESIAN_POINT('Ctrl Pts',(-17.9910678502179,16.7597300059441,
19.1292720600837));
#136698=CARTESIAN_POINT('Ctrl Pts',(-18.0723097397469,16.7379925193227,
19.1334422679448));
#136699=CARTESIAN_POINT('Ctrl Pts',(-18.153537434481,16.7162588307316,19.1376117471763));
#136700=CARTESIAN_POINT('Ctrl Pts',(-18.2358521335503,16.6985272720948,
19.1417812264079));
#136701=CARTESIAN_POINT('Ctrl Pts',(-18.318825260664,16.6848903555433,19.1459507056394));
#136702=CARTESIAN_POINT('Ctrl Pts',(-18.401808780157,16.6712517309688,19.1501207070979));
#136703=CARTESIAN_POINT('Ctrl Pts',(-18.4854504373051,16.6617088401247,
19.1542907085565));
#136704=CARTESIAN_POINT('Ctrl Pts',(-18.5693138750506,16.6563026636705,
19.1584607100151));
#136705=CARTESIAN_POINT('Ctrl Pts',(-18.6532675334726,16.6508906712265,
19.1626351975806));
#136706=CARTESIAN_POINT('Ctrl Pts',(-18.737442988877,16.6496243068331,19.1668096851461));
#136707=CARTESIAN_POINT('Ctrl Pts',(-18.8214017259729,16.6524924392731,
19.1709841727116));
#136708=CARTESIAN_POINT('Ctrl Pts',(-18.9054095853483,16.6553622497897,
19.1751611026715));
#136709=CARTESIAN_POINT('Ctrl Pts',(-18.9892000156136,16.6623713344674,
19.1793380326314));
#136710=CARTESIAN_POINT('Ctrl Pts',(-19.0723398854136,16.67345667585,19.1835149625913));
#136711=CARTESIAN_POINT('Ctrl Pts',(-19.1556201623819,16.6845607382313,
19.1876989465784));
#136712=CARTESIAN_POINT('Ctrl Pts',(-19.2382472329086,16.6997547190923,
19.1918829305655));
#136713=CARTESIAN_POINT('Ctrl Pts',(-19.31979874243,16.7189245931619,19.1960669145527));
#136714=CARTESIAN_POINT('Ctrl Pts',(-19.3683964965226,16.7303482054467,
19.1985602126673));
#136715=CARTESIAN_POINT('Ctrl Pts',(-19.4166125841186,16.7431827530992,
19.2010535107819));
#136716=CARTESIAN_POINT('Ctrl Pts',(-19.4643607861717,16.7573958913422,
19.2035468088965));
#136717=CARTESIAN_POINT('Ctrl Pts',(-19.5444991251657,16.7812505547997,
19.2077314433106));
#136718=CARTESIAN_POINT('Ctrl Pts',(-19.623616676388,16.8090798944626,19.2119160777247));
#136719=CARTESIAN_POINT('Ctrl Pts',(-19.7012904347964,16.8407786570129,
19.2161007121388));
#136720=CARTESIAN_POINT('Ctrl Pts',(-19.7788536342256,16.8724323002991,
19.2202793902439));
#136721=CARTESIAN_POINT('Ctrl Pts',(-19.8549767005509,16.907944254222,19.224458068349));
#136722=CARTESIAN_POINT('Ctrl Pts',(-19.9292512406659,16.9471593537339,
19.228636746454));
#136723=CARTESIAN_POINT('Ctrl Pts',(-20.0048570980567,16.98707735547,19.2328903243342));
#136724=CARTESIAN_POINT('Ctrl Pts',(-20.0785470456703,17.0308324287623,
19.2371439022144));
#136725=CARTESIAN_POINT('Ctrl Pts',(-20.1499110578951,17.0782093688948,
19.2413974800945));
#136726=CARTESIAN_POINT('Ctrl Pts',(-20.2198915399285,17.124667814887,19.2455685940936));
#136727=CARTESIAN_POINT('Ctrl Pts',(-20.2876350664231,17.1746086809012,
19.2497397080927));
#136728=CARTESIAN_POINT('Ctrl Pts',(-20.3527809100898,17.2277833287488,
19.2539108220917));
#136729=CARTESIAN_POINT('Ctrl Pts',(-20.4179048934389,17.2809401333293,
19.2580805364332));
#136730=CARTESIAN_POINT('Ctrl Pts',(-20.4804325690375,17.337328274011,19.2622502507746));
#136731=CARTESIAN_POINT('Ctrl Pts',(-20.5400350473179,17.3966578581041,
19.2664199651161));
#136732=CARTESIAN_POINT('Ctrl Pts',(-20.5996354046852,17.455985330995,19.2705895310811));
#136733=CARTESIAN_POINT('Ctrl Pts',(-20.6563104462575,17.5182537140389,
19.2747590970462));
#136734=CARTESIAN_POINT('Ctrl Pts',(-20.7097680140135,17.58313613751,19.2789286630112));
#136735=CARTESIAN_POINT('Ctrl Pts',(-20.7651050833054,17.6502997462216,
19.2832448257251));
#136736=CARTESIAN_POINT('Ctrl Pts',(-20.8169938810693,17.7202642276976,
19.287560988439));
#136737=CARTESIAN_POINT('Ctrl Pts',(-20.865156923198,17.7926311591461,19.2918771511529));
#136738=CARTESIAN_POINT('Ctrl Pts',(-20.9117510597953,17.8626407461657,
19.2960527153652));
#136739=CARTESIAN_POINT('Ctrl Pts',(-20.9548582452776,17.9348982385166,
19.3002282795775));
#136740=CARTESIAN_POINT('Ctrl Pts',(-20.9942733140223,18.0090164119595,
19.3044038437898));
#136741=CARTESIAN_POINT('Ctrl Pts',(-21.0356791435329,18.0868781169103,
19.3087903057545));
#136742=CARTESIAN_POINT('Ctrl Pts',(-21.073009829653,18.1667928797188,19.3131767677192));
#136743=CARTESIAN_POINT('Ctrl Pts',(-21.106084856171,18.248288498498,19.3175632296839));
#136744=CARTESIAN_POINT('Ctrl Pts',(-21.1391598826889,18.3297841172771,
19.3219496916486));
#136745=CARTESIAN_POINT('Ctrl Pts',(-21.1679791313068,18.4128600189273,
19.3263361536133));
#136746=CARTESIAN_POINT('Ctrl Pts',(-21.1924232051052,18.4970284707355,
19.330722615578));
#136747=CARTESIAN_POINT('Ctrl Pts',(-21.2214742546483,18.5970601546363,
19.3359357942367));
#136748=CARTESIAN_POINT('Ctrl Pts',(-21.2444357643533,18.6989346521836,
19.3411489728953));
#136749=CARTESIAN_POINT('Ctrl Pts',(-21.2611151500594,18.8019901977457,
19.3463621515539));
#136750=CARTESIAN_POINT('Ctrl Pts',(-21.2775287210165,18.9034033756297,
19.3514922492285));
#136751=CARTESIAN_POINT('Ctrl Pts',(-21.2878587863005,19.0059603454814,
19.3566223469032));
#136752=CARTESIAN_POINT('Ctrl Pts',(-21.2919675308107,19.1090092586637,
19.3617524445778));
#136753=CARTESIAN_POINT('Ctrl Pts',(-21.2932910194166,19.1422028685647,
19.3634049264499));
#136754=CARTESIAN_POINT('Ctrl Pts',(-21.2939693565913,19.1754473495009,
19.3650574083219));
#136755=CARTESIAN_POINT('Ctrl Pts',(-21.2939989850552,19.2087204131754,
19.3667098901939));
#136756=CARTESIAN_POINT('Ctrl Pts',(-21.2939989850559,19.2087204138716,
19.3667098902285));
#136757=CARTESIAN_POINT('Ctrl Pts',(-21.294073180434,19.292042596975,19.3708480242597));
#136758=CARTESIAN_POINT('Ctrl Pts',(-21.2900751830218,19.3754486069202,
19.374986158291));
#136759=CARTESIAN_POINT('Ctrl Pts',(-21.2820071809338,19.4585063754929,
19.3791242923222));
#136760=CARTESIAN_POINT('Ctrl Pts',(-21.2739428344705,19.541526510458,19.3832605513583));
#136761=CARTESIAN_POINT('Ctrl Pts',(-21.2618121886757,19.6241982519104,
19.3873968103944));
#136762=CARTESIAN_POINT('Ctrl Pts',(-21.2456694473256,19.7060925038528,
19.3915330694305));
#136763=CARTESIAN_POINT('Ctrl Pts',(-21.2295289836483,19.7879752008609,
19.3956687448579));
#136764=CARTESIAN_POINT('Ctrl Pts',(-21.2093776397595,19.8690801670299,
19.3998044202852));
#136765=CARTESIAN_POINT('Ctrl Pts',(-21.1853208566118,19.9489878440326,
19.4039400957126));
#136766=CARTESIAN_POINT('Ctrl Pts',(-21.1612599617805,20.0289091785175,
19.4080764779921));
#136767=CARTESIAN_POINT('Ctrl Pts',(-21.1332924395122,20.1076323699233,
19.4122128602716));
#136768=CARTESIAN_POINT('Ctrl Pts',(-21.1015733410929,20.1847538059213,
19.4163492425511));
#136769=CARTESIAN_POINT('Ctrl Pts',(-21.0698191717518,20.2619605129384,
19.420490198313));
#136770=CARTESIAN_POINT('Ctrl Pts',(-21.0343053289548,20.3375614976483,
19.4246311540749));
#136771=CARTESIAN_POINT('Ctrl Pts',(-20.9952344193577,20.4111745292715,
19.4287721098369));
#136772=CARTESIAN_POINT('Ctrl Pts',(-20.956138222721,20.4848352039023,19.4329157456621));
#136773=CARTESIAN_POINT('Ctrl Pts',(-20.9134806196,20.5565049647657,19.4370593814874));
#136774=CARTESIAN_POINT('Ctrl Pts',(-20.8675081508492,20.6258296612172,
19.4412030173127));
#136775=CARTESIAN_POINT('Ctrl Pts',(-20.8214607545843,20.6952673454484,
19.4453534065784));
#136776=CARTESIAN_POINT('Ctrl Pts',(-20.7720879921639,20.7623519651645,
19.4495037958442));
#136777=CARTESIAN_POINT('Ctrl Pts',(-20.7196769297106,20.8267620897939,
19.4536541851099));
#136778=CARTESIAN_POINT('Ctrl Pts',(-20.701811538935,20.8487176082006,19.4550689308264));
#136779=CARTESIAN_POINT('Ctrl Pts',(-20.6835934338612,20.8703626873999,
19.456483676543));
#136780=CARTESIAN_POINT('Ctrl Pts',(-20.665034920053,20.8916856153177,19.4578984222595));
#136781=CARTESIAN_POINT('Ctrl Pts',(-20.6101412425939,20.9547560712659,
19.4620830566462));
#136782=CARTESIAN_POINT('Ctrl Pts',(-20.5520521994161,21.0152517076034,
19.466267691033));
#136783=CARTESIAN_POINT('Ctrl Pts',(-20.4910387353968,21.0728310563301,
19.4704523254197));
#136784=CARTESIAN_POINT('Ctrl Pts',(-20.4301121164969,21.1303284479757,
19.474631003497));
#136785=CARTESIAN_POINT('Ctrl Pts',(-20.3662696766025,21.1849174841126,
19.4788096815743));
#136786=CARTESIAN_POINT('Ctrl Pts',(-20.2998217436364,21.2362906623878,
19.4829883596516));
#136787=CARTESIAN_POINT('Ctrl Pts',(-20.2321827790938,21.2885846680655,
19.4872419375387));
#136788=CARTESIAN_POINT('Ctrl Pts',(-20.161844312329,21.3375460297091,19.4914955154257));
#136789=CARTESIAN_POINT('Ctrl Pts',(-20.0891719990913,21.3828906171534,
19.4957490933128));
#136790=CARTESIAN_POINT('Ctrl Pts',(-20.0179085806091,21.4273561111906,
19.4999202072832));
#136791=CARTESIAN_POINT('Ctrl Pts',(-19.9444014087256,21.4683435613089,
19.5040913212537));
#136792=CARTESIAN_POINT('Ctrl Pts',(-19.8690261614781,21.5056275542581,
19.5082624352241));
#136793=CARTESIAN_POINT('Ctrl Pts',(-19.793676207128,21.5428990362007,19.5124321495367));
#136794=CARTESIAN_POINT('Ctrl Pts',(-19.7164598343519,21.5764693252628,
19.5166018638493));
#136795=CARTESIAN_POINT('Ctrl Pts',(-19.6377770918877,21.6061590694939,
19.5207715781619));
#136796=CARTESIAN_POINT('Ctrl Pts',(-19.5590971492983,21.6358477572345,
19.5249411440979));
#136797=CARTESIAN_POINT('Ctrl Pts',(-19.4789513714795,21.6616560130841,
19.5291107100339));
#136798=CARTESIAN_POINT('Ctrl Pts',(-19.3977582580605,21.6834532300645,
19.5332802759699));
#136799=CARTESIAN_POINT('Ctrl Pts',(-19.313710494605,21.706016810393,19.5375964387175));
#136800=CARTESIAN_POINT('Ctrl Pts',(-19.2285408859855,21.7242819108903,
19.541912601465));
#136801=CARTESIAN_POINT('Ctrl Pts',(-19.1427269885521,21.7381609067942,
19.5462287642126));
#136802=CARTESIAN_POINT('Ctrl Pts',(-19.0597084701407,21.7515877958115,
19.5504043283956));
#136803=CARTESIAN_POINT('Ctrl Pts',(-18.9760874671013,21.7609099414407,
19.5545798925786));
#136804=CARTESIAN_POINT('Ctrl Pts',(-18.8923014001317,21.7661009112589,
19.5587554567616));
#136805=CARTESIAN_POINT('Ctrl Pts',(-18.8042834975712,21.7715540646552,
19.5631419187915));
#136806=CARTESIAN_POINT('Ctrl Pts',(-18.716084001952,21.7724477372194,19.5675283808214));
#136807=CARTESIAN_POINT('Ctrl Pts',(-18.6282074804569,21.7688131172564,
19.5719148428513));
#136808=CARTESIAN_POINT('Ctrl Pts',(-18.5403309589617,21.7651784972933,
19.5763013048811));
#136809=CARTESIAN_POINT('Ctrl Pts',(-18.4527779822413,21.7570157144011,
19.580687766911));
#136810=CARTESIAN_POINT('Ctrl Pts',(-18.3660419494175,21.7444180217665,
19.5850742289409));
#136811=CARTESIAN_POINT('Ctrl Pts',(-18.2832967675751,21.7323999672867,
19.589258863475));
#136812=CARTESIAN_POINT('Ctrl Pts',(-18.2009870108079,21.7163014146079,
19.5934434980091));
#136813=CARTESIAN_POINT('Ctrl Pts',(-18.1195464570135,21.696165355366,19.5976281325432));
#136814=CARTESIAN_POINT('Ctrl Pts',(-18.0382218237528,21.6760579573085,
19.6018068107688));
#136815=CARTESIAN_POINT('Ctrl Pts',(-17.9577643787564,21.651924577293,19.6059854889943));
#136816=CARTESIAN_POINT('Ctrl Pts',(-17.8786006574804,21.6238597068245,
19.6101641672199));
#136817=CARTESIAN_POINT('Ctrl Pts',(-17.7980179867947,21.595291794928,19.61441774507));
#136818=CARTESIAN_POINT('Ctrl Pts',(-17.7187763530359,21.5626501319716,
19.6186713229201));
#136819=CARTESIAN_POINT('Ctrl Pts',(-17.6413125871929,21.526088382307,19.6229249007702));
#136820=CARTESIAN_POINT('Ctrl Pts',(-17.565350604394,21.4902354519867,19.62709601489));
#136821=CARTESIAN_POINT('Ctrl Pts',(-17.4910986051224,21.4506132807032,
19.6312671290099));
#136822=CARTESIAN_POINT('Ctrl Pts',(-17.4189494736645,21.4074157423367,
19.6354382431297));
#136823=CARTESIAN_POINT('Ctrl Pts',(-17.346824552547,21.364232699323,19.6396079575918));
#136824=CARTESIAN_POINT('Ctrl Pts',(-17.2768014922038,21.3174769080653,
19.6437776720538));
#136825=CARTESIAN_POINT('Ctrl Pts',(-17.2092476380545,21.2673876664533,
19.6479473865159));
#136826=CARTESIAN_POINT('Ctrl Pts',(-17.1416961877673,21.2173002072362,
19.6521169526012));
#136827=CARTESIAN_POINT('Ctrl Pts',(-17.0766141380014,21.1638798081924,
19.6562865186866));
#136828=CARTESIAN_POINT('Ctrl Pts',(-17.0143378344858,21.1074076662202,
19.6604560847719));
#136829=CARTESIAN_POINT('Ctrl Pts',(-16.9498719776595,21.0489500376595,
19.6647722473428));
#136830=CARTESIAN_POINT('Ctrl Pts',(-16.8884132283835,20.987222429568,19.6690884099137));
#136831=CARTESIAN_POINT('Ctrl Pts',(-16.8302937573553,20.9225789615778,
19.6734045724845));
#136832=CARTESIAN_POINT('Ctrl Pts',(-16.7740675179232,20.8600412432427,
19.6775801368151));
#136833=CARTESIAN_POINT('Ctrl Pts',(-16.7209666048,20.794775110764,19.6817557011457));
#136834=CARTESIAN_POINT('Ctrl Pts',(-16.6712500110187,20.7271340583726,
19.6859312654763));
#136835=CARTESIAN_POINT('Ctrl Pts',(-16.6190223558411,20.6560766247986,
19.6903177271673));
#136836=CARTESIAN_POINT('Ctrl Pts',(-16.5705302090253,20.5823985401207,
19.6947041888583));
#136837=CARTESIAN_POINT('Ctrl Pts',(-16.5260204587339,20.5065409469987,
19.6990906505493));
#136838=CARTESIAN_POINT('Ctrl Pts',(-16.4815107084424,20.4306833538766,
19.7034771122403));
#136839=CARTESIAN_POINT('Ctrl Pts',(-16.4409835545861,20.3526468022858,
19.7078635739313));
#136840=CARTESIAN_POINT('Ctrl Pts',(-16.4046276535517,20.2728966388503,
19.7122500356223));
#136841=CARTESIAN_POINT('Ctrl Pts',(-16.3699445411192,20.1968158980013,
19.7164346697444));
#136842=CARTESIAN_POINT('Ctrl Pts',(-16.3389281684758,20.1188925846309,
19.7206193038666));
#136843=CARTESIAN_POINT('Ctrl Pts',(-16.3117771822155,20.0395147077777,
19.7248039379887));
#136844=CARTESIAN_POINT('Ctrl Pts',(-16.2846648420245,19.96024981551,19.728982615802));
#136845=CARTESIAN_POINT('Ctrl Pts',(-16.2614071073245,19.8795349037591,
19.7331612936152));
#136846=CARTESIAN_POINT('Ctrl Pts',(-16.2421554012761,19.7977797677242,
19.7373399714285));
#136847=CARTESIAN_POINT('Ctrl Pts',(-16.2225586206514,19.7145592229168,
19.7415935493816));
#136848=CARTESIAN_POINT('Ctrl Pts',(-16.2071130980708,19.6302612335118,
19.7458471273348));
#136849=CARTESIAN_POINT('Ctrl Pts',(-16.1959260745095,19.5453362809289,
19.7501007052879));
#136850=CARTESIAN_POINT('Ctrl Pts',(-16.1849559341096,19.462057770949,19.7542718189977));
#136851=CARTESIAN_POINT('Ctrl Pts',(-16.1780807097821,19.3781768678583,
19.7584429327075));
#136852=CARTESIAN_POINT('Ctrl Pts',(-16.175350045093,19.294128865351,19.7626140464172));
#136853=CARTESIAN_POINT('Ctrl Pts',(-16.172620296704,19.2101090659342,19.766783760471));
#136854=CARTESIAN_POINT('Ctrl Pts',(-16.1740323608365,19.125922737868,19.7709534745247));
#136855=CARTESIAN_POINT('Ctrl Pts',(-16.1795838629489,19.0420082878573,
19.7751231885784));
#136856=CARTESIAN_POINT('Ctrl Pts',(-16.1851351675175,18.9580968238458,
19.7792927542576));
#136857=CARTESIAN_POINT('Ctrl Pts',(-16.1948255859832,18.8744576776277,
19.7834623199368));
#136858=CARTESIAN_POINT('Ctrl Pts',(-16.2086007338245,18.7915258692123,
19.787631885616));
#136859=CARTESIAN_POINT('Ctrl Pts',(-16.2228602008279,18.7056782689351,
19.7919480486733));
#136860=CARTESIAN_POINT('Ctrl Pts',(-16.2414968944959,18.6205891924188,
19.7962642117307));
#136861=CARTESIAN_POINT('Ctrl Pts',(-16.2643928538834,18.5367296211091,
19.800580374788));
#136862=CARTESIAN_POINT('Ctrl Pts',(-16.2865429768018,18.4556017775032,
19.8047559387221));
#136863=CARTESIAN_POINT('Ctrl Pts',(-16.312678943375,18.3756249997159,19.8089315026562));
#136864=CARTESIAN_POINT('Ctrl Pts',(-16.3426437089087,18.2972083995474,
19.8131070665903));
#136865=CARTESIAN_POINT('Ctrl Pts',(-16.3741219298082,18.2148311468531,
19.8174935292092));
#136866=CARTESIAN_POINT('Ctrl Pts',(-16.4098256651864,18.1341763575637,
19.8218799918281));
#136867=CARTESIAN_POINT('Ctrl Pts',(-16.4495176195312,18.0556904080171,
19.826266454447));
#136868=CARTESIAN_POINT('Ctrl Pts',(-16.4892095738761,17.9772044584704,
19.830652917066));
#136869=CARTESIAN_POINT('Ctrl Pts',(-16.5328893929524,17.9008878144519,
19.8350393796849));
#136870=CARTESIAN_POINT('Ctrl Pts',(-16.5802679097329,17.8271509896836,
19.8394258423038));
#136871=CARTESIAN_POINT('Ctrl Pts',(-16.6254567089839,17.7568220980618,
19.8436095735005));
#136872=CARTESIAN_POINT('Ctrl Pts',(-16.6741780301137,17.6885781039117,
19.8477933046972));
#136873=CARTESIAN_POINT('Ctrl Pts',(-16.7262132891215,17.6227958180323,
19.8519770358939));
#136874=CARTESIAN_POINT('Ctrl Pts',(-16.7781836605484,17.5570955621741,
19.8561555500089));
#136875=CARTESIAN_POINT('Ctrl Pts',(-16.8334594864223,17.4938512802374,
19.8603340641239));
#136876=CARTESIAN_POINT('Ctrl Pts',(-16.8917781973556,17.43341207535,19.8645125782389));
#136877=CARTESIAN_POINT('Ctrl Pts',(-16.9500311212107,17.3730410495877,
19.8686863787341));
#136878=CARTESIAN_POINT('Ctrl Pts',(-17.0113197908349,17.3154691416354,
19.8728601792292));
#136879=CARTESIAN_POINT('Ctrl Pts',(-17.0753415571247,17.2610122641723,
19.8770339797244));
#136880=CARTESIAN_POINT('Ctrl Pts',(-17.1076991478945,17.2334889161351,
19.8791434830418));
#136881=CARTESIAN_POINT('Ctrl Pts',(-17.1407542697565,17.206760744079,19.8812529863593));
#136882=CARTESIAN_POINT('Ctrl Pts',(-17.174464231106,17.180864983421,19.8833624896767));
#136883=CARTESIAN_POINT('Origin',(-18.734,19.211,-1.76670989022852));
#136884=CARTESIAN_POINT('',(-17.174464231106,17.180864983421,20.7499611441365));
#136885=CARTESIAN_POINT('',(-17.1763037726969,17.1832235620119,20.6832232089404));
#136886=CARTESIAN_POINT('',(-17.174464231106,17.180864983421,-1.76670989022852));
#136887=CARTESIAN_POINT('',(-21.2939995273706,19.2094444092821,20.2332901098006));
#136888=CARTESIAN_POINT('Ctrl Pts',(-21.2939995273706,19.209444409282,20.2332901098006));
#136889=CARTESIAN_POINT('Ctrl Pts',(-21.2940497238898,19.292051655634,20.2374173417521));
#136890=CARTESIAN_POINT('Ctrl Pts',(-21.2900972916445,19.3748187808655,
20.2415445737036));
#136891=CARTESIAN_POINT('Ctrl Pts',(-21.2821221995875,19.4573194185792,
20.2456718056551));
#136892=CARTESIAN_POINT('Ctrl Pts',(-21.2739869560054,19.5414767898907,
20.249881918467));
#136893=CARTESIAN_POINT('Ctrl Pts',(-21.2616656478282,19.6253563615795,
20.254092031279));
#136894=CARTESIAN_POINT('Ctrl Pts',(-21.2451929662144,19.7085036546953,
20.2583021440909));
#136895=CARTESIAN_POINT('Ctrl Pts',(-21.2290800677258,19.7898349111956,
20.262420302989));
#136896=CARTESIAN_POINT('Ctrl Pts',(-21.2089953889688,19.8704650608503,
20.2665384618872));
#136897=CARTESIAN_POINT('Ctrl Pts',(-21.1850236968841,19.9499741790566,
20.2706566207853));
#136898=CARTESIAN_POINT('Ctrl Pts',(-21.1610629739661,20.0294469148178,
20.274772895262));
#136899=CARTESIAN_POINT('Ctrl Pts',(-21.1332189034159,20.1077991846501,
20.2788891697386));
#136900=CARTESIAN_POINT('Ctrl Pts',(-21.1016267106028,20.1846240338243,
20.2830054442153));
#136901=CARTESIAN_POINT('Ctrl Pts',(-21.0700389112288,20.2614381991786,
20.287121146253));
#136902=CARTESIAN_POINT('Ctrl Pts',(-21.0347042052762,20.3367249283834,
20.2912368482907));
#136903=CARTESIAN_POINT('Ctrl Pts',(-20.9958062168364,20.4100965922228,
20.2953525503285));
#136904=CARTESIAN_POINT('Ctrl Pts',(-20.9553538829569,20.4864001534601,
20.2996327138962));
#136905=CARTESIAN_POINT('Ctrl Pts',(-20.9110477401698,20.5606318825454,
20.3039128774639));
#136906=CARTESIAN_POINT('Ctrl Pts',(-20.8631463404351,20.6323851909359,
20.3081930410317));
#136907=CARTESIAN_POINT('Ctrl Pts',(-20.8170263796525,20.7014700149142,
20.3123140265766));
#136908=CARTESIAN_POINT('Ctrl Pts',(-20.7675741880587,20.7682571483522,
20.3164350121215));
#136909=CARTESIAN_POINT('Ctrl Pts',(-20.7150628498031,20.832416043195,20.3205559976664));
#136910=CARTESIAN_POINT('Ctrl Pts',(-20.6625158670912,20.8966184888021,
20.3246797805174));
#136911=CARTESIAN_POINT('Ctrl Pts',(-20.6069059263909,20.958188799342,20.3288035633684));
#136912=CARTESIAN_POINT('Ctrl Pts',(-20.5485433933874,21.0168328476119,
20.3329273462195));
#136913=CARTESIAN_POINT('Ctrl Pts',(-20.4900913059675,21.0755668822695,
20.3370574568111));
#136914=CARTESIAN_POINT('Ctrl Pts',(-20.4288785557237,21.1313653881747,
20.3411875674027));
#136915=CARTESIAN_POINT('Ctrl Pts',(-20.3652483070037,21.1839746478091,
20.3453176779943));
#136916=CARTESIAN_POINT('Ctrl Pts',(-20.358074893939,21.1899055998009,20.3457832897099));
#136917=CARTESIAN_POINT('Ctrl Pts',(-20.3508707850611,21.1957960645337,
20.3462489014256));
#136918=CARTESIAN_POINT('Ctrl Pts',(-20.3436364935458,21.2016457139947,
20.3467145131413));
#136919=CARTESIAN_POINT('Ctrl Pts',(-20.278618922688,21.2542189338493,20.3508991582656));
#136920=CARTESIAN_POINT('Ctrl Pts',(-20.2109019654201,21.3037012778441,
20.3550838033898));
#136921=CARTESIAN_POINT('Ctrl Pts',(-20.1408117781385,21.3498035489242,
20.3592684485141));
#136922=CARTESIAN_POINT('Ctrl Pts',(-20.0708213570877,21.3958401981249,
20.363447137223));
#136923=CARTESIAN_POINT('Ctrl Pts',(-19.9984647969504,21.4385060803063,
20.3676258259318));
#136924=CARTESIAN_POINT('Ctrl Pts',(-19.9241011364256,21.4775522903914,
20.3718045146407));
#136925=CARTESIAN_POINT('Ctrl Pts',(-19.8484048007059,21.5172982497258,
20.3760580898566));
#136926=CARTESIAN_POINT('Ctrl Pts',(-19.7706290904141,21.5532932160129,
20.3803116650725));
#136927=CARTESIAN_POINT('Ctrl Pts',(-19.6911834656511,21.5853209161957,
20.3845652402884));
#136928=CARTESIAN_POINT('Ctrl Pts',(-19.6132778082301,21.6167277941182,
20.3887363645583));
#136929=CARTESIAN_POINT('Ctrl Pts',(-19.5337668439884,21.64431965604,20.3929074888282));
#136930=CARTESIAN_POINT('Ctrl Pts',(-19.4530597043389,21.6679397920169,
20.3970786130981));
#136931=CARTESIAN_POINT('Ctrl Pts',(-19.372379649495,21.6915520012255,20.4012483375651));
#136932=CARTESIAN_POINT('Ctrl Pts',(-19.2905046576306,21.7111950025156,
20.4054180620321));
#136933=CARTESIAN_POINT('Ctrl Pts',(-19.207859856905,21.7267616810847,20.409587786499));
#136934=CARTESIAN_POINT('Ctrl Pts',(-19.1252180001543,21.7423278051371,
20.413757362432));
#136935=CARTESIAN_POINT('Ctrl Pts',(-19.0418068413031,21.7538178108621,
20.4179269383649));
#136936=CARTESIAN_POINT('Ctrl Pts',(-18.9580612092297,21.7611757928658,
20.4220965142979));
#136937=CARTESIAN_POINT('Ctrl Pts',(-18.8713716383373,21.7687924325249,
20.4264126647583));
#136938=CARTESIAN_POINT('Ctrl Pts',(-18.7843241655967,21.7719810786356,
20.4307288152187));
#136939=CARTESIAN_POINT('Ctrl Pts',(-18.6974043027306,21.7707384153349,
20.4350449656791));
#136940=CARTESIAN_POINT('Ctrl Pts',(-18.6133154147565,21.7695362255058,
20.4392205393694));
#136941=CARTESIAN_POINT('Ctrl Pts',(-18.5293464188556,21.7641870271194,
20.4433961130596));
#136942=CARTESIAN_POINT('Ctrl Pts',(-18.4459326767646,21.7547407920785,
20.4475716867499));
#136943=CARTESIAN_POINT('Ctrl Pts',(-18.3583065669897,21.7448175251454,
20.4519581255954));
#136944=CARTESIAN_POINT('Ctrl Pts',(-18.2712938435843,21.7303726259076,
20.4563445644409));
#136945=CARTESIAN_POINT('Ctrl Pts',(-18.1853859711599,21.7115244744573,
20.4607310032863));
#136946=CARTESIAN_POINT('Ctrl Pts',(-18.0994780987355,21.6926763230069,
20.4651174421318));
#136947=CARTESIAN_POINT('Ctrl Pts',(-18.0146756167237,21.6694251461088,
20.4695038809773));
#136948=CARTESIAN_POINT('Ctrl Pts',(-17.9314482086413,21.6419485025781,
20.4738903198228));
#136949=CARTESIAN_POINT('Ctrl Pts',(-17.8520491325438,21.6157357421323,
20.478074989269));
#136950=CARTESIAN_POINT('Ctrl Pts',(-17.773787899996,21.5855801451821,20.4822596587152));
#136951=CARTESIAN_POINT('Ctrl Pts',(-17.6970842255972,21.5515994268124,
20.4864443281614));
#136952=CARTESIAN_POINT('Ctrl Pts',(-17.6204897238313,21.517667073329,20.4906230415516));
#136953=CARTESIAN_POINT('Ctrl Pts',(-17.5454487937957,21.4799205972817,
20.4948017549418));
#136954=CARTESIAN_POINT('Ctrl Pts',(-17.4723650688358,21.4385271716561,
20.498980468332));
#136955=CARTESIAN_POINT('Ctrl Pts',(-17.397972153007,21.3963922417504,20.5032340374225));
#136956=CARTESIAN_POINT('Ctrl Pts',(-17.3256077133136,21.3504785638631,
20.507487606513));
#136957=CARTESIAN_POINT('Ctrl Pts',(-17.2556752275784,21.3010133653268,
20.5117411756035));
#136958=CARTESIAN_POINT('Ctrl Pts',(-17.1870977913373,21.2525066311086,
20.5159123252493));
#136959=CARTESIAN_POINT('Ctrl Pts',(-17.120859296763,21.2005850589633,20.520083474895));
#136960=CARTESIAN_POINT('Ctrl Pts',(-17.0573129692034,21.1455078445844,
20.5242546245408));
#136961=CARTESIAN_POINT('Ctrl Pts',(-16.993787964182,21.0904491109903,20.5284243745857));
#136962=CARTESIAN_POINT('Ctrl Pts',(-16.9329536794658,21.03223713911,20.5325941246305));
#136963=CARTESIAN_POINT('Ctrl Pts',(-16.8751302971831,20.9711714200467,
20.5367638746754));
#136964=CARTESIAN_POINT('Ctrl Pts',(-16.817308972357,20.910107873808,20.5409334763533));
#136965=CARTESIAN_POINT('Ctrl Pts',(-16.7624986526345,20.8461911168958,
20.5451030780312));
#136966=CARTESIAN_POINT('Ctrl Pts',(-16.7109817117549,20.77975651566,20.5492726797091));
#136967=CARTESIAN_POINT('Ctrl Pts',(-16.6576544768729,20.7109874171091,
20.5535888002753));
#136968=CARTESIAN_POINT('Ctrl Pts',(-16.6078567137602,20.6395206409879,
20.5579049208416));
#136969=CARTESIAN_POINT('Ctrl Pts',(-16.561854000255,20.5657626197204,20.5622210414078));
#136970=CARTESIAN_POINT('Ctrl Pts',(-16.517349008247,20.4944059562344,20.5663966409904));
#136971=CARTESIAN_POINT('Ctrl Pts',(-16.4763959330767,20.4209053859485,
20.5705722405729));
#136972=CARTESIAN_POINT('Ctrl Pts',(-16.4391884113254,20.3456540320665,
20.5747478401554));
#136973=CARTESIAN_POINT('Ctrl Pts',(-16.4001026787487,20.2666040401448,
20.5791342212135));
#136974=CARTESIAN_POINT('Ctrl Pts',(-16.3651508277233,20.1856223925876,
20.5835206022717));
#136975=CARTESIAN_POINT('Ctrl Pts',(-16.3344993330483,20.1031863870843,
20.5879069833298));
#136976=CARTESIAN_POINT('Ctrl Pts',(-16.3038478383734,20.0207503815809,
20.592293364388));
#136977=CARTESIAN_POINT('Ctrl Pts',(-16.2774968013516,19.9368605943871,
20.5966797454461));
#136978=CARTESIAN_POINT('Ctrl Pts',(-16.255551151987,19.8520080403421,20.6010661265042));
#136979=CARTESIAN_POINT('Ctrl Pts',(-16.2346154332719,19.7710603693828,
20.6052506479319));
#136980=CARTESIAN_POINT('Ctrl Pts',(-16.217610614143,19.6889352736661,20.6094351693596));
#136981=CARTESIAN_POINT('Ctrl Pts',(-16.2046649078707,19.6060493535286,
20.6136196907873));
#136982=CARTESIAN_POINT('Ctrl Pts',(-16.1917376291181,19.5232814170601,
20.6177982557728));
#136983=CARTESIAN_POINT('Ctrl Pts',(-16.18285805684,19.4397552579918,20.6219768207584));
#136984=CARTESIAN_POINT('Ctrl Pts',(-16.1781041141918,19.3559007277721,
20.6261553857439));
#136985=CARTESIAN_POINT('Ctrl Pts',(-16.1732647974111,19.2705402879725,
20.6304089918873));
#136986=CARTESIAN_POINT('Ctrl Pts',(-16.1727008781513,19.1848400329948,
20.6346625980307));
#136987=CARTESIAN_POINT('Ctrl Pts',(-16.1764397024494,19.0992622517103,
20.6389162041741));
#136988=CARTESIAN_POINT('Ctrl Pts',(-16.180105918999,19.0153463859165,20.6430872055358));
#136989=CARTESIAN_POINT('Ctrl Pts',(-16.1879092340601,18.9315487603075,
20.6472582068975));
#136990=CARTESIAN_POINT('Ctrl Pts',(-16.1998229072908,18.8483066546134,
20.6514292082593));
#136991=CARTESIAN_POINT('Ctrl Pts',(-16.2117325838689,18.7650924739572,
20.6555988103847));
#136992=CARTESIAN_POINT('Ctrl Pts',(-16.2277498149937,18.6824338981452,
20.6597684125102));
#136993=CARTESIAN_POINT('Ctrl Pts',(-16.2477960925062,18.6007622345655,
20.6639380146357));
#136994=CARTESIAN_POINT('Ctrl Pts',(-16.267841659387,18.5190934662099,20.6681074689506));
#136995=CARTESIAN_POINT('Ctrl Pts',(-16.2919158781826,18.4384119871214,
20.6722769232655));
#136996=CARTESIAN_POINT('Ctrl Pts',(-16.319889610317,18.3591367325534,20.6764463775805));
#136997=CARTESIAN_POINT('Ctrl Pts',(-16.3488485357305,18.2770695213162,
20.6807626738809));
#136998=CARTESIAN_POINT('Ctrl Pts',(-16.3819865976511,18.1965099318425,
20.6850789701814));
#136999=CARTESIAN_POINT('Ctrl Pts',(-16.4191057647636,18.1179013403772,
20.6893952664818));
#137000=CARTESIAN_POINT('Ctrl Pts',(-16.4550137295479,18.0418577555219,
20.6935707215798));
#137001=CARTESIAN_POINT('Ctrl Pts',(-16.4946467243009,17.9676401977748,
20.6977461766778));
#137002=CARTESIAN_POINT('Ctrl Pts',(-16.5377790112352,17.8956242481676,
20.7019216317759));
#137003=CARTESIAN_POINT('Ctrl Pts',(-16.5830936242914,17.8199645713389,
20.7063083486775));
#137004=CARTESIAN_POINT('Ctrl Pts',(-16.6322706438836,17.7467356488664,
20.7106950655792));
#137005=CARTESIAN_POINT('Ctrl Pts',(-16.68499874854,17.6763359092247,20.7150817824808));
#137006=CARTESIAN_POINT('Ctrl Pts',(-16.7377268531964,17.605936169583,20.7194684993824));
#137007=CARTESIAN_POINT('Ctrl Pts',(-16.7940056129075,17.538366010084,20.7238552162841));
#137008=CARTESIAN_POINT('Ctrl Pts',(-16.8534788424305,17.473979511942,20.7282419331857));
#137009=CARTESIAN_POINT('Ctrl Pts',(-16.9102019217452,17.4125703624776,
20.7324258003262));
#137010=CARTESIAN_POINT('Ctrl Pts',(-16.9700416925391,17.3538283670977,
20.7366096674668));
#137011=CARTESIAN_POINT('Ctrl Pts',(-17.0327174013502,17.2980866408717,
20.7407935346073));
#137012=CARTESIAN_POINT('Ctrl Pts',(-17.0784953388461,17.2573732399787,
20.7438494044504));
#137013=CARTESIAN_POINT('Ctrl Pts',(-17.1257852505876,17.2182598417392,
20.7469052742935));
#137014=CARTESIAN_POINT('Ctrl Pts',(-17.174464231106,17.180864983421,20.7499611441365));
#137015=CARTESIAN_POINT('Ctrl Pts',(-17.174464231106,17.180864983421,19.9498236312055));
#137016=CARTESIAN_POINT('Ctrl Pts',(-17.2410375710667,17.1297238011471,
19.9540083585624));
#137017=CARTESIAN_POINT('Ctrl Pts',(-17.3100351878123,17.0819328152026,
19.9581930859192));
#137018=CARTESIAN_POINT('Ctrl Pts',(-17.381077330528,17.037707509232,19.9623778132761));
#137019=CARTESIAN_POINT('Ctrl Pts',(-17.3969746033918,17.0278111050749,
19.9633142398831));
#137020=CARTESIAN_POINT('Ctrl Pts',(-17.4129741644655,17.0180930627761,
19.96425066649));
#137021=CARTESIAN_POINT('Ctrl Pts',(-17.4290716121177,17.0085554711869,
19.965187093097));
#137022=CARTESIAN_POINT('Ctrl Pts',(-17.501006718607,16.9659345736727,19.9693717283973));
#137023=CARTESIAN_POINT('Ctrl Pts',(-17.5751659817943,16.9267623274508,
19.9735563636976));
#137024=CARTESIAN_POINT('Ctrl Pts',(-17.6511848627828,16.8912777367509,
19.9777409989979));
#137025=CARTESIAN_POINT('Ctrl Pts',(-17.7270955400278,16.8558436541026,
19.9819196779726));
#137026=CARTESIAN_POINT('Ctrl Pts',(-17.8048601641239,16.8240869938583,
19.9860983569473));
#137027=CARTESIAN_POINT('Ctrl Pts',(-17.8840874845047,16.7962021376512,
19.990277035922));
#137028=CARTESIAN_POINT('Ctrl Pts',(-17.9647348762107,16.7678174729877,
19.9945306135827));
#137029=CARTESIAN_POINT('Ctrl Pts',(-18.046897502032,16.7434450254351,19.9987841912434));
#137030=CARTESIAN_POINT('Ctrl Pts',(-18.1301389337682,16.723239599019,20.0030377689041));
#137031=CARTESIAN_POINT('Ctrl Pts',(-18.2117665887586,16.7034258891629,
20.0072088837266));
#137032=CARTESIAN_POINT('Ctrl Pts',(-18.2944311263189,16.6876191861685,
20.0113799985491));
#137033=CARTESIAN_POINT('Ctrl Pts',(-18.3777050584843,16.6759154028612,
20.0155511133716));
#137034=CARTESIAN_POINT('Ctrl Pts',(-18.4609510469056,16.6642155469237,
20.0197208285176));
#137035=CARTESIAN_POINT('Ctrl Pts',(-18.5448055686335,16.6566159403141,
20.0238905436636));
#137036=CARTESIAN_POINT('Ctrl Pts',(-18.6288324772911,16.6531611090283,
20.0280602588097));
#137037=CARTESIAN_POINT('Ctrl Pts',(-18.712856395511,16.6497064006967,20.0322298255595));
#137038=CARTESIAN_POINT('Ctrl Pts',(-18.7970522287831,16.6503961924512,
20.0363993923093));
#137039=CARTESIAN_POINT('Ctrl Pts',(-18.880981635612,16.6552229364061,20.0405689590591));
#137040=CARTESIAN_POINT('Ctrl Pts',(-18.9678618596805,16.6602193805865,
20.0448851207857));
#137041=CARTESIAN_POINT('Ctrl Pts',(-19.0544560473056,16.6696490660325,
20.0492012825123));
#137042=CARTESIAN_POINT('Ctrl Pts',(-19.1402833031872,16.6834450792216,
20.0535174442389));
#137043=CARTESIAN_POINT('Ctrl Pts',(-19.2233147795964,16.6967916942552,
20.0576930091793));
#137044=CARTESIAN_POINT('Ctrl Pts',(-19.3056280709207,16.7142243988718,
20.0618685741196));
#137045=CARTESIAN_POINT('Ctrl Pts',(-19.3867996159112,16.735630802998,20.0660441390599));
#137046=CARTESIAN_POINT('Ctrl Pts',(-19.4720708905892,16.7581183799726,
20.0704305991796));
#137047=CARTESIAN_POINT('Ctrl Pts',(-19.5560814939681,16.7849914459207,
20.0748170592994));
#137048=CARTESIAN_POINT('Ctrl Pts',(-19.6383622323597,16.8160618060832,
20.0792035194192));
#137049=CARTESIAN_POINT('Ctrl Pts',(-19.7206429707512,16.8471321662457,
20.0835899795389));
#137050=CARTESIAN_POINT('Ctrl Pts',(-19.8011933431587,16.8823995182362,
20.0879764396587));
#137051=CARTESIAN_POINT('Ctrl Pts',(-19.8795742651096,16.9216202579916,
20.0923628997785));
#137052=CARTESIAN_POINT('Ctrl Pts',(-19.9543489005549,16.9590364613751,
20.0965475399714));
#137053=CARTESIAN_POINT('Ctrl Pts',(-20.0274276526341,17.0001895262269,
20.1007321801642));
#137054=CARTESIAN_POINT('Ctrl Pts',(-20.0984122381085,17.0449023003337,
20.1049168203571));
#137055=CARTESIAN_POINT('Ctrl Pts',(-20.1692957865176,17.0895514317855,
20.1090955042742));
#137056=CARTESIAN_POINT('Ctrl Pts',(-20.2380907031438,17.137749965204,20.1132741881914));
#137057=CARTESIAN_POINT('Ctrl Pts',(-20.3044217668728,17.189274134772,20.1174528721085));
#137058=CARTESIAN_POINT('Ctrl Pts',(-20.3719416499117,17.2417217469061,
20.1217064485398));
#137059=CARTESIAN_POINT('Ctrl Pts',(-20.4369080598406,17.2976151641855,
20.1259600249711));
#137060=CARTESIAN_POINT('Ctrl Pts',(-20.4989546019222,17.3566712122297,
20.1302136014024));
#137061=CARTESIAN_POINT('Ctrl Pts',(-20.5597983571728,17.4145824448741,
20.1343847212528));
#137062=CARTESIAN_POINT('Ctrl Pts',(-20.6178340905372,17.4755344539392,
20.1385558411033));
#137063=CARTESIAN_POINT('Ctrl Pts',(-20.6727497630573,17.5392197045529,
20.1427269609537));
#137064=CARTESIAN_POINT('Ctrl Pts',(-20.7276470081433,17.6028835850239,
20.1468966811484));
#137065=CARTESIAN_POINT('Ctrl Pts',(-20.7794259715033,17.6692785374397,
20.151066401343));
#137066=CARTESIAN_POINT('Ctrl Pts',(-20.8278131357729,17.7380619318977,
20.1552361215377));
#137067=CARTESIAN_POINT('Ctrl Pts',(-20.8761985781537,17.8068428786539,
20.1594056933502));
#137068=CARTESIAN_POINT('Ctrl Pts',(-20.9211921974361,17.8780117217137,
20.1635752651627));
#137069=CARTESIAN_POINT('Ctrl Pts',(-20.9625630739946,17.9511957988531,
20.1677448369751));
#137070=CARTESIAN_POINT('Ctrl Pts',(-21.0053883703184,18.0269527092786,
20.1720609927655));
#137071=CARTESIAN_POINT('Ctrl Pts',(-21.0443311966684,18.104868729537,20.1763771485559));
#137072=CARTESIAN_POINT('Ctrl Pts',(-21.0791875184544,18.1845032862763,
20.1806933043463));
#137073=CARTESIAN_POINT('Ctrl Pts',(-21.112908500301,18.2615439866305,20.1848688743318));
#137074=CARTESIAN_POINT('Ctrl Pts',(-21.1428049786358,18.3401925327768,
20.1890444443173));
#137075=CARTESIAN_POINT('Ctrl Pts',(-21.1687421896672,18.4200319413184,
20.1932200143028));
#137076=CARTESIAN_POINT('Ctrl Pts',(-21.1959893070235,18.5039034775277,
20.1976064629957));
#137077=CARTESIAN_POINT('Ctrl Pts',(-21.2188665678873,18.5890887630882,
20.2019929116885));
#137078=CARTESIAN_POINT('Ctrl Pts',(-21.2372782491424,18.6750914188312,
20.2063793603814));
#137079=CARTESIAN_POINT('Ctrl Pts',(-21.2556899303975,18.7610940745742,
20.2107658090742));
#137080=CARTESIAN_POINT('Ctrl Pts',(-21.2696360151223,18.8479135155775,
20.215152257767));
#137081=CARTESIAN_POINT('Ctrl Pts',(-21.2790836672405,18.935048687726,20.2195387064599));
#137082=CARTESIAN_POINT('Ctrl Pts',(-21.288956382332,19.0261041921328,20.2241225075637));
#137083=CARTESIAN_POINT('Ctrl Pts',(-21.2939437779116,19.1176988534549,
20.2287063086676));
#137084=CARTESIAN_POINT('Ctrl Pts',(-21.2939995273702,19.2094444086991,
20.2332901097715));
#137085=CARTESIAN_POINT('',(-21.2937660450662,19.2120076676442,20.1667099326));
#137086=CARTESIAN_POINT('Ctrl Pts',(-17.174464231106,17.180864983421,19.8833624896767));
#137087=CARTESIAN_POINT('Ctrl Pts',(-17.2411054517724,17.1296716556555,
19.8875327666645));
#137088=CARTESIAN_POINT('Ctrl Pts',(-17.3103077755869,17.08173412414,19.8917030436522));
#137089=CARTESIAN_POINT('Ctrl Pts',(-17.3817164411788,17.0373097790757,
19.89587332064));
#137090=CARTESIAN_POINT('Ctrl Pts',(-17.4531115618229,16.9928938605158,
19.9000428066007));
#137091=CARTESIAN_POINT('Ctrl Pts',(-17.5267118022329,16.951990047319,19.9042122925615));
#137092=CARTESIAN_POINT('Ctrl Pts',(-17.6021342305576,16.9148118805367,
19.9083817785222));
#137093=CARTESIAN_POINT('Ctrl Pts',(-17.6775649772729,16.8776296133492,
19.9125517243384));
#137094=CARTESIAN_POINT('Ctrl Pts',(-17.7548178977551,16.8441740106921,
19.9167216701545));
#137095=CARTESIAN_POINT('Ctrl Pts',(-17.8334875675827,16.8146116009582,
19.9208916159707));
#137096=CARTESIAN_POINT('Ctrl Pts',(-17.9122411807607,16.7850176470763,
19.9250660112681));
#137097=CARTESIAN_POINT('Ctrl Pts',(-17.9924141299049,16.7593253418245,
19.9292404065656));
#137098=CARTESIAN_POINT('Ctrl Pts',(-18.0735836975314,16.7376520043808,
19.933414801863));
#137099=CARTESIAN_POINT('Ctrl Pts',(-18.1547996667123,16.7159662771144,
19.9375915835035));
#137100=CARTESIAN_POINT('Ctrl Pts',(-18.2370129388557,16.6983041884075,
19.9417683651439));
#137101=CARTESIAN_POINT('Ctrl Pts',(-18.319790788349,16.6847318572678,19.9459451467843));
#137102=CARTESIAN_POINT('Ctrl Pts',(-18.4027096905814,16.6711363989934,
19.9501290456246));
#137103=CARTESIAN_POINT('Ctrl Pts',(-18.4861946340951,16.6616446663111,
19.9543129444648));
#137104=CARTESIAN_POINT('Ctrl Pts',(-18.5698082620909,16.6562708415172,
19.958496843305));
#137105=CARTESIAN_POINT('Ctrl Pts',(-18.6237987490351,16.6528008878227,
19.9611984451984));
#137106=CARTESIAN_POINT('Ctrl Pts',(-18.6778428604002,16.6510468155004,
19.9639000470918));
#137107=CARTESIAN_POINT('Ctrl Pts',(-18.7318236815484,16.6510009250709,
19.9666016489852));
#137108=CARTESIAN_POINT('Ctrl Pts',(-18.8154370558738,16.6509298432759,
19.970786284298));
#137109=CARTESIAN_POINT('Ctrl Pts',(-18.8992095168452,16.6549593424997,
19.9749709196109));
#137110=CARTESIAN_POINT('Ctrl Pts',(-18.9827056282392,16.6631095960615,
19.9791555549237));
#137111=CARTESIAN_POINT('Ctrl Pts',(-19.0660828933652,16.671248248757,19.9833342339317));
#137112=CARTESIAN_POINT('Ctrl Pts',(-19.1491841362882,16.6834959609934,
19.9875129129397));
#137113=CARTESIAN_POINT('Ctrl Pts',(-19.2315736415637,16.6998209002102,
19.9916915919477));
#137114=CARTESIAN_POINT('Ctrl Pts',(-19.3154398964185,16.7164384476547,
19.9959451696027));
#137115=CARTESIAN_POINT('Ctrl Pts',(-19.3985681651269,16.737280826455,20.0001987472576));
#137116=CARTESIAN_POINT('Ctrl Pts',(-19.4805039902943,16.7622591414209,
20.0044523249126));
#137117=CARTESIAN_POINT('Ctrl Pts',(-19.5608513518334,16.7867532097861,
20.0086234398184));
#137118=CARTESIAN_POINT('Ctrl Pts',(-19.6400516319826,16.8152241408901,
20.0127945547242));
#137119=CARTESIAN_POINT('Ctrl Pts',(-19.7176880447477,16.847536898824,20.0169656696301));
#137120=CARTESIAN_POINT('Ctrl Pts',(-19.7952984058592,16.8798388138977,
20.0211353848777));
#137121=CARTESIAN_POINT('Ctrl Pts',(-19.8713455174284,16.9159798188824,
20.0253051001254));
#137122=CARTESIAN_POINT('Ctrl Pts',(-19.9454312968479,16.9557762388141,
20.029474815373));
#137123=CARTESIAN_POINT('Ctrl Pts',(-20.019514439946,16.9955712426016,20.0336443822425));
#137124=CARTESIAN_POINT('Ctrl Pts',(-20.0916359848007,17.0390211842644,
20.037813949112));
#137125=CARTESIAN_POINT('Ctrl Pts',(-20.1614224652667,17.085896448252,20.0419835159816));
#137126=CARTESIAN_POINT('Ctrl Pts',(-20.233662517875,17.1344197655748,20.046299677622));
#137127=CARTESIAN_POINT('Ctrl Pts',(-20.3033998138019,17.1866134578921,
20.0506158392624));
#137128=CARTESIAN_POINT('Ctrl Pts',(-20.3702544757161,17.2421751498168,
20.0549320009028));
#137129=CARTESIAN_POINT('Ctrl Pts',(-20.43493138463,17.2959269508853,20.059107566006));
#137130=CARTESIAN_POINT('Ctrl Pts',(-20.4969102614717,17.3528303456934,
20.0632831311092));
#137131=CARTESIAN_POINT('Ctrl Pts',(-20.5558837277202,17.4125729976815,
20.0674586962125));
#137132=CARTESIAN_POINT('Ctrl Pts',(-20.6178357603199,17.4753330652,20.0718451561215));
#137133=CARTESIAN_POINT('Ctrl Pts',(-20.6764704133147,17.5412263089036,
20.0762316160305));
#137134=CARTESIAN_POINT('Ctrl Pts',(-20.7314796146231,17.6098519152917,
20.0806180759396));
#137135=CARTESIAN_POINT('Ctrl Pts',(-20.7864888159316,17.6784775216799,
20.0850045358486));
#137136=CARTESIAN_POINT('Ctrl Pts',(-20.8378722882314,17.7498349754593,
20.0893909957576));
#137137=CARTESIAN_POINT('Ctrl Pts',(-20.8853760800034,17.8234910946631,
20.0937774556667));
#137138=CARTESIAN_POINT('Ctrl Pts',(-20.9317208338504,17.8953500892083,
20.0980568909951));
#137139=CARTESIAN_POINT('Ctrl Pts',(-20.9745398785638,17.9696546343097,
20.1023363263235));
#137140=CARTESIAN_POINT('Ctrl Pts',(-21.0135728623478,18.0460332342734,
20.106615761652));
#137141=CARTESIAN_POINT('Ctrl Pts',(-21.0525424990579,18.1222878785374,
20.1108882518361));
#137142=CARTESIAN_POINT('Ctrl Pts',(-21.0877380947942,18.2006095044151,
20.1151607420202));
#137143=CARTESIAN_POINT('Ctrl Pts',(-21.118942960611,18.2805984336684,20.1194332322043));
#137144=CARTESIAN_POINT('Ctrl Pts',(-21.1500944339135,18.3604504993293,
20.1236984120223));
#137145=CARTESIAN_POINT('Ctrl Pts',(-21.1772686129624,18.4419637894576,
20.1279635918403));
#137146=CARTESIAN_POINT('Ctrl Pts',(-21.2002957124611,18.5247161966825,
20.1322287716583));
#137147=CARTESIAN_POINT('Ctrl Pts',(-21.2232995986398,18.6073851822802,
20.136489651804));
#137148=CARTESIAN_POINT('Ctrl Pts',(-21.2421646000029,18.6912903874225,
20.1407505319496));
#137149=CARTESIAN_POINT('Ctrl Pts',(-21.2567699771926,18.7759923653821,
20.1450114120952));
#137150=CARTESIAN_POINT('Ctrl Pts',(-21.271362764314,18.8606213288853,20.1492686192942));
#137151=CARTESIAN_POINT('Ctrl Pts',(-21.2817031594057,18.9460452737795,
20.1535258264931));
#137152=CARTESIAN_POINT('Ctrl Pts',(-21.2877212408942,19.0318134385456,
20.1577830336921));
#137153=CARTESIAN_POINT('Ctrl Pts',(-21.2919276409715,19.0917619812152,
20.1607586525376));
#137154=CARTESIAN_POINT('Ctrl Pts',(-21.2940234518455,19.1518784236118,
20.163734271383));
#137155=CARTESIAN_POINT('Ctrl Pts',(-21.293999801981,19.2120069046681,20.1667098902285));
#137156=CARTESIAN_POINT('Ctrl Pts',(-21.2901594272135,19.212019439545,20.166710586346));
#137157=CARTESIAN_POINT('Ctrl Pts',(-21.2914431884923,19.5768333887026,
20.1847914783466));
#137158=CARTESIAN_POINT('Ctrl Pts',(-21.0477248310816,20.7953392166858,
20.2452643059079));
#137159=CARTESIAN_POINT('Ctrl Pts',(-19.1741877278151,22.2059163556896,
20.3481290690295));
#137160=CARTESIAN_POINT('Ctrl Pts',(-16.4540142726395,21.2022206477943,
20.4753048757109));
#137161=CARTESIAN_POINT('Ctrl Pts',(-15.9020680968674,18.7161854390005,
20.5870029223479));
#137162=CARTESIAN_POINT('Ctrl Pts',(-16.7482596547722,17.5166786748788,
20.6563090334244));
#137163=CARTESIAN_POINT('Ctrl Pts',(-17.1763037726968,17.1832235620119,
20.6832232089404));
#137164=CARTESIAN_POINT('Origin',(-18.734,19.211,-1.76670989022852));
#137165=CARTESIAN_POINT('',(-17.1769962058593,17.1841776921994,21.549922496891));
#137166=CARTESIAN_POINT('',(-17.1722616694474,17.1780320626177,21.4832513372676));
#137167=CARTESIAN_POINT('',(-17.174464231106,17.180864983421,-1.76670989022852));
#137168=CARTESIAN_POINT('',(-21.2938947673487,19.209658313364,21.0332900820457));
#137169=CARTESIAN_POINT('Ctrl Pts',(-21.2904840295148,19.2096606602608,
21.0332901097715));
#137170=CARTESIAN_POINT('Ctrl Pts',(-21.288030249326,19.7238724906044,21.0587831909243));
#137171=CARTESIAN_POINT('Ctrl Pts',(-20.8878309688531,21.0966582904734,
21.1266682076376));
#137172=CARTESIAN_POINT('Ctrl Pts',(-18.6471934916355,22.2367210801752,
21.2369451599114));
#137173=CARTESIAN_POINT('Ctrl Pts',(-16.1425598602209,20.7760159325242,
21.3641209665928));
#137174=CARTESIAN_POINT('Ctrl Pts',(-16.0386997413532,18.3992339415041,
21.468446745586));
#137175=CARTESIAN_POINT('Ctrl Pts',(-16.8637709644904,17.4236621366429,
21.5303805890188));
#137176=CARTESIAN_POINT('Ctrl Pts',(-17.1769962058593,17.1841776921994,
21.549922496891));
#137177=CARTESIAN_POINT('Ctrl Pts',(-17.174464231106,17.180864983421,20.7499611441365));
#137178=CARTESIAN_POINT('Ctrl Pts',(-17.2444595711224,17.1270950442199,
20.7543551689586));
#137179=CARTESIAN_POINT('Ctrl Pts',(-17.3173285036894,17.0768805205813,
20.7587491937808));
#137180=CARTESIAN_POINT('Ctrl Pts',(-17.3926685577946,17.0305344620583,
20.7631432186029));
#137181=CARTESIAN_POINT('Ctrl Pts',(-17.4641971206759,16.9865330739424,
20.7673149474996));
#137182=CARTESIAN_POINT('Ctrl Pts',(-17.5379524259981,16.9460185574918,
20.7714866763963));
#137183=CARTESIAN_POINT('Ctrl Pts',(-17.6135585392101,16.9092157066869,
20.775658405293));
#137184=CARTESIAN_POINT('Ctrl Pts',(-17.6891339188667,16.8724278160804,
20.7798284384001));
#137185=CARTESIAN_POINT('Ctrl Pts',(-17.7665581992986,16.8393487961018,
20.7839984715072));
#137186=CARTESIAN_POINT('Ctrl Pts',(-17.8454310841992,16.8101573808614,
20.7881685046143));
#137187=CARTESIAN_POINT('Ctrl Pts',(-17.9242955646648,16.780969076162,20.7923380933764));
#137188=CARTESIAN_POINT('Ctrl Pts',(-18.0046079113321,16.7556677122338,
20.7965076821384));
#137189=CARTESIAN_POINT('Ctrl Pts',(-18.0859493836776,16.7343832757804,
20.8006772709005));
#137190=CARTESIAN_POINT('Ctrl Pts',(-18.1673065855882,16.7130947234078,
20.8048476659649));
#137191=CARTESIAN_POINT('Ctrl Pts',(-18.249692863051,16.6958247560999,20.8090180610293));
#137192=CARTESIAN_POINT('Ctrl Pts',(-18.3326772440529,16.6826527047182,
20.8131884560938));
#137193=CARTESIAN_POINT('Ctrl Pts',(-18.4157540950087,16.6694659756469,
20.8173634982524));
#137194=CARTESIAN_POINT('Ctrl Pts',(-18.4994299245131,16.6603863469597,
20.8215385404111));
#137195=CARTESIAN_POINT('Ctrl Pts',(-18.5832671191098,16.6554414311899,
20.8257135825697));
#137196=CARTESIAN_POINT('Ctrl Pts',(-18.6671584825602,16.6504933204133,
20.8298913223049));
#137197=CARTESIAN_POINT('Ctrl Pts',(-18.7512109590877,16.6496852437991,
20.8340690620401));
#137198=CARTESIAN_POINT('Ctrl Pts',(-18.8349877955741,16.6529926768781,
20.8382468017752));
#137199=CARTESIAN_POINT('Ctrl Pts',(-18.9189003990789,16.6563054699152,
20.8424313118695));
#137200=CARTESIAN_POINT('Ctrl Pts',(-19.0025360138916,16.6637470414522,
20.8466158219638));
#137201=CARTESIAN_POINT('Ctrl Pts',(-19.0854643589663,16.6752411777978,
20.8508003320581));
#137202=CARTESIAN_POINT('Ctrl Pts',(-19.1159668534451,16.679468922004,20.8523394679944));
#137203=CARTESIAN_POINT('Ctrl Pts',(-19.1463737794482,16.6842444410465,
20.8538786039308));
#137204=CARTESIAN_POINT('Ctrl Pts',(-19.1766642028218,16.6895622348469,
20.8554177398671));
#137205=CARTESIAN_POINT('Ctrl Pts',(-19.2590223527151,16.7040210508733,
20.859602573687));
#137206=CARTESIAN_POINT('Ctrl Pts',(-19.3408244952178,16.7225461130517,
20.8637874075069));
#137207=CARTESIAN_POINT('Ctrl Pts',(-19.4216382791443,16.7450815915656,
20.8679722413268));
#137208=CARTESIAN_POINT('Ctrl Pts',(-19.5023370763704,16.7675850052487,
20.8721511207141));
#137209=CARTESIAN_POINT('Ctrl Pts',(-19.5820498690828,16.7940873783028,
20.8763300001013));
#137210=CARTESIAN_POINT('Ctrl Pts',(-19.6603530717567,16.8244816182466,
20.8805088794886));
#137211=CARTESIAN_POINT('Ctrl Pts',(-19.7400550248593,16.8554187983857,
20.8847624072828));
#137212=CARTESIAN_POINT('Ctrl Pts',(-19.8182960576181,16.8903881737628,
20.8890159350769));
#137213=CARTESIAN_POINT('Ctrl Pts',(-19.8946441220391,16.9292232313445,
20.8932694628711));
#137214=CARTESIAN_POINT('Ctrl Pts',(-19.9695165810178,16.9673077103391,
20.8974407812627));
#137215=CARTESIAN_POINT('Ctrl Pts',(-20.0425681641203,17.0091095557739,
20.9016120996543));
#137216=CARTESIAN_POINT('Ctrl Pts',(-20.1134118643469,17.0544233358169,
20.9057834180459));
#137217=CARTESIAN_POINT('Ctrl Pts',(-20.1842318054824,17.0997219188245,
20.9099533374884));
#137218=CARTESIAN_POINT('Ctrl Pts',(-20.25284494715,17.1485298496368,20.9141232569309));
#137219=CARTESIAN_POINT('Ctrl Pts',(-20.3188911542426,17.2005970480514,
20.9182931763733));
#137220=CARTESIAN_POINT('Ctrl Pts',(-20.384935018117,17.2526623992016,20.9224629478735));
#137221=CARTESIAN_POINT('Ctrl Pts',(-20.4484117677876,17.3079865025997,
20.9266327193736));
#137222=CARTESIAN_POINT('Ctrl Pts',(-20.508993493609,17.3662783143125,20.9308024908737));
#137223=CARTESIAN_POINT('Ctrl Pts',(-20.5716985989686,17.4266132444502,
20.9351184121799));
#137224=CARTESIAN_POINT('Ctrl Pts',(-20.6313015884265,17.490127419461,20.9394343334862));
#137225=CARTESIAN_POINT('Ctrl Pts',(-20.6874809779157,17.5564571420112,
20.9437502547924));
#137226=CARTESIAN_POINT('Ctrl Pts',(-20.7418360321654,17.6206329135953,
20.9479260235017));
#137227=CARTESIAN_POINT('Ctrl Pts',(-20.7929861867178,17.6874437676863,
20.952101792211));
#137228=CARTESIAN_POINT('Ctrl Pts',(-20.8406829832797,17.7565286843805,
20.9562775609204));
#137229=CARTESIAN_POINT('Ctrl Pts',(-20.8907810730049,17.8290916782227,
20.9606635585251));
#137230=CARTESIAN_POINT('Ctrl Pts',(-20.9370686538008,17.9041632231126,
20.9650495561297));
#137231=CARTESIAN_POINT('Ctrl Pts',(-20.9793120563334,17.981295251012,20.9694355537344));
#137232=CARTESIAN_POINT('Ctrl Pts',(-21.021555458866,18.0584272789114,20.9738215513391));
#137233=CARTESIAN_POINT('Ctrl Pts',(-21.0597544996862,18.13761923468,20.9782075489438));
#137234=CARTESIAN_POINT('Ctrl Pts',(-21.0937343932684,18.2184005877363,
20.9825935465485));
#137235=CARTESIAN_POINT('Ctrl Pts',(-21.1297845102027,18.3041035407708,
20.9872467608424));
#137236=CARTESIAN_POINT('Ctrl Pts',(-21.1612011557346,18.3918658581185,
20.9918999751363));
#137237=CARTESIAN_POINT('Ctrl Pts',(-21.1877704304992,18.4811981951189,
20.9965531894303));
#137238=CARTESIAN_POINT('Ctrl Pts',(-21.2142564917145,18.5702507480116,
21.0011918301056));
#137239=CARTESIAN_POINT('Ctrl Pts',(-21.2359253488098,18.6608632602714,
21.0058304707809));
#137240=CARTESIAN_POINT('Ctrl Pts',(-21.2526114411354,18.7525281812567,
21.0104691114562));
#137241=CARTESIAN_POINT('Ctrl Pts',(-21.2692072331732,18.8436970382994,
21.0150826491548));
#137242=CARTESIAN_POINT('Ctrl Pts',(-21.2808739262263,18.9359066855585,
21.0196961868533));
#137243=CARTESIAN_POINT('Ctrl Pts',(-21.2874965126302,19.0286389296337,
21.0243097245519));
#137244=CARTESIAN_POINT('Ctrl Pts',(-21.2917935179279,19.0888074075896,
21.0273031767656));
#137245=CARTESIAN_POINT('Ctrl Pts',(-21.2939679583765,19.1491955214723,
21.0302966289794));
#137246=CARTESIAN_POINT('Ctrl Pts',(-21.2939996483756,19.2096582411964,
21.0332900811932));
#137247=CARTESIAN_POINT('',(-21.2964371679699,19.2128544327287,20.9667098902285));
#137248=CARTESIAN_POINT('Ctrl Pts',(-17.1763037726968,17.1832235620119,
20.6832232089404));
#137249=CARTESIAN_POINT('Ctrl Pts',(-17.4224626840759,16.9914607409853,
20.6987009689849));
#137250=CARTESIAN_POINT('Ctrl Pts',(-18.4657781420964,16.4381425114079,
20.7565706645898));
#137251=CARTESIAN_POINT('Ctrl Pts',(-20.5735369877998,16.8838680312786,
20.8510662250192));
#137252=CARTESIAN_POINT('Ctrl Pts',(-21.2904548994085,18.4784657038926,
20.9300840254041));
#137253=CARTESIAN_POINT('Ctrl Pts',(-21.2964371679699,19.2128544327287,
20.9667098902285));
#137254=CARTESIAN_POINT('Ctrl Pts',(-21.2964371679699,19.2128544327287,
20.9667098902285));
#137255=CARTESIAN_POINT('Ctrl Pts',(-21.2973789664463,19.3284704701528,
20.9724759609646));
#137256=CARTESIAN_POINT('Ctrl Pts',(-21.2376963737069,20.2931122040567,
21.0206339672611));
#137257=CARTESIAN_POINT('Ctrl Pts',(-20.0126665865687,21.9547543377114,
21.1111839091181));
#137258=CARTESIAN_POINT('Ctrl Pts',(-17.1190396137422,21.7713501236625,
21.2383597157995));
#137259=CARTESIAN_POINT('Ctrl Pts',(-15.7420433199098,19.3016368730853,
21.3623821918493));
#137260=CARTESIAN_POINT('Ctrl Pts',(-16.5519396301118,17.6604732932792,
21.4440127323387));
#137261=CARTESIAN_POINT('Ctrl Pts',(-17.1722616694474,17.1780320626177,
21.4832513372676));
#137262=CARTESIAN_POINT('Origin',(18.734,19.211,-1.76670989022852));
#137263=CARTESIAN_POINT('',(20.2955776349071,17.1782440534666,0.7498178112644));
#137264=CARTESIAN_POINT('',(20.2916906334339,17.1833020127912,0.683386617883875));
#137265=CARTESIAN_POINT('',(20.2935357313021,17.1808649545432,-1.76670989022852));
#137266=CARTESIAN_POINT('',(16.1740007446525,19.2129525932361,0.233290109771496));
#137267=CARTESIAN_POINT('Ctrl Pts',(16.1719919784605,19.2129541253863,0.233290109771496));
#137268=CARTESIAN_POINT('Ctrl Pts',(16.1708576353774,19.3442909950989,0.239839092339242));
#137269=CARTESIAN_POINT('Ctrl Pts',(16.2398215309513,20.3246257991586,0.288780010467465));
#137270=CARTESIAN_POINT('Ctrl Pts',(17.5061738855977,21.978179087,0.380112864156167));
#137271=CARTESIAN_POINT('Ctrl Pts',(20.3959079781532,21.7409373178462,0.507288670837601));
#137272=CARTESIAN_POINT('Ctrl Pts',(21.7186679484337,19.2624153691283,0.630523653207013));
#137273=CARTESIAN_POINT('Ctrl Pts',(20.9031377918545,17.6518060150516,0.711366700015944));
#137274=CARTESIAN_POINT('Ctrl Pts',(20.2955776349071,17.1782440534666,0.7498178112644));
#137275=CARTESIAN_POINT('',(19.395767528315,16.7380131948456,1.73172587381032E-11));
#137276=CARTESIAN_POINT('Ctrl Pts',(19.395767528315,16.7380131948456,1.73172587381032E-11));
#137277=CARTESIAN_POINT('Ctrl Pts',(19.3150528289901,16.7164140633987,0.0041815967549353));
#137278=CARTESIAN_POINT('Ctrl Pts',(19.2331283959629,16.6987302550736,0.00836319349255328));
#137279=CARTESIAN_POINT('Ctrl Pts',(19.1504091887632,16.685093551314,0.0125447902301714));
#137280=CARTESIAN_POINT('Ctrl Pts',(19.0678077744006,16.6714762663337,0.0167204323393492));
#137281=CARTESIAN_POINT('Ctrl Pts',(18.9844142845817,16.6618947132319,0.0208960744485263));
#137282=CARTESIAN_POINT('Ctrl Pts',(18.9006573782918,16.6564305023623,0.0250717165577041));
#137283=CARTESIAN_POINT('Ctrl Pts',(18.8165042143108,16.6509404400653,0.0292671138175207));
#137284=CARTESIAN_POINT('Ctrl Pts',(18.7319846403618,16.6496069070114,0.0334625110773381));
#137285=CARTESIAN_POINT('Ctrl Pts',(18.6475423744123,16.6524603620468,0.0376579083371547));
#137286=CARTESIAN_POINT('Ctrl Pts',(18.5636493738553,16.6552952564233,0.0418260161051873));
#137287=CARTESIAN_POINT('Ctrl Pts',(18.4798331446954,16.6622628172183,0.0459941238732202));
#137288=CARTESIAN_POINT('Ctrl Pts',(18.3965307038144,16.6733407490106,0.0501622316412529));
#137289=CARTESIAN_POINT('Ctrl Pts',(18.3132563453466,16.6844149462778,0.0543289342820943));
#137290=CARTESIAN_POINT('Ctrl Pts',(18.2304958875343,16.6995967018794,0.0584956369229356));
#137291=CARTESIAN_POINT('Ctrl Pts',(18.1486808927462,16.718811896609,0.0626623395637771));
#137292=CARTESIAN_POINT('Ctrl Pts',(18.0668688404716,16.7380264002553,0.0668288923472635));
#137293=CARTESIAN_POINT('Ctrl Pts',(17.9860026319441,16.7612739482847,0.0709954451307501));
#137294=CARTESIAN_POINT('Ctrl Pts',(17.9065019549449,16.7884296737907,0.0751619979142366));
#137295=CARTESIAN_POINT('Ctrl Pts',(17.8260462587421,16.8159116133658,0.0793786023208257));
#137296=CARTESIAN_POINT('Ctrl Pts',(17.7469895837595,16.8473961156675,0.0835952067274143));
#137297=CARTESIAN_POINT('Ctrl Pts',(17.6697476948766,16.8827029761992,0.0878118111340034));
#137298=CARTESIAN_POINT('Ctrl Pts',(17.5933154552392,16.9176397503257,0.0919842171059645));
#137299=CARTESIAN_POINT('Ctrl Pts',(17.5186605203447,16.9563188567597,0.0961566230779257));
#137300=CARTESIAN_POINT('Ctrl Pts',(17.4461607527195,16.9985194750769,0.100329029049887));
#137301=CARTESIAN_POINT('Ctrl Pts',(17.3725089964354,17.041390642215,0.10456773267379));
#137302=CARTESIAN_POINT('Ctrl Pts',(17.3010819091514,17.0878959373098,0.108806436297694));
#137303=CARTESIAN_POINT('Ctrl Pts',(17.2322432877688,17.1377593537487,0.113045139921597));
#137304=CARTESIAN_POINT('Ctrl Pts',(17.1634046663863,17.1876227701875,0.1172838435455));
#137305=CARTESIAN_POINT('Ctrl Pts',(17.0971548535428,17.2408439496524,0.121522547169403));
#137306=CARTESIAN_POINT('Ctrl Pts',(17.0338195264424,17.2971070151826,0.125761250793306));
#137307=CARTESIAN_POINT('Ctrl Pts',(16.9721381147478,17.3519008477408,0.129889266471862));
#137308=CARTESIAN_POINT('Ctrl Pts',(16.9129812130569,17.4097927309776,0.134017282150418));
#137309=CARTESIAN_POINT('Ctrl Pts',(16.8566825236081,17.4705175689386,0.138145297828974));
#137310=CARTESIAN_POINT('Ctrl Pts',(16.8004749046566,17.5311441765279,0.142266635901988));
#137311=CARTESIAN_POINT('Ctrl Pts',(16.7471166302611,17.5945942890769,0.146387973975001));
#137312=CARTESIAN_POINT('Ctrl Pts',(16.6969071786038,17.6605636623788,0.150509312048014));
#137313=CARTESIAN_POINT('Ctrl Pts',(16.6467433533799,17.7264730878598,0.154626904970446));
#137314=CARTESIAN_POINT('Ctrl Pts',(16.5997229600923,17.7948968581842,0.158744497892878));
#137315=CARTESIAN_POINT('Ctrl Pts',(16.5561068210809,17.8654958932736,0.16286209081531));
#137316=CARTESIAN_POINT('Ctrl Pts',(16.5125163943093,17.9360533093806,0.16697725636706));
#137317=CARTESIAN_POINT('Ctrl Pts',(16.4723264875143,18.0087830434683,0.171092421918811));
#137318=CARTESIAN_POINT('Ctrl Pts',(16.4357550862559,18.0833163934643,0.175207587470561));
#137319=CARTESIAN_POINT('Ctrl Pts',(16.3991935732988,18.1578295908767,0.179321640349689));
#137320=CARTESIAN_POINT('Ctrl Pts',(16.3662488306646,18.2341450104433,0.183435693228817));
#137321=CARTESIAN_POINT('Ctrl Pts',(16.3370925482536,18.3118700495687,0.187549746107944));
#137322=CARTESIAN_POINT('Ctrl Pts',(16.3079200305285,18.3896383689178,0.191666089846375));
#137323=CARTESIAN_POINT('Ctrl Pts',(16.2825403575632,18.4688174331029,0.195782433584806));
#137324=CARTESIAN_POINT('Ctrl Pts',(16.2610764229501,18.5489962371172,0.199898777323237));
#137325=CARTESIAN_POINT('Ctrl Pts',(16.239606571517,18.6291971434892,0.204016255786767));
#137326=CARTESIAN_POINT('Ctrl Pts',(16.2220547120702,18.7103978759457,0.208133734250297));
#137327=CARTESIAN_POINT('Ctrl Pts',(16.2084928021298,18.7921761784404,0.212251212713827));
#137328=CARTESIAN_POINT('Ctrl Pts',(16.1949128183452,18.874063466196,0.21637417850653));
#137329=CARTESIAN_POINT('Ctrl Pts',(16.1853334600005,18.9565293904166,0.220497144299234));
#137330=CARTESIAN_POINT('Ctrl Pts',(16.1797748247972,19.0391461249782,0.224620110091938));
#137331=CARTESIAN_POINT('Ctrl Pts',(16.1758784899859,19.0970564657531,0.227510109985124));
#137332=CARTESIAN_POINT('Ctrl Pts',(16.1739565734894,19.1550408159346,0.230400109878309));
#137333=CARTESIAN_POINT('Ctrl Pts',(16.1740007446525,19.2129525932361,0.233290109771496));
#137334=CARTESIAN_POINT('',(18.0722627314315,16.7380050975816,0.));
#137335=CARTESIAN_POINT('Origin',(18.734,19.211,0.));
#137336=CARTESIAN_POINT('',(16.1765334933267,19.2078568329122,0.166709890228504));
#137337=CARTESIAN_POINT('Ctrl Pts',(18.0722627314315,16.7380050975816,-1.38777878078145E-15));
#137338=CARTESIAN_POINT('Ctrl Pts',(17.2488902483963,16.9583275322964,0.0423919355604767));
#137339=CARTESIAN_POINT('Ctrl Pts',(16.3345567825823,17.8262089039162,0.0979618989699788));
#137340=CARTESIAN_POINT('Ctrl Pts',(16.1744956276614,18.942407731855,0.153531862379481));
#137341=CARTESIAN_POINT('Ctrl Pts',(16.1765334933267,19.2078568329122,0.166709890228504));
#137342=CARTESIAN_POINT('Ctrl Pts',(16.1765334933267,19.2078568329122,0.166709890228504));
#137343=CARTESIAN_POINT('Ctrl Pts',(16.1810511662408,19.7963216342631,0.195923797939959));
#137344=CARTESIAN_POINT('Ctrl Pts',(16.6739009423912,21.2477390833877,0.267529641211891));
#137345=CARTESIAN_POINT('Ctrl Pts',(19.0860575192109,22.2167215957953,0.381527420044302));
#137346=CARTESIAN_POINT('Ctrl Pts',(21.4520483322073,20.5433423167195,0.508703226725735));
#137347=CARTESIAN_POINT('Ctrl Pts',(21.3518777067184,18.250992735458,0.60932295933893));
#137348=CARTESIAN_POINT('Ctrl Pts',(20.5461545393492,17.3761757621948,0.667550756391643));
#137349=CARTESIAN_POINT('Ctrl Pts',(20.2916906334338,17.1833020127911,0.683386617883882));
#137350=CARTESIAN_POINT('Origin',(18.734,19.211,-1.76670989022852));
#137351=CARTESIAN_POINT('',(20.2940723354197,17.180154697314,1.55000083039626));
#137352=CARTESIAN_POINT('',(20.2935357313021,17.1808649545431,1.48324950807533));
#137353=CARTESIAN_POINT('',(20.2935357313021,17.1808649545432,-1.76670989022852));
#137354=CARTESIAN_POINT('',(16.1715629762874,19.209145560805,1.0332901097715));
#137355=CARTESIAN_POINT('Ctrl Pts',(16.1715629762874,19.209145560805,1.0332901097715));
#137356=CARTESIAN_POINT('Ctrl Pts',(16.1775452442342,19.9435342473242,1.06991597459592));
#137357=CARTESIAN_POINT('Ctrl Pts',(16.8944631203331,21.5381318465523,1.14893377498083));
#137358=CARTESIAN_POINT('Ctrl Pts',(19.6025525656016,22.1108086232828,1.27034351092621));
#137359=CARTESIAN_POINT('Ctrl Pts',(21.6424137421715,20.050299112292,1.39751931760764));
#137360=CARTESIAN_POINT('Ctrl Pts',(21.1817796660755,17.9755451208384,1.49073842409766));
#137361=CARTESIAN_POINT('Ctrl Pts',(20.4294541348775,17.2819919278148,1.5415655950272));
#137362=CARTESIAN_POINT('Ctrl Pts',(20.2940723354196,17.1801546973139,1.55000083039627));
#137363=CARTESIAN_POINT('Ctrl Pts',(20.2955776349071,17.1782440534666,0.7498178112644));
#137364=CARTESIAN_POINT('Ctrl Pts',(20.2333092697084,17.1297090584855,0.753758635576423));
#137365=CARTESIAN_POINT('Ctrl Pts',(19.4740834540712,16.5951984416462,0.800091395448925));
#137366=CARTESIAN_POINT('Ctrl Pts',(17.4553334985585,16.4672458544258,0.888816090881905));
#137367=CARTESIAN_POINT('Ctrl Pts',(16.2303037681755,18.1288878534983,0.979366032738912));
#137368=CARTESIAN_POINT('Ctrl Pts',(16.1706211779077,19.0935295300429,1.02752403903544));
#137369=CARTESIAN_POINT('Ctrl Pts',(16.1715629762874,19.209145560805,1.0332901097715));
#137370=CARTESIAN_POINT('',(16.1740711683132,19.2123417124082,0.96670991823092));
#137371=CARTESIAN_POINT('Ctrl Pts',(20.2916906334338,17.1833020127911,0.683386617883882));
#137372=CARTESIAN_POINT('Ctrl Pts',(19.8649653595043,16.8598608424138,0.709942691952123));
#137373=CARTESIAN_POINT('Ctrl Pts',(18.4990491173507,16.3489928111998,0.778890701580843));
#137374=CARTESIAN_POINT('Ctrl Pts',(16.5801690015235,17.3253417016998,0.873331792362383));
#137375=CARTESIAN_POINT('Ctrl Pts',(16.1799697185864,18.6981275092202,0.941216809075682));
#137376=CARTESIAN_POINT('Ctrl Pts',(16.1775159392447,19.2123393420905,0.966709890228504));
#137377=CARTESIAN_POINT('Ctrl Pts',(16.1740003516256,19.2123417611365,0.966709918806587));
#137378=CARTESIAN_POINT('Ctrl Pts',(16.174049215721,19.3055715198376,0.971325636241826));
#137379=CARTESIAN_POINT('Ctrl Pts',(16.17919506457,19.3986231969093,0.975941353677064));
#137380=CARTESIAN_POINT('Ctrl Pts',(16.1893550117453,19.490967647685,0.980557071112303));
#137381=CARTESIAN_POINT('Ctrl Pts',(16.1995507644016,19.5836375369126,0.985189055165875));
#137382=CARTESIAN_POINT('Ctrl Pts',(16.2147958902436,19.6755949409525,0.989821039219448));
#137383=CARTESIAN_POINT('Ctrl Pts',(16.2349566280026,19.7663217309596,0.99445302327302));
#137384=CARTESIAN_POINT('Ctrl Pts',(16.2552161964654,19.8574932761445,0.99910771394821));
#137385=CARTESIAN_POINT('Ctrl Pts',(16.2804395585911,19.9474218535553,1.0037624046234));
#137386=CARTESIAN_POINT('Ctrl Pts',(16.3104425150043,20.0356023992939,1.00841709529859));
#137387=CARTESIAN_POINT('Ctrl Pts',(16.3297568898048,20.0923685421719,1.01141354801622));
#137388=CARTESIAN_POINT('Ctrl Pts',(16.3510510137503,20.1484107097619,1.01441000073385));
#137389=CARTESIAN_POINT('Ctrl Pts',(16.3742656055452,20.2035994094432,1.01740645345148));
#137390=CARTESIAN_POINT('Ctrl Pts',(16.4066870270799,20.2806757634937,1.0215912893308));
#137391=CARTESIAN_POINT('Ctrl Pts',(16.4429490448682,20.3563053000825,1.02577612521011));
#137392=CARTESIAN_POINT('Ctrl Pts',(16.4829010312601,20.4300789281004,1.02996096108943));
#137393=CARTESIAN_POINT('Ctrl Pts',(16.5227961672129,20.5037475785304,1.03413984207691));
#137394=CARTESIAN_POINT('Ctrl Pts',(16.5663706250003,20.575565165042,1.03831872306438));
#137395=CARTESIAN_POINT('Ctrl Pts',(16.6134257496347,20.6451425482453,1.04249760405186));
#137396=CARTESIAN_POINT('Ctrl Pts',(16.6613214086794,20.7159627755642,1.04675113138857));
#137397=CARTESIAN_POINT('Ctrl Pts',(16.7128231204605,20.7844615349321,1.05100465872528));
#137398=CARTESIAN_POINT('Ctrl Pts',(16.7676724163246,20.8502546579703,1.05525818606199));
#137399=CARTESIAN_POINT('Ctrl Pts',(16.8214616326485,20.9147761886841,1.05942950491759));
#137400=CARTESIAN_POINT('Ctrl Pts',(16.878469877553,20.9766953676843,1.06360082377319));
#137401=CARTESIAN_POINT('Ctrl Pts',(16.9384107604235,21.0356805974518,1.06777214262879));
#137402=CARTESIAN_POINT('Ctrl Pts',(16.9983315346257,21.0946460391488,1.07194206211116));
#137403=CARTESIAN_POINT('Ctrl Pts',(17.0611826653049,21.150679164025,1.07611198159354));
#137404=CARTESIAN_POINT('Ctrl Pts',(17.1266402115777,21.2034845069819,1.08028190107591));
#137405=CARTESIAN_POINT('Ctrl Pts',(17.1920954288672,21.2562879711218,1.08445167219232));
#137406=CARTESIAN_POINT('Ctrl Pts',(17.2601565188202,21.3058635935363,1.08862144330872));
#137407=CARTESIAN_POINT('Ctrl Pts',(17.3304667737115,21.3519564411039,1.09279121442512));
#137408=CARTESIAN_POINT('Ctrl Pts',(17.4032413841786,21.399664830616,1.09710713490077));
#137409=CARTESIAN_POINT('Ctrl Pts',(17.4784253144497,21.4436414778788,1.10142305537642));
#137410=CARTESIAN_POINT('Ctrl Pts',(17.5555924541958,21.4836538794968,1.10573897585207));
#137411=CARTESIAN_POINT('Ctrl Pts',(17.6302537040283,21.5223669369383,1.10991474312749));
#137412=CARTESIAN_POINT('Ctrl Pts',(17.7067708828925,21.5573691217994,1.11409051040291));
#137413=CARTESIAN_POINT('Ctrl Pts',(17.78473673888,21.5884985301968,1.11826627767833));
#137414=CARTESIAN_POINT('Ctrl Pts',(17.8666278007654,21.6211951546004,1.12265227475409));
#137415=CARTESIAN_POINT('Ctrl Pts',(17.950116683959,21.6496186282125,1.12703827182985));
#137416=CARTESIAN_POINT('Ctrl Pts',(18.0347145603764,21.6736408333191,1.13142426890561));
#137417=CARTESIAN_POINT('Ctrl Pts',(18.1193124367938,21.6976630384256,1.13581026598138));
#137418=CARTESIAN_POINT('Ctrl Pts',(18.2050187243926,21.7172839196893,1.14019626305714));
#137419=CARTESIAN_POINT('Ctrl Pts',(18.2913357968955,21.7324377651034,1.1445822601329));
#137420=CARTESIAN_POINT('Ctrl Pts',(18.3736918326046,21.7468962099727,1.14876698652964));
#137421=CARTESIAN_POINT('Ctrl Pts',(18.4569101590231,21.7573423934243,1.15295171292637));
#137422=CARTESIAN_POINT('Ctrl Pts',(18.5405652833629,21.7636815332899,1.1571364393231));
#137423=CARTESIAN_POINT('Ctrl Pts',(18.6241013816905,21.7700116537136,1.16131521161602));
#137424=CARTESIAN_POINT('Ctrl Pts',(18.7080725887003,21.7722463032879,1.16549398390893));
#137425=CARTESIAN_POINT('Ctrl Pts',(18.7920441907127,21.7703418825793,1.16967275620184));
#137426=CARTESIAN_POINT('Ctrl Pts',(18.8775185285604,21.7684033808102,1.1739263108107));
#137427=CARTESIAN_POINT('Ctrl Pts',(18.9629928008506,21.7621761208413,1.17817986541955));
#137428=CARTESIAN_POINT('Ctrl Pts',(19.0480040535634,21.7516694893956,1.18243342002841));
#137429=CARTESIAN_POINT('Ctrl Pts',(19.1313696312364,21.7413662486844,1.18660463296569));
#137430=CARTESIAN_POINT('Ctrl Pts',(19.2142894786525,21.7269479022129,1.19077584590298));
#137431=CARTESIAN_POINT('Ctrl Pts',(19.2963297754537,21.7084757703806,1.19494705884027));
#137432=CARTESIAN_POINT('Ctrl Pts',(19.3783425741987,21.6900098299901,1.19911687368111));
#137433=CARTESIAN_POINT('Ctrl Pts',(19.4594759594167,21.6674929036788,1.20328668852194));
#137434=CARTESIAN_POINT('Ctrl Pts',(19.5393061675985,21.641037443421,1.20745650336278));
#137435=CARTESIAN_POINT('Ctrl Pts',(19.6191335625861,21.6145829154461,1.21162617126051));
#137436=CARTESIAN_POINT('Ctrl Pts',(19.6976574354581,21.5841902749986,1.21579583915825));
#137437=CARTESIAN_POINT('Ctrl Pts',(19.7744703683971,21.5500214647343,1.21996550705598));
#137438=CARTESIAN_POINT('Ctrl Pts',(19.853979866456,21.51465313743,1.22428155370251));
#137439=CARTESIAN_POINT('Ctrl Pts',(19.9316555794736,21.475238789784,1.22859760034904));
#137440=CARTESIAN_POINT('Ctrl Pts',(20.0070713188011,21.4320108998486,1.23291364699557));
#137441=CARTESIAN_POINT('Ctrl Pts',(20.0800341869216,21.3901889822938,1.23708931569658));
#137442=CARTESIAN_POINT('Ctrl Pts',(20.1508814665265,21.3447980820665,1.24126498439758));
#137443=CARTESIAN_POINT('Ctrl Pts',(20.2192566079351,21.2960929975867,1.24544065309859));
#137444=CARTESIAN_POINT('Ctrl Pts',(20.2910797103399,21.2449318562982,1.24982688871788));
#137445=CARTESIAN_POINT('Ctrl Pts',(20.3601743374505,21.1901138572313,1.25421312433717));
#137446=CARTESIAN_POINT('Ctrl Pts',(20.4261681137408,21.1319807585811,1.25859935995646));
#137447=CARTESIAN_POINT('Ctrl Pts',(20.492161890031,21.073847659931,1.26298559557576));
#137448=CARTESIAN_POINT('Ctrl Pts',(20.5550544538034,21.0123999213878,1.26737183119505));
#137449=CARTESIAN_POINT('Ctrl Pts',(20.6145211583455,20.948020487218,1.27175806681434));
#137450=CARTESIAN_POINT('Ctrl Pts',(20.6712532036771,20.8866016309711,1.27594259528124));
#137451=CARTESIAN_POINT('Ctrl Pts',(20.7250787538107,20.8222861461377,1.28012712374813));
#137452=CARTESIAN_POINT('Ctrl Pts',(20.7756877958407,20.7553804402786,1.28431165221502));
#137453=CARTESIAN_POINT('Ctrl Pts',(20.8262247807555,20.6885699947122,1.2884902227535));
#137454=CARTESIAN_POINT('Ctrl Pts',(20.8735540790342,20.6191770173187,1.29266879329197));
#137455=CARTESIAN_POINT('Ctrl Pts',(20.9174037187929,20.5475433778076,1.29684736383044));
#137456=CARTESIAN_POINT('Ctrl Pts',(20.9620407606535,20.4746234226361,1.30110096839983));
#137457=CARTESIAN_POINT('Ctrl Pts',(21.0030716129383,20.399381892885,1.30535457296922));
#137458=CARTESIAN_POINT('Ctrl Pts',(21.0402535236503,20.3222131589622,1.30960817753861));
#137459=CARTESIAN_POINT('Ctrl Pts',(21.0767133936984,20.2465429753506,1.31377918077288));
#137460=CARTESIAN_POINT('Ctrl Pts',(21.1094722631679,20.1690202013163,1.31795018400715));
#137461=CARTESIAN_POINT('Ctrl Pts',(21.1383468618206,20.0900427566698,1.32212118724142));
#137462=CARTESIAN_POINT('Ctrl Pts',(21.1672117644678,20.0110918324171,1.32629078986506));
#137463=CARTESIAN_POINT('Ctrl Pts',(21.1921948288651,19.9306876393951,1.3304603924887));
#137464=CARTESIAN_POINT('Ctrl Pts',(21.2131612203807,19.8492473214674,1.33462999511233));
#137465=CARTESIAN_POINT('Ctrl Pts',(21.2341268617413,19.7678099173871,1.33879944855205));
#137466=CARTESIAN_POINT('Ctrl Pts',(21.2510760020805,19.6853369078529,1.34296890199176));
#137467=CARTESIAN_POINT('Ctrl Pts',(21.2639242673564,19.6022584841778,1.34713835543148));
#137468=CARTESIAN_POINT('Ctrl Pts',(21.2772250225956,19.5162542061506,1.3514546486035));
#137469=CARTESIAN_POINT('Ctrl Pts',(21.2861305797708,19.4296015962165,1.35577094177553));
#137470=CARTESIAN_POINT('Ctrl Pts',(21.290605703432,19.342784965678,1.36008723494755));
#137471=CARTESIAN_POINT('Ctrl Pts',(21.2949348020335,19.2588011962232,1.36426268576165));
#137472=CARTESIAN_POINT('Ctrl Pts',(21.2951181996998,19.1746644168246,1.36843813657575));
#137473=CARTESIAN_POINT('Ctrl Pts',(21.2911771388899,19.0908123120325,1.37261358738984));
#137474=CARTESIAN_POINT('Ctrl Pts',(21.287036673876,19.0027175773967,1.37700030174083));
#137475=CARTESIAN_POINT('Ctrl Pts',(21.2783434334409,18.9149376655593,1.38138701609182));
#137476=CARTESIAN_POINT('Ctrl Pts',(21.2651832584911,18.8279708732557,1.38577373044281));
#137477=CARTESIAN_POINT('Ctrl Pts',(21.2520230835413,18.7410040809521,1.3901604447938));
#137478=CARTESIAN_POINT('Ctrl Pts',(21.2343961650043,18.6548509616386,1.39454715914479));
#137479=CARTESIAN_POINT('Ctrl Pts',(21.2124488481584,18.5699919602204,1.39893387349578));
#137480=CARTESIAN_POINT('Ctrl Pts',(21.1915163487695,18.489056736666,1.40311775146669));
#137481=CARTESIAN_POINT('Ctrl Pts',(21.1665762583416,18.4089973678034,1.40730162943759));
#137482=CARTESIAN_POINT('Ctrl Pts',(21.1377183903467,18.3302401576427,1.4114855074085));
#137483=CARTESIAN_POINT('Ctrl Pts',(21.108898908102,18.2515877076328,1.41566382012784));
#137484=CARTESIAN_POINT('Ctrl Pts',(21.0761721516232,18.1742344053255,1.41984213284718));
#137485=CARTESIAN_POINT('Ctrl Pts',(21.0396783460786,18.0985938851192,1.42402044556652));
#137486=CARTESIAN_POINT('Ctrl Pts',(21.0032221314464,18.0230312794007,1.42819445436126));
#137487=CARTESIAN_POINT('Ctrl Pts',(20.9630067732795,17.9491783637443,1.43236846315601));
#137488=CARTESIAN_POINT('Ctrl Pts',(20.9192209916458,17.8774298977292,1.43654247195075));
#137489=CARTESIAN_POINT('Ctrl Pts',(20.875464056581,17.8057287004162,1.44071373086123));
#137490=CARTESIAN_POINT('Ctrl Pts',(20.8281416078255,17.7361295913329,1.44488498977172));
#137491=CARTESIAN_POINT('Ctrl Pts',(20.7774882160362,17.6690026229202,1.4490562486822));
#137492=CARTESIAN_POINT('Ctrl Pts',(20.7268554210923,17.6019029498917,1.45322581146194));
#137493=CARTESIAN_POINT('Ctrl Pts',(20.6728946531877,17.5372737855256,1.45739537424168));
#137494=CARTESIAN_POINT('Ctrl Pts',(20.6158828834061,17.4754548945236,1.46156493702142));
#137495=CARTESIAN_POINT('Ctrl Pts',(20.5588584214485,17.4136222411659,1.46573542804501));
#137496=CARTESIAN_POINT('Ctrl Pts',(20.4987819085052,17.3546014533543,1.46990591906861));
#137497=CARTESIAN_POINT('Ctrl Pts',(20.4359689312939,17.2986972632686,1.47407641009221));
#137498=CARTESIAN_POINT('Ctrl Pts',(20.3899160331811,17.2577097144467,1.47713410941991));
#137499=CARTESIAN_POINT('Ctrl Pts',(20.3423929859753,17.2183967604034,1.48019180874762));
#137500=CARTESIAN_POINT('Ctrl Pts',(20.2935357313021,17.1808649545431,1.48324950807533));
#137501=CARTESIAN_POINT('Origin',(18.734,19.211,-1.76670989022852));
#137502=CARTESIAN_POINT('',(20.2935357313021,17.1808649545432,2.34989189381266));
#137503=CARTESIAN_POINT('',(20.2935357313021,17.1808649545431,2.28327545725186));
#137504=CARTESIAN_POINT('',(20.2935357313021,17.1808649545432,-1.76670989022852));
#137505=CARTESIAN_POINT('',(16.1742339456424,19.2099923322427,1.83329006740172));
#137506=CARTESIAN_POINT('Ctrl Pts',(16.174000198019,19.2099930951884,1.8332901097715));
#137507=CARTESIAN_POINT('Ctrl Pts',(16.1739663681253,19.2960037291259,1.83754657623673));
#137508=CARTESIAN_POINT('Ctrl Pts',(16.1782715498352,19.3819895204514,1.84180304270196));
#137509=CARTESIAN_POINT('Ctrl Pts',(16.1868819594924,19.4674950052547,1.84605950916719));
#137510=CARTESIAN_POINT('Ctrl Pts',(16.1954973714593,19.5530501653856,1.85031844847222));
#137511=CARTESIAN_POINT('Ctrl Pts',(16.2084229438551,19.6381240334814,1.85457738777724));
#137512=CARTESIAN_POINT('Ctrl Pts',(16.2255732751461,19.7222683894382,1.85883632708227));
#137513=CARTESIAN_POINT('Ctrl Pts',(16.2427520342423,19.8065522202146,1.86310232586009));
#137514=CARTESIAN_POINT('Ctrl Pts',(16.2641694501953,19.8899030371078,1.86736832463791));
#137515=CARTESIAN_POINT('Ctrl Pts',(16.2896893999656,19.9718848076808,1.87163432341573));
#137516=CARTESIAN_POINT('Ctrl Pts',(16.3152317962993,20.0539386868993,1.87590407443496));
#137517=CARTESIAN_POINT('Ctrl Pts',(16.3448837660451,20.1346207148683,1.88017382545418));
#137518=CARTESIAN_POINT('Ctrl Pts',(16.378460747601,20.2135142544661,1.8844435764734));
#137519=CARTESIAN_POINT('Ctrl Pts',(16.4121081360956,20.2925732244374,1.88872228065292));
#137520=CARTESIAN_POINT('Ctrl Pts',(16.4496967908718,20.3698358236637,1.89300098483243));
#137521=CARTESIAN_POINT('Ctrl Pts',(16.4909957509127,20.4449092100217,1.89727968901195));
#137522=CARTESIAN_POINT('Ctrl Pts',(16.5197685295451,20.4972124623244,1.90026064078576));
#137523=CARTESIAN_POINT('Ctrl Pts',(16.5503412786202,20.5484536572702,1.90324159255957));
#137524=CARTESIAN_POINT('Ctrl Pts',(16.5826239200438,20.5985089054101,1.90622254433338));
#137525=CARTESIAN_POINT('Ctrl Pts',(16.6279420233601,20.668776046099,1.9104071796206));
#137526=CARTESIAN_POINT('Ctrl Pts',(16.6767906254528,20.7369513808156,1.91459181490782));
#137527=CARTESIAN_POINT('Ctrl Pts',(16.728950354716,20.8026582296292,1.91877645019504));
#137528=CARTESIAN_POINT('Ctrl Pts',(16.7810358412063,20.8682715530599,1.92295512918358));
#137529=CARTESIAN_POINT('Ctrl Pts',(16.8364228098494,20.9314230124316,1.92713380817211));
#137530=CARTESIAN_POINT('Ctrl Pts',(16.8948480567165,20.9917639174008,1.93131248716064));
#137531=CARTESIAN_POINT('Ctrl Pts',(16.9543205181261,21.0531863731819,1.93556606482123));
#137532=CARTESIAN_POINT('Ctrl Pts',(17.0169409883732,21.1116961215209,1.93981964248182));
#137533=CARTESIAN_POINT('Ctrl Pts',(17.0823881640283,21.1669596987868,1.94407322014241));
#137534=CARTESIAN_POINT('Ctrl Pts',(17.146566536076,21.2211518986328,1.9482443350439));
#137535=CARTESIAN_POINT('Ctrl Pts',(17.2134626230233,21.2722223587372,1.95241544994539));
#137536=CARTESIAN_POINT('Ctrl Pts',(17.2827368115693,21.319894297471,1.95658656484688));
#137537=CARTESIAN_POINT('Ctrl Pts',(17.3519877545813,21.3675502394867,1.96075628009585));
#137538=CARTESIAN_POINT('Ctrl Pts',(17.4236148357139,21.4118096644136,1.96492599534481));
#137539=CARTESIAN_POINT('Ctrl Pts',(17.4972477392584,21.4524378968757,1.96909571059377));
#137540=CARTESIAN_POINT('Ctrl Pts',(17.5708780226965,21.4930646836486,1.97326527747024));
#137541=CARTESIAN_POINT('Ctrl Pts',(17.6465135834381,21.5300603133609,1.9774348443467));
#137542=CARTESIAN_POINT('Ctrl Pts',(17.72375887895,21.563235718915,1.98160441122317));
#137543=CARTESIAN_POINT('Ctrl Pts',(17.8037199856921,21.5975775144528,1.98592057287247));
#137544=CARTESIAN_POINT('Ctrl Pts',(17.8854056436201,21.6278252451698,1.99023673452178));
#137545=CARTESIAN_POINT('Ctrl Pts',(17.9683557183345,21.6538239465735,1.99455289617108));
#137546=CARTESIAN_POINT('Ctrl Pts',(18.0486037412687,21.6789757549798,1.99872846129521));
#137547=CARTESIAN_POINT('Ctrl Pts',(18.1300346026437,21.700151030558,2.00290402641934));
#137548=CARTESIAN_POINT('Ctrl Pts',(18.2122191472968,21.7172611080556,2.00707959154347));
#137549=CARTESIAN_POINT('Ctrl Pts',(18.2985545772998,21.7352353622707,2.01146605145537));
#137550=CARTESIAN_POINT('Ctrl Pts',(18.3857212504018,21.7487228766122,2.01585251136725));
#137551=CARTESIAN_POINT('Ctrl Pts',(18.4732153214812,21.7576824206111,2.02023897127914));
#137552=CARTESIAN_POINT('Ctrl Pts',(18.5607093925606,21.7666419646101,2.02462543119104));
#137553=CARTESIAN_POINT('Ctrl Pts',(18.6485302783064,21.7710735849926,2.02901189110292));
#137554=CARTESIAN_POINT('Ctrl Pts',(18.7361763184418,21.7709990749291,2.03339835101482));
#137555=CARTESIAN_POINT('Ctrl Pts',(18.8197896747139,21.7709279931498,2.03758298542408));
#137556=CARTESIAN_POINT('Ctrl Pts',(18.9035551457575,21.7667560675609,2.04176761983334));
#137557=CARTESIAN_POINT('Ctrl Pts',(18.9870372618431,21.7584638651253,2.0459522542426));
#137558=CARTESIAN_POINT('Ctrl Pts',(19.0704005515262,21.7501834656078,2.05013093234558));
#137559=CARTESIAN_POINT('Ctrl Pts',(19.1534808335082,21.7377944834677,2.05430961044856));
#137560=CARTESIAN_POINT('Ctrl Pts',(19.2358424472483,21.7213294919472,2.05848828855154));
#137561=CARTESIAN_POINT('Ctrl Pts',(19.3196803332538,21.7045693773805,2.06274186643257));
#137562=CARTESIAN_POINT('Ctrl Pts',(19.4027730512143,21.6835856916762,2.0669954443136));
#137563=CARTESIAN_POINT('Ctrl Pts',(19.4846662953176,21.6584681025652,2.07124902219463));
#137564=CARTESIAN_POINT('Ctrl Pts',(19.564971879664,21.6338374667537,2.07542013619847));
#137565=CARTESIAN_POINT('Ctrl Pts',(19.6441236233218,21.6052319257752,2.07959125020231));
#137566=CARTESIAN_POINT('Ctrl Pts',(19.7217049706295,21.5727872239035,2.08376236420615));
#137567=CARTESIAN_POINT('Ctrl Pts',(19.7992602848139,21.5403534091452,2.08793207855493));
#137568=CARTESIAN_POINT('Ctrl Pts',(19.8752458251399,21.5040831693519,2.09210179290371));
#137569=CARTESIAN_POINT('Ctrl Pts',(19.9492638220018,21.4641608559829,2.09627150725249));
#137570=CARTESIAN_POINT('Ctrl Pts',(20.0232791850298,21.4242399631974,2.10044107322742));
#137571=CARTESIAN_POINT('Ctrl Pts',(20.0953267393072,21.380667474352,2.10461063920235));
#137572=CARTESIAN_POINT('Ctrl Pts',(20.1650334097657,21.3336736395721,2.10878020517728));
#137573=CARTESIAN_POINT('Ctrl Pts',(20.2371908797456,21.2850275602218,2.11309636788719));
#137574=CARTESIAN_POINT('Ctrl Pts',(20.3068393549607,21.2327153644361,2.11741253059711));
#137575=CARTESIAN_POINT('Ctrl Pts',(20.3735994723772,21.1770400733913,2.12172869330702));
#137576=CARTESIAN_POINT('Ctrl Pts',(20.4381848869942,21.1231783982594,2.12590425753552));
#137577=CARTESIAN_POINT('Ctrl Pts',(20.5000669160019,21.0661697225462,2.13007982176402));
#137578=CARTESIAN_POINT('Ctrl Pts',(20.5589387125309,21.0063269049135,2.13425538599252));
#137579=CARTESIAN_POINT('Ctrl Pts',(20.6207839821297,20.9434615702666,2.13864184794314));
#137580=CARTESIAN_POINT('Ctrl Pts',(20.679306546588,20.8774687014452,2.14302830989376));
#137581=CARTESIAN_POINT('Ctrl Pts',(20.7341990153408,20.8087496359034,2.14741477184438));
#137582=CARTESIAN_POINT('Ctrl Pts',(20.7890914840937,20.7400305703616,2.151801233795));
#137583=CARTESIAN_POINT('Ctrl Pts',(20.8403535806943,20.6685858238657,2.15618769574562));
#137584=CARTESIAN_POINT('Ctrl Pts',(20.887732090256,20.5948490103337,2.16057415769625));
#137585=CARTESIAN_POINT('Ctrl Pts',(20.9329306422986,20.5245049401061,2.16475879183929));
#137586=CARTESIAN_POINT('Ctrl Pts',(20.9747633711854,20.4518132565708,2.16894342598234));
#137587=CARTESIAN_POINT('Ctrl Pts',(21.0129782252718,20.3771296020326,2.17312806012539));
#137588=CARTESIAN_POINT('Ctrl Pts',(21.0511386852003,20.3025522505172,2.17730673795496));
#137589=CARTESIAN_POINT('Ctrl Pts',(21.085691291295,20.2259889658798,2.18148541578452));
#137590=CARTESIAN_POINT('Ctrl Pts',(21.1164276176735,20.1478237008885,2.18566409361409));
#137591=CARTESIAN_POINT('Ctrl Pts',(21.147714872981,20.0682573736757,2.18991767156257));
#137592=CARTESIAN_POINT('Ctrl Pts',(21.1750474280244,19.9870314755977,2.19417124951106));
#137593=CARTESIAN_POINT('Ctrl Pts',(21.1982547719725,19.9045765414219,2.19842482745954));
#137594=CARTESIAN_POINT('Ctrl Pts',(21.2210121944986,19.8237201633461,2.20259594117414));
#137595=CARTESIAN_POINT('Ctrl Pts',(21.2398027993353,19.7416824418436,2.20676705488875));
#137596=CARTESIAN_POINT('Ctrl Pts',(21.2545152522169,19.6588871100422,2.21093816860335));
#137597=CARTESIAN_POINT('Ctrl Pts',(21.2692227681827,19.5761195610708,2.2151078826576));
#137598=CARTESIAN_POINT('Ctrl Pts',(21.2798547695702,19.492595359254,2.21927759671185));
#137599=CARTESIAN_POINT('Ctrl Pts',(21.2863509615983,19.4087487517745,2.22344731076611));
#137600=CARTESIAN_POINT('Ctrl Pts',(21.2928469224602,19.3249051279663,2.2276168764416));
#137601=CARTESIAN_POINT('Ctrl Pts',(21.295207331893,19.2407395800305,2.23178644211709));
#137602=CARTESIAN_POINT('Ctrl Pts',(21.2934238553146,19.1566904350362,2.23595600779258));
#137603=CARTESIAN_POINT('Ctrl Pts',(21.2915776736484,19.0696862139402,2.24027217084134));
#137604=CARTESIAN_POINT('Ctrl Pts',(21.2852907961475,18.9828072608782,2.2445883338901));
#137605=CARTESIAN_POINT('Ctrl Pts',(21.2746126736334,18.8965365799124,2.24890449693885));
#137606=CARTESIAN_POINT('Ctrl Pts',(21.2642823912514,18.8130761687307,2.25308006085864));
#137607=CARTESIAN_POINT('Ctrl Pts',(21.2498426885277,18.7301854650859,2.25725562477843));
#137608=CARTESIAN_POINT('Ctrl Pts',(21.231390539663,18.6482918230541,2.26143118869822));
#137609=CARTESIAN_POINT('Ctrl Pts',(21.2120064127082,18.5622619104639,2.26581765131146));
#137610=CARTESIAN_POINT('Ctrl Pts',(21.1881940056825,18.4773329923524,2.27020411392471));
#137611=CARTESIAN_POINT('Ctrl Pts',(21.1601243952751,18.3939807721656,2.27459057653795));
#137612=CARTESIAN_POINT('Ctrl Pts',(21.1320547848677,18.3106285519788,2.27897703915119));
#137613=CARTESIAN_POINT('Ctrl Pts',(21.0997282551214,18.2288535413399,2.28336350176444));
#137614=CARTESIAN_POINT('Ctrl Pts',(21.0633723464423,18.1491033611364,2.28774996437768));
#137615=CARTESIAN_POINT('Ctrl Pts',(21.0286887000586,18.073021449015,2.29193466292273));
#137616=CARTESIAN_POINT('Ctrl Pts',(20.9902091092478,17.9984989913316,2.29611936146777));
#137617=CARTESIAN_POINT('Ctrl Pts',(20.9480961900758,17.9259404445351,2.30030406001282));
#137618=CARTESIAN_POINT('Ctrl Pts',(20.906052378713,17.8535009671904,2.30448189141701));
#137619=CARTESIAN_POINT('Ctrl Pts',(20.8603873210463,17.7830193881584,2.30865972282119));
#137620=CARTESIAN_POINT('Ctrl Pts',(20.8113109120553,17.7148785561807,2.31283755422537));
#137621=CARTESIAN_POINT('Ctrl Pts',(20.7622817553091,17.6468033322485,2.31701136308764));
#137622=CARTESIAN_POINT('Ctrl Pts',(20.7098480348099,17.5810647524346,2.32118517194992));
#137623=CARTESIAN_POINT('Ctrl Pts',(20.6542641570255,17.5180187339361,2.32535898081219));
#137624=CARTESIAN_POINT('Ctrl Pts',(20.5987134202879,17.455010305673,2.32953030110402));
#137625=CARTESIAN_POINT('Ctrl Pts',(20.5400165562338,17.3946915975892,2.33370162139586));
#137626=CARTESIAN_POINT('Ctrl Pts',(20.4784688819012,17.3373862937953,2.33787294168769));
#137627=CARTESIAN_POINT('Ctrl Pts',(20.4193558194132,17.2823477884285,2.34187925906268));
#137628=CARTESIAN_POINT('Ctrl Pts',(20.3576135213163,17.2300890706105,2.34588557643767));
#137629=CARTESIAN_POINT('Ctrl Pts',(20.2935357313021,17.1808649545431,2.34989189381266));
#137630=CARTESIAN_POINT('Ctrl Pts',(20.2940723354196,17.1801546973139,1.55000083039627));
#137631=CARTESIAN_POINT('Ctrl Pts',(19.7490823055711,16.7702009552852,1.58395753058768));
#137632=CARTESIAN_POINT('Ctrl Pts',(18.1401763481965,16.3317555889403,1.66030616633957));
#137633=CARTESIAN_POINT('Ctrl Pts',(16.4202753011031,17.6266608733541,1.75473569408333));
#137634=CARTESIAN_POINT('Ctrl Pts',(16.1765569575323,18.8451666316293,1.81520852163568));
#137635=CARTESIAN_POINT('Ctrl Pts',(16.1778407186761,19.2099805598359,1.83328941362754));
#137636=CARTESIAN_POINT('',(16.1740004726294,19.2125555906437,1.76670989019937));
#137637=CARTESIAN_POINT('Ctrl Pts',(20.2935357313021,17.1808649545431,1.48324950807533));
#137638=CARTESIAN_POINT('Ctrl Pts',(20.2268277547837,17.129620347355,1.4874243831541));
#137639=CARTESIAN_POINT('Ctrl Pts',(20.157631652809,17.0816980355692,1.49159925823288));
#137640=CARTESIAN_POINT('Ctrl Pts',(20.086318576514,17.037331564471,1.49577413331165));
#137641=CARTESIAN_POINT('Ctrl Pts',(20.0149603661994,16.9929370138496,1.49995165066732));
#137642=CARTESIAN_POINT('Ctrl Pts',(19.9414829166633,16.9521030063531,1.50412916802298));
#137643=CARTESIAN_POINT('Ctrl Pts',(19.866281573762,16.9150168908027,1.50830668537865));
#137644=CARTESIAN_POINT('Ctrl Pts',(19.7909572166317,16.8778701098476,1.51249103631011));
#137645=CARTESIAN_POINT('Ctrl Pts',(19.7139037594437,16.8444836393503,1.51667538724156));
#137646=CARTESIAN_POINT('Ctrl Pts',(19.6355356364855,16.814996348887,1.52085973817302));
#137647=CARTESIAN_POINT('Ctrl Pts',(19.6027604934786,16.8026641642521,1.52260971884108));
#137648=CARTESIAN_POINT('Ctrl Pts',(19.5697555724601,16.7910133725809,1.52435969950915));
#137649=CARTESIAN_POINT('Ctrl Pts',(19.5365517913736,16.7800514974268,1.52610968017721));
#137650=CARTESIAN_POINT('Ctrl Pts',(19.457153209384,16.7538389001049,1.53029432358246));
#137651=CARTESIAN_POINT('Ctrl Pts',(19.3763213117682,16.7314715386277,1.53447896698771));
#137652=CARTESIAN_POINT('Ctrl Pts',(19.2944633944868,16.713104729289,1.53866361039297));
#137653=CARTESIAN_POINT('Ctrl Pts',(19.2127219865111,16.6947640616392,1.54284229774762));
#137654=CARTESIAN_POINT('Ctrl Pts',(19.1299579046074,16.6804127358414,1.54702098510228));
#137655=CARTESIAN_POINT('Ctrl Pts',(19.0465949713152,16.670156757313,1.55119967245693));
#137656=CARTESIAN_POINT('Ctrl Pts',(18.9617380512092,16.6597169765107,1.555453248057));
#137657=CARTESIAN_POINT('Ctrl Pts',(18.8762610609814,16.6535209330019,1.55970682365707));
#137658=CARTESIAN_POINT('Ctrl Pts',(18.7906234644726,16.6516262908143,1.56396039925714));
#137659=CARTESIAN_POINT('Ctrl Pts',(18.7066458766309,16.6497683745809,1.5681315230761));
#137660=CARTESIAN_POINT('Ctrl Pts',(18.622514334468,16.6520466005142,1.57230264689506));
#137661=CARTESIAN_POINT('Ctrl Pts',(18.5386669502935,16.6584630267727,1.57647377071402));
#137662=CARTESIAN_POINT('Ctrl Pts',(18.4548476979935,16.6648773002377,1.58064349506736));
#137663=CARTESIAN_POINT('Ctrl Pts',(18.3713128726456,16.6754269815325,1.58481321942069));
#137664=CARTESIAN_POINT('Ctrl Pts',(18.288498029712,16.6900620804015,1.58898294377403));
#137665=CARTESIAN_POINT('Ctrl Pts',(18.2056861301166,16.7046966591217,1.5931525199304));
#137666=CARTESIAN_POINT('Ctrl Pts',(18.1235946149205,16.7234162858241,1.59732209608676));
#137667=CARTESIAN_POINT('Ctrl Pts',(18.0426500224208,16.7461196360673,1.60149167224312));
#137668=CARTESIAN_POINT('Ctrl Pts',(17.9588599467864,16.7696210878046,1.60580782346108));
#137669=CARTESIAN_POINT('Ctrl Pts',(17.8762994412696,16.7973914245207,1.61012397467904));
#137670=CARTESIAN_POINT('Ctrl Pts',(17.7954238786637,16.8292622175274,1.614440125897));
#137671=CARTESIAN_POINT('Ctrl Pts',(17.7171824223146,16.8600949830687,1.61861570064709));
#137672=CARTESIAN_POINT('Ctrl Pts',(17.640518246769,16.894764965485,1.62279127539718));
#137673=CARTESIAN_POINT('Ctrl Pts',(17.5658209824088,16.9330716027803,1.62696685014727));
#137674=CARTESIAN_POINT('Ctrl Pts',(17.4873515388116,16.9733127085343,1.63135328959917));
#137675=CARTESIAN_POINT('Ctrl Pts',(17.4110533973333,17.0175671442341,1.63573972905106));
#137676=CARTESIAN_POINT('Ctrl Pts',(17.3373445043262,17.0655505304473,1.64012616850296));
#137677=CARTESIAN_POINT('Ctrl Pts',(17.263635611319,17.1135339166605,1.64451260795485));
#137678=CARTESIAN_POINT('Ctrl Pts',(17.1925163913081,17.1652458506637,1.64889904740675));
#137679=CARTESIAN_POINT('Ctrl Pts',(17.1243635063082,17.2203542861233,1.65328548685865));
#137680=CARTESIAN_POINT('Ctrl Pts',(17.0601943716838,17.27224146029,1.65741552513525));
#137681=CARTESIAN_POINT('Ctrl Pts',(16.9984022161797,17.3273436089106,1.66154556341186));
#137682=CARTESIAN_POINT('Ctrl Pts',(16.9393333495131,17.3854119814071,1.66567560168847));
#137683=CARTESIAN_POINT('Ctrl Pts',(16.8791242534032,17.4446012704164,1.66988536370976));
#137684=CARTESIAN_POINT('Ctrl Pts',(16.8217451257373,17.5068722664466,1.67409512573104));
#137685=CARTESIAN_POINT('Ctrl Pts',(16.7675298311078,17.5719163917429,1.67830488775233));
#137686=CARTESIAN_POINT('Ctrl Pts',(16.7144792339723,17.6355631857096,1.6824242122078));
#137687=CARTESIAN_POINT('Ctrl Pts',(16.6644582224381,17.701864774228,1.68654353666328));
#137688=CARTESIAN_POINT('Ctrl Pts',(16.6177431433907,17.7704942149182,1.69066286111875));
#137689=CARTESIAN_POINT('Ctrl Pts',(16.5710563616802,17.8390820837981,1.69477969032184));
#137690=CARTESIAN_POINT('Ctrl Pts',(16.5276718045391,17.9099946168291,1.69889651952493));
#137691=CARTESIAN_POINT('Ctrl Pts',(16.4878244173549,17.9828732752973,1.70301334872802));
#137692=CARTESIAN_POINT('Ctrl Pts',(16.4479884744815,18.0557310027567,1.70712899556318));
#137693=CARTESIAN_POINT('Ctrl Pts',(16.4116879110196,18.1305533194009,1.71124464239834));
#137694=CARTESIAN_POINT('Ctrl Pts',(16.3791125474012,18.206955635645,1.7153602892335));
#137695=CARTESIAN_POINT('Ctrl Pts',(16.3452431867613,18.2863928948241,1.71963942264732));
#137696=CARTESIAN_POINT('Ctrl Pts',(16.3154014151592,18.367537815818,1.72391855606114));
#137697=CARTESIAN_POINT('Ctrl Pts',(16.2897454150196,18.4499352696373,1.72819768947497));
#137698=CARTESIAN_POINT('Ctrl Pts',(16.265047031356,18.529257218353,1.73231710318821));
#137699=CARTESIAN_POINT('Ctrl Pts',(16.2442275674438,18.6097393677812,1.73643651690145));
#137700=CARTESIAN_POINT('Ctrl Pts',(16.2273766224859,18.690962267427,1.74055593061469));
#137701=CARTESIAN_POINT('Ctrl Pts',(16.2105163819041,18.7722299727216,1.74467761675363));
#137702=CARTESIAN_POINT('Ctrl Pts',(16.1976290874525,18.8542387741595,1.74879930289257));
#137703=CARTESIAN_POINT('Ctrl Pts',(16.1887526583662,18.9365624480759,1.75292098903151));
#137704=CARTESIAN_POINT('Ctrl Pts',(16.1798641545679,19.018998107865,1.75704828194913));
#137705=CARTESIAN_POINT('Ctrl Pts',(16.1749974202386,19.1017490235124,1.76117557486675));
#137706=CARTESIAN_POINT('Ctrl Pts',(16.1741383212113,19.1843882456639,1.76530286778437));
#137707=CARTESIAN_POINT('Ctrl Pts',(16.1740406969644,19.1937790045501,1.76577187525603));
#137708=CARTESIAN_POINT('Ctrl Pts',(16.173994768433,19.2031683266851,1.7662408827277));
#137709=CARTESIAN_POINT('Ctrl Pts',(16.1740004726294,19.2125555906437,1.76670989019937));
#137710=CARTESIAN_POINT('Ctrl Pts',(16.1740004726297,19.2125555912267,1.7667098902285));
#137711=CARTESIAN_POINT('Ctrl Pts',(16.1740562220857,19.3043011464569,1.77129369133236));
#137712=CARTESIAN_POINT('Ctrl Pts',(16.1790436176611,19.3958958077681,1.77587749243622));
#137713=CARTESIAN_POINT('Ctrl Pts',(16.188916332748,19.4869513121681,1.78046129354008));
#137714=CARTESIAN_POINT('Ctrl Pts',(16.1979293239672,19.5700776309547,1.78464593360467));
#137715=CARTESIAN_POINT('Ctrl Pts',(16.2110359189468,19.6529166093026,1.78883057366926));
#137716=CARTESIAN_POINT('Ctrl Pts',(16.2282088654964,19.7350331957452,1.79301521373385));
#137717=CARTESIAN_POINT('Ctrl Pts',(16.2453573687607,19.8170329007231,1.79719389754915));
#137718=CARTESIAN_POINT('Ctrl Pts',(16.2665606336754,19.898311809733,1.80137258136445));
#137719=CARTESIAN_POINT('Ctrl Pts',(16.2917396796525,19.9784402437038,1.80555126517975));
#137720=CARTESIAN_POINT('Ctrl Pts',(16.3173699981905,20.0600047830626,1.80980484163982));
#137721=CARTESIAN_POINT('Ctrl Pts',(16.3471199654275,20.1403767219199,1.8140584180999));
#137722=CARTESIAN_POINT('Ctrl Pts',(16.3808518403883,20.2191139513548,1.81831199455997));
#137723=CARTESIAN_POINT('Ctrl Pts',(16.4139298144973,20.2963248398595,1.82248311437409));
#137724=CARTESIAN_POINT('Ctrl Pts',(16.450836503808,20.3719633895875,1.82665423418821));
#137725=CARTESIAN_POINT('Ctrl Pts',(16.4913923918018,20.4456299508969,1.83082535400233));
#137726=CARTESIAN_POINT('Ctrl Pts',(16.5319346711508,20.5192717931798,1.8349950741852));
#137727=CARTESIAN_POINT('Ctrl Pts',(16.5761234956298,20.5909425585429,1.83916479436806));
#137728=CARTESIAN_POINT('Ctrl Pts',(16.6237330294819,20.6602664741656,1.84333451455093));
#137729=CARTESIAN_POINT('Ctrl Pts',(16.671340869397,20.7295879232582,1.84750408637604));
#137730=CARTESIAN_POINT('Ctrl Pts',(16.7223689155627,20.7965623098985,1.85167365820116));
#137731=CARTESIAN_POINT('Ctrl Pts',(16.7765483378666,20.8608433229889,1.85584323002627));
#137732=CARTESIAN_POINT('Ctrl Pts',(16.8326324731959,20.9273841771355,1.86015938587588));
#137733=CARTESIAN_POINT('Ctrl Pts',(16.8920933523659,20.9910383498724,1.86447554172548));
#137734=CARTESIAN_POINT('Ctrl Pts',(16.9545891221584,21.0514610639237,1.86879169757509));
#137735=CARTESIAN_POINT('Ctrl Pts',(17.0150492802823,21.1099156898598,1.872967267634));
#137736=CARTESIAN_POINT('Ctrl Pts',(17.0783492738879,21.1653458606137,1.87714283769291));
#137737=CARTESIAN_POINT('Ctrl Pts',(17.1441452212348,21.2174799481773,1.88131840775181));
#137738=CARTESIAN_POINT('Ctrl Pts',(17.2132640592835,21.2722469619589,1.88570485649677));
#137739=CARTESIAN_POINT('Ctrl Pts',(17.2851371185139,21.323375865423,1.89009130524172));
#137740=CARTESIAN_POINT('Ctrl Pts',(17.3593324933327,21.3706039558477,1.89447775398667));
#137741=CARTESIAN_POINT('Ctrl Pts',(17.4335278681516,21.4178320462725,1.89886420273162));
#137742=CARTESIAN_POINT('Ctrl Pts',(17.5100450161993,21.4611591039616,1.90325065147657));
#137743=CARTESIAN_POINT('Ctrl Pts',(17.5884257348941,21.5003797420103,1.90763710022152));
#137744=CARTESIAN_POINT('Ctrl Pts',(17.6632002791351,21.5377958997562,1.91182173531038));
#137745=CARTESIAN_POINT('Ctrl Pts',(17.7399490034729,21.5716144630813,1.91600637039924));
#137746=CARTESIAN_POINT('Ctrl Pts',(17.818291348554,21.6016228614457,1.9201910054881));
#137747=CARTESIAN_POINT('Ctrl Pts',(17.8965221835546,21.6315885467804,1.92436968429629));
#137748=CARTESIAN_POINT('Ctrl Pts',(17.9763417077984,21.6577546763325,1.92854836310447));
#137749=CARTESIAN_POINT('Ctrl Pts',(18.0573458795764,21.679955082887,1.93272704191266));
#137750=CARTESIAN_POINT('Ctrl Pts',(18.1398019751846,21.7025534109142,1.93698061962059));
#137751=CARTESIAN_POINT('Ctrl Pts',(18.22348517397,21.7210422324029,1.94123419732852));
#137752=CARTESIAN_POINT('Ctrl Pts',(18.3079491747639,21.7352980597219,1.94548777503645));
#137753=CARTESIAN_POINT('Ctrl Pts',(18.3907756952125,21.7492775132387,1.94965888980362));
#137754=CARTESIAN_POINT('Ctrl Pts',(18.4743525389348,21.759186555656,1.95383000457078));
#137755=CARTESIAN_POINT('Ctrl Pts',(18.5582464958671,21.7649598089604,1.95800111933795));
#137756=CARTESIAN_POINT('Ctrl Pts',(18.6421123018319,21.7707311250256,1.96217083447015));
#137757=CARTESIAN_POINT('Ctrl Pts',(18.7262945511122,21.772369376577,1.96634054960234));
#137758=CARTESIAN_POINT('Ctrl Pts',(18.8103550385056,21.769861056817,1.97051026473454));
#137759=CARTESIAN_POINT('Ctrl Pts',(18.8944125351025,21.7673528263009,1.97467983151203));
#137760=CARTESIAN_POINT('Ctrl Pts',(18.9783478186234,21.7606983323763,1.97884939828952));
#137761=CARTESIAN_POINT('Ctrl Pts',(19.0617241844592,21.7499361667676,1.983018965067));
#137762=CARTESIAN_POINT('Ctrl Pts',(19.1480319248283,21.7387956212922,1.98733512688666));
#137763=CARTESIAN_POINT('Ctrl Pts',(19.2337401905613,21.7232532494629,1.99165128870633));
#137764=CARTESIAN_POINT('Ctrl Pts',(19.3183740371403,21.7034098749436,1.99596745052599));
#137765=CARTESIAN_POINT('Ctrl Pts',(19.4002509797481,21.6842128881312,2.00014301559692));
#137766=CARTESIAN_POINT('Ctrl Pts',(19.4811219860911,21.6609909777928,2.00431858066786));
#137767=CARTESIAN_POINT('Ctrl Pts',(19.5605725242402,21.6338862668667,2.00849414573879));
#137768=CARTESIAN_POINT('Ctrl Pts',(19.6440358680187,21.6054125792273,2.01288060593282));
#137769=CARTESIAN_POINT('Ctrl Pts',(19.7259309366151,21.572653764432,2.01726706612684));
#137770=CARTESIAN_POINT('Ctrl Pts',(19.8058030522818,21.5358307932233,2.02165352632086));
#137771=CARTESIAN_POINT('Ctrl Pts',(19.8856751679486,21.4990078220147,2.02603998651489));
#137772=CARTESIAN_POINT('Ctrl Pts',(19.9635238523773,21.4581210315221,2.03042644670891));
#137773=CARTESIAN_POINT('Ctrl Pts',(20.0389283879064,21.4134445287989,2.03481290690294));
#137774=CARTESIAN_POINT('Ctrl Pts',(20.1108634458295,21.3708236600586,2.03899753937791));
#137775=CARTESIAN_POINT('Ctrl Pts',(20.1808420875566,21.3245955126394,2.04318217185287));
#137776=CARTESIAN_POINT('Ctrl Pts',(20.2484795854888,21.274965015483,2.04736680432784));
#137777=CARTESIAN_POINT('Ctrl Pts',(20.316020809252,21.225405161609,2.05154548046162));
#137778=CARTESIAN_POINT('Ctrl Pts',(20.3812271405885,21.1724528472506,2.0557241565954));
#137779=CARTESIAN_POINT('Ctrl Pts',(20.4437401591169,21.1163578635792,2.05990283272918));
#137780=CARTESIAN_POINT('Ctrl Pts',(20.5073737155061,21.0592573845008,2.06415641109815));
#137781=CARTESIAN_POINT('Ctrl Pts',(20.5682160360671,20.9989007052303,2.06840998946712));
#137782=CARTESIAN_POINT('Ctrl Pts',(20.6259217120567,20.9355962528802,2.07266356783608));
#137783=CARTESIAN_POINT('Ctrl Pts',(20.6825086171466,20.8735191179108,2.07683467979915));
#137784=CARTESIAN_POINT('Ctrl Pts',(20.7360790917207,20.8086078455881,2.08100579176223));
#137785=CARTESIAN_POINT('Ctrl Pts',(20.7863436748012,20.7411913084655,2.0851769037253));
#137786=CARTESIAN_POINT('Ctrl Pts',(20.8365913908688,20.6737973939438,2.089346616011));
#137787=CARTESIAN_POINT('Ctrl Pts',(20.8835351438624,20.6039002527225,2.0935163282967));
#137788=CARTESIAN_POINT('Ctrl Pts',(20.9269263844747,20.5318610344297,2.0976860405824));
#137789=CARTESIAN_POINT('Ctrl Pts',(20.9703160808612,20.459824379899,2.10185560447463));
#137790=CARTESIAN_POINT('Ctrl Pts',(21.0101532796088,20.3856461943776,2.10602516836686));
#137791=CARTESIAN_POINT('Ctrl Pts',(21.0462340502372,20.3097145657193,2.11019473225908));
#137792=CARTESIAN_POINT('Ctrl Pts',(21.0835834151515,20.2311131928022,2.11451089736952));
#137793=CARTESIAN_POINT('Ctrl Pts',(21.1169070503632,20.1506332529357,2.11882706247996));
#137794=CARTESIAN_POINT('Ctrl Pts',(21.146032653323,20.0687286746423,2.12314322759041));
#137795=CARTESIAN_POINT('Ctrl Pts',(21.1742094633538,19.989492212262,2.12731878970826));
#137796=CARTESIAN_POINT('Ctrl Pts',(21.1984574605128,19.9089229687612,2.13149435182612));
#137797=CARTESIAN_POINT('Ctrl Pts',(21.2186717693869,19.8274464278522,2.13566991394397));
#137798=CARTESIAN_POINT('Ctrl Pts',(21.2399070877349,19.741854568399,2.14005638055071));
#137799=CARTESIAN_POINT('Ctrl Pts',(21.2566904008882,19.6552619177352,2.14444284715744));
#137800=CARTESIAN_POINT('Ctrl Pts',(21.2689614014552,19.568170397895,2.14882931376417));
#137801=CARTESIAN_POINT('Ctrl Pts',(21.2812324020222,19.4810788780547,2.15321578037091));
#137802=CARTESIAN_POINT('Ctrl Pts',(21.2889911145764,19.3934890737086,2.15760224697764));
#137803=CARTESIAN_POINT('Ctrl Pts',(21.292240293453,19.3059031135093,2.16198871358438));
#137804=CARTESIAN_POINT('Ctrl Pts',(21.2953400676656,19.2223445557526,2.16617348044054));
#137805=CARTESIAN_POINT('Ctrl Pts',(21.2943474565447,19.1384784653558,2.17035824729669));
#137806=CARTESIAN_POINT('Ctrl Pts',(21.2892265251101,19.0547393031703,2.17454301415285));
#137807=CARTESIAN_POINT('Ctrl Pts',(21.2841129263194,18.9711200467996,2.17872178885592));
#137808=CARTESIAN_POINT('Ctrl Pts',(21.2748827772654,18.8876278129311,2.18290056355899));
#137809=CARTESIAN_POINT('Ctrl Pts',(21.2615521105228,18.8046992141384,2.18707933826206));
#137810=CARTESIAN_POINT('Ctrl Pts',(21.248237345914,18.7218695407559,2.19125312811061));
#137811=CARTESIAN_POINT('Ctrl Pts',(21.2308318605463,18.6396026176039,2.19542691795915));
#137812=CARTESIAN_POINT('Ctrl Pts',(21.2094035421096,18.5583306321642,2.1996007078077));
#137813=CARTESIAN_POINT('Ctrl Pts',(21.1879892259254,18.4771117535917,2.20377177030927));
#137814=CARTESIAN_POINT('Ctrl Pts',(21.162557413063,18.3968869653703,2.20794283281085));
#137815=CARTESIAN_POINT('Ctrl Pts',(21.1332269868703,18.3180779062689,2.21211389531242));
#137816=CARTESIAN_POINT('Ctrl Pts',(21.1039069279456,18.2392967033815,2.21628348349098));
#137817=CARTESIAN_POINT('Ctrl Pts',(21.0706911534652,18.1619306662444,2.22045307166954));
#137818=CARTESIAN_POINT('Ctrl Pts',(21.0337478604524,18.0863846087019,2.2246226598481));
#137819=CARTESIAN_POINT('Ctrl Pts',(20.9968065436247,18.0108425922986,2.22879202498541));
#137820=CARTESIAN_POINT('Ctrl Pts',(20.9561383080875,17.93712077445,2.23296139012273));
#137821=CARTESIAN_POINT('Ctrl Pts',(20.9119581930928,17.8656011338119,2.23713075526004));
#137822=CARTESIAN_POINT('Ctrl Pts',(20.8677415457808,17.794022353939,2.24130356802463));
#137823=CARTESIAN_POINT('Ctrl Pts',(20.8200074610593,17.7246497803965,2.24547638078923));
#137824=CARTESIAN_POINT('Ctrl Pts',(20.7690150632332,17.657837518991,2.24964919355382));
#137825=CARTESIAN_POINT('Ctrl Pts',(20.7180006960884,17.5909964725131,2.25382380411293));
#137826=CARTESIAN_POINT('Ctrl Pts',(20.6637255153181,17.5267182882163,2.25799841467205));
#137827=CARTESIAN_POINT('Ctrl Pts',(20.6064883375299,17.4653232184008,2.26217302523117));
#137828=CARTESIAN_POINT('Ctrl Pts',(20.549164702276,17.4038354105723,2.26635394159121));
#137829=CARTESIAN_POINT('Ctrl Pts',(20.4888704631805,17.3452397372343,2.27053485795125));
#137830=CARTESIAN_POINT('Ctrl Pts',(20.4259403387529,17.2898186212383,2.2747157743113));
#137831=CARTESIAN_POINT('Ctrl Pts',(20.3829942581873,17.2519969939294,2.27756900195815));
#137832=CARTESIAN_POINT('Ctrl Pts',(20.3388212989463,17.2156530150771,2.280422229605));
#137833=CARTESIAN_POINT('Ctrl Pts',(20.2935357313021,17.1808649545431,2.28327545725186));
#137834=CARTESIAN_POINT('Origin',(18.734,19.211,-1.76670989022852));
#137835=CARTESIAN_POINT('',(20.2935357313021,17.1808649545432,3.14981136862994));
#137836=CARTESIAN_POINT('',(20.2933493626094,17.1811161618322,3.08342410898731));
#137837=CARTESIAN_POINT('',(20.2935357313021,17.1808649545432,-1.76670989022852));
#137838=CARTESIAN_POINT('',(16.1740010149448,19.2132795868243,2.63329010980609));
#137839=CARTESIAN_POINT('Ctrl Pts',(16.1740010149447,19.2132795868243,2.63329010980609));
#137840=CARTESIAN_POINT('Ctrl Pts',(16.1740928743929,19.3164386732002,2.6384134288319));
#137841=CARTESIAN_POINT('Ctrl Pts',(16.1804238944875,19.4193213099348,2.64353674785771));
#137842=CARTESIAN_POINT('Ctrl Pts',(16.1928719236876,19.5212710102101,2.64866006688352));
#137843=CARTESIAN_POINT('Ctrl Pts',(16.2055250386105,19.6249003681759,2.65386779441843));
#137844=CARTESIAN_POINT('Ctrl Pts',(16.2244983314989,19.7275658814857,2.65907552195333));
#137845=CARTESIAN_POINT('Ctrl Pts',(16.2496149571641,19.8286009706384,2.66428324948824));
#137846=CARTESIAN_POINT('Ctrl Pts',(16.2576437833531,19.8608980307853,2.66594796113282));
#137847=CARTESIAN_POINT('Ctrl Pts',(16.2662999939973,19.8930286552691,2.6676126727774));
#137848=CARTESIAN_POINT('Ctrl Pts',(16.2755767948953,19.9249715292663,2.66927738442198));
#137849=CARTESIAN_POINT('Ctrl Pts',(16.2988961609903,20.0052672671023,2.67346201883521));
#137850=CARTESIAN_POINT('Ctrl Pts',(16.3261969265522,20.084568763058,2.67764665324844));
#137851=CARTESIAN_POINT('Ctrl Pts',(16.3573766633344,20.1624523191503,2.68183128766167));
#137852=CARTESIAN_POINT('Ctrl Pts',(16.3885120196228,20.240225017646,2.68600996576606));
#137853=CARTESIAN_POINT('Ctrl Pts',(16.4235152107072,20.3165833617541,2.69018864387045));
#137854=CARTESIAN_POINT('Ctrl Pts',(16.4622338002162,20.391117932039,2.69436732197484));
#137855=CARTESIAN_POINT('Ctrl Pts',(16.5016463923758,20.4669884804673,2.6986208998552));
#137856=CARTESIAN_POINT('Ctrl Pts',(16.5449087556001,20.5409687666981,2.70287447773556));
#137857=CARTESIAN_POINT('Ctrl Pts',(16.5918084260801,20.6126473381798,2.70712805561591));
#137858=CARTESIAN_POINT('Ctrl Pts',(16.6377988552167,20.6829362811212,2.71129916961483));
#137859=CARTESIAN_POINT('Ctrl Pts',(16.687286554129,20.751011556649,2.71547028361374));
#137860=CARTESIAN_POINT('Ctrl Pts',(16.7400252973105,20.8165107863339,2.71964139761265));
#137861=CARTESIAN_POINT('Ctrl Pts',(16.7927463434995,20.8819880371221,2.72381111195413));
#137862=CARTESIAN_POINT('Ctrl Pts',(16.8487159791041,20.9448906007937,2.72798082629561));
#137863=CARTESIAN_POINT('Ctrl Pts',(16.9076465125811,21.004887660639,2.73215054063709));
#137864=CARTESIAN_POINT('Ctrl Pts',(16.9665749490585,21.0648825855332,2.73632010660235));
#137865=CARTESIAN_POINT('Ctrl Pts',(17.0284637509526,21.1219718845683,2.74048967256761));
#137866=CARTESIAN_POINT('Ctrl Pts',(17.0929880053962,21.1758612250147,2.74465923853288));
#137867=CARTESIAN_POINT('Ctrl Pts',(17.1597808523044,21.2316452475883,2.74897540124709));
#137868=CARTESIAN_POINT('Ctrl Pts',(17.2293975200615,21.2839997657394,2.7532915639613));
#137869=CARTESIAN_POINT('Ctrl Pts',(17.3014414464079,21.3326446428491,2.75760772667551));
#137870=CARTESIAN_POINT('Ctrl Pts',(17.3711385501858,21.3797049187129,2.76178329088849));
#137871=CARTESIAN_POINT('Ctrl Pts',(17.4431067778014,21.4232933214559,2.76595885510147));
#137872=CARTESIAN_POINT('Ctrl Pts',(17.5169602827149,21.4632021060621,2.77013441931445));
#137873=CARTESIAN_POINT('Ctrl Pts',(17.5945439513518,21.5051265878347,2.77452088127928));
#137874=CARTESIAN_POINT('Ctrl Pts',(17.6742078257196,21.5429897170844,2.77890734324411));
#137875=CARTESIAN_POINT('Ctrl Pts',(17.7554809190361,21.5766078305986,2.78329380520893));
#137876=CARTESIAN_POINT('Ctrl Pts',(17.8367540123527,21.6102259441129,2.78768026717376));
#137877=CARTESIAN_POINT('Ctrl Pts',(17.9196357523206,21.639598919772,2.79206672913859));
#137878=CARTESIAN_POINT('Ctrl Pts',(18.0036392138267,21.6646041086574,2.79645319110342));
#137879=CARTESIAN_POINT('Ctrl Pts',(18.0837775523631,21.6884587719788,2.80063782549363));
#137880=CARTESIAN_POINT('Ctrl Pts',(18.1652349468392,21.7084275441979,2.80482245988383));
#137881=CARTESIAN_POINT('Ctrl Pts',(18.247599691841,21.7243672115755,2.80900709427403));
#137882=CARTESIAN_POINT('Ctrl Pts',(18.3298472008232,21.7402841908096,2.81318577235515));
#137883=CARTESIAN_POINT('Ctrl Pts',(18.4129990472136,21.7521833699231,2.81736445043626));
#137884=CARTESIAN_POINT('Ctrl Pts',(18.4966284631471,21.7599713128029,2.82154312851737));
#137885=CARTESIAN_POINT('Ctrl Pts',(18.5817568763298,21.7678988489684,2.82579670640352));
#137886=CARTESIAN_POINT('Ctrl Pts',(18.6673796862237,21.7715661738212,2.83005028428966));
#137887=CARTESIAN_POINT('Ctrl Pts',(18.7530359237116,21.7709292243358,2.83430386217581));
#137888=CARTESIAN_POINT('Ctrl Pts',(18.8370315478211,21.7703046233595,2.83847497615096));
#137889=CARTESIAN_POINT('Ctrl Pts',(18.921058833767,21.7655411558159,2.84264609012612));
#137890=CARTESIAN_POINT('Ctrl Pts',(19.0046798014456,21.7566497098166,2.84681720410127));
#137891=CARTESIAN_POINT('Ctrl Pts',(19.0882727093013,21.7477612474278,2.85098691841887));
#137892=CARTESIAN_POINT('Ctrl Pts',(19.1714591125977,21.7347476061797,2.85515663273647));
#137893=CARTESIAN_POINT('Ctrl Pts',(19.2538051248627,21.7176716243191,2.85932634705406));
#137894=CARTESIAN_POINT('Ctrl Pts',(19.3361482069038,21.7005962500951,2.86349591299536));
#137895=CARTESIAN_POINT('Ctrl Pts',(19.4176505070952,21.6794589169156,2.86766547893665));
#137896=CARTESIAN_POINT('Ctrl Pts',(19.4978886690214,21.654373508357,2.87183504487794));
#137897=CARTESIAN_POINT('Ctrl Pts',(19.5809479058551,21.6284061277425,2.87615120762019));
#137898=CARTESIAN_POINT('Ctrl Pts',(19.6626519528601,21.5982080349117,2.88046737036243));
#137899=CARTESIAN_POINT('Ctrl Pts',(19.7425506078302,21.5639610433336,2.88478353310467));
#137900=CARTESIAN_POINT('Ctrl Pts',(19.8198465724097,21.5308296439505,2.88895909729369));
#137901=CARTESIAN_POINT('Ctrl Pts',(19.8954525574108,21.4939093297994,2.89313466148271));
#137902=CARTESIAN_POINT('Ctrl Pts',(19.9689850307412,21.4534120883203,2.89731022567173));
#137903=CARTESIAN_POINT('Ctrl Pts',(20.0462314546531,21.4108694273588,2.90169668769058));
#137904=CARTESIAN_POINT('Ctrl Pts',(20.1211888996701,21.364379309383,2.90608314970944));
#137905=CARTESIAN_POINT('Ctrl Pts',(20.193447997866,21.3142383463424,2.91046961172829));
#137906=CARTESIAN_POINT('Ctrl Pts',(20.2657070960619,21.2640973833017,2.91485607374715));
#137907=CARTESIAN_POINT('Ctrl Pts',(20.3352674349797,21.2103059903068,2.919242535766));
#137908=CARTESIAN_POINT('Ctrl Pts',(20.401762322946,21.1532072068041,2.92362899778486));
#137909=CARTESIAN_POINT('Ctrl Pts',(20.4651976823984,21.0987356230994,2.92781363217407));
#137910=CARTESIAN_POINT('Ctrl Pts',(20.5260796023552,21.0410515629438,2.93199826656328));
#137911=CARTESIAN_POINT('Ctrl Pts',(20.584064814394,20.9804236865549,2.93618290095249));
#137912=CARTESIAN_POINT('Ctrl Pts',(20.6419674916594,20.919882106445,2.94036157903251));
#137913=CARTESIAN_POINT('Ctrl Pts',(20.6969813355446,20.8564053626881,2.94454025711254));
#137914=CARTESIAN_POINT('Ctrl Pts',(20.7487967797138,20.7903017243247,2.94871893519257));
#137915=CARTESIAN_POINT('Ctrl Pts',(20.8015409785421,20.723013225673,2.95297251307897));
#137916=CARTESIAN_POINT('Ctrl Pts',(20.8509706214137,20.6530030460431,2.95722609096538));
#137917=CARTESIAN_POINT('Ctrl Pts',(20.8967991444563,20.5806349370322,2.96147966885178));
#137918=CARTESIAN_POINT('Ctrl Pts',(20.9417391920986,20.5096698251147,2.96565078282566));
#137919=CARTESIAN_POINT('Ctrl Pts',(20.9832162459024,20.4364378006298,2.96982189679954));
#137920=CARTESIAN_POINT('Ctrl Pts',(21.021002390723,20.361313029061,2.97399301077341));
#137921=CARTESIAN_POINT('Ctrl Pts',(21.0587758560373,20.2862134663357,2.97816272508966));
#137922=CARTESIAN_POINT('Ctrl Pts',(21.0928606655495,20.2092228285369,2.98233243940591));
#137923=CARTESIAN_POINT('Ctrl Pts',(21.1230748017628,20.1307399586743,2.98650215372215));
#137924=CARTESIAN_POINT('Ctrl Pts',(21.153287862827,20.0522598815699,2.99067171966203));
#137925=CARTESIAN_POINT('Ctrl Pts',(21.1796303599629,19.972288107602,2.9948412856019));
#137926=CARTESIAN_POINT('Ctrl Pts',(21.2019688964371,19.8912422555377,2.99901085154177));
#137927=CARTESIAN_POINT('Ctrl Pts',(21.2250928283449,19.8073469311187,3.00332701428548));
#137928=CARTESIAN_POINT('Ctrl Pts',(21.2439258622492,19.7223011025982,3.00764317702919));
#137929=CARTESIAN_POINT('Ctrl Pts',(21.2583771885884,19.6365817309687,3.0119593397729));
#137930=CARTESIAN_POINT('Ctrl Pts',(21.2723577644625,19.5536546590302,3.01613490396034));
#137931=CARTESIAN_POINT('Ctrl Pts',(21.2822377087348,19.4700977247691,3.02031046814778));
#137932=CARTESIAN_POINT('Ctrl Pts',(21.2879876706469,19.3863481627603,3.02448603233521));
#137933=CARTESIAN_POINT('Ctrl Pts',(21.294028049485,19.2983686091941,3.02887249435706));
#137934=CARTESIAN_POINT('Ctrl Pts',(21.295510260803,19.2101770410253,3.03325895637891));
#137935=CARTESIAN_POINT('Ctrl Pts',(21.2924621252161,19.1222782223196,3.03764541840075));
#137936=CARTESIAN_POINT('Ctrl Pts',(21.2894139896292,19.034379403614,3.0420318804226));
#137937=CARTESIAN_POINT('Ctrl Pts',(21.2818356329245,18.9467739058741,3.04641834244444));
#137938=CARTESIAN_POINT('Ctrl Pts',(21.2698170137414,18.859955739515,3.05080480446629));
#137939=CARTESIAN_POINT('Ctrl Pts',(21.2583547009868,18.7771561299731,3.0549882301007));
#137940=CARTESIAN_POINT('Ctrl Pts',(21.2428114366921,18.6947644704986,3.0591716557351));
#137941=CARTESIAN_POINT('Ctrl Pts',(21.223227274647,18.6132144404944,3.06335508136951));
#137942=CARTESIAN_POINT('Ctrl Pts',(21.2036685685073,18.5317704109331,3.06753306929936));
#137943=CARTESIAN_POINT('Ctrl Pts',(21.1800794975097,18.451166282156,3.07171105722921));
#137944=CARTESIAN_POINT('Ctrl Pts',(21.1525516402429,18.3718290022419,3.07588904515905));
#137945=CARTESIAN_POINT('Ctrl Pts',(21.1250513038495,18.2925710394797,3.08006285616094));
#137946=CARTESIAN_POINT('Ctrl Pts',(21.0936201503635,18.2145778427157,3.08423666716283));
#137947=CARTESIAN_POINT('Ctrl Pts',(21.0584001058549,18.1382632438935,3.08841047816471));
#137948=CARTESIAN_POINT('Ctrl Pts',(21.0232047055557,18.0620020440089,3.09258136866283));
#137949=CARTESIAN_POINT('Ctrl Pts',(20.984225873128,17.9874175251834,3.09675225916096));
#137950=CARTESIAN_POINT('Ctrl Pts',(20.9416538964403,17.9149042189978,3.10092314965908));
#137951=CARTESIAN_POINT('Ctrl Pts',(20.8990871157843,17.8423997632687,3.10509353108808));
#137952=CARTESIAN_POINT('Ctrl Pts',(20.8529282822876,17.7719664217416,3.10926391251708));
#137953=CARTESIAN_POINT('Ctrl Pts',(20.8034134872375,17.7039738493179,3.11343429394608));
#137954=CARTESIAN_POINT('Ctrl Pts',(20.7539049126747,17.6359898187238,3.11760415145481));
#137955=CARTESIAN_POINT('Ctrl Pts',(20.7010414902565,17.5704463163578,3.12177400896353));
#137956=CARTESIAN_POINT('Ctrl Pts',(20.6451014451984,17.5076822768019,3.12594386647225));
#137957=CARTESIAN_POINT('Ctrl Pts',(20.589118959079,17.4448706188996,3.13011688760334));
#137958=CARTESIAN_POINT('Ctrl Pts',(20.5300554962174,17.3848429785817,3.13428990873442));
#137959=CARTESIAN_POINT('Ctrl Pts',(20.4682278066193,17.3279031053214,3.13846292986551));
#137960=CARTESIAN_POINT('Ctrl Pts',(20.412181461353,17.2762875295669,3.14224574278699));
#137961=CARTESIAN_POINT('Ctrl Pts',(20.3538643315057,17.2272089688724,3.14602855570846));
#137962=CARTESIAN_POINT('Ctrl Pts',(20.2935357313021,17.1808649545431,3.14981136862994));
#137963=CARTESIAN_POINT('Ctrl Pts',(20.2935357313021,17.1808649545431,2.34989189381266));
#137964=CARTESIAN_POINT('Ctrl Pts',(20.2268473226505,17.1296353792553,2.35406143415155));
#137965=CARTESIAN_POINT('Ctrl Pts',(20.157629382282,17.0816932397055,2.35823097449044));
#137966=CARTESIAN_POINT('Ctrl Pts',(20.086244262461,17.0372853327446,2.36240051482933));
#137967=CARTESIAN_POINT('Ctrl Pts',(20.0113055121266,16.9906667508754,2.36677761951515));
#137968=CARTESIAN_POINT('Ctrl Pts',(19.9339786728819,16.9479437267017,2.37115472420096));
#137969=CARTESIAN_POINT('Ctrl Pts',(19.8547138818835,16.9093483332716,2.37553182888678));
#137970=CARTESIAN_POINT('Ctrl Pts',(19.779100692075,16.8725309674222,2.37970728741321));
#137971=CARTESIAN_POINT('Ctrl Pts',(19.7017246208009,16.8394694658615,2.38388274593965));
#137972=CARTESIAN_POINT('Ctrl Pts',(19.6229967480141,16.8103157679486,2.38805820446608));
#137973=CARTESIAN_POINT('Ctrl Pts',(19.5442131803373,16.7811414456755,2.39223661686));
#137974=CARTESIAN_POINT('Ctrl Pts',(19.4640763462349,16.75588056566,2.39641502925392));
#137975=CARTESIAN_POINT('Ctrl Pts',(19.3830113793374,16.7346348755705,2.40059344164783));
#137976=CARTESIAN_POINT('Ctrl Pts',(19.301820161026,16.7133560972246,2.40477836154422));
#137977=CARTESIAN_POINT('Ctrl Pts',(19.2196983754079,16.6961050747908,2.40896328144061));
#137978=CARTESIAN_POINT('Ctrl Pts',(19.1370795418308,16.682932183869,2.413148201337));
#137979=CARTESIAN_POINT('Ctrl Pts',(19.1253819274855,16.6810670958358,2.41374072457771));
#137980=CARTESIAN_POINT('Ctrl Pts',(19.1136743529045,16.6792836744105,2.41433324781841));
#137981=CARTESIAN_POINT('Ctrl Pts',(19.1019580505852,16.6775819782338,2.41492577105911));
#137982=CARTESIAN_POINT('Ctrl Pts',(19.0192128717126,16.6655639241852,2.41911040544304));
#137983=CARTESIAN_POINT('Ctrl Pts',(18.9357242972397,16.6575816378624,2.42329503982696));
#137984=CARTESIAN_POINT('Ctrl Pts',(18.8519204122533,16.6537173061286,2.42747967421088));
#137985=CARTESIAN_POINT('Ctrl Pts',(18.7682358117202,16.6498584747926,2.43165835228592));
#137986=CARTESIAN_POINT('Ctrl Pts',(18.6842372477564,16.6501059764731,2.43583703036095));
#137987=CARTESIAN_POINT('Ctrl Pts',(18.6003605130585,16.6544905657264,2.44001570843599));
#137988=CARTESIAN_POINT('Ctrl Pts',(18.514980347945,16.6589537456027,2.44426928632368));
#137989=CARTESIAN_POINT('Ctrl Pts',(18.4297268997694,16.6677038557791,2.44852286421137));
#137990=CARTESIAN_POINT('Ctrl Pts',(18.3450626650523,16.6807178518031,2.45277644209906));
#137991=CARTESIAN_POINT('Ctrl Pts',(18.2620398119427,16.6934795460874,2.45694755606873));
#137992=CARTESIAN_POINT('Ctrl Pts',(18.1795840056908,16.7103412009465,2.4611186700384));
#137993=CARTESIAN_POINT('Ctrl Pts',(18.0981270507744,16.7312287217481,2.46528978400808));
#137994=CARTESIAN_POINT('Ctrl Pts',(18.016697429521,16.7521092335416,2.46945949832042));
#137995=CARTESIAN_POINT('Ctrl Pts',(17.9362664391868,16.7770128141615,2.47362921263276));
#137996=CARTESIAN_POINT('Ctrl Pts',(17.857254322942,16.8058145564718,2.4777989269451));
#137997=CARTESIAN_POINT('Ctrl Pts',(17.7782450182824,16.8346152738942,2.48196849288137));
#137998=CARTESIAN_POINT('Ctrl Pts',(17.700654919247,16.8673137188575,2.48613805881764));
#137999=CARTESIAN_POINT('Ctrl Pts',(17.6248864697081,16.9037359975669,2.49030762475391));
#138000=CARTESIAN_POINT('Ctrl Pts',(17.5464540946267,16.9414388388213,2.4946237875028));
#138001=CARTESIAN_POINT('Ctrl Pts',(17.469974326197,16.9831320174923,2.49893995025168));
#138002=CARTESIAN_POINT('Ctrl Pts',(17.3958663510851,17.0285705423446,2.50325611300057));
#138003=CARTESIAN_POINT('Ctrl Pts',(17.3241724357538,17.0725289118538,2.50743167718523));
#138004=CARTESIAN_POINT('Ctrl Pts',(17.2546985266634,17.1199920607125,2.51160724136989));
#138005=CARTESIAN_POINT('Ctrl Pts',(17.1877934784103,17.1706947795505,2.51578280555456));
#138006=CARTESIAN_POINT('Ctrl Pts',(17.1175092148078,17.2239583724964,2.52016926758556));
#138007=CARTESIAN_POINT('Ctrl Pts',(17.0500605848375,17.2807970211555,2.52455572961656));
#138008=CARTESIAN_POINT('Ctrl Pts',(16.9858097729218,17.3408580455087,2.52894219164756));
#138009=CARTESIAN_POINT('Ctrl Pts',(16.9215589610062,17.400919069862,2.53332865367856));
#138010=CARTESIAN_POINT('Ctrl Pts',(16.8605063152545,17.464201999529,2.53771511570955));
#138011=CARTESIAN_POINT('Ctrl Pts',(16.802965079949,17.53031438468,2.54210157774055));
#138012=CARTESIAN_POINT('Ctrl Pts',(16.7485317522924,17.5928559186595,2.54625111891253));
#138013=CARTESIAN_POINT('Ctrl Pts',(16.6970294692197,17.6581717364498,2.55040066008451));
#138014=CARTESIAN_POINT('Ctrl Pts',(16.6487573722079,17.7259534743858,2.55455020125649));
#138015=CARTESIAN_POINT('Ctrl Pts',(16.600549374283,17.7936452069609,2.55869423237573));
#138016=CARTESIAN_POINT('Ctrl Pts',(16.5555633203294,17.8637959851695,2.56283826349497));
#138017=CARTESIAN_POINT('Ctrl Pts',(16.5140597201748,17.9360626862432,2.56698229461421));
#138018=CARTESIAN_POINT('Ctrl Pts',(16.4725982721945,18.0082559913085,2.57112211694382));
#138019=CARTESIAN_POINT('Ctrl Pts',(16.4346124893249,18.0825605501313,2.57526193927342));
#138020=CARTESIAN_POINT('Ctrl Pts',(16.4003201033264,18.1586036203684,2.57940176160303));
#138021=CARTESIAN_POINT('Ctrl Pts',(16.3660518421391,18.2345931940449,2.58353867155343));
#138022=CARTESIAN_POINT('Ctrl Pts',(16.3354720095434,18.3123184246929,2.58767558150382));
#138023=CARTESIAN_POINT('Ctrl Pts',(16.3087521158413,18.3913825890187,2.59181249145422));
#138024=CARTESIAN_POINT('Ctrl Pts',(16.2820372325134,18.4704319276473,2.59594862567298));
#138025=CARTESIAN_POINT('Ctrl Pts',(16.2591810094474,18.5508192612106,2.60008475989173));
#138026=CARTESIAN_POINT('Ctrl Pts',(16.2403061251843,18.6321296702138,2.60422089411049));
#138027=CARTESIAN_POINT('Ctrl Pts',(16.2214331728159,18.7134317568803,2.6083566049849));
#138028=CARTESIAN_POINT('Ctrl Pts',(16.2065408484307,18.7956562735366,2.61249231585931));
#138029=CARTESIAN_POINT('Ctrl Pts',(16.1957010120579,18.878376717874,2.61662802673372));
#138030=CARTESIAN_POINT('Ctrl Pts',(16.1848552750843,18.9611421905962,2.62076598885789));
#138031=CARTESIAN_POINT('Ctrl Pts',(16.1780664813585,19.0444036643639,2.62490395098206));
#138032=CARTESIAN_POINT('Ctrl Pts',(16.175354661978,19.1277291514511,2.62904191310623));
#138033=CARTESIAN_POINT('Ctrl Pts',(16.1744266413965,19.1562442389712,2.63045797866132));
#138034=CARTESIAN_POINT('Ctrl Pts',(16.1739756253558,19.1847668138065,2.63187404421641));
#138035=CARTESIAN_POINT('Ctrl Pts',(16.1740010149441,19.213279586128,2.6332901097715));
#138036=CARTESIAN_POINT('',(16.1740009418753,19.2088040034395,2.56670989022851));
#138037=CARTESIAN_POINT('Ctrl Pts',(20.2935357313021,17.1808649545431,2.28327545725186));
#138038=CARTESIAN_POINT('Ctrl Pts',(20.2623792546742,17.1569307642185,2.28523847825651));
#138039=CARTESIAN_POINT('Ctrl Pts',(20.2306962622582,17.1337328627522,2.28720149926116));
#138040=CARTESIAN_POINT('Ctrl Pts',(20.1985254700647,17.1112940330771,2.28916452026581));
#138041=CARTESIAN_POINT('Ctrl Pts',(20.1299459675149,17.0634604650486,2.29334915467531));
#138042=CARTESIAN_POINT('Ctrl Pts',(20.0588929044646,17.0189012759396,2.2975337890848));
#138043=CARTESIAN_POINT('Ctrl Pts',(19.9857121094414,16.9778818224111,2.3017184234943));
#138044=CARTESIAN_POINT('Ctrl Pts',(19.9126354781723,16.9369207549698,2.30589710159751));
#138045=CARTESIAN_POINT('Ctrl Pts',(19.8374375284665,16.8994896383239,2.31007577970071));
#138046=CARTESIAN_POINT('Ctrl Pts',(19.7604940332793,16.8658113083076,2.31425445780392));
#138047=CARTESIAN_POINT('Ctrl Pts',(19.6821713816824,16.8315293186239,2.31850803568489));
#138048=CARTESIAN_POINT('Ctrl Pts',(19.6020403867561,16.8011362520523,2.32276161356587));
#138049=CARTESIAN_POINT('Ctrl Pts',(19.5205248076185,16.7748188230346,2.32701519144684));
#138050=CARTESIAN_POINT('Ctrl Pts',(19.4405895664632,16.7490116085441,2.33118630545089));
#138051=CARTESIAN_POINT('Ctrl Pts',(19.3593234056723,16.7271235613564,2.33535741945494));
#138052=CARTESIAN_POINT('Ctrl Pts',(19.2771455317487,16.7092820040337,2.33952853345898));
#138053=CARTESIAN_POINT('Ctrl Pts',(19.1949952333547,16.6914464336072,2.34369824780796));
#138054=CARTESIAN_POINT('Ctrl Pts',(19.1119342786025,16.6776547538833,2.34786796215693));
#138055=CARTESIAN_POINT('Ctrl Pts',(19.0283943159519,16.6679836833525,2.3520376765059));
#138056=CARTESIAN_POINT('Ctrl Pts',(18.9448573259619,16.6583129569542,2.35620724248102));
#138057=CARTESIAN_POINT('Ctrl Pts',(18.8608418190422,16.6527626002741,2.36037680845614));
#138058=CARTESIAN_POINT('Ctrl Pts',(18.7767854909837,16.6513575636896,2.36454637443126));
#138059=CARTESIAN_POINT('Ctrl Pts',(18.6897738473637,16.6499031277727,2.36886253714093));
#138060=CARTESIAN_POINT('Ctrl Pts',(18.602718986005,16.6528909431625,2.3731786998506));
#138061=CARTESIAN_POINT('Ctrl Pts',(18.516105438621,16.6602899106089,2.37749486256026));
#138062=CARTESIAN_POINT('Ctrl Pts',(18.4323133171228,16.6674478575809,2.38167042678893));
#138063=CARTESIAN_POINT('Ctrl Pts',(18.3489346599913,16.6787338735485,2.3858459910176));
#138064=CARTESIAN_POINT('Ctrl Pts',(18.2664001913304,16.694067259752,2.39002155524626));
#138065=CARTESIAN_POINT('Ctrl Pts',(18.1796971048655,16.7101750984693,2.39440801719643));
#138066=CARTESIAN_POINT('Ctrl Pts',(18.0939262957202,16.7307497815375,2.39879447914659));
#138067=CARTESIAN_POINT('Ctrl Pts',(18.0095696123178,16.7556383945735,2.40318094109676));
#138068=CARTESIAN_POINT('Ctrl Pts',(17.9252129289154,16.7805270076095,2.40756740304692));
#138069=CARTESIAN_POINT('Ctrl Pts',(17.8422708932813,16.8097292861762,2.41195386499709));
#138070=CARTESIAN_POINT('Ctrl Pts',(17.7611994326656,16.8430348279179,2.41634032694725));
#138071=CARTESIAN_POINT('Ctrl Pts',(17.6838581936306,16.8748079308751,2.42052496109137));
#138072=CARTESIAN_POINT('Ctrl Pts',(17.6079312972171,16.9104332654877,2.42470959523549));
#138073=CARTESIAN_POINT('Ctrl Pts',(17.5338290567806,16.9497636773101,2.4288942293796));
#138074=CARTESIAN_POINT('Ctrl Pts',(17.4598322917951,16.9890381071151,2.43307290721024));
#138075=CARTESIAN_POINT('Ctrl Pts',(17.3876554268513,17.0320069250301,2.43725158504088));
#138076=CARTESIAN_POINT('Ctrl Pts',(17.3176892303787,17.0784747823637,2.44143026287152));
#138077=CARTESIAN_POINT('Ctrl Pts',(17.2464689347497,17.1257755462096,2.44568384081973));
#138078=CARTESIAN_POINT('Ctrl Pts',(17.1775397858983,17.1767018411992,2.44993741876795));
#138079=CARTESIAN_POINT('Ctrl Pts',(17.1112881539821,17.2309984179822,2.45419099671616));
#138080=CARTESIAN_POINT('Ctrl Pts',(17.046320944273,17.2842423455401,2.45836211043189));
#138081=CARTESIAN_POINT('Ctrl Pts',(16.9839287319629,17.3407267365349,2.46253322414762));
#138082=CARTESIAN_POINT('Ctrl Pts',(16.9244454837024,17.4001680220001,2.46670433786335));
#138083=CARTESIAN_POINT('Ctrl Pts',(16.864982195661,17.4595893613273,2.47087405191874));
#138084=CARTESIAN_POINT('Ctrl Pts',(16.80842625819,17.5219652996602,2.47504376597413));
#138085=CARTESIAN_POINT('Ctrl Pts',(16.7550758225251,17.5869744152861,2.47921348002952));
#138086=CARTESIAN_POINT('Ctrl Pts',(16.7017272853287,17.6519812175709,2.48338304570617));
#138087=CARTESIAN_POINT('Ctrl Pts',(16.6515843143223,17.7196206546924,2.48755261138281));
#138088=CARTESIAN_POINT('Ctrl Pts',(16.6049048052609,17.789538198987,2.49172217705945));
#138089=CARTESIAN_POINT('Ctrl Pts',(16.5565840956936,17.8619139677013,2.49603834010689));
#138090=CARTESIAN_POINT('Ctrl Pts',(16.5119752240704,17.9367305827085,2.50035450315433));
#138091=CARTESIAN_POINT('Ctrl Pts',(16.4713143087829,18.0135637959534,2.50467066620176));
#138092=CARTESIAN_POINT('Ctrl Pts',(16.4319779238963,18.087894165226,2.50884623012272));
#138093=CARTESIAN_POINT('Ctrl Pts',(16.3963363916594,18.1641113217507,2.51302179404367));
#138094=CARTESIAN_POINT('Ctrl Pts',(16.3645549999772,18.241809414064,2.51719735796462));
#138095=CARTESIAN_POINT('Ctrl Pts',(16.331168399037,18.3234318687324,2.5215838205753));
#138096=CARTESIAN_POINT('Ctrl Pts',(16.3020423326827,18.4066882445185,2.52597028318598));
#138097=CARTESIAN_POINT('Ctrl Pts',(16.2773090396161,18.491090613224,2.53035674579666));
#138098=CARTESIAN_POINT('Ctrl Pts',(16.2525757465496,18.5754929819294,2.53474320840733));
#138099=CARTESIAN_POINT('Ctrl Pts',(16.2322352869838,18.6610407614778,2.53912967101801));
#138100=CARTESIAN_POINT('Ctrl Pts',(16.2163575306379,18.7472367021162,2.54351613362869));
#138101=CARTESIAN_POINT('Ctrl Pts',(16.1935441105101,18.8710844400618,2.54981867488401));
#138102=CARTESIAN_POINT('Ctrl Pts',(16.179864182312,18.9966631544576,2.55612121613934));
#138103=CARTESIAN_POINT('Ctrl Pts',(16.1755170133968,19.1228818562274,2.56242375739466));
#138104=CARTESIAN_POINT('Ctrl Pts',(16.1745315620438,19.1514941307573,2.56385246833928));
#138105=CARTESIAN_POINT('Ctrl Pts',(16.1740255308992,19.180139168944,2.56528117928389));
#138106=CARTESIAN_POINT('Ctrl Pts',(16.1740009418753,19.2088040034395,2.56670989022851));
#138107=CARTESIAN_POINT('Ctrl Pts',(16.17268506744,19.2088155460777,2.56671052147119));
#138108=CARTESIAN_POINT('Ctrl Pts',(16.1790130470455,19.904586810716,2.60137099441749));
#138109=CARTESIAN_POINT('Ctrl Pts',(16.8320815026504,21.4617759084344,2.67842340292429));
#138110=CARTESIAN_POINT('Ctrl Pts',(19.467398376245,22.1479063348824,2.79786774699155));
#138111=CARTESIAN_POINT('Ctrl Pts',(21.6004480826227,20.1840197191269,2.92504355367299));
#138112=CARTESIAN_POINT('Ctrl Pts',(21.2286613330159,18.0460023426628,3.02022900767158));
#138113=CARTESIAN_POINT('Ctrl Pts',(20.4604812953147,17.3068568960671,3.07302252610969));
#138114=CARTESIAN_POINT('Ctrl Pts',(20.2933493626091,17.181116161832,3.08342410898733));
#138115=CARTESIAN_POINT('Origin',(18.734,19.211,-1.76670989022852));
#138116=CARTESIAN_POINT('',(20.2935357313021,17.1808649545431,3.9499316895625));
#138117=CARTESIAN_POINT('',(20.2935357313021,17.1808649545432,3.88329345306099));
#138118=CARTESIAN_POINT('',(20.2935357313021,17.1808649545432,-1.76670989022852));
#138119=CARTESIAN_POINT('',(16.1740000028035,19.2108801919503,3.43329010980363));
#138120=CARTESIAN_POINT('Ctrl Pts',(16.1740000028035,19.2108801919503,3.43329010980363));
#138121=CARTESIAN_POINT('Ctrl Pts',(16.173996094898,19.2943824116246,3.43746913841142));
#138122=CARTESIAN_POINT('Ctrl Pts',(16.1780820066338,19.3780422026732,3.4416481670192));
#138123=CARTESIAN_POINT('Ctrl Pts',(16.1862780259001,19.4614251239166,3.44582719562699));
#138124=CARTESIAN_POINT('Ctrl Pts',(16.1944623792895,19.5446893613378,3.45000027597725));
#138125=CARTESIAN_POINT('Ctrl Pts',(16.2067451760218,19.6276770564327,3.45417335632751));
#138126=CARTESIAN_POINT('Ctrl Pts',(16.2230946976723,19.7099534675123,3.45834643667778));
#138127=CARTESIAN_POINT('Ctrl Pts',(16.2396087147061,19.7930576758859,3.46256150311587));
#138128=CARTESIAN_POINT('Ctrl Pts',(16.2602717621694,19.8754357285734,3.46677656955397));
#138129=CARTESIAN_POINT('Ctrl Pts',(16.2849973159137,19.9566445891563,3.47099163599206));
#138130=CARTESIAN_POINT('Ctrl Pts',(16.3094325809408,20.0369000225196,3.47515721572334));
#138131=CARTESIAN_POINT('Ctrl Pts',(16.3378353258574,20.1160131199902,3.47932279545462));
#138132=CARTESIAN_POINT('Ctrl Pts',(16.3700710228283,20.1935679573893,3.4834883751859));
#138133=CARTESIAN_POINT('Ctrl Pts',(16.4022960455082,20.2710971138511,3.48765257555782));
#138134=CARTESIAN_POINT('Ctrl Pts',(16.4383513227395,20.3470686092118,3.49181677592973));
#138135=CARTESIAN_POINT('Ctrl Pts',(16.4780536821042,20.4210852080628,3.49598097630165));
#138136=CARTESIAN_POINT('Ctrl Pts',(16.5177548909312,20.495099661981,3.50014505599888));
#138137=CARTESIAN_POINT('Ctrl Pts',(16.561102752779,20.5671589258651,3.50430913569611));
#138138=CARTESIAN_POINT('Ctrl Pts',(16.6078681568273,20.636890383391,3.50847321539335));
#138139=CARTESIAN_POINT('Ctrl Pts',(16.6556310871523,20.7081092430383,3.5127261167099));
#138140=CARTESIAN_POINT('Ctrl Pts',(16.7069587733461,20.7768994173764,3.51697901802646));
#138141=CARTESIAN_POINT('Ctrl Pts',(16.761561649075,20.8428967344168,3.52123191934301));
#138142=CARTESIAN_POINT('Ctrl Pts',(16.8151012611779,20.9076089076679,3.52540200532769));
#138143=CARTESIAN_POINT('Ctrl Pts',(16.8717892886061,20.9696357146529,3.52957209131237));
#138144=CARTESIAN_POINT('Ctrl Pts',(16.9313144499797,21.028670159228,3.53374217729704));
#138145=CARTESIAN_POINT('Ctrl Pts',(16.9926128107595,21.0894631852106,3.53803648627954));
#138146=CARTESIAN_POINT('Ctrl Pts',(17.0569196193486,21.1470823903912,3.54233079526204));
#138147=CARTESIAN_POINT('Ctrl Pts',(17.1238587796064,21.2012374859271,3.54662510424453));
#138148=CARTESIAN_POINT('Ctrl Pts',(17.1907979398641,21.255392581463,3.55091941322703));
#138149=CARTESIAN_POINT('Ctrl Pts',(17.2603689845985,21.3060833143331,3.55521372220952));
#138150=CARTESIAN_POINT('Ctrl Pts',(17.3321657913456,21.3530692919339,3.55950803119202));
#138151=CARTESIAN_POINT('Ctrl Pts',(17.4021289421207,21.3988552702266,3.56369266558496));
#138152=CARTESIAN_POINT('Ctrl Pts',(17.4744678068902,21.4412951999105,3.5678772999779));
#138153=CARTESIAN_POINT('Ctrl Pts',(17.5488288662329,21.4801340603158,3.57206193437084));
#138154=CARTESIAN_POINT('Ctrl Pts',(17.6230840818118,21.5189176384105,3.57624061245467));
#138155=CARTESIAN_POINT('Ctrl Pts',(17.6993553703912,21.5541101172787,3.58041929053851));
#138156=CARTESIAN_POINT('Ctrl Pts',(17.7772605377966,21.5854998634371,3.58459796862235));
#138157=CARTESIAN_POINT('Ctrl Pts',(17.8565620993408,21.6174522482369,3.58885154650781));
#138158=CARTESIAN_POINT('Ctrl Pts',(17.9375562869758,21.6454639674282,3.59310512439327));
#138159=CARTESIAN_POINT('Ctrl Pts',(18.0198140087909,21.6693609112497,3.59735870227874));
#138160=CARTESIAN_POINT('Ctrl Pts',(18.1004770041531,21.6927945661834,3.60152981625657));
#138161=CARTESIAN_POINT('Ctrl Pts',(18.1823545166283,21.7122714336376,3.60570093023441));
#138162=CARTESIAN_POINT('Ctrl Pts',(18.265023760118,21.7276766352526,3.60987204421225));
#138163=CARTESIAN_POINT('Ctrl Pts',(18.3476652631446,21.7430766675033,3.6140417585325));
#138164=CARTESIAN_POINT('Ctrl Pts',(18.4310975176837,21.754407663177,3.61821147285276));
#138165=CARTESIAN_POINT('Ctrl Pts',(18.5148867965887,21.7616056935737,3.62238118717302));
#138166=CARTESIAN_POINT('Ctrl Pts',(18.5986730939115,21.7688034678337,3.62655075311695));
#138167=CARTESIAN_POINT('Ctrl Pts',(18.682815931923,21.7718685307012,3.63072031906087));
#138168=CARTESIAN_POINT('Ctrl Pts',(18.7668770686623,21.7707888776921,3.6348898850048));
#138169=CARTESIAN_POINT('Ctrl Pts',(18.8538936912739,21.769671265415,3.63920604774385));
#138170=CARTESIAN_POINT('Ctrl Pts',(18.9408222331038,21.7641120647909,3.64352221048291));
#138171=CARTESIAN_POINT('Ctrl Pts',(19.0271792931093,21.7541566806023,3.64783837322197));
#138172=CARTESIAN_POINT('Ctrl Pts',(19.1107232809634,21.744525592007,3.65201393741353));
#138173=CARTESIAN_POINT('Ctrl Pts',(19.1937319902683,21.730780456376,3.6561895016051));
#138174=CARTESIAN_POINT('Ctrl Pts',(19.2757772698989,21.7130146661882,3.66036506579667));
#138175=CARTESIAN_POINT('Ctrl Pts',(19.3619664615668,21.6943515681706,3.66475152780947));
#138176=CARTESIAN_POINT('Ctrl Pts',(19.4470917766266,21.6712511277376,3.66913798982227));
#138177=CARTESIAN_POINT('Ctrl Pts',(19.5306760960811,21.6438804323133,3.67352445183507));
#138178=CARTESIAN_POINT('Ctrl Pts',(19.6142604155355,21.616509736889,3.67791091384787));
#138179=CARTESIAN_POINT('Ctrl Pts',(19.6963032254017,21.584869066222,3.68229737586066));
#138180=CARTESIAN_POINT('Ctrl Pts',(19.7763550154477,21.5491822045707,3.68668383787346));
#138181=CARTESIAN_POINT('Ctrl Pts',(19.8527235039631,21.515137348327,3.69086847226646));
#138182=CARTESIAN_POINT('Ctrl Pts',(19.9275644240484,21.4772837399298,3.69505310665946));
#138183=CARTESIAN_POINT('Ctrl Pts',(20.0004719903204,21.4357805954147,3.69923774105245));
#138184=CARTESIAN_POINT('Ctrl Pts',(20.0732757816959,21.3943365254888,3.70341641913635));
#138185=CARTESIAN_POINT('Ctrl Pts',(20.1441512890029,21.3492534633191,3.70759509722024));
#138186=CARTESIAN_POINT('Ctrl Pts',(20.2127136875159,21.3007382205322,3.71177377530413));
#138187=CARTESIAN_POINT('Ctrl Pts',(20.2825050177484,21.2513533768849,3.71602735318958));
#138188=CARTESIAN_POINT('Ctrl Pts',(20.3498990582276,21.1984122950061,3.72028093107503));
#138189=CARTESIAN_POINT('Ctrl Pts',(20.4145171508851,21.1421815309755,3.72453450896047));
#138190=CARTESIAN_POINT('Ctrl Pts',(20.4778824957237,21.0870409100319,3.72870562293838));
#138191=CARTESIAN_POINT('Ctrl Pts',(20.5385782035452,21.0287373383814,3.73287673691628));
#138192=CARTESIAN_POINT('Ctrl Pts',(20.5962788337327,20.9675641307482,3.73704785089418));
#138193=CARTESIAN_POINT('Ctrl Pts',(20.6539601019164,20.9064114503757,3.7412175652145));
#138194=CARTESIAN_POINT('Ctrl Pts',(20.7086479730736,20.8423913807966,3.74538727953482));
#138195=CARTESIAN_POINT('Ctrl Pts',(20.7600539250066,20.7758340145094,3.74955699385514));
#138196=CARTESIAN_POINT('Ctrl Pts',(20.811458047695,20.7092790166189,3.75372655979913));
#138197=CARTESIAN_POINT('Ctrl Pts',(20.8595802028306,20.6401872661395,3.75789612574311));
#138198=CARTESIAN_POINT('Ctrl Pts',(20.9041730844803,20.5689207574072,3.7620656916871));
#138199=CARTESIAN_POINT('Ctrl Pts',(20.9503337968388,20.4951486061425,3.76638185442608));
#138200=CARTESIAN_POINT('Ctrl Pts',(20.9927121598377,20.4190463693452,3.77069801716507));
#138201=CARTESIAN_POINT('Ctrl Pts',(21.0310846958975,20.3410450875402,3.77501417990405));
#138202=CARTESIAN_POINT('Ctrl Pts',(21.0682072506301,20.2655846892878,3.77918974409567));
#138203=CARTESIAN_POINT('Ctrl Pts',(21.1015808067414,20.1883475199542,3.7833653082873));
#138204=CARTESIAN_POINT('Ctrl Pts',(21.1310521424428,20.1097441384567,3.78754087247892));
#138205=CARTESIAN_POINT('Ctrl Pts',(21.1620120052503,20.0271706870183,3.79192733449158));
#138206=CARTESIAN_POINT('Ctrl Pts',(21.1886649090815,19.9430899381566,3.79631379650424));
#138207=CARTESIAN_POINT('Ctrl Pts',(21.2108930925539,19.8579935146962,3.80070025851691));
#138208=CARTESIAN_POINT('Ctrl Pts',(21.2331212760262,19.7728970912358,3.80508672052957));
#138209=CARTESIAN_POINT('Ctrl Pts',(21.2509246961548,19.6867855767775,3.80947318254223));
#138210=CARTESIAN_POINT('Ctrl Pts',(21.2642482087236,19.6001580684646,3.81385964455489));
#138211=CARTESIAN_POINT('Ctrl Pts',(21.2769586867287,19.5175164202231,3.818044278948));
#138212=CARTESIAN_POINT('Ctrl Pts',(21.285639763102,19.4340976099864,3.8222289133411));
#138213=CARTESIAN_POINT('Ctrl Pts',(21.2902056694013,19.3503290196652,3.82641354773421));
#138214=CARTESIAN_POINT('Ctrl Pts',(21.2947650766981,19.2666796635638,3.83059222581821));
#138215=CARTESIAN_POINT('Ctrl Pts',(21.2952209238071,19.1826819717238,3.83477090390222));
#138216=CARTESIAN_POINT('Ctrl Pts',(21.2915388082527,19.0987714640507,3.83894958198623));
#138217=CARTESIAN_POINT('Ctrl Pts',(21.2877906934233,19.0133569208346,3.84320315987165));
#138218=CARTESIAN_POINT('Ctrl Pts',(21.2797547375529,18.9280331946163,3.84745673775707));
#138219=CARTESIAN_POINT('Ctrl Pts',(21.2674501116906,18.843262958658,3.85171031564249));
#138220=CARTESIAN_POINT('Ctrl Pts',(21.2553840350109,18.7601361591377,3.8558814296205));
#138221=CARTESIAN_POINT('Ctrl Pts',(21.2392133934507,18.6775420566421,3.86005254359852));
#138222=CARTESIAN_POINT('Ctrl Pts',(21.2190086634415,18.5959130609251,3.86422365757653));
#138223=CARTESIAN_POINT('Ctrl Pts',(21.1988107133247,18.5143114566061,3.86839337189696));
#138224=CARTESIAN_POINT('Ctrl Pts',(21.1745814736228,18.433674762078,3.87256308621739));
#138225=CARTESIAN_POINT('Ctrl Pts',(21.1464423282957,18.3544242516582,3.87673280053782));
#138226=CARTESIAN_POINT('Ctrl Pts',(21.11830418428,18.2751765613115,3.88090236648192));
#138227=CARTESIAN_POINT('Ctrl Pts',(21.0862565659977,18.1973153902313,3.88507193242603));
#138228=CARTESIAN_POINT('Ctrl Pts',(21.0504699913875,18.1212446242384,3.88924149837013));
#138229=CARTESIAN_POINT('Ctrl Pts',(21.0134252049626,18.0424993039591,3.89355766110898));
#138230=CARTESIAN_POINT('Ctrl Pts',(20.9723738713789,17.9656731098162,3.89787382384784));
#138231=CARTESIAN_POINT('Ctrl Pts',(20.9275574633286,17.8911872651487,3.90218998658669));
#138232=CARTESIAN_POINT('Ctrl Pts',(20.8842009450553,17.8191277890345,3.90636555077843));
#138233=CARTESIAN_POINT('Ctrl Pts',(20.8373211816344,17.749258894982,3.91054111497017));
#138234=CARTESIAN_POINT('Ctrl Pts',(20.7871804520949,17.6819316460225,3.91471667916191));
#138235=CARTESIAN_POINT('Ctrl Pts',(20.734507233507,17.6112038577767,3.91910314117432));
#138236=CARTESIAN_POINT('Ctrl Pts',(20.6782353411158,17.5432816689316,3.92348960318672));
#138237=CARTESIAN_POINT('Ctrl Pts',(20.6187144099126,17.4785302042842,3.92787606519912));
#138238=CARTESIAN_POINT('Ctrl Pts',(20.5591934787095,17.4137787396368,3.93226252721153));
#138239=CARTESIAN_POINT('Ctrl Pts',(20.4964239761435,17.3521983512227,3.93664898922393));
#138240=CARTESIAN_POINT('Ctrl Pts',(20.4307957154099,17.2941055584183,3.94103545123633));
#138241=CARTESIAN_POINT('Ctrl Pts',(20.3864285506525,17.2548326524971,3.94400086401172));
#138242=CARTESIAN_POINT('Ctrl Pts',(20.3406387660481,17.2170491807618,3.94696627678711));
#138243=CARTESIAN_POINT('Ctrl Pts',(20.2935357313021,17.1808649545431,3.9499316895625));
#138244=CARTESIAN_POINT('Ctrl Pts',(20.2935357313021,17.1808649545431,3.14981136862994));
#138245=CARTESIAN_POINT('Ctrl Pts',(20.2269038112494,17.1296787734071,3.15398942161489));
#138246=CARTESIAN_POINT('Ctrl Pts',(20.1578180650956,17.081829284706,3.15816747459984));
#138247=CARTESIAN_POINT('Ctrl Pts',(20.0866541153584,17.0375403513743,3.16234552758478));
#138248=CARTESIAN_POINT('Ctrl Pts',(20.0153772777577,16.9931811622027,3.16653020824394));
#138249=CARTESIAN_POINT('Ctrl Pts',(19.9420160606565,16.9523940190638,3.1707148889031));
#138250=CARTESIAN_POINT('Ctrl Pts',(19.8669695044245,16.9153562771972,3.17489956956227));
#138251=CARTESIAN_POINT('Ctrl Pts',(19.8485514076067,16.9062663902008,3.17592658342408));
#138252=CARTESIAN_POINT('Ctrl Pts',(19.8300318839738,16.8974021064279,3.1769535972859));
#138253=CARTESIAN_POINT('Ctrl Pts',(19.8114169849418,16.8887655931067,3.17798061114772));
#138254=CARTESIAN_POINT('Ctrl Pts',(19.7355693750926,16.8535755610944,3.18216524554016));
#138255=CARTESIAN_POINT('Ctrl Pts',(19.6578547653245,16.8220398921686,3.1863498799326));
#138256=CARTESIAN_POINT('Ctrl Pts',(19.5786598305131,16.7943598176978,3.19053451432504));
#138257=CARTESIAN_POINT('Ctrl Pts',(19.499577619889,16.7667191423869,3.19471319240838));
#138258=CARTESIAN_POINT('Ctrl Pts',(19.4190197000616,16.7429233112,3.19889187049171));
#138259=CARTESIAN_POINT('Ctrl Pts',(19.3373948467029,16.7231264785017,3.20307054857505));
#138260=CARTESIAN_POINT('Ctrl Pts',(19.2543069264953,16.7029748018014,3.20732412646064));
#138261=CARTESIAN_POINT('Ctrl Pts',(19.1701138843274,16.6869671007256,3.21157770434622));
#138262=CARTESIAN_POINT('Ctrl Pts',(19.0852654759066,16.6752136199127,3.21583128223181));
#138263=CARTESIAN_POINT('Ctrl Pts',(19.0020620194663,16.6636880032626,3.22000239620915));
#138264=CARTESIAN_POINT('Ctrl Pts',(18.9182288577837,16.6562531921902,3.22417351018649));
#138265=CARTESIAN_POINT('Ctrl Pts',(18.8342009436324,16.6529617338876,3.22834462416382));
#138266=CARTESIAN_POINT('Ctrl Pts',(18.7502012258591,16.6496713800656,3.23251433848359));
#138267=CARTESIAN_POINT('Ctrl Pts',(18.6660073447032,16.6505216357631,3.23668405280335));
#138268=CARTESIAN_POINT('Ctrl Pts',(18.5820577129979,16.6555130519956,3.24085376712311));
#138269=CARTESIAN_POINT('Ctrl Pts',(18.4981110685808,16.6605042906122,3.24502333306654));
#138270=CARTESIAN_POINT('Ctrl Pts',(18.4144091155048,16.6696363686189,3.24919289900998));
#138271=CARTESIAN_POINT('Ctrl Pts',(18.3313872270485,16.6828578056098,3.25336246495342));
#138272=CARTESIAN_POINT('Ctrl Pts',(18.2454463913856,16.6965440920191,3.25767862769306));
#138273=CARTESIAN_POINT('Ctrl Pts',(18.1602348531237,16.7146125685865,3.26199479043271));
#138274=CARTESIAN_POINT('Ctrl Pts',(18.0762243702395,16.7369484199206,3.26631095317235));
#138275=CARTESIAN_POINT('Ctrl Pts',(17.9949505200243,16.7585566832401,3.27048651736343));
#138276=CARTESIAN_POINT('Ctrl Pts',(17.9148011124186,16.784158383043,3.27466208155451));
#138277=CARTESIAN_POINT('Ctrl Pts',(17.8361862981298,16.813599208156,3.27883764574559));
#138278=CARTESIAN_POINT('Ctrl Pts',(17.7536008364222,16.8445270193708,3.28322410775951));
#138279=CARTESIAN_POINT('Ctrl Pts',(17.6727096022458,16.8796917438774,3.28761056977344));
#138280=CARTESIAN_POINT('Ctrl Pts',(17.5939605452813,16.9188590702828,3.29199703178737));
#138281=CARTESIAN_POINT('Ctrl Pts',(17.5152114883168,16.9580263966883,3.2963834938013));
#138282=CARTESIAN_POINT('Ctrl Pts',(17.4386050767024,17.001195973874,3.30076995581523));
#138283=CARTESIAN_POINT('Ctrl Pts',(17.364553744478,17.0480813808105,3.30515641782915));
#138284=CARTESIAN_POINT('Ctrl Pts',(17.2939096238495,17.092809520654,3.30934105222176));
#138285=CARTESIAN_POINT('Ctrl Pts',(17.2253276726157,17.1410855493988,3.31352568661436));
#138286=CARTESIAN_POINT('Ctrl Pts',(17.1591863942882,17.19269325739,3.31771032100696));
#138287=CARTESIAN_POINT('Ctrl Pts',(17.0931392598839,17.2442275081965,3.32188899909045));
#138288=CARTESIAN_POINT('Ctrl Pts',(17.0295262575255,17.2990837381083,3.32606767717394));
#138289=CARTESIAN_POINT('Ctrl Pts',(16.9686982691563,17.3570016723092,3.33024635525743));
#138290=CARTESIAN_POINT('Ctrl Pts',(16.9067799828036,17.4159577438638,3.33449993314298));
#138291=CARTESIAN_POINT('Ctrl Pts',(16.8477479425957,17.4780861035064,3.33875351102853));
#138292=CARTESIAN_POINT('Ctrl Pts',(16.7919382910611,17.5430682511945,3.34300708891407));
#138293=CARTESIAN_POINT('Ctrl Pts',(16.7372106185328,17.6067905931384,3.34717820289155));
#138294=CARTESIAN_POINT('Ctrl Pts',(16.6855818186072,17.6732566930094,3.35134931686903));
#138295=CARTESIAN_POINT('Ctrl Pts',(16.6373315068437,17.742129267156,3.35552043084651));
#138296=CARTESIAN_POINT('Ctrl Pts',(16.5890973859384,17.810978730445,3.3596901451664));
#138297=CARTESIAN_POINT('Ctrl Pts',(16.5442397654171,17.8822326878121,3.36385985948629));
#138298=CARTESIAN_POINT('Ctrl Pts',(16.5029964131481,17.9555228016989,3.36802957380618));
#138299=CARTESIAN_POINT('Ctrl Pts',(16.4617545284947,18.0288103076089,3.37219913974973));
#138300=CARTESIAN_POINT('Ctrl Pts',(16.4241268812486,18.1041334246491,3.37636870569329));
#138301=CARTESIAN_POINT('Ctrl Pts',(16.3903058438335,18.1810982074242,3.38053827163684));
#138302=CARTESIAN_POINT('Ctrl Pts',(16.3552957004569,18.2607689770351,3.38485443437632));
#138303=CARTESIAN_POINT('Ctrl Pts',(16.3243650403573,18.3421985193633,3.3891705971158));
#138304=CARTESIAN_POINT('Ctrl Pts',(16.2976726756056,18.4249280132142,3.39348675985528));
#138305=CARTESIAN_POINT('Ctrl Pts',(16.2718498118346,18.5049626024846,3.39766232404646));
#138306=CARTESIAN_POINT('Ctrl Pts',(16.2499934356292,18.5862132848944,3.40183788823764));
#138307=CARTESIAN_POINT('Ctrl Pts',(16.2321958025117,18.6682516628952,3.40601345242882));
#138308=CARTESIAN_POINT('Ctrl Pts',(16.2134992532484,18.7544336043728,3.41039991444245));
#138309=CARTESIAN_POINT('Ctrl Pts',(16.1992823307861,18.8414843294194,3.41478637645608));
#138310=CARTESIAN_POINT('Ctrl Pts',(16.1895904829899,18.9289003549305,3.41917283846971));
#138311=CARTESIAN_POINT('Ctrl Pts',(16.1798986351937,19.0163163804415,3.42355930048334));
#138312=CARTESIAN_POINT('Ctrl Pts',(16.174731820223,19.1040971227329,3.42794576249697));
#138313=CARTESIAN_POINT('Ctrl Pts',(16.1740724460423,19.1917407557755,3.43233222451059));
#138314=CARTESIAN_POINT('Ctrl Pts',(16.1740244495167,19.1981204260764,3.43265151959756));
#138315=CARTESIAN_POINT('Ctrl Pts',(16.1740003013853,19.204500276023,3.43297081468453));
#138316=CARTESIAN_POINT('Ctrl Pts',(16.1740000028035,19.2108801913083,3.4332901097715));
#138317=CARTESIAN_POINT('',(16.174394460606,19.210617605254,3.3667098651142));
#138318=CARTESIAN_POINT('Ctrl Pts',(20.2933493626091,17.181116161832,3.08342410898733));
#138319=CARTESIAN_POINT('Ctrl Pts',(19.7793305315605,16.794397093965,3.11541446167017));
#138320=CARTESIAN_POINT('Ctrl Pts',(18.2370602654925,16.3326324953136,3.1897967499135));
#138321=CARTESIAN_POINT('Ctrl Pts',(16.4590845281242,17.5465283070756,3.28422525531049));
#138322=CARTESIAN_POINT('Ctrl Pts',(16.1776267405031,18.8060181972744,3.34666340802465));
#138323=CARTESIAN_POINT('Ctrl Pts',(16.1781627672566,19.2106133248248,3.36670962517832));
#138324=CARTESIAN_POINT('Ctrl Pts',(16.1740000284928,19.2106180532904,3.36670989022851));
#138325=CARTESIAN_POINT('Ctrl Pts',(16.1739869935966,19.297984518944,3.37103154303559));
#138326=CARTESIAN_POINT('Ctrl Pts',(16.1784506871913,19.3852864628672,3.37535319584266));
#138327=CARTESIAN_POINT('Ctrl Pts',(16.1873453738308,19.472055961455,3.37967484864974));
#138328=CARTESIAN_POINT('Ctrl Pts',(16.1966194662204,19.5625266412114,3.38418084296216));
#138329=CARTESIAN_POINT('Ctrl Pts',(16.2107109130556,19.6524179424094,3.38868683727458));
#138330=CARTESIAN_POINT('Ctrl Pts',(16.2295088315793,19.7412112666689,3.39319283158699));
#138331=CARTESIAN_POINT('Ctrl Pts',(16.2475982064586,19.8266577339084,3.39752898296558));
#138332=CARTESIAN_POINT('Ctrl Pts',(16.2700454505064,19.9110871351913,3.40186513434416));
#138333=CARTESIAN_POINT('Ctrl Pts',(16.2967009964589,19.9940540002691,3.40620128572275));
#138334=CARTESIAN_POINT('Ctrl Pts',(16.3233900671467,20.0771252129449,3.41054289068791));
#138335=CARTESIAN_POINT('Ctrl Pts',(16.354297844581,20.1587298407162,3.41488449565307));
#138336=CARTESIAN_POINT('Ctrl Pts',(16.3892268388774,20.2384428562597,3.41922610061823));
#138337=CARTESIAN_POINT('Ctrl Pts',(16.4242296046623,20.318324229007,3.42357687523362));
#138338=CARTESIAN_POINT('Ctrl Pts',(16.4632703651621,20.3963056454692,3.42792764984902));
#138339=CARTESIAN_POINT('Ctrl Pts',(16.5061059491326,20.4719869539808,3.43227842446442));
#138340=CARTESIAN_POINT('Ctrl Pts',(16.5109248522386,20.4805009243496,3.43276787644252));
#138341=CARTESIAN_POINT('Ctrl Pts',(16.5157917376009,20.4889858169829,3.43325732842063));
#138342=CARTESIAN_POINT('Ctrl Pts',(16.5207062260026,20.4974410868688,3.43374678039873));
#138343=CARTESIAN_POINT('Ctrl Pts',(16.5627232942887,20.5697305345463,3.43793141479118));
#138344=CARTESIAN_POINT('Ctrl Pts',(16.608363899273,20.6400938357955,3.44211604918362));
#138345=CARTESIAN_POINT('Ctrl Pts',(16.6574263400685,20.7081445604478,3.44630068357607));
#138346=CARTESIAN_POINT('Ctrl Pts',(16.706418946552,20.7760984233165,3.4504793616594));
#138347=CARTESIAN_POINT('Ctrl Pts',(16.7588234476461,20.8417458779044,3.45465803974274));
#138348=CARTESIAN_POINT('Ctrl Pts',(16.8143930615574,20.9047264247461,3.45883671782607));
#138349=CARTESIAN_POINT('Ctrl Pts',(16.8709587208711,20.9688358526381,3.46309029571166));
#138350=CARTESIAN_POINT('Ctrl Pts',(16.9308038360937,21.0301814068961,3.46734387359725));
#138351=CARTESIAN_POINT('Ctrl Pts',(16.9936228831501,21.0884151089051,3.47159745148283));
#138352=CARTESIAN_POINT('Ctrl Pts',(17.0552240603869,21.1455198369567,3.47576856546018));
#138353=CARTESIAN_POINT('Ctrl Pts',(17.1196845346185,21.1996319675306,3.47993967943753));
#138354=CARTESIAN_POINT('Ctrl Pts',(17.1866778681087,21.250459296029,3.48411079341487));
#138355=CARTESIAN_POINT('Ctrl Pts',(17.2536487213388,21.3012695689266,3.48828050773465));
#138356=CARTESIAN_POINT('Ctrl Pts',(17.3231503796756,21.3487969510059,3.49245022205442));
#138357=CARTESIAN_POINT('Ctrl Pts',(17.394823786903,21.3927898776635,3.49661993637419));
#138358=CARTESIAN_POINT('Ctrl Pts',(17.4664946436828,21.436781238864,3.50078950231762));
#138359=CARTESIAN_POINT('Ctrl Pts',(17.5403367031862,21.4772381547839,3.50495906826106));
#138360=CARTESIAN_POINT('Ctrl Pts',(17.6159635983351,21.513953452537,3.50912863420449));
#138361=CARTESIAN_POINT('Ctrl Pts',(17.694249441846,21.5519596148777,3.51344479694413));
#138362=CARTESIAN_POINT('Ctrl Pts',(17.7744474914061,21.5859559226942,3.51776095968377));
#138363=CARTESIAN_POINT('Ctrl Pts',(17.8561052781563,21.6157662791546,3.52207712242341));
#138364=CARTESIAN_POINT('Ctrl Pts',(17.9351030710676,21.6446055663798,3.5262526866145));
#138365=CARTESIAN_POINT('Ctrl Pts',(18.0154664958611,21.6695273345316,3.53042825080558));
#138366=CARTESIAN_POINT('Ctrl Pts',(18.0967709615464,21.6904231491521,3.53460381499666));
#138367=CARTESIAN_POINT('Ctrl Pts',(18.1821819225493,21.7123743617041,3.53899027701058));
#138368=CARTESIAN_POINT('Ctrl Pts',(18.2686309144573,21.7298821146794,3.5433767390245));
#138369=CARTESIAN_POINT('Ctrl Pts',(18.3556165397335,21.7428819002862,3.54776320103841));
#138370=CARTESIAN_POINT('Ctrl Pts',(18.4426021650096,21.755881685893,3.55214966305233));
#138371=CARTESIAN_POINT('Ctrl Pts',(18.5301238388031,21.7643735238079,3.55653612506624));
#138372=CARTESIAN_POINT('Ctrl Pts',(18.6176794289204,21.7683559636358,3.56092258708016));
#138373=CARTESIAN_POINT('Ctrl Pts',(18.7012064565128,21.7721551655022,3.56510722147276));
#138374=CARTESIAN_POINT('Ctrl Pts',(18.7850752514673,21.771864959913,3.56929185586537));
#138375=CARTESIAN_POINT('Ctrl Pts',(18.8688517103013,21.7674457780733,3.57347649025797));
#138376=CARTESIAN_POINT('Ctrl Pts',(18.9525089237153,21.7630328863919,3.57765516834146));
#138377=CARTESIAN_POINT('Ctrl Pts',(19.0360736066034,21.7545027162291,3.58183384642494));
#138378=CARTESIAN_POINT('Ctrl Pts',(19.119109057661,21.7418676404955,3.58601252450843));
#138379=CARTESIAN_POINT('Ctrl Pts',(19.2036328595138,21.7290060901084,3.59026610239398));
#138380=CARTESIAN_POINT('Ctrl Pts',(19.2876077883165,21.71189100391,3.59451968027953));
#138381=CARTESIAN_POINT('Ctrl Pts',(19.3705758747359,21.690590925073,3.59877325816508));
#138382=CARTESIAN_POINT('Ctrl Pts',(19.4519354628898,21.6697037898308,3.60294437214256));
#138383=CARTESIAN_POINT('Ctrl Pts',(19.5323264333863,21.6447926020538,3.60711548612004));
#138384=CARTESIAN_POINT('Ctrl Pts',(19.6113263938457,21.6159736794114,3.61128660009752));
#138385=CARTESIAN_POINT('Ctrl Pts',(19.6902998451052,21.587164427237,3.61545631441741));
#138386=CARTESIAN_POINT('Ctrl Pts',(19.7678827815191,21.5544502019412,3.6196260287373));
#138387=CARTESIAN_POINT('Ctrl Pts',(19.843669326747,21.5179967458314,3.62379574305719));
#138388=CARTESIAN_POINT('Ctrl Pts',(19.9194531751643,21.4815445868922,3.62796530900074));
#138389=CARTESIAN_POINT('Ctrl Pts',(19.9934403452927,21.4413536618681,3.63213487494429));
#138390=CARTESIAN_POINT('Ctrl Pts',(20.0652475043496,21.3976367055739,3.63630444088784));
#138391=CARTESIAN_POINT('Ctrl Pts',(20.1395793145537,21.3523827150158,3.64062060362732));
#138392=CARTESIAN_POINT('Ctrl Pts',(20.2115745125429,21.3033504035826,3.6449367663668));
#138393=CARTESIAN_POINT('Ctrl Pts',(20.2808401159379,21.2508249081049,3.64925292910628));
#138394=CARTESIAN_POINT('Ctrl Pts',(20.3478493995712,21.2000104251303,3.65342849329747));
#138395=CARTESIAN_POINT('Ctrl Pts',(20.412303860261,21.1459271830854,3.65760405748865));
#138396=CARTESIAN_POINT('Ctrl Pts',(20.4738824987383,21.088873502285,3.66177962167984));
#138397=CARTESIAN_POINT('Ctrl Pts',(20.5385713278795,21.0289381756777,3.66616608369346));
#138398=CARTESIAN_POINT('Ctrl Pts',(20.6000857771511,20.9657248689593,3.67055254570709));
#138399=CARTESIAN_POINT('Ctrl Pts',(20.6581002087315,20.8996202612664,3.67493900772071));
#138400=CARTESIAN_POINT('Ctrl Pts',(20.716114640312,20.8335156535734,3.67932546973434));
#138401=CARTESIAN_POINT('Ctrl Pts',(20.7706287541777,20.7645202473234,3.68371193174797));
#138402=CARTESIAN_POINT('Ctrl Pts',(20.8213695361432,20.6930554711554,3.6880983937616));
#138403=CARTESIAN_POINT('Ctrl Pts',(20.8697756595073,20.6248788952852,3.69228302815506));
#138404=CARTESIAN_POINT('Ctrl Pts',(20.914928230553,20.5542014284548,3.69646766254852));
#138405=CARTESIAN_POINT('Ctrl Pts',(20.956559006204,20.4813666651568,3.70065229694198));
#138406=CARTESIAN_POINT('Ctrl Pts',(20.9981305255987,20.4086355731291,3.70483097502634));
#138407=CARTESIAN_POINT('Ctrl Pts',(21.0361899803433,20.3337536798786,3.70900965311069));
#138408=CARTESIAN_POINT('Ctrl Pts',(21.0705113959643,20.2570948793149,3.71318833119505));
#138409=CARTESIAN_POINT('Ctrl Pts',(21.1054479982897,20.1790620248545,3.71744190908039));
#138410=CARTESIAN_POINT('Ctrl Pts',(21.1365109555626,20.099188327509,3.72169548696572));
#138411=CARTESIAN_POINT('Ctrl Pts',(21.1635100116305,20.0178959681318,3.72594906485105));
#138412=CARTESIAN_POINT('Ctrl Pts',(21.1899856383155,19.9381796197599,3.73012017882943));
#138413=CARTESIAN_POINT('Ctrl Pts',(21.2125533792703,19.857099582236,3.73429129280781));
#138414=CARTESIAN_POINT('Ctrl Pts',(21.2310824062636,19.7750739812547,3.73846240678619));
#138415=CARTESIAN_POINT('Ctrl Pts',(21.2496052156631,19.693075904756,3.742632121107));
#138416=CARTESIAN_POINT('Ctrl Pts',(21.2640919013284,19.6101333433019,3.74680183542781));
#138417=CARTESIAN_POINT('Ctrl Pts',(21.2744621331458,19.526677287831,3.75097154974862));
#138418=CARTESIAN_POINT('Ctrl Pts',(21.2848319959459,19.4432242020848,3.7551411156931));
#138419=CARTESIAN_POINT('Ctrl Pts',(21.2910856402585,19.3592581152789,3.75931068163757));
#138420=CARTESIAN_POINT('Ctrl Pts',(21.293194451632,19.2752164989405,3.76348024758204));
#138421=CARTESIAN_POINT('Ctrl Pts',(21.2953774062114,19.1882200830673,3.76779641032046));
#138422=CARTESIAN_POINT('Ctrl Pts',(21.2931186269949,19.1011432548623,3.77211257305888));
#138423=CARTESIAN_POINT('Ctrl Pts',(21.2864451550249,19.0144707894736,3.77642873579729));
#138424=CARTESIAN_POINT('Ctrl Pts',(21.2799890707009,18.93062167051,3.78060429998941));
#138425=CARTESIAN_POINT('Ctrl Pts',(21.2694016000863,18.847151436045,3.78477986418152));
#138426=CARTESIAN_POINT('Ctrl Pts',(21.2547598325397,18.7644914707931,3.78895542837364));
#138427=CARTESIAN_POINT('Ctrl Pts',(21.2393785441268,18.67765654723,3.7933418903852));
#138428=CARTESIAN_POINT('Ctrl Pts',(21.2195227615801,18.591716466318,3.79772835239677));
#138429=CARTESIAN_POINT('Ctrl Pts',(21.1953413592831,18.5071543400132,3.80211481440834));
#138430=CARTESIAN_POINT('Ctrl Pts',(21.1711599569862,18.4225922137084,3.8065012764199));
#138431=CARTESIAN_POINT('Ctrl Pts',(21.1426531949957,18.3394085662325,3.81088773843147));
#138432=CARTESIAN_POINT('Ctrl Pts',(21.1100276507034,18.2580610706384,3.81527420044303));
#138433=CARTESIAN_POINT('Ctrl Pts',(21.0789046619562,18.1804599993028,3.81945864581514));
#138434=CARTESIAN_POINT('Ctrl Pts',(21.0439180829639,18.1042408407741,3.82364309118724));
#138435=CARTESIAN_POINT('Ctrl Pts',(21.0052116068273,18.0298150707814,3.82782753655935));
#138436=CARTESIAN_POINT('Ctrl Pts',(20.9665579257085,17.9554908163553,3.83200627441451));
#138437=CARTESIAN_POINT('Ctrl Pts',(20.9241946333113,17.8829554976095,3.83618501226968));
#138438=CARTESIAN_POINT('Ctrl Pts',(20.8783138059651,17.8126015226168,3.84036375012484));
#138439=CARTESIAN_POINT('Ctrl Pts',(20.8324875829291,17.7423312782476,3.84453751472404));
#138440=CARTESIAN_POINT('Ctrl Pts',(20.7831523972201,17.6742375999625,3.84871127932324));
#138441=CARTESIAN_POINT('Ctrl Pts',(20.7305459075039,17.6086877834737,3.85288504392244));
#138442=CARTESIAN_POINT('Ctrl Pts',(20.6779756656234,17.543183133256,3.85705593264199));
#138443=CARTESIAN_POINT('Ctrl Pts',(20.6221388841159,17.4802192208246,3.86122682136153));
#138444=CARTESIAN_POINT('Ctrl Pts',(20.5633154981094,17.4201329450859,3.86539771008108));
#138445=CARTESIAN_POINT('Ctrl Pts',(20.5045103316182,17.3600652800204,3.86956730694078));
#138446=CARTESIAN_POINT('Ctrl Pts',(20.4427207177847,17.302873811311,3.87373690380047));
#138447=CARTESIAN_POINT('Ctrl Pts',(20.3782648488343,17.2488600694935,3.87790650066017));
#138448=CARTESIAN_POINT('Ctrl Pts',(20.3505067138017,17.2255988713528,3.87970215146044));
#138449=CARTESIAN_POINT('Ctrl Pts',(20.3222545464684,17.2029265501561,3.88149780226072));
#138450=CARTESIAN_POINT('Ctrl Pts',(20.2935357313021,17.1808649545432,3.88329345306099));
#138451=CARTESIAN_POINT('Origin',(18.734,19.211,-1.76670989022852));
#138452=CARTESIAN_POINT('',(20.2917777939293,17.1831894823609,4.74997346808548));
#138453=CARTESIAN_POINT('',(20.2944552424268,17.1796893591268,4.68319930761182));
#138454=CARTESIAN_POINT('',(20.2935357313021,17.1808649545432,-1.76670989022852));
#138455=CARTESIAN_POINT('',(16.1740009581142,19.2087851537238,4.23329008724976));
#138456=CARTESIAN_POINT('Ctrl Pts',(16.1756127741342,19.2087870016449,4.2332901097715));
#138457=CARTESIAN_POINT('Ctrl Pts',(16.1805387735992,19.8078855990186,4.26304769694121));
#138458=CARTESIAN_POINT('Ctrl Pts',(16.6895187210545,21.2679843244803,4.3351972196714));
#138459=CARTESIAN_POINT('Ctrl Pts',(19.1239734425187,22.2128679703362,4.44973867796207));
#138460=CARTESIAN_POINT('Ctrl Pts',(21.469181135151,20.5079482468907,4.5769144846435));
#138461=CARTESIAN_POINT('Ctrl Pts',(21.340005854912,18.2299561683482,4.67699274801797));
#138462=CARTESIAN_POINT('Ctrl Pts',(20.5375803645769,17.3693101922807,4.73467907583197));
#138463=CARTESIAN_POINT('Ctrl Pts',(20.2917777939292,17.1831894823608,4.74997346808549));
#138464=CARTESIAN_POINT('Ctrl Pts',(20.2935357313021,17.1808649545431,3.9499316895625));
#138465=CARTESIAN_POINT('Ctrl Pts',(20.2271357280555,17.129856930297,3.95411195987788));
#138466=CARTESIAN_POINT('Ctrl Pts',(20.1581247140608,17.082028628014,3.95829223019326));
#138467=CARTESIAN_POINT('Ctrl Pts',(20.086840669308,17.0376564644616,3.96247250050864));
#138468=CARTESIAN_POINT('Ctrl Pts',(20.0156413539939,16.9933370424243,3.966647802083));
#138469=CARTESIAN_POINT('Ctrl Pts',(19.9421747637508,16.952465839246,3.97082310365735));
#138470=CARTESIAN_POINT('Ctrl Pts',(19.8668100020607,16.9152775648543,3.9749984052317));
#138471=CARTESIAN_POINT('Ctrl Pts',(19.7915083801787,16.8781204464094,3.97917020878212));
#138472=CARTESIAN_POINT('Ctrl Pts',(19.7143121580704,16.8446403283179,3.98334201233255));
#138473=CARTESIAN_POINT('Ctrl Pts',(19.6356161995566,16.8150266636089,3.98751381588297));
#138474=CARTESIAN_POINT('Ctrl Pts',(19.5569539799023,16.7854256949937,3.99168383088037));
#138475=CARTESIAN_POINT('Ctrl Pts',(19.4767937305971,16.7596880499491,3.99585384587777));
#138476=CARTESIAN_POINT('Ctrl Pts',(19.3955503834759,16.7379550974309,4.00002386087518));
#138477=CARTESIAN_POINT('Ctrl Pts',(19.3143174962085,16.7162249429696,4.00419333899481));
#138478=CARTESIAN_POINT('Ctrl Pts',(19.2320022326464,16.6984985750593,4.00836281711444));
#138479=CARTESIAN_POINT('Ctrl Pts',(19.1490334553667,16.6848671390985,4.01253229523407));
#138480=CARTESIAN_POINT('Ctrl Pts',(19.0660504717973,16.6712333691015,4.01670248727063));
#138481=CARTESIAN_POINT('Ctrl Pts',(18.982414206433,16.6616959965769,4.02087267930718));
#138482=CARTESIAN_POINT('Ctrl Pts',(18.8985610919208,16.6562946066081,4.02504287134374));
#138483=CARTESIAN_POINT('Ctrl Pts',(18.8146155488082,16.6508872628602,4.0292176600493));
#138484=CARTESIAN_POINT('Ctrl Pts',(18.7304531392929,16.6496250299137,4.03339244875486));
#138485=CARTESIAN_POINT('Ctrl Pts',(18.6465122154691,16.652495380587,4.03756723746043));
#138486=CARTESIAN_POINT('Ctrl Pts',(18.5625187191745,16.6553675289701,4.0417446408496));
#138487=CARTESIAN_POINT('Ctrl Pts',(18.4787474427678,16.6623773741964,4.04592204423879));
#138488=CARTESIAN_POINT('Ctrl Pts',(18.3956311376542,16.6734605396182,4.05009944762796));
#138489=CARTESIAN_POINT('Ctrl Pts',(18.3123782640378,16.6845619158027,4.05428371491377));
#138490=CARTESIAN_POINT('Ctrl Pts',(18.2297829614727,16.6997498876352,4.05846798219958));
#138491=CARTESIAN_POINT('Ctrl Pts',(18.148266884597,16.718909167482,4.06265224948539));
#138492=CARTESIAN_POINT('Ctrl Pts',(18.1121674891097,16.7273938547603,4.06450525229618));
#138493=CARTESIAN_POINT('Ctrl Pts',(18.0762795331303,16.7366567267922,4.06635825510697));
#138494=CARTESIAN_POINT('Ctrl Pts',(18.040638468227,16.7466847226344,4.06821125791776));
#138495=CARTESIAN_POINT('Ctrl Pts',(17.960150287027,16.7693309356085,4.07239589231081));
#138496=CARTESIAN_POINT('Ctrl Pts',(17.8806229756134,16.7959667334644,4.07658052670385));
#138497=CARTESIAN_POINT('Ctrl Pts',(17.8024810747699,16.8264932392761,4.08076516109689));
#138498=CARTESIAN_POINT('Ctrl Pts',(17.7244503992502,16.8569762943851,4.08494383918083));
#138499=CARTESIAN_POINT('Ctrl Pts',(17.6478016421982,16.8913388913935,4.08912251726477));
#138500=CARTESIAN_POINT('Ctrl Pts',(17.5729454850808,16.9294320274457,4.0933011953487));
#138501=CARTESIAN_POINT('Ctrl Pts',(17.496747585145,16.9682079555846,4.09755477323414));
#138502=CARTESIAN_POINT('Ctrl Pts',(17.4224076460745,17.0108493474659,4.10180835111958));
#138503=CARTESIAN_POINT('Ctrl Pts',(17.3503388850128,17.0571471919204,4.10606192900502));
#138504=CARTESIAN_POINT('Ctrl Pts',(17.279667317515,17.1025474623173,4.11023304298296));
#138505=CARTESIAN_POINT('Ctrl Pts',(17.2111800563177,17.1514634154306,4.1144041569609));
#138506=CARTESIAN_POINT('Ctrl Pts',(17.1452415288499,17.2036518686713,4.11857527093885));
#138507=CARTESIAN_POINT('Ctrl Pts',(17.0793251276917,17.2558228095726,4.12274498525921));
#138508=CARTESIAN_POINT('Ctrl Pts',(17.0159561221395,17.3112637844565,4.12691469957958));
#138509=CARTESIAN_POINT('Ctrl Pts',(16.9554677262144,17.3696898818767,4.13108441389994));
#138510=CARTESIAN_POINT('Ctrl Pts',(16.8949814827259,17.4281139002458,4.13525397984399));
#138511=CARTESIAN_POINT('Ctrl Pts',(16.8373759753513,17.4895225097358,4.13942354578803));
#138512=CARTESIAN_POINT('Ctrl Pts',(16.7829482470742,17.5535932733921,4.14359311173208));
#138513=CARTESIAN_POINT('Ctrl Pts',(16.7266069070147,17.6199166860587,4.14790927447101));
#138514=CARTESIAN_POINT('Ctrl Pts',(16.6736713066578,17.6890925366905,4.15222543720993));
#138515=CARTESIAN_POINT('Ctrl Pts',(16.6244248933202,17.7607266225718,4.15654159994886));
#138516=CARTESIAN_POINT('Ctrl Pts',(16.5767826767175,17.8300272356399,4.16071716414053));
#138517=CARTESIAN_POINT('Ctrl Pts',(16.5325931948251,17.9016279637396,4.16489272833221));
#138518=CARTESIAN_POINT('Ctrl Pts',(16.4920674161604,17.9751447133591,4.16906829252389));
#138519=CARTESIAN_POINT('Ctrl Pts',(16.449494776756,18.0523746192327,4.17345475453644));
#138520=CARTESIAN_POINT('Ctrl Pts',(16.4109659295263,18.1317186646457,4.17784121654899));
#138521=CARTESIAN_POINT('Ctrl Pts',(16.3766684749371,18.2127074171643,4.18222767856154));
#138522=CARTESIAN_POINT('Ctrl Pts',(16.342371020348,18.293696169683,4.18661414057409));
#138523=CARTESIAN_POINT('Ctrl Pts',(16.3123050853067,18.3763290580522,4.19100060258664));
#138524=CARTESIAN_POINT('Ctrl Pts',(16.2865973915759,18.4601202011779,4.1953870645992));
#138525=CARTESIAN_POINT('Ctrl Pts',(16.256634152739,18.557781782967,4.20049964335899));
#138526=CARTESIAN_POINT('Ctrl Pts',(16.2324986213398,18.6573099274652,4.20561222211878));
#138527=CARTESIAN_POINT('Ctrl Pts',(16.2143850329176,18.7580757042789,4.21072480087858));
#138528=CARTESIAN_POINT('Ctrl Pts',(16.1965183144929,18.8574681448718,4.21576770033044));
#138529=CARTESIAN_POINT('Ctrl Pts',(16.184510545625,18.9580647258724,4.2208105997823));
#138530=CARTESIAN_POINT('Ctrl Pts',(16.1785021632639,19.0592409592912,4.22585349923416));
#138531=CARTESIAN_POINT('Ctrl Pts',(16.1755487125961,19.1089746473601,4.22833236190603));
#138532=CARTESIAN_POINT('Ctrl Pts',(16.1740441624119,19.1588480714529,4.23081122457789));
#138533=CARTESIAN_POINT('Ctrl Pts',(16.1740009581142,19.2087851537238,4.23329008724976));
#138534=CARTESIAN_POINT('',(16.1740010840393,19.2133559031925,4.16670989022851));
#138535=CARTESIAN_POINT('Ctrl Pts',(20.2935357313021,17.1808649545432,3.88329345306099));
#138536=CARTESIAN_POINT('Ctrl Pts',(20.2268447748805,17.1296334220759,3.88746332109265));
#138537=CARTESIAN_POINT('Ctrl Pts',(20.1576354377003,17.0816982854579,3.89163318912431));
#138538=CARTESIAN_POINT('Ctrl Pts',(20.0862723391846,17.0373027992206,3.89580305715597));
#138539=CARTESIAN_POINT('Ctrl Pts',(20.0148340436107,16.9928605323637,3.8999773190805));
#138540=CARTESIAN_POINT('Ctrl Pts',(19.9412378466428,16.9519656067142,3.90415158100503));
#138541=CARTESIAN_POINT('Ctrl Pts',(19.8658750615154,16.9148164609249,3.90832584292955));
#138542=CARTESIAN_POINT('Ctrl Pts',(19.7904707123725,16.8776468266721,3.91250240703927));
#138543=CARTESIAN_POINT('Ctrl Pts',(19.7132982573728,16.844227268621,3.91667897114898));
#138544=CARTESIAN_POINT('Ctrl Pts',(19.6347689490016,16.8147080101719,3.92085553525869));
#138545=CARTESIAN_POINT('Ctrl Pts',(19.5561040137784,16.7851377694311,3.9250393126529));
#138546=CARTESIAN_POINT('Ctrl Pts',(19.4760779832782,16.7594814223516,3.92922309004711));
#138547=CARTESIAN_POINT('Ctrl Pts',(19.3951169799099,16.7378392007646,3.93340686744132));
#138548=CARTESIAN_POINT('Ctrl Pts',(19.3367851907664,16.7222461441856,3.9364212473357));
#138549=CARTESIAN_POINT('Ctrl Pts',(19.2779683349948,16.708735793246,3.93943562723009));
#138550=CARTESIAN_POINT('Ctrl Pts',(19.2188278686569,16.6973289917387,3.94245000712447));
#138551=CARTESIAN_POINT('Ctrl Pts',(19.1367276562993,16.6814937965827,3.94663464151747));
#138552=CARTESIAN_POINT('Ctrl Pts',(19.0536980417284,16.6696556340513,3.95081927591047));
#138553=CARTESIAN_POINT('Ctrl Pts',(18.9701628470245,16.6619164176737,3.95500391030348));
#138554=CARTESIAN_POINT('Ctrl Pts',(18.8867465543309,16.6541882171128,3.95918258838736));
#138555=CARTESIAN_POINT('Ctrl Pts',(18.8028265650706,16.6505474159413,3.96336126647125));
#138556=CARTESIAN_POINT('Ctrl Pts',(18.7188367813175,16.651044907269,3.96753994455514));
#138557=CARTESIAN_POINT('Ctrl Pts',(18.6333415410517,16.6515513157713,3.97179352244059));
#138558=CARTESIAN_POINT('Ctrl Pts',(18.5477744529634,16.6563459251098,3.97604710032604));
#138559=CARTESIAN_POINT('Ctrl Pts',(18.4625985845179,16.6654271230872,3.98030067821149));
#138560=CARTESIAN_POINT('Ctrl Pts',(18.3790740164904,16.6743322643211,3.98447179218939));
#138561=CARTESIAN_POINT('Ctrl Pts',(18.2959261128669,16.6873592186152,3.98864290616729));
#138562=CARTESIAN_POINT('Ctrl Pts',(18.2135896449265,16.7044539576676,3.9928140201452));
#138563=CARTESIAN_POINT('Ctrl Pts',(18.1312808057832,16.7215429604151,3.99698373446551));
#138564=CARTESIAN_POINT('Ctrl Pts',(18.049783311613,16.7426969435999,4.00115344878583));
#138565=CARTESIAN_POINT('Ctrl Pts',(17.9695227367355,16.7678105857401,4.00532316310615));
#138566=CARTESIAN_POINT('Ctrl Pts',(17.8892650178734,16.7929233342292,4.00949272905015));
#138567=CARTESIAN_POINT('Ctrl Pts',(17.8102445695787,16.8219953233349,4.01366229499415));
#138568=CARTESIAN_POINT('Ctrl Pts',(17.7328714533942,16.8548714735458,4.01783186093816));
#138569=CARTESIAN_POINT('Ctrl Pts',(17.652777993893,16.8889035086419,4.02214802367714));
#138570=CARTESIAN_POINT('Ctrl Pts',(17.5744503476379,16.9270119844461,4.02646418641611));
#138571=CARTESIAN_POINT('Ctrl Pts',(17.4983185918994,16.9689715751859,4.03078034915509));
#138572=CARTESIAN_POINT('Ctrl Pts',(17.4246668200984,17.0095643366696,4.03495591334672));
#138573=CARTESIAN_POINT('Ctrl Pts',(17.3530704495475,17.0537608783684,4.03913147753835));
#138574=CARTESIAN_POINT('Ctrl Pts',(17.2838902366718,17.1013124225847,4.04330704172998));
#138575=CARTESIAN_POINT('Ctrl Pts',(17.2112158957015,17.1512656822582,4.04769350374263));
#138576=CARTESIAN_POINT('Ctrl Pts',(17.141208670627,17.2049214186627,4.05207996575528));
#138577=CARTESIAN_POINT('Ctrl Pts',(17.0742466821562,17.261944094207,4.05646642776793));
#138578=CARTESIAN_POINT('Ctrl Pts',(17.0072846936854,17.3189667697514,4.06085288978059));
#138579=CARTESIAN_POINT('Ctrl Pts',(16.9433683113269,17.3793559306723,4.06523935179324));
#138580=CARTESIAN_POINT('Ctrl Pts',(16.8828286089282,17.4427340469043,4.06962581380589));
#138581=CARTESIAN_POINT('Ctrl Pts',(16.8258191500137,17.5024164036099,4.07375648865202));
#138582=CARTESIAN_POINT('Ctrl Pts',(16.7715797255597,17.5649836670307,4.07788716349815));
#138583=CARTESIAN_POINT('Ctrl Pts',(16.720421868205,17.6301448177784,4.08201783834428));
#138584=CARTESIAN_POINT('Ctrl Pts',(16.6693300782615,17.6952218166721,4.08614317866297));
#138585=CARTESIAN_POINT('Ctrl Pts',(16.6213122506322,17.7628856907896,4.09026851898165));
#138586=CARTESIAN_POINT('Ctrl Pts',(16.5766430483354,17.8328088002369,4.09439385930034));
#138587=CARTESIAN_POINT('Ctrl Pts',(16.5320173182039,17.9026638603613,4.09851518482882));
#138588=CARTESIAN_POINT('Ctrl Pts',(16.4907340001792,17.9747733973529,4.10263651035731));
#138589=CARTESIAN_POINT('Ctrl Pts',(16.4530264539488,18.0487781269419,4.10675783588579));
#138590=CARTESIAN_POINT('Ctrl Pts',(16.4153436115609,18.1227343728356,4.11087646135587));
#138591=CARTESIAN_POINT('Ctrl Pts',(16.3812321043788,18.1985829265154,4.11499508682596));
#138592=CARTESIAN_POINT('Ctrl Pts',(16.350880245421,18.2759383788566,4.11911371229604));
#138593=CARTESIAN_POINT('Ctrl Pts',(16.3205285952524,18.3532932990729,4.12323230943428));
#138594=CARTESIAN_POINT('Ctrl Pts',(16.293936732308,18.4321546644583,4.12735090657251));
#138595=CARTESIAN_POINT('Ctrl Pts',(16.271245067881,18.5121165016089,4.13146950371074));
#138596=CARTESIAN_POINT('Ctrl Pts',(16.2485547151171,18.592073716666,4.13558786277865));
#138597=CARTESIAN_POINT('Ctrl Pts',(16.2297642345969,18.6731308198829,4.13970622184656));
#138598=CARTESIAN_POINT('Ctrl Pts',(16.2149637529306,18.7548680169618,4.14382458091447));
#138599=CARTESIAN_POINT('Ctrl Pts',(16.2001500672814,18.8366781344071,4.14794661410215));
#138600=CARTESIAN_POINT('Ctrl Pts',(16.1893335672673,18.9191690901925,4.15206864728983));
#138601=CARTESIAN_POINT('Ctrl Pts',(16.1825528364003,19.0019130052847,4.15619068047751));
#138602=CARTESIAN_POINT('Ctrl Pts',(16.1767848147302,19.0722990307275,4.15969708372784));
#138603=CARTESIAN_POINT('Ctrl Pts',(16.1739362156169,19.1428678239494,4.16320348697818));
#138604=CARTESIAN_POINT('Ctrl Pts',(16.1740010840393,19.2133559031925,4.16670989022851));
#138605=CARTESIAN_POINT('Ctrl Pts',(16.1740881651155,19.2133565881468,4.16670992828903));
#138606=CARTESIAN_POINT('Ctrl Pts',(16.1722334682522,19.4149927583358,4.17674049235513));
#138607=CARTESIAN_POINT('Ctrl Pts',(16.2862272813843,20.4667260563269,4.22916299198171));
#138608=CARTESIAN_POINT('Ctrl Pts',(17.7370129313198,22.0692002669558,4.32397742716876));
#138609=CARTESIAN_POINT('Ctrl Pts',(20.5976439135897,21.5963979425813,4.4511532338502));
#138610=CARTESIAN_POINT('Ctrl Pts',(21.6812140247095,19.0907282283214,4.57089386066455));
#138611=CARTESIAN_POINT('Ctrl Pts',(20.8466207950879,17.6125715727613,4.64824255191842));
#138612=CARTESIAN_POINT('Ctrl Pts',(20.2944552424269,17.1796893591269,4.68319930761182));
#138613=CARTESIAN_POINT('Origin',(18.734,19.211,-1.76670989022852));
#138614=CARTESIAN_POINT('',(20.2935357313021,17.1808649545431,5.54983331802439));
#138615=CARTESIAN_POINT('',(20.2935357313021,17.1808649545431,5.48336965260678));
#138616=CARTESIAN_POINT('',(20.2935357313021,17.1808649545432,-1.76670989022852));
#138617=CARTESIAN_POINT('',(16.1741505041835,19.2121967451321,5.03329016024809));
#138618=CARTESIAN_POINT('Ctrl Pts',(16.1740002797795,19.2121968587701,5.03329016239966));
#138619=CARTESIAN_POINT('Ctrl Pts',(16.1740435234787,19.3046921980315,5.03786858507908));
#138620=CARTESIAN_POINT('Ctrl Pts',(16.1791038614083,19.3970207371689,5.0424470077585));
#138621=CARTESIAN_POINT('Ctrl Pts',(16.1891023385012,19.4886614710357,5.04702543043792));
#138622=CARTESIAN_POINT('Ctrl Pts',(16.199131888135,19.5805869993194,5.05161808160682));
#138623=CARTESIAN_POINT('Ctrl Pts',(16.2141301908471,19.6718201549905,5.05621073277571));
#138624=CARTESIAN_POINT('Ctrl Pts',(16.2339673694789,19.7618510200861,5.0608033839446));
#138625=CARTESIAN_POINT('Ctrl Pts',(16.2538962421947,19.8522980379953,5.06541726388547));
#138626=CARTESIAN_POINT('Ctrl Pts',(16.2787086950664,19.9415313458139,5.07003114382633));
#138627=CARTESIAN_POINT('Ctrl Pts',(16.3082244096461,20.0290542679085,5.07464502376719));
#138628=CARTESIAN_POINT('Ctrl Pts',(16.331622411587,20.0984363421765,5.07830258630121));
#138629=CARTESIAN_POINT('Ctrl Pts',(16.3579750606107,20.1667439285256,5.08196014883522));
#138630=CARTESIAN_POINT('Ctrl Pts',(16.3871718743355,20.233740313369,5.08561771136923));
#138631=CARTESIAN_POINT('Ctrl Pts',(16.4205760854035,20.310391190454,5.08980234576228));
#138632=CARTESIAN_POINT('Ctrl Pts',(16.457801705802,20.385546444256,5.09398698015532));
#138633=CARTESIAN_POINT('Ctrl Pts',(16.4986929228154,20.4587989704629,5.09817161454837));
#138634=CARTESIAN_POINT('Ctrl Pts',(16.5395259362427,20.5319472307656,5.10235029263232));
#138635=CARTESIAN_POINT('Ctrl Pts',(16.5840139603303,20.6031977447539,5.10652897071627));
#138636=CARTESIAN_POINT('Ctrl Pts',(16.6319534129312,20.6721639695094,5.11070764880021));
#138637=CARTESIAN_POINT('Ctrl Pts',(16.6807521457666,20.7423663642785,5.11496122668565));
#138638=CARTESIAN_POINT('Ctrl Pts',(16.7331270652481,20.8102013305708,5.11921480457108));
#138639=CARTESIAN_POINT('Ctrl Pts',(16.7888147952353,20.8752879916542,5.12346838245652));
#138640=CARTESIAN_POINT('Ctrl Pts',(16.843422909911,20.9391128208063,5.12763949643447));
#138641=CARTESIAN_POINT('Ctrl Pts',(16.9012162179244,21.0002945906744,5.13181061041243));
#138642=CARTESIAN_POINT('Ctrl Pts',(16.9619041398262,21.0585054160556,5.13598172439038));
#138643=CARTESIAN_POINT('Ctrl Pts',(17.0225716973097,21.1166967082321,5.14015143871075));
#138644=CARTESIAN_POINT('Ctrl Pts',(17.0861316079122,21.1719187176575,5.14432115303112));
#138645=CARTESIAN_POINT('Ctrl Pts',(17.1522562065727,21.2238801683047,5.14849086735149));
#138646=CARTESIAN_POINT('Ctrl Pts',(17.2183784522363,21.2758397699405,5.15266043329554));
#138647=CARTESIAN_POINT('Ctrl Pts',(17.2870648422624,21.3245387599152,5.15682999923959));
#138648=CARTESIAN_POINT('Ctrl Pts',(17.3579554657572,21.3697268098999,5.16099956518364));
#138649=CARTESIAN_POINT('Ctrl Pts',(17.431338516121,21.4165036159765,5.16531572792255));
#138650=CARTESIAN_POINT('Ctrl Pts',(17.5070832408527,21.459517715654,5.16963189066148));
#138651=CARTESIAN_POINT('Ctrl Pts',(17.5847604857697,21.4985420299815,5.17394805340039));
#138652=CARTESIAN_POINT('Ctrl Pts',(17.6599074026038,21.5362951313743,5.17812361759207));
#138653=CARTESIAN_POINT('Ctrl Pts',(17.736862419498,21.5703142429023,5.18229918178375));
#138654=CARTESIAN_POINT('Ctrl Pts',(17.8152162748904,21.6004427104398,5.18647474597543));
#138655=CARTESIAN_POINT('Ctrl Pts',(17.8975275972501,21.6320928952489,5.19086120798797));
#138656=CARTESIAN_POINT('Ctrl Pts',(17.9813822273946,21.6594488930309,5.19524767000051));
#138657=CARTESIAN_POINT('Ctrl Pts',(18.0662895457781,21.6823888300554,5.19963413201305));
#138658=CARTESIAN_POINT('Ctrl Pts',(18.1511968641616,21.70532876708,5.20402059402559));
#138659=CARTESIAN_POINT('Ctrl Pts',(18.2371562875637,21.723852595477,5.20840705603813));
#138660=CARTESIAN_POINT('Ctrl Pts',(18.3236691980734,21.7379009939035,5.21279351805067));
#138661=CARTESIAN_POINT('Ctrl Pts',(18.4062015213278,21.7513030046936,5.21697815244372));
#138662=CARTESIAN_POINT('Ctrl Pts',(18.4895447184805,21.7606822624715,5.22116278683676));
#138663=CARTESIAN_POINT('Ctrl Pts',(18.5732721407629,21.7659494232303,5.22534742122981));
#138664=CARTESIAN_POINT('Ctrl Pts',(18.6568803874232,21.7712090868378,5.22952609931376));
#138665=CARTESIAN_POINT('Ctrl Pts',(18.7408713177055,21.7723682508116,5.2337047773977));
#138666=CARTESIAN_POINT('Ctrl Pts',(18.8248097150324,21.7693888671693,5.23788345548165));
#138667=CARTESIAN_POINT('Ctrl Pts',(18.910252647806,21.7663560802164,5.24213703336708));
#138668=CARTESIAN_POINT('Ctrl Pts',(18.9956406698881,21.7590348421053,5.24639061125252));
#138669=CARTESIAN_POINT('Ctrl Pts',(19.0805109637125,21.7474404491387,5.25064418913795));
#138670=CARTESIAN_POINT('Ctrl Pts',(19.1637358812804,21.7360708361044,5.2548153031159));
#138671=CARTESIAN_POINT('Ctrl Pts',(19.2464624890053,21.72059234168,5.25898641709386));
#138672=CARTESIAN_POINT('Ctrl Pts',(19.328257802176,21.7010718191556,5.26315753107181));
#138673=CARTESIAN_POINT('Ctrl Pts',(19.4100256681394,21.6815578469311,5.26732724539218));
#138674=CARTESIAN_POINT('Ctrl Pts',(19.4908624130938,21.658004647022,5.27149695971255));
#138675=CARTESIAN_POINT('Ctrl Pts',(19.570345761113,21.6305300717016,5.27566667403293));
#138676=CARTESIAN_POINT('Ctrl Pts',(19.6498262807736,21.6030564740445,5.27983623997697));
#138677=CARTESIAN_POINT('Ctrl Pts',(19.7279530647407,21.5716619295133,5.28400580592101));
#138678=CARTESIAN_POINT('Ctrl Pts',(19.8043208135646,21.5365135682362,5.28817537186506));
#138679=CARTESIAN_POINT('Ctrl Pts',(19.8833735582273,21.5001294339367,5.29249153460398));
#138680=CARTESIAN_POINT('Ctrl Pts',(19.9605407918122,21.4597228236284,5.2968076973429));
#138681=CARTESIAN_POINT('Ctrl Pts',(20.0353992838381,21.4155316745345,5.30112386008182));
#138682=CARTESIAN_POINT('Ctrl Pts',(20.1078192683599,21.3727800474742,5.3052994242735));
#138683=CARTESIAN_POINT('Ctrl Pts',(20.1780782485913,21.3264869565082,5.30947498846518));
#138684=CARTESIAN_POINT('Ctrl Pts',(20.2458229776825,21.2769117319361,5.31365055265686));
#138685=CARTESIAN_POINT('Ctrl Pts',(20.3169893319923,21.2248325806247,5.3180370146694));
#138686=CARTESIAN_POINT('Ctrl Pts',(20.3853803178148,21.169131389708,5.32242347668194));
#138687=CARTESIAN_POINT('Ctrl Pts',(20.450627895575,21.110154724643,5.32680993869448));
#138688=CARTESIAN_POINT('Ctrl Pts',(20.5158754733353,21.0511780595779,5.33119640070702));
#138689=CARTESIAN_POINT('Ctrl Pts',(20.577979287096,20.9889263848496,5.33558286271956));
#138690=CARTESIAN_POINT('Ctrl Pts',(20.6366195645772,20.923786849695,5.3399693247321));
#138691=CARTESIAN_POINT('Ctrl Pts',(20.6925617159657,20.8616444811129,5.34415395912515));
#138692=CARTESIAN_POINT('Ctrl Pts',(20.7455602793472,20.7966428559979,5.3483385935182));
#138693=CARTESIAN_POINT('Ctrl Pts',(20.7953091936644,20.7290923582294,5.35252322791124));
#138694=CARTESIAN_POINT('Ctrl Pts',(20.8449872965599,20.6616380102333,5.35670190599518));
#138695=CARTESIAN_POINT('Ctrl Pts',(20.891424667568,20.5916423631925,5.36088058407913));
#138696=CARTESIAN_POINT('Ctrl Pts',(20.9343537398779,20.5194507707229,5.36505926216307));
#138697=CARTESIAN_POINT('Ctrl Pts',(20.9780522849564,20.4459651958413,5.36931284004851));
#138698=CARTESIAN_POINT('Ctrl Pts',(21.0181151991572,20.3702045348864,5.37356641793394));
#138699=CARTESIAN_POINT('Ctrl Pts',(21.0543048298795,20.2925662237875,5.37781999581938));
#138700=CARTESIAN_POINT('Ctrl Pts',(21.0897928539919,20.216433082848,5.38199110979733));
#138701=CARTESIAN_POINT('Ctrl Pts',(21.1215562334332,20.1384948820618,5.38616222377528));
#138702=CARTESIAN_POINT('Ctrl Pts',(21.1494168148283,20.0591518794677,5.39033333775324));
#138703=CARTESIAN_POINT('Ctrl Pts',(21.1772680473363,19.9798355011845,5.39450305207361));
#138704=CARTESIAN_POINT('Ctrl Pts',(21.2012189304411,19.899115690981,5.39867276639398));
#138705=CARTESIAN_POINT('Ctrl Pts',(21.2211399893043,19.8174113072851,5.40284248071435));
#138706=CARTESIAN_POINT('Ctrl Pts',(21.2410603392908,19.7357098309817,5.40701204665839));
#138707=CARTESIAN_POINT('Ctrl Pts',(21.2569510420042,19.6530242979868,5.41118161260244));
#138708=CARTESIAN_POINT('Ctrl Pts',(21.2687332465284,19.5697859653663,5.41535117854648));
#138709=CARTESIAN_POINT('Ctrl Pts',(21.2809296988286,19.4836210756564,5.4196673412854));
#138710=CARTESIAN_POINT('Ctrl Pts',(21.2887232939913,19.3968643124031,5.42398350402433));
#138711=CARTESIAN_POINT('Ctrl Pts',(21.2920850129342,19.3100003363693,5.42829966676325));
#138712=CARTESIAN_POINT('Ctrl Pts',(21.2953372242362,19.2259659452185,5.43247523095493));
#138713=CARTESIAN_POINT('Ctrl Pts',(21.2944419142066,19.1418316894466,5.43665079514661));
#138714=CARTESIAN_POINT('Ctrl Pts',(21.2894259327675,19.0580349643244,5.44082635933829));
#138715=CARTESIAN_POINT('Ctrl Pts',(21.2841566060303,18.9700058658239,5.44521282135083));
#138716=CARTESIAN_POINT('Ctrl Pts',(21.2743394628619,18.8823498716688,5.44959928336337));
#138717=CARTESIAN_POINT('Ctrl Pts',(21.2600666971253,18.7955640342066,5.45398574537592));
#138718=CARTESIAN_POINT('Ctrl Pts',(21.2457939313886,18.7087781967445,5.45837220738846));
#138719=CARTESIAN_POINT('Ctrl Pts',(21.2270657409798,18.6228630666792,5.462758669401));
#138720=CARTESIAN_POINT('Ctrl Pts',(21.2040345704695,18.5382970784324,5.46714513141354));
#138721=CARTESIAN_POINT('Ctrl Pts',(21.1820669712702,18.4576363176228,5.47132902816127));
#138722=CARTESIAN_POINT('Ctrl Pts',(21.1561032921526,18.3779026599639,5.475512924909));
#138723=CARTESIAN_POINT('Ctrl Pts',(21.1262387968719,18.2995212351674,5.47969682165673));
#138724=CARTESIAN_POINT('Ctrl Pts',(21.0964141293854,18.2212443411597,5.48387513868927));
#138725=CARTESIAN_POINT('Ctrl Pts',(21.0626991366596,18.1443165254359,5.48805345572181));
#138726=CARTESIAN_POINT('Ctrl Pts',(21.0252393289081,18.0691495992624,5.49223177275434));
#138727=CARTESIAN_POINT('Ctrl Pts',(20.9878182356733,17.9940603577164,5.49640577151794));
#138728=CARTESIAN_POINT('Ctrl Pts',(20.9466602184269,17.9207288006228,5.50057977028155));
#138729=CARTESIAN_POINT('Ctrl Pts',(20.901959036502,17.8495472406105,5.50475376904515));
#138730=CARTESIAN_POINT('Ctrl Pts',(20.8572882174576,17.7784140300401,5.50892493265719));
#138731=CARTESIAN_POINT('Ctrl Pts',(20.8090792576707,17.7094283045818,5.51309609626923));
#138732=CARTESIAN_POINT('Ctrl Pts',(20.7575714330078,17.6429570619672,5.51726725988127));
#138733=CARTESIAN_POINT('Ctrl Pts',(20.7060846236992,17.5765129398283,5.52143672164546));
#138734=CARTESIAN_POINT('Ctrl Pts',(20.6513019074186,17.5125816237505,5.52560618340965));
#138735=CARTESIAN_POINT('Ctrl Pts',(20.5935045656374,17.4514992837814,5.52977564517384));
#138736=CARTESIAN_POINT('Ctrl Pts',(20.5356974931344,17.3904066600305,5.53394580890583));
#138737=CARTESIAN_POINT('Ctrl Pts',(20.4748750940599,17.3321643081518,5.53811597263781));
#138738=CARTESIAN_POINT('Ctrl Pts',(20.4113567585147,17.2770728285003,5.54228613636979));
#138739=CARTESIAN_POINT('Ctrl Pts',(20.3730381658033,17.2438378900763,5.54480186358799));
#138740=CARTESIAN_POINT('Ctrl Pts',(20.3337391477832,17.2117489416272,5.54731759080619));
#138741=CARTESIAN_POINT('Ctrl Pts',(20.2935357313021,17.1808649545431,5.54983331802439));
#138742=CARTESIAN_POINT('Ctrl Pts',(20.2917777939292,17.1831894823608,4.74997346808549));
#138743=CARTESIAN_POINT('Ctrl Pts',(19.8562818492272,16.8534337186942,4.77707101139245));
#138744=CARTESIAN_POINT('Ctrl Pts',(18.4733993778667,16.3463965487828,4.84656049025989));
#138745=CARTESIAN_POINT('Ctrl Pts',(16.5671405518731,17.3473640177625,4.94099937082189));
#138746=CARTESIAN_POINT('Ctrl Pts',(16.1797898343239,18.7088775035926,5.00834070807693));
#138747=CARTESIAN_POINT('Ctrl Pts',(16.1776748250889,19.2121940791439,5.0332901097715));
#138748=CARTESIAN_POINT('',(16.1737368487789,19.2101644346317,4.96670989022851));
#138749=CARTESIAN_POINT('Ctrl Pts',(20.2944552424269,17.1796893591269,4.68319930761182));
#138750=CARTESIAN_POINT('Ctrl Pts',(20.1770115575366,17.0876168239104,4.6906344874789));
#138751=CARTESIAN_POINT('Ctrl Pts',(19.3369083402612,16.541881966795,4.74046160290647));
#138752=CARTESIAN_POINT('Ctrl Pts',(17.2348043502142,16.5812273130942,4.8326806538945));
#138753=CARTESIAN_POINT('Ctrl Pts',(16.1917618195022,18.2701494080764,4.91974900156632));
#138754=CARTESIAN_POINT('Ctrl Pts',(16.169904976237,19.1644257529645,4.96442541367765));
#138755=CARTESIAN_POINT('Ctrl Pts',(16.170099683962,19.2101632476096,4.96670989022851));
#138756=CARTESIAN_POINT('Ctrl Pts',(16.1740001363332,19.210164520558,4.96670989022851));
#138757=CARTESIAN_POINT('Ctrl Pts',(16.1739730621524,19.2931227545131,4.97085977152528));
#138758=CARTESIAN_POINT('Ctrl Pts',(16.1779827035226,19.3762448671897,4.97500965282206));
#138759=CARTESIAN_POINT('Ctrl Pts',(16.1860506816107,19.4591013319584,4.97915953411883));
#138760=CARTESIAN_POINT('Ctrl Pts',(16.194107496698,19.5418431550195,4.98330367356457));
#138761=CARTESIAN_POINT('Ctrl Pts',(16.2062114544436,19.6243195978693,4.9874478130103));
#138762=CARTESIAN_POINT('Ctrl Pts',(16.2223321624273,19.7061006702712,4.99159195245604));
#138763=CARTESIAN_POINT('Ctrl Pts',(16.2384354396281,19.7877933155319,4.99573161098225));
#138764=CARTESIAN_POINT('Ctrl Pts',(16.2585467481878,19.8687916269891,4.99987126950846));
#138765=CARTESIAN_POINT('Ctrl Pts',(16.2825840079949,19.9486717658564,5.00401092803467));
#138766=CARTESIAN_POINT('Ctrl Pts',(16.3066073287287,20.0285055826754,5.00814818599591));
#138767=CARTESIAN_POINT('Ctrl Pts',(16.3345519481597,20.1072220663068,5.01228544395717));
#138768=CARTESIAN_POINT('Ctrl Pts',(16.3662852025772,20.1844097996554,5.01642270191841));
#138769=CARTESIAN_POINT('Ctrl Pts',(16.398009961529,20.2615768686959,5.02055885227397));
#138770=CARTESIAN_POINT('Ctrl Pts',(16.4335211635115,20.3372155671951,5.02469500262952));
#138771=CARTESIAN_POINT('Ctrl Pts',(16.4726375176033,20.4109332161453,5.02883115298508));
#138772=CARTESIAN_POINT('Ctrl Pts',(16.5117556109319,20.4846541428151,5.03296748724695));
#138773=CARTESIAN_POINT('Ctrl Pts',(16.5544789534247,20.5564534375443,5.03710382150882));
#138774=CARTESIAN_POINT('Ctrl Pts',(16.6005803897988,20.6259631680044,5.04124015577069));
#138775=CARTESIAN_POINT('Ctrl Pts',(16.6467285005472,20.6955432720456,5.04538067777221));
#138776=CARTESIAN_POINT('Ctrl Pts',(16.6962612737686,20.7628287929976,5.04952119977374));
#138777=CARTESIAN_POINT('Ctrl Pts',(16.7489086678718,20.827481488638,5.05366172177526));
#138778=CARTESIAN_POINT('Ctrl Pts',(16.8015842228015,20.8921687666805,5.0578044585212));
#138779=CARTESIAN_POINT('Ctrl Pts',(16.8573774008546,20.9542200685977,5.06194719526713));
#138780=CARTESIAN_POINT('Ctrl Pts',(16.9159800655225,21.0133327988588,5.06608993201307));
#138781=CARTESIAN_POINT('Ctrl Pts',(16.9746826938387,21.0725463628314,5.07023973538442));
#138782=CARTESIAN_POINT('Ctrl Pts',(17.0362040315226,21.1288110311767,5.07438953875576));
#138783=CARTESIAN_POINT('Ctrl Pts',(17.1002018437174,21.1818636646221,5.07853934212711));
#138784=CARTESIAN_POINT('Ctrl Pts',(17.1438608301668,21.2180559050325,5.08137031717053));
#138785=CARTESIAN_POINT('Ctrl Pts',(17.1886716656524,21.2527541562677,5.08420129221395));
#138786=CARTESIAN_POINT('Ctrl Pts',(17.2345184376715,21.2858867545572,5.08703226725736));
#138787=CARTESIAN_POINT('Ctrl Pts',(17.3022873074279,21.3348620398235,5.09121690165041));
#138788=CARTESIAN_POINT('Ctrl Pts',(17.3725842232475,21.38060482739,5.09540153604346));
#138789=CARTESIAN_POINT('Ctrl Pts',(17.4450678487464,21.4228440065847,5.09958617043651));
#138790=CARTESIAN_POINT('Ctrl Pts',(17.5174483027762,21.4650230635361,5.10376484852045));
#138791=CARTESIAN_POINT('Ctrl Pts',(17.5920088899904,21.5037081881329,5.10794352660439));
#138792=CARTESIAN_POINT('Ctrl Pts',(17.6683776217254,21.5386702831201,5.11212220468833));
#138793=CARTESIAN_POINT('Ctrl Pts',(17.7461152080915,21.5742590485331,5.11637578257377));
#138794=CARTESIAN_POINT('Ctrl Pts',(17.8257260077702,21.6059897185084,5.12062936045921));
#138795=CARTESIAN_POINT('Ctrl Pts',(17.9067894477689,21.6336685085413,5.12488293834464));
#138796=CARTESIAN_POINT('Ctrl Pts',(17.986281314801,21.6608106912186,5.12905405232259));
#138797=CARTESIAN_POINT('Ctrl Pts',(18.067169544845,21.6840565436589,5.13322516630055));
#138798=CARTESIAN_POINT('Ctrl Pts',(18.1490371223203,21.7032717411504,5.1373962802785));
#138799=CARTESIAN_POINT('Ctrl Pts',(18.2308772283394,21.7224804907968,5.14156599459888));
#138800=CARTESIAN_POINT('Ctrl Pts',(18.3136955816371,21.7376611666003,5.14573570891925));
#138801=CARTESIAN_POINT('Ctrl Pts',(18.3970618790072,21.7487298324727,5.14990542323963));
#138802=CARTESIAN_POINT('Ctrl Pts',(18.4804252098464,21.7597981044744,5.15407498918367));
#138803=CARTESIAN_POINT('Ctrl Pts',(18.5643359898475,21.7667545977695,5.15824455512771));
#138804=CARTESIAN_POINT('Ctrl Pts',(18.6483570024151,21.7695670358552,5.16241412107175));
#138805=CARTESIAN_POINT('Ctrl Pts',(18.7353320901336,21.7724783557944,5.16673028381067));
#138806=CARTESIAN_POINT('Ctrl Pts',(18.822424779069,21.7709487709588,5.17104644654959));
#138807=CARTESIAN_POINT('Ctrl Pts',(18.909150084646,21.7650012623036,5.17536260928851));
#138808=CARTESIAN_POINT('Ctrl Pts',(18.9930503225158,21.7592474931174,5.1795381734802));
#138809=CARTESIAN_POINT('Ctrl Pts',(19.076606282259,21.7493593099811,5.18371373767188));
#138810=CARTESIAN_POINT('Ctrl Pts',(19.1593859487961,21.735410187463,5.18788930186356));
#138811=CARTESIAN_POINT('Ctrl Pts',(19.2463466195001,21.7207565279273,5.1922757638761));
#138812=CARTESIAN_POINT('Ctrl Pts',(19.3324499449363,21.7016210383821,5.19666222588864));
#138813=CARTESIAN_POINT('Ctrl Pts',(19.4172115835233,21.6781485427796,5.20104868790118));
#138814=CARTESIAN_POINT('Ctrl Pts',(19.5019732221104,21.6546760471771,5.20543514991372));
#138815=CARTESIAN_POINT('Ctrl Pts',(19.5853926474676,21.6268668011754,5.20982161192626));
#138816=CARTESIAN_POINT('Ctrl Pts',(19.6670104728636,21.5949235427183,5.2142080739388));
#138817=CARTESIAN_POINT('Ctrl Pts',(19.7448729411266,21.5644500409342,5.21839270833185));
#138818=CARTESIAN_POINT('Ctrl Pts',(19.8213857737636,21.5301011627872,5.22257734272491));
#138819=CARTESIAN_POINT('Ctrl Pts',(19.8961362506934,21.4920171710937,5.22676197711796));
#138820=CARTESIAN_POINT('Ctrl Pts',(19.9707803295714,21.4539873872486,5.2309406552019));
#138821=CARTESIAN_POINT('Ctrl Pts',(20.0436666290094,21.4122332570929,5.23511933328584));
#138822=CARTESIAN_POINT('Ctrl Pts',(20.1144011640627,21.3669435582256,5.23929801136979));
#138823=CARTESIAN_POINT('Ctrl Pts',(20.1864035648208,21.3208420740552,5.24355158925522));
#138824=CARTESIAN_POINT('Ctrl Pts',(20.2561758527105,21.2710772000454,5.24780516714066));
#138825=CARTESIAN_POINT('Ctrl Pts',(20.3233274374462,21.217897679649,5.2520587450261));
#138826=CARTESIAN_POINT('Ctrl Pts',(20.3891771576762,21.1657491480268,5.25622985900405));
#138827=CARTESIAN_POINT('Ctrl Pts',(20.4525065055987,21.1103174864332,5.26040097298199));
#138828=CARTESIAN_POINT('Ctrl Pts',(20.5129768127641,21.0518806315586,5.26457208695994));
#138829=CARTESIAN_POINT('Ctrl Pts',(20.5734268285339,20.993463385735,5.26874180128032));
#138830=CARTESIAN_POINT('Ctrl Pts',(20.6310193783563,20.9320432687884,5.27291151560069));
#138831=CARTESIAN_POINT('Ctrl Pts',(20.6854509703001,20.8679366646057,5.27708122992106));
#138832=CARTESIAN_POINT('Ctrl Pts',(20.7398806253343,20.8038323416111,5.28125079586511));
#138833=CARTESIAN_POINT('Ctrl Pts',(20.7911492490274,20.7370420726791,5.28542036180915));
#138834=CARTESIAN_POINT('Ctrl Pts',(20.8389930448979,20.6679160171168,5.2895899277532));
#138835=CARTESIAN_POINT('Ctrl Pts',(20.8885189696094,20.5963595747172,5.29390609049212));
#138836=CARTESIAN_POINT('Ctrl Pts',(20.9343744515018,20.5223004707788,5.29822225323104));
#138837=CARTESIAN_POINT('Ctrl Pts',(20.9763163009699,20.446158939734,5.30253841596996));
#138838=CARTESIAN_POINT('Ctrl Pts',(21.016891899103,20.3724977110544,5.30671398016164));
#138839=CARTESIAN_POINT('Ctrl Pts',(21.0538047581691,20.2968880859402,5.31088954435332));
#138840=CARTESIAN_POINT('Ctrl Pts',(21.0868828170839,20.2197330910957,5.31506510854501));
#138841=CARTESIAN_POINT('Ctrl Pts',(21.1216315701187,20.1386811808803,5.31945157055755));
#138842=CARTESIAN_POINT('Ctrl Pts',(21.1521477486479,20.0559242327775,5.32383803257009));
#138843=CARTESIAN_POINT('Ctrl Pts',(21.1782909617847,19.9719478918674,5.32822449458262));
#138844=CARTESIAN_POINT('Ctrl Pts',(21.2044341749215,19.8879715509573,5.33261095659516));
#138845=CARTESIAN_POINT('Ctrl Pts',(21.226204352714,19.8027763982256,5.3369974186077));
#138846=CARTESIAN_POINT('Ctrl Pts',(21.2435233083642,19.7168584434175,5.34138388062024));
#138847=CARTESIAN_POINT('Ctrl Pts',(21.2600453931921,19.6348937010711,5.34556851501329));
#138848=CARTESIAN_POINT('Ctrl Pts',(21.2725783676241,19.5519661209787,5.34975314940633));
#138849=CARTESIAN_POINT('Ctrl Pts',(21.2810167729394,19.4684986570166,5.35393778379938));
#138850=CARTESIAN_POINT('Ctrl Pts',(21.2894431672292,19.3851499986583,5.35811646188332));
#138851=CARTESIAN_POINT('Ctrl Pts',(21.2937865229904,19.3012634366145,5.36229513996726));
#138852=CARTESIAN_POINT('Ctrl Pts',(21.293992315731,19.2172724316077,5.36647381805121));
#138853=CARTESIAN_POINT('Ctrl Pts',(21.2942017971586,19.1317759481995,5.37072739593664));
#138854=CARTESIAN_POINT('Ctrl Pts',(21.290123829677,19.0461717133521,5.37498097382208));
#138855=CARTESIAN_POINT('Ctrl Pts',(21.2817561480521,18.9609227917969,5.37923455170752));
#138856=CARTESIAN_POINT('Ctrl Pts',(21.2735506902637,18.8773265869357,5.38340566568547));
#138857=CARTESIAN_POINT('Ctrl Pts',(21.2612204100085,18.7940725203434,5.38757677966342));
#138858=CARTESIAN_POINT('Ctrl Pts',(21.2448156932503,18.7115958004499,5.39174789364137));
#138859=CARTESIAN_POINT('Ctrl Pts',(21.2284164812531,18.6291467564163,5.39591760796174));
#138860=CARTESIAN_POINT('Ctrl Pts',(21.2079456377351,18.5474749918556,5.40008732228212));
#138861=CARTESIAN_POINT('Ctrl Pts',(21.1835049170498,18.4670069480508,5.40425703660249));
#138862=CARTESIAN_POINT('Ctrl Pts',(21.1590650660704,18.3865417676445,5.40842660254653));
#138863=CARTESIAN_POINT('Ctrl Pts',(21.1306557533066,18.3072806627591,5.41259616849058));
#138864=CARTESIAN_POINT('Ctrl Pts',(21.0984286192895,18.2296349790804,5.41676573443462));
#138865=CARTESIAN_POINT('Ctrl Pts',(21.0650684189969,18.1492593689498,5.42108189717354));
#138866=CARTESIAN_POINT('Ctrl Pts',(21.0276171353223,18.0706153771457,5.42539805991246));
#138867=CARTESIAN_POINT('Ctrl Pts',(20.9862964849992,17.9941349525685,5.42971422265138));
#138868=CARTESIAN_POINT('Ctrl Pts',(20.9463218505141,17.9201458697776,5.43388978684306));
#138869=CARTESIAN_POINT('Ctrl Pts',(20.9027263517805,17.8481819408653,5.43806535103475));
#138870=CARTESIAN_POINT('Ctrl Pts',(20.8557557370745,17.7786059926852,5.44224091522643));
#138871=CARTESIAN_POINT('Ctrl Pts',(20.8064127482817,17.7055159287636,5.44662737723897));
#138872=CARTESIAN_POINT('Ctrl Pts',(20.753345080151,17.6350618855121,5.45101383925151));
#138873=CARTESIAN_POINT('Ctrl Pts',(20.6968850924154,17.5676247799199,5.45540030126405));
#138874=CARTESIAN_POINT('Ctrl Pts',(20.6404251046797,17.5001876743276,5.45978676327659));
#138875=CARTESIAN_POINT('Ctrl Pts',(20.5805732479925,17.4357678796896,5.46417322528913));
#138876=CARTESIAN_POINT('Ctrl Pts',(20.5177042670235,17.3746996193972,5.46855968730167));
#138877=CARTESIAN_POINT('Ctrl Pts',(20.4577251723828,17.3164384720528,5.47274451766051));
#138878=CARTESIAN_POINT('Ctrl Pts',(20.3947769753971,17.2610106350633,5.47692934801934));
#138879=CARTESIAN_POINT('Ctrl Pts',(20.3291582734114,17.2087337632655,5.48111417837818));
#138880=CARTESIAN_POINT('Ctrl Pts',(20.3173695604846,17.1993419737956,5.48186600312105));
#138881=CARTESIAN_POINT('Ctrl Pts',(20.3054947581847,17.1900517964612,5.48261782786391));
#138882=CARTESIAN_POINT('Ctrl Pts',(20.2935357313021,17.1808649545431,5.48336965260678));
#138883=CARTESIAN_POINT('Origin',(18.734,19.211,-1.76670989022852));
#138884=CARTESIAN_POINT('',(20.295886890029,17.177834979693,6.34984102629757));
#138885=CARTESIAN_POINT('',(20.2935357313021,17.1808649545431,6.28334280090994));
#138886=CARTESIAN_POINT('',(20.2935357313021,17.1808649545432,-1.76670989022852));
#138887=CARTESIAN_POINT('',(16.1740005630998,19.2126979607665,5.83329010977151));
#138888=CARTESIAN_POINT('Ctrl Pts',(16.1712326816491,19.2126997966084,5.83329010977151));
#138889=CARTESIAN_POINT('Ctrl Pts',(16.1704460797826,19.3154768238875,5.83841759033362));
#138890=CARTESIAN_POINT('Ctrl Pts',(16.2227680075723,20.2671650151133,5.88593700645621));
#138891=CARTESIAN_POINT('Ctrl Pts',(17.4141948907083,21.935225591005,5.97584835813926));
#138892=CARTESIAN_POINT('Ctrl Pts',(20.3102571304128,21.7953188766137,6.10302416482072));
#138893=CARTESIAN_POINT('Ctrl Pts',(21.7315664652912,19.3340467278774,6.22768838754014));
#138894=CARTESIAN_POINT('Ctrl Pts',(20.9266954619927,17.6674200774838,6.30996067469909));
#138895=CARTESIAN_POINT('Ctrl Pts',(20.295886890029,17.177834979693,6.34984102629757));
#138896=CARTESIAN_POINT('Ctrl Pts',(20.2935357313021,17.1808649545431,5.54983331802439));
#138897=CARTESIAN_POINT('Ctrl Pts',(20.2268224860743,17.1296162999688,5.55400789674241));
#138898=CARTESIAN_POINT('Ctrl Pts',(20.1576175666066,17.0816880438637,5.55818247546043));
#138899=CARTESIAN_POINT('Ctrl Pts',(20.0862915869519,17.0373147735104,5.56235705417845));
#138900=CARTESIAN_POINT('Ctrl Pts',(20.0149229584389,16.9929149704781,5.56653412905591));
#138901=CARTESIAN_POINT('Ctrl Pts',(19.9414311470599,16.9520746080451,5.57071120393336));
#138902=CARTESIAN_POINT('Ctrl Pts',(19.8662111296425,16.9149821520917,5.57488827881081));
#138903=CARTESIAN_POINT('Ctrl Pts',(19.7908651648739,16.8778275890457,5.57907234772436));
#138904=CARTESIAN_POINT('Ctrl Pts',(19.713785638875,16.8444336437072,5.58325641663791));
#138905=CARTESIAN_POINT('Ctrl Pts',(19.6353868855367,16.8149403841761,5.58744048555146));
#138906=CARTESIAN_POINT('Ctrl Pts',(19.5924128561123,16.7987737469663,5.58973396973263));
#138907=CARTESIAN_POINT('Ctrl Pts',(19.549042711016,16.7837782504094,5.5920274539138));
#138908=CARTESIAN_POINT('Ctrl Pts',(19.5053461655915,16.7699704850561,5.59432093809498));
#138909=CARTESIAN_POINT('Ctrl Pts',(19.4256185318271,16.7447771786174,5.59850557248802));
#138910=CARTESIAN_POINT('Ctrl Pts',(19.3445069543662,16.7234471296282,5.60269020688107));
#138911=CARTESIAN_POINT('Ctrl Pts',(19.2624206826507,16.7061304261206,5.60687484127412));
#138912=CARTESIAN_POINT('Ctrl Pts',(19.1804512505827,16.688838370797,5.61105351935806));
#138913=CARTESIAN_POINT('Ctrl Pts',(19.097510326263,16.6755484082766,5.615232197442));
#138914=CARTESIAN_POINT('Ctrl Pts',(19.0140230530434,16.6663611081797,5.61941087552595));
#138915=CARTESIAN_POINT('Ctrl Pts',(18.9290393304527,16.6570091323315,5.62366445341138));
#138916=CARTESIAN_POINT('Ctrl Pts',(18.8434899394339,16.651908491303,5.62791803129682));
#138917=CARTESIAN_POINT('Ctrl Pts',(18.7578350465908,16.6511109612809,5.63217160918225));
#138918=CARTESIAN_POINT('Ctrl Pts',(18.6738407409873,16.6503288929346,5.6363427231602));
#138919=CARTESIAN_POINT('Ctrl Pts',(18.58974546897,16.6536845805936,5.64051383713816));
#138920=CARTESIAN_POINT('Ctrl Pts',(18.5059873315598,16.6611744720411,5.64468495111611));
#138921=CARTESIAN_POINT('Ctrl Pts',(18.4222573000016,16.6686618501832,5.64885466543648));
#138922=CARTESIAN_POINT('Ctrl Pts',(18.3388646361981,16.6802806360296,5.65302437975685));
#138923=CARTESIAN_POINT('Ctrl Pts',(18.2562442180638,16.6959752659613,5.65719409407722));
#138924=CARTESIAN_POINT('Ctrl Pts',(18.1736267399186,16.7116693374106,5.66136366002127));
#138925=CARTESIAN_POINT('Ctrl Pts',(18.0917819045974,16.7314388778862,5.66553322596531));
#138926=CARTESIAN_POINT('Ctrl Pts',(18.0111349162343,16.7551771092621,5.66970279190935));
#138927=CARTESIAN_POINT('Ctrl Pts',(17.9276524792492,16.7797499475688,5.67401895464827));
#138928=CARTESIAN_POINT('Ctrl Pts',(17.8454541950086,16.8085755987089,5.67833511738719));
#138929=CARTESIAN_POINT('Ctrl Pts',(17.7649932472178,16.8414798137466,5.68265128012612));
#138930=CARTESIAN_POINT('Ctrl Pts',(17.6871533063383,16.8733121774403,5.6868268443178));
#138931=CARTESIAN_POINT('Ctrl Pts',(17.6109396593042,16.9089612248341,5.69100240850947));
#138932=CARTESIAN_POINT('Ctrl Pts',(17.5367393343476,16.948221420801,5.69517797270115));
#138933=CARTESIAN_POINT('Ctrl Pts',(17.458791327372,16.989464555934,5.69956443471369));
#138934=CARTESIAN_POINT('Ctrl Pts',(17.3830658746254,17.0346929255447,5.70395089672624));
#138935=CARTESIAN_POINT('Ctrl Pts',(17.3099772536615,17.0836168145088,5.70833735873878));
#138936=CARTESIAN_POINT('Ctrl Pts',(17.2368886326976,17.1325407034729,5.71272382075132));
#138937=CARTESIAN_POINT('Ctrl Pts',(17.1664372628671,17.185159703645,5.71711028276386));
#138938=CARTESIAN_POINT('Ctrl Pts',(17.0989955289255,17.2411369642621,5.72149674477641));
#138939=CARTESIAN_POINT('Ctrl Pts',(17.0355419517776,17.2938040179914,5.72562381401755));
#138940=CARTESIAN_POINT('Ctrl Pts',(16.9745020021859,17.3496514870446,5.72975088325869));
#138941=CARTESIAN_POINT('Ctrl Pts',(16.9162185170908,17.4084267059583,5.73387795249983));
#138942=CARTESIAN_POINT('Ctrl Pts',(16.8577217299028,17.4674170265802,5.73802012571948));
#138943=CARTESIAN_POINT('Ctrl Pts',(16.8020020379166,17.5293563204315,5.74216229893914));
#138944=CARTESIAN_POINT('Ctrl Pts',(16.7493744028763,17.5939467419898,5.74630447215879));
#138945=CARTESIAN_POINT('Ctrl Pts',(16.6970742796338,17.658135205051,5.75042086784546));
#138946=CARTESIAN_POINT('Ctrl Pts',(16.6478281605157,17.7249415391099,5.75453726353214));
#138947=CARTESIAN_POINT('Ctrl Pts',(16.6019085746493,17.7940362905332,5.75865365921882));
#138948=CARTESIAN_POINT('Ctrl Pts',(16.5560170315912,17.8630888462173,5.76276754104799));
#138949=CARTESIAN_POINT('Ctrl Pts',(16.5134482524876,17.9344266527044,5.76688142287718));
#138950=CARTESIAN_POINT('Ctrl Pts',(16.4744330306067,18.0076891046671,5.77099530470636));
#138951=CARTESIAN_POINT('Ctrl Pts',(16.4354291736145,18.0809302157386,5.77510798818765));
#138952=CARTESIAN_POINT('Ctrl Pts',(16.3999770407451,18.1560944409467,5.77922067166894));
#138953=CARTESIAN_POINT('Ctrl Pts',(16.3682620211174,18.2327956168202,5.78333335515023));
#138954=CARTESIAN_POINT('Ctrl Pts',(16.3361584999703,18.3104363640294,5.78749641803534));
#138955=CARTESIAN_POINT('Ctrl Pts',(16.3078844956125,18.3896515290332,5.79165948092045));
#138956=CARTESIAN_POINT('Ctrl Pts',(16.2835818660733,18.4700202641616,5.79582254380555));
#138957=CARTESIAN_POINT('Ctrl Pts',(16.2595524301163,18.5494855487963,5.79993880837771));
#138958=CARTESIAN_POINT('Ctrl Pts',(16.2394055983611,18.6300781193828,5.80405507294986));
#138959=CARTESIAN_POINT('Ctrl Pts',(16.2232275631063,18.7113783730311,5.80817133752201));
#138960=CARTESIAN_POINT('Ctrl Pts',(16.2067736327736,18.7940650953989,5.81235779956359));
#138961=CARTESIAN_POINT('Ctrl Pts',(16.1944252132088,18.877483359597,5.81654426160518));
#138962=CARTESIAN_POINT('Ctrl Pts',(16.186218055036,18.9611857471735,5.82073072364676));
#138963=CARTESIAN_POINT('Ctrl Pts',(16.1780108968631,19.04488813475,5.82491718568835));
#138964=CARTESIAN_POINT('Ctrl Pts',(16.1739449655996,19.1288741338656,5.82910364772993));
#138965=CARTESIAN_POINT('Ctrl Pts',(16.1740005630998,19.2126979607665,5.83329010977151));
#138966=CARTESIAN_POINT('',(16.1740007055014,19.2090994299067,5.76670989019962));
#138967=CARTESIAN_POINT('Ctrl Pts',(20.2935357313021,17.1808649545431,5.48336965260678));
#138968=CARTESIAN_POINT('Ctrl Pts',(20.227081572348,17.1298153282562,5.48754740732368));
#138969=CARTESIAN_POINT('Ctrl Pts',(20.1580238969575,17.081959642987,5.49172516204058));
#138970=CARTESIAN_POINT('Ctrl Pts',(20.0867037125059,17.0375712189784,5.49590291675747));
#138971=CARTESIAN_POINT('Ctrl Pts',(20.0154603367112,16.9932305993224,5.50007617221891));
#138972=CARTESIAN_POINT('Ctrl Pts',(19.9419596834941,16.95235006111,5.50424942768034));
#138973=CARTESIAN_POINT('Ctrl Pts',(19.8665733319354,16.9151607966173,5.50842268314178));
#138974=CARTESIAN_POINT('Ctrl Pts',(19.7912312554809,16.877993373725,5.51259348761154));
#138975=CARTESIAN_POINT('Ctrl Pts',(19.7140060910258,16.8445131234673,5.5167642920813));
#138976=CARTESIAN_POINT('Ctrl Pts',(19.6352947388022,16.8149057210102,5.52093509655106));
#138977=CARTESIAN_POINT('Ctrl Pts',(19.5566060026711,16.7853068256329,5.52510470262571));
#138978=CARTESIAN_POINT('Ctrl Pts',(19.4764323572486,16.7595787296885,5.52927430870036));
#138979=CARTESIAN_POINT('Ctrl Pts',(19.3951901708556,16.737858767081,5.533443914775));
#138980=CARTESIAN_POINT('Ctrl Pts',(19.3139469571518,16.7161385298238,5.53761357357449));
#138981=CARTESIAN_POINT('Ctrl Pts',(19.2316356204149,16.6984266441197,5.54178323237398));
#138982=CARTESIAN_POINT('Ctrl Pts',(19.1486858298494,16.6848100501898,5.54595289117347));
#138983=CARTESIAN_POINT('Ctrl Pts',(19.0656524342559,16.6711797321056,5.55012675256875));
#138984=CARTESIAN_POINT('Ctrl Pts',(18.9819797544012,16.6616530259133,5.55430061396403));
#138985=CARTESIAN_POINT('Ctrl Pts',(18.8981052937467,16.6562652872432,5.55847447535931));
#138986=CARTESIAN_POINT('Ctrl Pts',(18.8141902295685,16.6508749403755,5.56265035731578));
#138987=CARTESIAN_POINT('Ctrl Pts',(18.7300736505504,16.6496275593595,5.56682623927225));
#138988=CARTESIAN_POINT('Ctrl Pts',(18.6461933267713,16.6525063048472,5.57100212122872));
#138989=CARTESIAN_POINT('Ctrl Pts',(18.5621614384985,16.6553902519792,5.57518554864289));
#138990=CARTESIAN_POINT('Ctrl Pts',(18.4783671181011,16.6624151854174,5.57936897605705));
#138991=CARTESIAN_POINT('Ctrl Pts',(18.3952432252439,16.6735122960777,5.58355240347122));
#138992=CARTESIAN_POINT('Ctrl Pts',(18.3145513419211,16.6842847313889,5.58761343364185));
#138993=CARTESIAN_POINT('Ctrl Pts',(18.2344915620021,16.6988941878814,5.59167446381248));
#138994=CARTESIAN_POINT('Ctrl Pts',(18.1554472698611,16.7172324209243,5.59573549398311));
#138995=CARTESIAN_POINT('Ctrl Pts',(18.073997132933,16.7361288086573,5.59992012837615));
#138996=CARTESIAN_POINT('Ctrl Pts',(17.9933221701874,16.7590549809083,5.6041047627692));
#138997=CARTESIAN_POINT('Ctrl Pts',(17.9138510440902,16.7859318174286,5.60828939716224));
#138998=CARTESIAN_POINT('Ctrl Pts',(17.834493035304,16.812770398099,5.6124680752462));
#138999=CARTESIAN_POINT('Ctrl Pts',(17.7563358916495,16.8435483273114,5.61664675333015));
#139000=CARTESIAN_POINT('Ctrl Pts',(17.6797967513069,16.8781357711078,5.6208254314141));
#139001=CARTESIAN_POINT('Ctrl Pts',(17.6018857018817,16.9133431699765,5.62507900929954));
#139002=CARTESIAN_POINT('Ctrl Pts',(17.525651701391,16.9524978888717,5.62933258718497));
#139003=CARTESIAN_POINT('Ctrl Pts',(17.4515171985762,16.9954102672083,5.63358616507041));
#139004=CARTESIAN_POINT('Ctrl Pts',(17.37881993776,17.0374907053542,5.63775727904836));
#139005=CARTESIAN_POINT('Ctrl Pts',(17.3081419118295,17.0831841629373,5.64192839302632));
#139006=CARTESIAN_POINT('Ctrl Pts',(17.2398584137959,17.1322645862507,5.64609950700427));
#139007=CARTESIAN_POINT('Ctrl Pts',(17.1715978289495,17.1813285401541,5.65026922132465));
#139008=CARTESIAN_POINT('Ctrl Pts',(17.1057305494611,17.2337769343488,5.65443893564503));
#139009=CARTESIAN_POINT('Ctrl Pts',(17.0426026198908,17.2893405862225,5.65860864996541));
#139010=CARTESIAN_POINT('Ctrl Pts',(16.9794769366831,17.344902260903,5.66277821590945));
#139011=CARTESIAN_POINT('Ctrl Pts',(16.9190907543423,17.4035786682715,5.66694778185349));
#139012=CARTESIAN_POINT('Ctrl Pts',(16.861755722101,17.4650614661809,5.67111734779753));
#139013=CARTESIAN_POINT('Ctrl Pts',(16.8024048608565,17.5287059234175,5.67543351053645));
#139014=CARTESIAN_POINT('Ctrl Pts',(16.7463240583274,17.5953574026467,5.67974967327537));
#139015=CARTESIAN_POINT('Ctrl Pts',(16.6938147044701,17.6646352435781,5.68406583601428));
#139016=CARTESIAN_POINT('Ctrl Pts',(16.6430158372917,17.731656366128,5.68824140020596));
#139017=CARTESIAN_POINT('Ctrl Pts',(16.5955595388125,17.8011349549808,5.69241696439764));
#139018=CARTESIAN_POINT('Ctrl Pts',(16.5516743299487,17.8726970933921,5.69659252858932));
#139019=CARTESIAN_POINT('Ctrl Pts',(16.5055725835125,17.9478736652917,5.70097899060186));
#139020=CARTESIAN_POINT('Ctrl Pts',(16.463412437974,18.0253492855826,5.7053654526144));
#139021=CARTESIAN_POINT('Ctrl Pts',(16.4254030213233,18.1046637084301,5.70975191462693));
#139022=CARTESIAN_POINT('Ctrl Pts',(16.3873936046726,18.1839781312776,5.71413837663947));
#139023=CARTESIAN_POINT('Ctrl Pts',(16.3535350701226,18.2651307919131,5.718524838652));
#139024=CARTESIAN_POINT('Ctrl Pts',(16.3239764935691,18.3476421955815,5.72291130066454));
#139025=CARTESIAN_POINT('Ctrl Pts',(16.2911969765864,18.4391447059584,5.72777574688621));
#139026=CARTESIAN_POINT('Ctrl Pts',(16.2636032939179,18.5325974942141,5.73264019310788));
#139027=CARTESIAN_POINT('Ctrl Pts',(16.2413973788042,18.6274486545232,5.73750463932955));
#139028=CARTESIAN_POINT('Ctrl Pts',(16.2191773325015,18.7223601753114,5.74237218114123));
#139029=CARTESIAN_POINT('Ctrl Pts',(16.2023520711405,18.818671733483,5.74723972295291));
#139030=CARTESIAN_POINT('Ctrl Pts',(16.191076093449,18.9158085274076,5.75210726476459));
#139031=CARTESIAN_POINT('Ctrl Pts',(16.1798001157575,19.0129453213322,5.75697480657626));
#139032=CARTESIAN_POINT('Ctrl Pts',(16.1740736044194,19.1109072194811,5.76184234838794));
#139033=CARTESIAN_POINT('Ctrl Pts',(16.1740007055014,19.2090994299067,5.76670989019962));
#139034=CARTESIAN_POINT('Ctrl Pts',(16.174000705501,19.2090994304895,5.76670989022851));
#139035=CARTESIAN_POINT('Ctrl Pts',(16.1739381768052,19.293323351932,5.77088500205647));
#139036=CARTESIAN_POINT('Ctrl Pts',(16.1780364138872,19.3775880720651,5.77506011388443));
#139037=CARTESIAN_POINT('Ctrl Pts',(16.1862808495761,19.4614538491682,5.77923522571239));
#139038=CARTESIAN_POINT('Ctrl Pts',(16.1945245019763,19.5453116583386,5.78340994087067));
#139039=CARTESIAN_POINT('Ctrl Pts',(16.2069135252696,19.6287701442273,5.78758465602896));
#139040=CARTESIAN_POINT('Ctrl Pts',(16.223381442754,19.7113943045357,5.79175937118724));
#139041=CARTESIAN_POINT('Ctrl Pts',(16.2398526754153,19.7940350980167,5.79593492676263));
#139042=CARTESIAN_POINT('Ctrl Pts',(16.2604043427346,19.8758407835677,5.80011048233803));
#139043=CARTESIAN_POINT('Ctrl Pts',(16.2849190524509,19.9563874914111,5.80428603791342));
#139044=CARTESIAN_POINT('Ctrl Pts',(16.3094630809744,20.0370305305357,5.80846658731946));
#139045=CARTESIAN_POINT('Ctrl Pts',(16.3379794801115,20.1164111473512,5.8126471367255));
#139046=CARTESIAN_POINT('Ctrl Pts',(16.3703013760236,20.1941219736187,5.81682768613154));
#139047=CARTESIAN_POINT('Ctrl Pts',(16.4026440716426,20.2718828081661,5.82101092579446));
#139048=CARTESIAN_POINT('Ctrl Pts',(16.4387969424261,20.3479712998167,5.82519416545737));
#139049=CARTESIAN_POINT('Ctrl Pts',(16.4785465454201,20.4220035979401,5.82937740512028));
#139050=CARTESIAN_POINT('Ctrl Pts',(16.5183679957904,20.4961697093842,5.83356820598561));
#139051=CARTESIAN_POINT('Ctrl Pts',(16.5617989238518,20.5682718138333,5.83775900685093));
#139052=CARTESIAN_POINT('Ctrl Pts',(16.6085819963923,20.6379542073733,5.84194980771626));
#139053=CARTESIAN_POINT('Ctrl Pts',(16.6388616407129,20.6830550948785,5.84466224092616));
#139054=CARTESIAN_POINT('Ctrl Pts',(16.6705446814796,20.7271429654286,5.84737467413607));
#139055=CARTESIAN_POINT('Ctrl Pts',(16.7035527014987,20.770129169764,5.85008710734598));
#139056=CARTESIAN_POINT('Ctrl Pts',(16.754476165831,20.8364465811684,5.85427174173903));
#139057=CARTESIAN_POINT('Ctrl Pts',(16.8087468503131,20.900389929485,5.85845637613207));
#139058=CARTESIAN_POINT('Ctrl Pts',(16.8661152556941,20.961601777101,5.86264101052512));
#139059=CARTESIAN_POINT('Ctrl Pts',(16.9234020042507,21.0227264972284,5.86681968860905));
#139060=CARTESIAN_POINT('Ctrl Pts',(16.9837774037101,21.0811271065649,5.87099836669299));
#139061=CARTESIAN_POINT('Ctrl Pts',(17.0469505633852,21.136477654614,5.87517704477692));
#139062=CARTESIAN_POINT('Ctrl Pts',(17.111256056546,21.1928203214572,5.87943062266236));
#139063=CARTESIAN_POINT('Ctrl Pts',(17.1784603025297,21.2460021244009,5.88368420054779));
#139064=CARTESIAN_POINT('Ctrl Pts',(17.2482157539318,21.2957170489387,5.88793777843323));
#139065=CARTESIAN_POINT('Ctrl Pts',(17.3166188597919,21.3444681526536,5.89210889241118));
#139066=CARTESIAN_POINT('Ctrl Pts',(17.3874747417492,21.3898853234966,5.89628000638914));
#139067=CARTESIAN_POINT('Ctrl Pts',(17.4604222489451,21.4317205389283,5.90045112036709));
#139068=CARTESIAN_POINT('Ctrl Pts',(17.5333452779005,21.4735417161494,5.90462083468746));
#139069=CARTESIAN_POINT('Ctrl Pts',(17.6083581394472,21.5117830963984,5.90879054900783));
#139070=CARTESIAN_POINT('Ctrl Pts',(17.6850725337908,21.546241137577,5.91296026332821));
#139071=CARTESIAN_POINT('Ctrl Pts',(17.761784198307,21.5806979525906,5.91712982927225));
#139072=CARTESIAN_POINT('Ctrl Pts',(17.8401968552426,21.6113715084925,5.92129939521629));
#139073=CARTESIAN_POINT('Ctrl Pts',(17.919900799999,21.6381057852013,5.92546896116033));
#139074=CARTESIAN_POINT('Ctrl Pts',(18.0024070371278,21.665780006099,5.92978512389925));
#139075=CARTESIAN_POINT('Ctrl Pts',(18.086296554875,21.6892326159301,5.93410128663818));
#139076=CARTESIAN_POINT('Ctrl Pts',(18.1710980677298,21.708346875115,5.9384174493771));
#139077=CARTESIAN_POINT('Ctrl Pts',(18.2531371802228,21.7268384893173,5.94259301356878));
#139078=CARTESIAN_POINT('Ctrl Pts',(18.3360293116296,21.7412700216398,5.94676857776046));
#139079=CARTESIAN_POINT('Ctrl Pts',(18.4193394847877,21.7515882704929,5.95094414195214));
#139080=CARTESIAN_POINT('Ctrl Pts',(18.5068574567409,21.7624276695664,5.95533060396469));
#139081=CARTESIAN_POINT('Ctrl Pts',(18.5948362284715,21.7687272994046,5.95971706597723));
#139082=CARTESIAN_POINT('Ctrl Pts',(18.6827702698546,21.7704873538952,5.96410352798978));
#139083=CARTESIAN_POINT('Ctrl Pts',(18.7707043112377,21.7722474083857,5.96848999000232));
#139084=CARTESIAN_POINT('Ctrl Pts',(18.8585930447506,21.7694679818952,5.97287645201486));
#139085=CARTESIAN_POINT('Ctrl Pts',(18.945938282031,21.7622119011579,5.97726291402741));
#139086=CARTESIAN_POINT('Ctrl Pts',(19.0292646354674,21.7552896834514,5.98144754842045));
#139087=CARTESIAN_POINT('Ctrl Pts',(19.1124065643326,21.7442679479863,5.9856321828135));
#139088=CARTESIAN_POINT('Ctrl Pts',(19.1949284709476,21.7291630099479,5.98981681720655));
#139089=CARTESIAN_POINT('Ctrl Pts',(19.2773329178427,21.7140795719192,5.99399549529049));
#139090=CARTESIAN_POINT('Ctrl Pts',(19.3591186468155,21.6949245577666,5.99817417337443));
#139091=CARTESIAN_POINT('Ctrl Pts',(19.4398541314692,21.6717661297018,6.00235285145837));
#139092=CARTESIAN_POINT('Ctrl Pts',(19.5220367416618,21.6481926034576,6.00660642934381));
#139093=CARTESIAN_POINT('Ctrl Pts',(19.6031306054563,21.6204707691485,6.01086000722925));
#139094=CARTESIAN_POINT('Ctrl Pts',(19.6826902922624,21.5887272192931,6.01511358511469));
#139095=CARTESIAN_POINT('Ctrl Pts',(19.7607075592917,21.557599080094,6.01928469909264));
#139096=CARTESIAN_POINT('Ctrl Pts',(19.8372491575629,21.5226039497269,6.02345581307059));
#139097=CARTESIAN_POINT('Ctrl Pts',(19.9119110552608,21.483911249014,6.02762692704854));
#139098=CARTESIAN_POINT('Ctrl Pts',(19.986547899438,21.4452315320104,6.03179664136892));
#139099=CARTESIAN_POINT('Ctrl Pts',(20.0593058876217,21.4028569203159,6.0359663556893));
#139100=CARTESIAN_POINT('Ctrl Pts',(20.1298036938044,21.3570037391305,6.04013607000967));
#139101=CARTESIAN_POINT('Ctrl Pts',(20.2002989913724,21.3111521895982,6.04430563595371));
#139102=CARTESIAN_POINT('Ctrl Pts',(20.268533881676,21.261822568227,6.04847520189775));
#139103=CARTESIAN_POINT('Ctrl Pts',(20.3341554111888,21.2092749210364,6.05264476784179));
#139104=CARTESIAN_POINT('Ctrl Pts',(20.4020841127265,21.154879763395,6.05696093058072));
#139105=CARTESIAN_POINT('Ctrl Pts',(20.4672118510046,21.0970364076613,6.06127709331964));
#139106=CARTESIAN_POINT('Ctrl Pts',(20.5291853686023,21.036077941447,6.06559325605856));
#139107=CARTESIAN_POINT('Ctrl Pts',(20.5891401053827,20.9771051908579,6.06976882025024));
#139108=CARTESIAN_POINT('Ctrl Pts',(20.6461426787833,20.9152175410395,6.07394438444192));
#139109=CARTESIAN_POINT('Ctrl Pts',(20.6999129097985,20.8507519419374,6.0781199486336));
#139110=CARTESIAN_POINT('Ctrl Pts',(20.7563989473557,20.7830303386772,6.08250641064614));
#139111=CARTESIAN_POINT('Ctrl Pts',(20.8093171796001,20.7124639847438,6.08689287265868));
#139112=CARTESIAN_POINT('Ctrl Pts',(20.8583941356916,20.639478055918,6.09127933467122));
#139113=CARTESIAN_POINT('Ctrl Pts',(20.9074710917831,20.5664921270922,6.09566579668377));
#139114=CARTESIAN_POINT('Ctrl Pts',(20.9527065384673,20.4910871600582,6.10005225869631));
#139115=CARTESIAN_POINT('Ctrl Pts',(20.9938836431733,20.4137160593082,6.10443872070885));
#139116=CARTESIAN_POINT('Ctrl Pts',(21.0331661282527,20.3399049175952,6.1086233551019));
#139117=CARTESIAN_POINT('Ctrl Pts',(21.0689017421373,20.2640298565515,6.11280798949495));
#139118=CARTESIAN_POINT('Ctrl Pts',(21.1008684225542,20.1864659759907,6.116992623888));
#139119=CARTESIAN_POINT('Ctrl Pts',(21.1327896023583,20.1090124980135,6.12117130197194));
#139120=CARTESIAN_POINT('Ctrl Pts',(21.1609523307067,20.0298753969623,6.12534998005588));
#139121=CARTESIAN_POINT('Ctrl Pts',(21.1851803441783,19.9494544131589,6.12952865813983));
#139122=CARTESIAN_POINT('Ctrl Pts',(21.2098426273791,19.8675919410183,6.13378223602526));
#139123=CARTESIAN_POINT('Ctrl Pts',(21.2304275222057,19.7843995318239,6.13803581391069));
#139124=CARTESIAN_POINT('Ctrl Pts',(21.2468003698023,19.7003202443407,6.14228939179613));
#139125=CARTESIAN_POINT('Ctrl Pts',(21.2628557977991,19.6178709979127,6.14646050577408));
#139126=CARTESIAN_POINT('Ctrl Pts',(21.2748609466778,19.5345694264046,6.15063161975203));
#139127=CARTESIAN_POINT('Ctrl Pts',(21.2827395777799,19.4508469609113,6.15480273372998));
#139128=CARTESIAN_POINT('Ctrl Pts',(21.2906155651312,19.3671525892999,6.15897244805035));
#139129=CARTESIAN_POINT('Ctrl Pts',(21.2943677416632,19.2830380618266,6.16314216237073));
#139130=CARTESIAN_POINT('Ctrl Pts',(21.2939715980996,19.1989411060454,6.1673118766911));
#139131=CARTESIAN_POINT('Ctrl Pts',(21.2935754686325,19.1148471427948,6.17148144263515));
#139132=CARTESIAN_POINT('Ctrl Pts',(21.2890313155854,19.0307712100168,6.1756510085792));
#139133=CARTESIAN_POINT('Ctrl Pts',(21.2803667494581,18.9471508437492,6.17982057452325));
#139134=CARTESIAN_POINT('Ctrl Pts',(21.2713975478746,18.8605904885606,6.18413673726217));
#139135=CARTESIAN_POINT('Ctrl Pts',(21.2580128490967,18.7745188559842,6.18845290000109));
#139136=CARTESIAN_POINT('Ctrl Pts',(21.2403015155518,18.6894132736132,6.19276906274001));
#139137=CARTESIAN_POINT('Ctrl Pts',(21.2231671268342,18.6070799966365,6.19694462693169));
#139138=CARTESIAN_POINT('Ctrl Pts',(21.2019838191122,18.5256512422048,6.20112019112337));
#139139=CARTESIAN_POINT('Ctrl Pts',(21.1768832583851,18.4455449811374,6.20529575531505));
#139140=CARTESIAN_POINT('Ctrl Pts',(21.1505149280066,18.3613927432581,6.20968221732759));
#139141=CARTESIAN_POINT('Ctrl Pts',(21.1198234271564,18.2787006554451,6.21406867934013));
#139142=CARTESIAN_POINT('Ctrl Pts',(21.0850182368018,18.1979288029831,6.21845514135267));
#139143=CARTESIAN_POINT('Ctrl Pts',(21.0502130464472,18.117156950521,6.22284160336521));
#139144=CARTESIAN_POINT('Ctrl Pts',(21.0112944915984,18.0383058200372,6.22722806537774));
#139145=CARTESIAN_POINT('Ctrl Pts',(20.9685260259017,17.9618028820206,6.23161452739028));
#139146=CARTESIAN_POINT('Ctrl Pts',(20.9264963505572,17.8866214698433,6.23592521685025));
#139147=CARTESIAN_POINT('Ctrl Pts',(20.880587598457,17.8134194333577,6.24023590631023));
#139148=CARTESIAN_POINT('Ctrl Pts',(20.8310139328075,17.7426224717018,6.2445465957702));
#139149=CARTESIAN_POINT('Ctrl Pts',(20.7829662991437,17.6740048612509,6.24872458876905));
#139150=CARTESIAN_POINT('Ctrl Pts',(20.7314763614704,17.6076468441108,6.25290258176791));
#139151=CARTESIAN_POINT('Ctrl Pts',(20.6767860578329,17.5439120198711,6.25708057476676));
#139152=CARTESIAN_POINT('Ctrl Pts',(20.6194902413024,17.4771407907252,6.26145761245729));
#139153=CARTESIAN_POINT('Ctrl Pts',(20.5586817691827,17.4132493747021,6.26583465014782));
#139154=CARTESIAN_POINT('Ctrl Pts',(20.4946892530986,17.3526207722795,6.27021168783835));
#139155=CARTESIAN_POINT('Ctrl Pts',(20.4306967370146,17.2919921698569,6.27458872552888));
#139156=CARTESIAN_POINT('Ctrl Pts',(20.3635205634202,17.2346268195884,6.27896576321941));
#139157=CARTESIAN_POINT('Ctrl Pts',(20.2935357313021,17.1808649545431,6.28334280090994));
#139158=CARTESIAN_POINT('Origin',(18.734,19.211,-1.76670989022852));
#139159=CARTESIAN_POINT('',(20.2935357313021,17.1808649545432,7.14996298022642));
#139160=CARTESIAN_POINT('',(20.2935357313021,17.1808649545432,7.08324142743447));
#139161=CARTESIAN_POINT('',(20.2935357313021,17.1808649545432,-1.76670989022852));
#139162=CARTESIAN_POINT('',(16.1740008768645,19.208881145288,6.6332901097715));
#139163=CARTESIAN_POINT('Ctrl Pts',(16.1740008768645,19.208881145288,6.6332901097715));
#139164=CARTESIAN_POINT('Ctrl Pts',(16.1739325519701,19.291431245901,6.63740642252224));
#139165=CARTESIAN_POINT('Ctrl Pts',(16.1778613169669,19.3741241408158,6.64152273527298));
#139166=CARTESIAN_POINT('Ctrl Pts',(16.1858020059738,19.456534077555,6.64563904802372));
#139167=CARTESIAN_POINT('Ctrl Pts',(16.1937337220434,19.5388508914938,6.64975070936243));
#139168=CARTESIAN_POINT('Ctrl Pts',(16.2056683130375,19.6208849121504,6.65386237070114));
#139169=CARTESIAN_POINT('Ctrl Pts',(16.2215685692311,19.7022110602219,6.65797403203985));
#139170=CARTESIAN_POINT('Ctrl Pts',(16.2374592000151,19.7834879765409,6.66208320433539));
#139171=CARTESIAN_POINT('Ctrl Pts',(16.2573106430752,19.8640574053625,6.66619237663093));
#139172=CARTESIAN_POINT('Ctrl Pts',(16.2810340922892,19.9435013690146,6.67030154892647));
#139173=CARTESIAN_POINT('Ctrl Pts',(16.3047507902537,20.0229227244023,6.67440955182852));
#139174=CARTESIAN_POINT('Ctrl Pts',(16.3323371713261,20.1012187954775,6.67851755473057));
#139175=CARTESIAN_POINT('Ctrl Pts',(16.3636541468012,20.1779852823199,6.68262555763262));
#139176=CARTESIAN_POINT('Ctrl Pts',(16.3949722554066,20.2547545467753,6.68673370917299));
#139177=CARTESIAN_POINT('Ctrl Pts',(16.4300210447236,20.3299936782016,6.69084186071336));
#139178=CARTESIAN_POINT('Ctrl Pts',(16.4686133150906,20.4033184003592,6.69495001225373));
#139179=CARTESIAN_POINT('Ctrl Pts',(16.5072438266208,20.4767157801408,6.69906223457025));
#139180=CARTESIAN_POINT('Ctrl Pts',(16.5494246053548,20.5481945435127,6.70317445688677));
#139181=CARTESIAN_POINT('Ctrl Pts',(16.5949228757402,20.6173957680782,6.70728667920329));
#139182=CARTESIAN_POINT('Ctrl Pts',(16.6404458510681,20.6866345679682,6.71140113440064));
#139183=CARTESIAN_POINT('Ctrl Pts',(16.6892896206456,20.7535929860938,6.715515589598));
#139184=CARTESIAN_POINT('Ctrl Pts',(16.7411800554792,20.8179438909682,6.71963004479535));
#139185=CARTESIAN_POINT('Ctrl Pts',(16.7931561866085,20.8824010704228,6.7237512949554));
#139186=CARTESIAN_POINT('Ctrl Pts',(16.8481887081045,20.9442417891331,6.72787254511546));
#139187=CARTESIAN_POINT('Ctrl Pts',(16.9059658904508,21.0031750177716,6.73199379527552));
#139188=CARTESIAN_POINT('Ctrl Pts',(16.9382542996129,21.0361094760171,6.73429692959297));
#139189=CARTESIAN_POINT('Ctrl Pts',(16.9713992632832,21.068136611825,6.73660006391043));
#139190=CARTESIAN_POINT('Ctrl Pts',(17.0053421035809,21.0992112903877,6.73890319822789));
#139191=CARTESIAN_POINT('Ctrl Pts',(17.067013876621,21.1556718136325,6.74308783262094));
#139192=CARTESIAN_POINT('Ctrl Pts',(17.1315694533286,21.2092127933028,6.74727246701399));
#139193=CARTESIAN_POINT('Ctrl Pts',(17.1987010234279,21.2595255801519,6.75145710140704));
#139194=CARTESIAN_POINT('Ctrl Pts',(17.2657370400465,21.3097667529765,6.75563577949099));
#139195=CARTESIAN_POINT('Ctrl Pts',(17.3353414020479,21.3567885864286,6.75981445757493));
#139196=CARTESIAN_POINT('Ctrl Pts',(17.4071710083241,21.4003206313485,6.76399313565888));
#139197=CARTESIAN_POINT('Ctrl Pts',(17.4802881086698,21.4446329568877,6.76824671354431));
#139198=CARTESIAN_POINT('Ctrl Pts',(17.5557106573434,21.4853288288425,6.77250029142975));
#139199=CARTESIAN_POINT('Ctrl Pts',(17.6330432222703,21.5221672751169,6.77675386931518));
#139200=CARTESIAN_POINT('Ctrl Pts',(17.7088765445241,21.5582915362259,6.78092498329313));
#139201=CARTESIAN_POINT('Ctrl Pts',(17.7865460506904,21.5907063974352,6.78509609727109));
#139202=CARTESIAN_POINT('Ctrl Pts',(17.8656529884827,21.6192303601585,6.78926721124904));
#139203=CARTESIAN_POINT('Ctrl Pts',(17.944733381178,21.6477447513906,6.79343692556941));
#139204=CARTESIAN_POINT('Ctrl Pts',(18.0252498151567,21.6723706812234,6.79760663988978));
#139205=CARTESIAN_POINT('Ctrl Pts',(18.1067845307987,21.6929751721551,6.80177635421015));
#139206=CARTESIAN_POINT('Ctrl Pts',(18.1883163450856,21.7135789298907,6.80594592015419));
#139207=CARTESIAN_POINT('Ctrl Pts',(18.2708659227709,21.7301614213603,6.81011548609824));
#139208=CARTESIAN_POINT('Ctrl Pts',(18.3540026821448,21.7426401873929,6.81428505204228));
#139209=CARTESIAN_POINT('Ctrl Pts',(18.440062427418,21.755557691445,6.8186012147812));
#139210=CARTESIAN_POINT('Ctrl Pts',(18.5267508916659,21.7640774486062,6.82291737752012));
#139211=CARTESIAN_POINT('Ctrl Pts',(18.6135836740996,21.7681663826307,6.82723354025904));
#139212=CARTESIAN_POINT('Ctrl Pts',(18.6975878877788,21.7721221200595,6.83140910445072));
#139213=CARTESIAN_POINT('Ctrl Pts',(18.7817266907701,21.7719313177434,6.83558466864241));
#139214=CARTESIAN_POINT('Ctrl Pts',(18.8655624783157,21.7676171622477,6.83976023283409));
#139215=CARTESIAN_POINT('Ctrl Pts',(18.9536326121894,21.7630851090138,6.84414669484663));
#139216=CARTESIAN_POINT('Ctrl Pts',(19.0413677347566,21.7540022746856,6.84853315685917));
#139217=CARTESIAN_POINT('Ctrl Pts',(19.1282700391328,21.7404566879554,6.8529196188717));
#139218=CARTESIAN_POINT('Ctrl Pts',(19.215172343509,21.7269111012251,6.85730608088424));
#139219=CARTESIAN_POINT('Ctrl Pts',(19.3012412773527,21.7089029553709,6.86169254289678));
#139220=CARTESIAN_POINT('Ctrl Pts',(19.3859971465595,21.6865806835727,6.86607900490932));
#139221=CARTESIAN_POINT('Ctrl Pts',(19.4668532725857,21.6652854925895,6.87026363930237));
#139222=CARTESIAN_POINT('Ctrl Pts',(19.5468154727231,21.6399851855305,6.87444827369542));
#139223=CARTESIAN_POINT('Ctrl Pts',(19.6254576099359,21.6107715161422,6.87863290808846));
#139224=CARTESIAN_POINT('Ctrl Pts',(19.7039878098005,21.5815994287963,6.88281158617242));
#139225=CARTESIAN_POINT('Ctrl Pts',(19.7812012513675,21.5485252020902,6.88699026425637));
#139226=CARTESIAN_POINT('Ctrl Pts',(19.8566848155709,21.5116909407581,6.89116894234032));
#139227=CARTESIAN_POINT('Ctrl Pts',(19.9335213684134,21.474196451764,6.89542252022575));
#139228=CARTESIAN_POINT('Ctrl Pts',(20.0085649515612,21.4328059278375,6.89967609811119));
#139229=CARTESIAN_POINT('Ctrl Pts',(20.0813989057343,21.3877214311496,6.90392967599662));
#139230=CARTESIAN_POINT('Ctrl Pts',(20.1528208315821,21.3435109854051,6.90810078997458));
#139231=CARTESIAN_POINT('Ctrl Pts',(20.2221176306652,21.2957487717612,6.91227190395253));
#139232=CARTESIAN_POINT('Ctrl Pts',(20.2889208543458,21.2446718360445,6.91644301793048));
#139233=CARTESIAN_POINT('Ctrl Pts',(20.3557016615595,21.1936120396869,6.92061273225086));
#139234=CARTESIAN_POINT('Ctrl Pts',(20.4199901900087,21.1392400094635,6.92478244657123));
#139235=CARTESIAN_POINT('Ctrl Pts',(20.4814485012998,21.0818350369033,6.92895216089161));
#139236=CARTESIAN_POINT('Ctrl Pts',(20.5429046256403,21.0244321070585,6.93312172683565));
#139237=CARTESIAN_POINT('Ctrl Pts',(20.6015303974546,20.9639967640997,6.93729129277969));
#139238=CARTESIAN_POINT('Ctrl Pts',(20.6570234159162,20.9008464255186,6.94146085872373));
#139239=CARTESIAN_POINT('Ctrl Pts',(20.7144675004488,20.8354757989374,6.94577702146265));
#139240=CARTESIAN_POINT('Ctrl Pts',(20.7685540894612,20.7671961022132,6.95009318420157));
#139241=CARTESIAN_POINT('Ctrl Pts',(20.8189931741053,20.6963967362069,6.95440934694048));
#139242=CARTESIAN_POINT('Ctrl Pts',(20.8677892108724,20.6279036521016,6.95858491113216));
#139243=CARTESIAN_POINT('Ctrl Pts',(20.9131715145603,20.5570529563654,6.96276047532384));
#139244=CARTESIAN_POINT('Ctrl Pts',(20.9549227142452,20.4842251557952,6.96693603951552));
#139245=CARTESIAN_POINT('Ctrl Pts',(20.9987826677721,20.40771899615,6.97132250152806));
#139246=CARTESIAN_POINT('Ctrl Pts',(21.0386347993092,20.3290312765029,6.97570896354059));
#139247=CARTESIAN_POINT('Ctrl Pts',(21.0742836736309,20.2486282219257,6.98009542555313));
#139248=CARTESIAN_POINT('Ctrl Pts',(21.1099325479526,20.1682251673484,6.98448188756567));
#139249=CARTESIAN_POINT('Ctrl Pts',(21.1413780286032,20.0861073468905,6.98886834957821));
#139250=CARTESIAN_POINT('Ctrl Pts',(21.1684852750765,20.0027584514458,6.99325481159075));
#139251=CARTESIAN_POINT('Ctrl Pts',(21.1943452769569,19.9232445622332,6.99743944598379));
#139252=CARTESIAN_POINT('Ctrl Pts',(21.2163537449119,19.8423144298574,7.00162408037684));
#139253=CARTESIAN_POINT('Ctrl Pts',(21.234357169427,19.7603760326908,7.00580871476988));
#139254=CARTESIAN_POINT('Ctrl Pts',(21.2523349682956,19.6785542646905,7.00998739285382));
#139255=CARTESIAN_POINT('Ctrl Pts',(21.2663189491972,19.5957275280112,7.01416607093776));
#139256=CARTESIAN_POINT('Ctrl Pts',(21.2762049862094,19.5123201090074,7.0183447490217));
#139257=CARTESIAN_POINT('Ctrl Pts',(21.2862682233301,19.4274176719616,7.02259832690714));
#139258=CARTESIAN_POINT('Ctrl Pts',(21.2920850111441,19.3419139888707,7.02685190479258));
#139259=CARTESIAN_POINT('Ctrl Pts',(21.2935997221946,19.2562687766721,7.03110548267801));
#139260=CARTESIAN_POINT('Ctrl Pts',(21.2950850676157,19.1722839640349,7.03527659665597));
#139261=CARTESIAN_POINT('Ctrl Pts',(21.2924336475013,19.0881635420989,7.03944771063392));
#139262=CARTESIAN_POINT('Ctrl Pts',(21.2856453456188,19.0043456262701,7.04361882461187));
#139263=CARTESIAN_POINT('Ctrl Pts',(21.2788593216167,18.9205558363527,7.04778853893224));
#139264=CARTESIAN_POINT('Ctrl Pts',(21.2679392098804,18.8370688090943,7.05195825325261));
#139265=CARTESIAN_POINT('Ctrl Pts',(21.252936930744,18.7543198724119,7.05612796757298));
#139266=CARTESIAN_POINT('Ctrl Pts',(21.2379351854531,18.6715738802916,7.06029753351702));
#139267=CARTESIAN_POINT('Ctrl Pts',(21.2188516444825,18.5895663790286,7.06446709946107));
#139268=CARTESIAN_POINT('Ctrl Pts',(21.1957895218785,18.5087234519298,7.06863666540511));
#139269=CARTESIAN_POINT('Ctrl Pts',(21.1719165634939,18.4250381872448,7.07295282814404));
#139270=CARTESIAN_POINT('Ctrl Pts',(21.1437801888442,18.3426014204637,7.07726899088296));
#139271=CARTESIAN_POINT('Ctrl Pts',(21.1115508461405,18.261867778433,7.08158515362188));
#139272=CARTESIAN_POINT('Ctrl Pts',(21.0803713708855,18.1837640263,7.08576071781356));
#139273=CARTESIAN_POINT('Ctrl Pts',(21.0453617283798,18.1072545529914,7.08993628200523));
#139274=CARTESIAN_POINT('Ctrl Pts',(21.006724205865,18.032728094167,7.09411184619691));
#139275=CARTESIAN_POINT('Ctrl Pts',(20.9661351939398,17.9544374810769,7.09849830820946));
#139276=CARTESIAN_POINT('Ctrl Pts',(20.9215424772638,17.8783359749763,7.102884770222));
#139277=CARTESIAN_POINT('Ctrl Pts',(20.8732322919594,17.8048402647501,7.10727123223455));
#139278=CARTESIAN_POINT('Ctrl Pts',(20.8249221066551,17.731344554524,7.11165769424709));
#139279=CARTESIAN_POINT('Ctrl Pts',(20.7728948573422,17.6604550629257,7.11604415625964));
#139280=CARTESIAN_POINT('Ctrl Pts',(20.7174842649081,17.5925469821889,7.12043061827219));
#139281=CARTESIAN_POINT('Ctrl Pts',(20.6646206180318,17.5277602935357,7.12461545674226));
#139282=CARTESIAN_POINT('Ctrl Pts',(20.6084810526672,17.4654457911788,7.12880029521234));
#139283=CARTESIAN_POINT('Ctrl Pts',(20.5493255613627,17.4059534337688,7.13298513368241));
#139284=CARTESIAN_POINT('Ctrl Pts',(20.4902614757737,17.346553002592,7.13716350583555));
#139285=CARTESIAN_POINT('Ctrl Pts',(20.428191047079,17.2899663736458,7.1413418779887));
#139286=CARTESIAN_POINT('Ctrl Pts',(20.3634146060967,17.2365106884466,7.14552025014184));
#139287=CARTESIAN_POINT('Ctrl Pts',(20.340456363622,17.2175647790412,7.14700116017003));
#139288=CARTESIAN_POINT('Ctrl Pts',(20.3171585650168,17.199011852374,7.14848207019823));
#139289=CARTESIAN_POINT('Ctrl Pts',(20.2935357313021,17.1808649545431,7.14996298022642));
#139290=CARTESIAN_POINT('Ctrl Pts',(20.295886890029,17.177834979693,6.34984102629757));
#139291=CARTESIAN_POINT('Ctrl Pts',(20.2561598407695,17.1470018994828,6.35235261025957));
#139292=CARTESIAN_POINT('Ctrl Pts',(19.528831972149,16.618320657574,6.39725612978206));
#139293=CARTESIAN_POINT('Ctrl Pts',(17.5479307751794,16.4259451726882,6.48455158486501));
#139294=CARTESIAN_POINT('Ctrl Pts',(16.2478508564243,18.0710820233979,6.57652302872766));
#139295=CARTESIAN_POINT('Ctrl Pts',(16.1710772436132,19.0646440698247,6.62610253702982));
#139296=CARTESIAN_POINT('Ctrl Pts',(16.172362658312,19.2088797893707,6.6332901097715));
#139297=CARTESIAN_POINT('',(16.174000571626,19.2127107672549,6.56670989025839));
#139298=CARTESIAN_POINT('Ctrl Pts',(20.2935357313021,17.1808649545431,6.28334280090994));
#139299=CARTESIAN_POINT('Ctrl Pts',(20.2268670407022,17.1296505265265,6.28751243828281));
#139300=CARTESIAN_POINT('Ctrl Pts',(20.1576502146725,17.081706158595,6.29168207565569));
#139301=CARTESIAN_POINT('Ctrl Pts',(20.0862433688758,17.0372847768552,6.29585171302856));
#139302=CARTESIAN_POINT('Ctrl Pts',(20.0148367281774,16.9928635227047,6.30002133842519));
#139303=CARTESIAN_POINT('Ctrl Pts',(19.9412404714991,16.9519654765769,6.30419096382183));
#139304=CARTESIAN_POINT('Ctrl Pts',(19.8658401643204,16.9147992591171,6.30836058921847));
#139305=CARTESIAN_POINT('Ctrl Pts',(19.7898457625222,16.8773402013408,6.31256306795624));
#139306=CARTESIAN_POINT('Ctrl Pts',(19.7120191739364,16.8436722636366,6.31676554669401));
#139307=CARTESIAN_POINT('Ctrl Pts',(19.632777078394,16.8139602082248,6.32096802543178));
#139308=CARTESIAN_POINT('Ctrl Pts',(19.5540386541307,16.7844370058318,6.32514379276286));
#139309=CARTESIAN_POINT('Ctrl Pts',(19.473903125821,16.7588196266226,6.32931956009393));
#139310=CARTESIAN_POINT('Ctrl Pts',(19.3927942358925,16.7372194610769,6.33349532742501));
#139311=CARTESIAN_POINT('Ctrl Pts',(19.3109070940739,16.7154120387227,6.33771116186612));
#139312=CARTESIAN_POINT('Ctrl Pts',(19.2280282808171,16.6976994334045,6.34192699630724));
#139313=CARTESIAN_POINT('Ctrl Pts',(19.1446022295193,16.6841430968269,6.34614283074836));
#139314=CARTESIAN_POINT('Ctrl Pts',(19.0611761782215,16.6705867602493,6.35035866518948));
#139315=CARTESIAN_POINT('Ctrl Pts',(18.9772033685603,16.6611866814948,6.3545744996306));
#139316=CARTESIAN_POINT('Ctrl Pts',(18.8931294701917,16.6559505265619,6.35879033407172));
#139317=CARTESIAN_POINT('Ctrl Pts',(18.8096777759695,16.650753122744,6.36297496846477));
#139318=CARTESIAN_POINT('Ctrl Pts',(18.7258158815285,16.6496388297568,6.36715960285782));
#139319=CARTESIAN_POINT('Ctrl Pts',(18.6419771668654,16.6526544802975,6.37134423725087));
#139320=CARTESIAN_POINT('Ctrl Pts',(18.5582577862359,16.6556658384328,6.3755229153348));
#139321=CARTESIAN_POINT('Ctrl Pts',(18.4745619756522,16.6627954472227,6.37970159341873));
#139322=CARTESIAN_POINT('Ctrl Pts',(18.391326582379,16.6740382484444,6.38388027150266));
#139323=CARTESIAN_POINT('Ctrl Pts',(18.3065992545013,16.6854825687981,6.3881338493881));
#139324=CARTESIAN_POINT('Ctrl Pts',(18.2223494934534,16.7011890198916,6.39238742727354));
#139325=CARTESIAN_POINT('Ctrl Pts',(18.1390363521675,16.7210967372691,6.39664100515897));
#139326=CARTESIAN_POINT('Ctrl Pts',(18.0573383986977,16.7406185046986,6.40081211913692));
#139327=CARTESIAN_POINT('Ctrl Pts',(17.97654154071,16.7641799807697,6.40498323311487));
#139328=CARTESIAN_POINT('Ctrl Pts',(17.8970700591986,16.7916719374607,6.40915434709282));
#139329=CARTESIAN_POINT('Ctrl Pts',(17.8176252451105,16.8191546689601,6.41332406141319));
#139330=CARTESIAN_POINT('Ctrl Pts',(17.7395053586246,16.8505651114303,6.41749377573356));
#139331=CARTESIAN_POINT('Ctrl Pts',(17.6631189946712,16.8857443425666,6.42166349005393));
#139332=CARTESIAN_POINT('Ctrl Pts',(17.5867353488724,16.9209223218749,6.42583305599797));
#139333=CARTESIAN_POINT('Ctrl Pts',(17.5120855204511,16.959868629993,6.43000262194201));
#139334=CARTESIAN_POINT('Ctrl Pts',(17.4395563508728,17.0023769811862,6.43417218788605));
#139335=CARTESIAN_POINT('Ctrl Pts',(17.3644771451664,17.0463798735677,6.43848835062497));
#139336=CARTESIAN_POINT('Ctrl Pts',(17.2916709526714,17.0941996856768,6.4428045133639));
#139337=CARTESIAN_POINT('Ctrl Pts',(17.221535475533,17.1455579015066,6.44712067610282));
#139338=CARTESIAN_POINT('Ctrl Pts',(17.1536846541856,17.1952431288576,6.4512962402945));
#139339=CARTESIAN_POINT('Ctrl Pts',(17.0883335592487,17.2482394397186,6.45547180448618));
#139340=CARTESIAN_POINT('Ctrl Pts',(17.0258081406205,17.3042539310255,6.45964736867786));
#139341=CARTESIAN_POINT('Ctrl Pts',(16.9601247117373,17.3630975811267,6.46403383069041));
#139342=CARTESIAN_POINT('Ctrl Pts',(16.8975603248985,17.4252719095173,6.46842029270295));
#139343=CARTESIAN_POINT('Ctrl Pts',(16.8384470475511,17.4903957443787,6.4728067547155));
#139344=CARTESIAN_POINT('Ctrl Pts',(16.7793337702037,17.55551957924,6.47719321672805));
#139345=CARTESIAN_POINT('Ctrl Pts',(16.7236719107427,17.6235924232491,6.4815796787406));
#139346=CARTESIAN_POINT('Ctrl Pts',(16.6717415022697,17.6941974787273,6.48596614075315));
#139347=CARTESIAN_POINT('Ctrl Pts',(16.6219091295866,17.7619500256717,6.4901753857061));
#139348=CARTESIAN_POINT('Ctrl Pts',(16.5753265021954,17.8322867639503,6.49438463065906));
#139349=CARTESIAN_POINT('Ctrl Pts',(16.5322706261132,17.9048653345982,6.49859387561201));
#139350=CARTESIAN_POINT('Ctrl Pts',(16.4892771418592,17.9773387323843,6.50279702099131));
#139351=CARTESIAN_POINT('Ctrl Pts',(16.4498004872777,18.0520471246589,6.5070001663706));
#139352=CARTESIAN_POINT('Ctrl Pts',(16.4140760664827,18.128617007389,6.5112033117499));
#139353=CARTESIAN_POINT('Ctrl Pts',(16.3783931208862,18.2050979943158,6.51540157737789));
#139354=CARTESIAN_POINT('Ctrl Pts',(16.3464539443372,18.2834357700826,6.51959984300588));
#139355=CARTESIAN_POINT('Ctrl Pts',(16.3184487740251,18.3632310015746,6.52379810863387));
#139356=CARTESIAN_POINT('Ctrl Pts',(16.2904693914728,18.4429527559108,6.52799250840908));
#139357=CARTESIAN_POINT('Ctrl Pts',(16.2664169618498,18.5241288717768,6.53218690818429));
#139358=CARTESIAN_POINT('Ctrl Pts',(16.2464336691667,18.6063399717985,6.5363813079595));
#139359=CARTESIAN_POINT('Ctrl Pts',(16.2264610773219,18.6885070486605,6.54057346167876));
#139360=CARTESIAN_POINT('Ctrl Pts',(16.210553397436,18.7717075687093,6.54476561539801));
#139361=CARTESIAN_POINT('Ctrl Pts',(16.1988026788696,18.8555080269072,6.54895776911726));
#139362=CARTESIAN_POINT('Ctrl Pts',(16.1870533030452,18.9392989093172,6.55314944380363));
#139363=CARTESIAN_POINT('Ctrl Pts',(16.1794600117858,19.0236891460433,6.55734111849001));
#139364=CARTESIAN_POINT('Ctrl Pts',(16.1760633700115,19.1082371810286,6.56153279317638));
#139365=CARTESIAN_POINT('Ctrl Pts',(16.1746649834927,19.1430453357189,6.56325849219375));
#139366=CARTESIAN_POINT('Ctrl Pts',(16.173977295445,19.1778801783156,6.56498419121113));
#139367=CARTESIAN_POINT('Ctrl Pts',(16.1740005716256,19.2127107666517,6.5667098902285));
#139368=CARTESIAN_POINT('Ctrl Pts',(16.174000571626,19.2127107672549,6.56670989025838));
#139369=CARTESIAN_POINT('Ctrl Pts',(16.1740643617891,19.3081666398866,6.57143929947811));
#139370=CARTESIAN_POINT('Ctrl Pts',(16.1794711562484,19.4034153336876,6.57616870869783));
#139371=CARTESIAN_POINT('Ctrl Pts',(16.1901275024527,19.4979019278825,6.58089811791755));
#139372=CARTESIAN_POINT('Ctrl Pts',(16.200836414009,19.5928546031322,6.58565085624608));
#139373=CARTESIAN_POINT('Ctrl Pts',(16.2168466650982,19.6870374428256,6.59040359457461));
#139374=CARTESIAN_POINT('Ctrl Pts',(16.2380139506883,19.7799056526714,6.59515633290315));
#139375=CARTESIAN_POINT('Ctrl Pts',(16.2593038089226,19.8733116311407,6.59993659274364));
#139376=CARTESIAN_POINT('Ctrl Pts',(16.2858104835354,19.9653875176628,6.60471685258415));
#139377=CARTESIAN_POINT('Ctrl Pts',(16.3173390825683,20.0556005032904,6.60949711242465));
#139378=CARTESIAN_POINT('Ctrl Pts',(16.3253523527952,20.0785289255476,6.61071205742796));
#139379=CARTESIAN_POINT('Ctrl Pts',(16.3336897868424,20.101337126465,6.61192700243127));
#139380=CARTESIAN_POINT('Ctrl Pts',(16.3423477078173,20.1240166007785,6.61314194743458));
#139381=CARTESIAN_POINT('Ctrl Pts',(16.3721681801721,20.2021315014283,6.61732658182763));
#139382=CARTESIAN_POINT('Ctrl Pts',(16.405875193857,20.2789292632221,6.62151121622068));
#139383=CARTESIAN_POINT('Ctrl Pts',(16.4433319467771,20.3539960060928,6.62569585061373));
#139384=CARTESIAN_POINT('Ctrl Pts',(16.4807353846457,20.4289559007464,6.62987452869767));
#139385=CARTESIAN_POINT('Ctrl Pts',(16.5218777565726,20.5021892624269,6.63405320678161));
#139386=CARTESIAN_POINT('Ctrl Pts',(16.5665735905077,20.5733005393213,6.63823188486556));
#139387=CARTESIAN_POINT('Ctrl Pts',(16.6120705651436,20.6456864347473,6.64248546275099));
#139388=CARTESIAN_POINT('Ctrl Pts',(16.6612494744651,20.715872969927,6.64673904063643));
#139389=CARTESIAN_POINT('Ctrl Pts',(16.7138648542455,20.7834674854786,6.65099261852186));
#139390=CARTESIAN_POINT('Ctrl Pts',(16.7654601822184,20.8497515494465,6.65516373249982));
#139391=CARTESIAN_POINT('Ctrl Pts',(16.8203596287513,20.9135428198972,6.65933484647777));
#139392=CARTESIAN_POINT('Ctrl Pts',(16.8782881026494,20.9745003130227,6.66350596045572));
#139393=CARTESIAN_POINT('Ctrl Pts',(16.9361971380886,21.0354373512728,6.66767567477609));
#139394=CARTESIAN_POINT('Ctrl Pts',(16.9971328656301,21.0935421675084,6.67184538909647));
#139395=CARTESIAN_POINT('Ctrl Pts',(17.0607814536891,21.1485086312792,6.67601510341684));
#139396=CARTESIAN_POINT('Ctrl Pts',(17.1244277768583,21.2034731391074,6.68018466936089));
#139397=CARTESIAN_POINT('Ctrl Pts',(17.1907864198802,21.2552992164785,6.68435423530494));
#139398=CARTESIAN_POINT('Ctrl Pts',(17.2595094445545,21.3037201441908,6.68852380124899));
#139399=CARTESIAN_POINT('Ctrl Pts',(17.3306486859972,21.3538434919877,6.69283996398791));
#139400=CARTESIAN_POINT('Ctrl Pts',(17.4043212347442,21.4003174810233,6.69715612672683));
#139401=CARTESIAN_POINT('Ctrl Pts',(17.4801089073795,21.4428954114938,6.70147228946575));
#139402=CARTESIAN_POINT('Ctrl Pts',(17.5534278045502,21.4840863703576,6.70564785365743));
#139403=CARTESIAN_POINT('Ctrl Pts',(17.6287256988458,21.5216310329473,6.70982341784911));
#139404=CARTESIAN_POINT('Ctrl Pts',(17.7056010183996,21.555353969571,6.71399898204079));
#139405=CARTESIAN_POINT('Ctrl Pts',(17.7863591275902,21.5907801715548,6.71838544405333));
#139406=CARTESIAN_POINT('Ctrl Pts',(17.8688576552588,21.6219882241026,6.72277190606587));
#139407=CARTESIAN_POINT('Ctrl Pts',(17.9526121488768,21.6488336748263,6.72715836807841));
#139408=CARTESIAN_POINT('Ctrl Pts',(18.0363666424948,21.67567912555,6.73154483009094));
#139409=CARTESIAN_POINT('Ctrl Pts',(18.1213765216826,21.6981618996353,6.73593129210348));
#139410=CARTESIAN_POINT('Ctrl Pts',(18.20714644876,21.7161996598167,6.74031775411602));
#139411=CARTESIAN_POINT('Ctrl Pts',(18.288969974351,21.7334074759138,6.74450238850907));
#139412=CARTESIAN_POINT('Ctrl Pts',(18.3717897057139,21.7466343835296,6.74868702290212));
#139413=CARTESIAN_POINT('Ctrl Pts',(18.4551835868306,21.755771386146,6.75287165729516));
#139414=CARTESIAN_POINT('Ctrl Pts',(18.5384587670797,21.76489538337,6.75705033537911));
#139415=CARTESIAN_POINT('Ctrl Pts',(18.6223060204196,21.7699409891981,6.76122901346305));
#139416=CARTESIAN_POINT('Ctrl Pts',(18.7062923578697,21.7708500515787,6.765407691547));
#139417=CARTESIAN_POINT('Ctrl Pts',(18.7917840900588,21.7717754082492,6.76966126943243));
#139418=CARTESIAN_POINT('Ctrl Pts',(18.8774194697488,21.7684143685408,6.77391484731787));
#139419=CARTESIAN_POINT('Ctrl Pts',(18.9627354674093,21.7607607899466,6.77816842520331));
#139420=CARTESIAN_POINT('Ctrl Pts',(19.0463974479747,21.7532555909081,6.78233953918126));
#139421=CARTESIAN_POINT('Ctrl Pts',(19.1297518403942,21.7416228491976,6.78651065315921));
#139422=CARTESIAN_POINT('Ctrl Pts',(19.212363029601,21.7259093049076,6.79068176713716));
#139423=CARTESIAN_POINT('Ctrl Pts',(19.2949464978254,21.7102010334492,6.79485148145753));
#139424=CARTESIAN_POINT('Ctrl Pts',(19.3767868065737,21.6904147648581,6.79902119577791));
#139425=CARTESIAN_POINT('Ctrl Pts',(19.4574566774989,21.6666486792256,6.80319091009828));
#139426=CARTESIAN_POINT('Ctrl Pts',(19.5381236778438,21.6428834392924,6.80736047604233));
#139427=CARTESIAN_POINT('Ctrl Pts',(19.6176198821349,21.6151387947156,6.81153004198637));
#139428=CARTESIAN_POINT('Ctrl Pts',(19.6955326893839,21.5835629364142,6.81569960793041));
#139429=CARTESIAN_POINT('Ctrl Pts',(19.7761848148199,21.5508769098878,6.82001577066933));
#139430=CARTESIAN_POINT('Ctrl Pts',(19.8551396382569,21.5140854441414,6.82433193340825));
#139431=CARTESIAN_POINT('Ctrl Pts',(19.9319633694496,21.4734066313236,6.82864809614717));
#139432=CARTESIAN_POINT('Ctrl Pts',(20.0062845756792,21.4340529265547,6.83282366033885));
#139433=CARTESIAN_POINT('Ctrl Pts',(20.0786110173902,21.3910615273712,6.83699922453054));
#139434=CARTESIAN_POINT('Ctrl Pts',(20.148577822739,21.3446751353979,6.84117478872222));
#139435=CARTESIAN_POINT('Ctrl Pts',(20.2220784850956,21.2959458770392,6.84556125073476));
#139436=CARTESIAN_POINT('Ctrl Pts',(20.2929744068256,21.2434699978815,6.8499477127473));
#139437=CARTESIAN_POINT('Ctrl Pts',(20.3608819013654,21.1875766564972,6.85433417475984));
#139438=CARTESIAN_POINT('Ctrl Pts',(20.4287893959052,21.1316833151129,6.85872063677238));
#139439=CARTESIAN_POINT('Ctrl Pts',(20.4937080861994,21.0723729590138,6.86310709878492));
#139440=CARTESIAN_POINT('Ctrl Pts',(20.5553006227462,21.0100175211999,6.86749356079746));
#139441=CARTESIAN_POINT('Ctrl Pts',(20.6140591953844,20.9505311495128,6.87167819519051));
#139442=CARTESIAN_POINT('Ctrl Pts',(20.6700096812721,20.8880523361676,6.87586282958356));
#139443=CARTESIAN_POINT('Ctrl Pts',(20.7228319806689,20.8228769657355,6.8800474639766));
#139444=CARTESIAN_POINT('Ctrl Pts',(20.7755790940605,20.7577943643762,6.88422614206054));
#139445=CARTESIAN_POINT('Ctrl Pts',(20.8252065780214,20.6900231841701,6.88840482014449));
#139446=CARTESIAN_POINT('Ctrl Pts',(20.8714311671561,20.6198960237255,6.89258349822843));
#139447=CARTESIAN_POINT('Ctrl Pts',(20.9184842988301,20.5485118843294,6.89683707611387));
#139448=CARTESIAN_POINT('Ctrl Pts',(20.9620110031542,20.4746868150558,6.9010906539993));
#139449=CARTESIAN_POINT('Ctrl Pts',(21.0017554861493,20.3988068256412,6.90534423188474));
#139450=CARTESIAN_POINT('Ctrl Pts',(21.0407294447865,20.324397917889,6.90951534586269));
#139451=CARTESIAN_POINT('Ctrl Pts',(21.0760663016048,20.2480134825273,6.91368645984064));
#139452=CARTESIAN_POINT('Ctrl Pts',(21.1075695674518,20.1700451024153,6.91785757381859));
#139453=CARTESIAN_POINT('Ctrl Pts',(21.1390622620736,20.0921028853463,6.92202728813896));
#139454=CARTESIAN_POINT('Ctrl Pts',(21.1667237483346,20.0125782052865,6.92619700245933));
#139455=CARTESIAN_POINT('Ctrl Pts',(21.1904053024889,19.9318834787289,6.9303667167797));
#139456=CARTESIAN_POINT('Ctrl Pts',(21.214086013952,19.8511916236359,6.93453628272375));
#139457=CARTESIAN_POINT('Ctrl Pts',(21.2337869461661,19.7693302464837,6.93870584866779));
#139458=CARTESIAN_POINT('Ctrl Pts',(21.2494093711531,19.6867264923413,6.94287541461183));
#139459=CARTESIAN_POINT('Ctrl Pts',(21.2655810613302,19.601218492106,6.94719157735075));
#139460=CARTESIAN_POINT('Ctrl Pts',(21.2773820094429,19.5149154578639,6.95150774008968));
#139461=CARTESIAN_POINT('Ctrl Pts',(21.2847607940422,19.4283001877063,6.9558239028286));
#139462=CARTESIAN_POINT('Ctrl Pts',(21.2918992155093,19.3445064008638,6.95999946702028));
#139463=CARTESIAN_POINT('Ctrl Pts',(21.2948991834511,19.2604208803107,6.96417503121195));
#139464=CARTESIAN_POINT('Ctrl Pts',(21.2937672733171,19.1764817953117,6.96835059540363));
#139465=CARTESIAN_POINT('Ctrl Pts',(21.2925781930931,19.0883031466757,6.97273705741617));
#139466=CARTESIAN_POINT('Ctrl Pts',(21.2868289009944,19.0002866979193,6.97712351942872));
#139467=CARTESIAN_POINT('Ctrl Pts',(21.2765884850301,18.9129332360151,6.98150998144126));
#139468=CARTESIAN_POINT('Ctrl Pts',(21.2663480690658,18.8255797741109,6.9858964434538));
#139469=CARTESIAN_POINT('Ctrl Pts',(21.2516167014297,18.7388898583324,6.99028290546634));
#139470=CARTESIAN_POINT('Ctrl Pts',(21.2325245180282,18.6533484665025,6.99466936747888));
#139471=CARTESIAN_POINT('Ctrl Pts',(21.2143148178507,18.5717609882543,6.99885307745108));
#139472=CARTESIAN_POINT('Ctrl Pts',(21.1920707686424,18.4909145868902,7.00303678742329));
#139473=CARTESIAN_POINT('Ctrl Pts',(21.1658678428323,18.4112382886144,7.00722049739549));
#139474=CARTESIAN_POINT('Ctrl Pts',(21.1396995424231,18.3316672771986,7.01139867887684));
#139475=CARTESIAN_POINT('Ctrl Pts',(21.1095828937132,18.253263732009,7.01557686035819));
#139476=CARTESIAN_POINT('Ctrl Pts',(21.0756441741,18.1764457182422,7.01975504183954));
#139477=CARTESIAN_POINT('Ctrl Pts',(21.0417401170704,18.0997061609065,7.02392895602483));
#139478=CARTESIAN_POINT('Ctrl Pts',(21.0040219265333,18.0245493373816,7.02810287021013));
#139479=CARTESIAN_POINT('Ctrl Pts',(20.9626649803004,17.9513760856579,7.03227678439542));
#139480=CARTESIAN_POINT('Ctrl Pts',(20.9205833372596,17.8769206207443,7.03652383798201));
#139481=CARTESIAN_POINT('Ctrl Pts',(20.8747343543852,17.8045193682345,7.0407708915686));
#139482=CARTESIAN_POINT('Ctrl Pts',(20.8253528335361,17.7345707515561,7.04501794515519));
#139483=CARTESIAN_POINT('Ctrl Pts',(20.776870658013,17.66589605193,7.04918765062193));
#139484=CARTESIAN_POINT('Ctrl Pts',(20.7249838328577,17.5995857759597,7.05335735608868));
#139485=CARTESIAN_POINT('Ctrl Pts',(20.6699585805744,17.5359882465187,7.05752706155542));
#139486=CARTESIAN_POINT('Ctrl Pts',(20.6134022489947,17.4706211139121,7.06181278920193));
#139487=CARTESIAN_POINT('Ctrl Pts',(20.5535305417894,17.4081203454085,7.06609851684844));
#139488=CARTESIAN_POINT('Ctrl Pts',(20.4906759552872,17.3488266492843,7.07038424449495));
#139489=CARTESIAN_POINT('Ctrl Pts',(20.4278213687851,17.2895329531601,7.07466997214145));
#139490=CARTESIAN_POINT('Ctrl Pts',(20.3619843020148,17.2334466741789,7.07895569978796));
#139491=CARTESIAN_POINT('Ctrl Pts',(20.2935357313021,17.1808649545431,7.08324142743447));
#139492=CARTESIAN_POINT('Origin',(18.734,19.211,-1.76670989022852));
#139493=CARTESIAN_POINT('',(20.2909847804557,17.1841769303995,7.94987222326386));
#139494=CARTESIAN_POINT('',(20.2961055579379,17.1775279377506,7.883296963941));
#139495=CARTESIAN_POINT('',(20.2935357313021,17.1808649545432,-1.76670989022852));
#139496=CARTESIAN_POINT('',(16.1743644999821,19.2104398261047,7.43329008494582));
#139497=CARTESIAN_POINT('Ctrl Pts',(16.1781030359051,19.2104411453813,7.4332901097715));
#139498=CARTESIAN_POINT('Ctrl Pts',(16.1790025448085,19.6723916862602,7.4561794192865));
#139499=CARTESIAN_POINT('Ctrl Pts',(16.519742516428,20.9911304253782,7.52146066436197));
#139500=CARTESIAN_POINT('Ctrl Pts',(18.635203471302,22.2364801012593,7.62913384499793));
#139501=CARTESIAN_POINT('Ctrl Pts',(21.2244732853929,20.9317072417885,7.75630965167935));
#139502=CARTESIAN_POINT('Ctrl Pts',(21.4803857485738,18.507708892409,7.86322244443467));
#139503=CARTESIAN_POINT('Ctrl Pts',(20.6448527341026,17.4566900324871,7.9277433016295));
#139504=CARTESIAN_POINT('Ctrl Pts',(20.2909847804557,17.1841769303995,7.94987222326386));
#139505=CARTESIAN_POINT('Ctrl Pts',(20.2935357313021,17.1808649545431,7.14996298022642));
#139506=CARTESIAN_POINT('Ctrl Pts',(20.2269740491137,17.1297327296497,7.15413571681833));
#139507=CARTESIAN_POINT('Ctrl Pts',(20.1578294014536,17.0818270510226,7.15830845341025));
#139508=CARTESIAN_POINT('Ctrl Pts',(20.0864499301619,17.0374132898812,7.16248119000217));
#139509=CARTESIAN_POINT('Ctrl Pts',(20.0151086378096,16.9930232844536,7.16665169471068));
#139510=CARTESIAN_POINT('Ctrl Pts',(19.9415352849612,16.9521217307261,7.1708221994192));
#139511=CARTESIAN_POINT('Ctrl Pts',(19.8661074862141,16.914931046406,7.17499270412771));
#139512=CARTESIAN_POINT('Ctrl Pts',(19.7906974050045,16.8777490979546,7.17916222920968));
#139513=CARTESIAN_POINT('Ctrl Pts',(19.7134341556442,16.844276490702,7.18333175429165));
#139514=CARTESIAN_POINT('Ctrl Pts',(19.6347192600783,16.8146893326357,7.18750127937362));
#139515=CARTESIAN_POINT('Ctrl Pts',(19.5559992417777,16.7851002490487,7.19167107580666));
#139516=CARTESIAN_POINT('Ctrl Pts',(19.4758278207703,16.7593972773767,7.19584087223971));
#139517=CARTESIAN_POINT('Ctrl Pts',(19.3946244766586,16.737707599001,7.20001066867275));
#139518=CARTESIAN_POINT('Ctrl Pts',(19.3133366757596,16.7159953619416,7.20418480196672));
#139519=CARTESIAN_POINT('Ctrl Pts',(19.2310152538687,16.6983048726722,7.20835893526069));
#139520=CARTESIAN_POINT('Ctrl Pts',(19.1480922894468,16.6847126893758,7.21253306855467));
#139521=CARTESIAN_POINT('Ctrl Pts',(19.0651252830309,16.6711132870074,7.21670941881175));
#139522=CARTESIAN_POINT('Ctrl Pts',(18.9815565552246,16.6616165772755,7.22088576906883));
#139523=CARTESIAN_POINT('Ctrl Pts',(18.8978233253707,16.6562471904185,7.22506211932592));
#139524=CARTESIAN_POINT('Ctrl Pts',(18.8139434930286,16.6508684026883,7.2292457816542));
#139525=CARTESIAN_POINT('Ctrl Pts',(18.7298990438713,16.6496313793322,7.2334294439825));
#139526=CARTESIAN_POINT('Ctrl Pts',(18.6461270288959,16.6525085810288,7.23761310631078));
#139527=CARTESIAN_POINT('Ctrl Pts',(18.5794262634492,16.6547994600957,7.24094421252506));
#139528=CARTESIAN_POINT('Ctrl Pts',(18.5128982458229,16.6596975650841,7.24427531873934));
#139529=CARTESIAN_POINT('Ctrl Pts',(18.4467595506041,16.6671657042506,7.24760642495362));
#139530=CARTESIAN_POINT('Ctrl Pts',(18.3636741606704,16.6765474021004,7.25179105934667));
#139531=CARTESIAN_POINT('Ctrl Pts',(18.2808942658293,16.6900213769478,7.25597569373972));
#139532=CARTESIAN_POINT('Ctrl Pts',(18.1988547913486,16.7075584477249,7.26016032813276));
#139533=CARTESIAN_POINT('Ctrl Pts',(18.116932089905,16.7250705566525,7.26433900621672));
#139534=CARTESIAN_POINT('Ctrl Pts',(18.0357481614728,16.7466341786849,7.26851768430068));
#139535=CARTESIAN_POINT('Ctrl Pts',(17.9557323296054,16.77216842869,7.27269636238463));
#139536=CARTESIAN_POINT('Ctrl Pts',(17.8742822714585,16.7981603617751,7.27694994027007));
#139537=CARTESIAN_POINT('Ctrl Pts',(17.7940430771259,16.8282666158667,7.2812035181555));
#139538=CARTESIAN_POINT('Ctrl Pts',(17.7154562415191,16.8623474901426,7.28545709604093));
#139539=CARTESIAN_POINT('Ctrl Pts',(17.63839296507,16.8957676401673,7.28962821001889));
#139540=CARTESIAN_POINT('Ctrl Pts',(17.5629189921761,16.9330094826425,7.29379932399685));
#139541=CARTESIAN_POINT('Ctrl Pts',(17.4894331713713,16.9738917305867,7.2979704379748));
#139542=CARTESIAN_POINT('Ctrl Pts',(17.4159720094435,17.0147602600978,7.30214015229517));
#139543=CARTESIAN_POINT('Ctrl Pts',(17.3444980763215,17.059266545551,7.30630986661554));
#139544=CARTESIAN_POINT('Ctrl Pts',(17.2753861385062,17.1071830870871,7.31047958093591));
#139545=CARTESIAN_POINT('Ctrl Pts',(17.2062766599905,17.155097923547,7.31464914687994));
#139546=CARTESIAN_POINT('Ctrl Pts',(17.1395293872397,17.2064225119979,7.31881871282397));
#139547=CARTESIAN_POINT('Ctrl Pts',(17.0754894346056,17.2608864893358,7.322988278768));
#139548=CARTESIAN_POINT('Ctrl Pts',(17.0091979162384,17.3172653529285,7.32730444150692));
#139549=CARTESIAN_POINT('Ctrl Pts',(16.9458080406878,17.377008133023,7.33162060424584));
#139550=CARTESIAN_POINT('Ctrl Pts',(16.885663067504,17.4397714478444,7.33593676698476));
#139551=CARTESIAN_POINT('Ctrl Pts',(16.8274773104956,17.5004902542869,7.34011233117644));
#139552=CARTESIAN_POINT('Ctrl Pts',(16.7723285700598,17.5640354429535,7.34428789536812));
#139553=CARTESIAN_POINT('Ctrl Pts',(16.7204869451086,17.6300619310733,7.3484634595598));
#139554=CARTESIAN_POINT('Ctrl Pts',(16.6660269229228,17.6994232601449,7.35284992157234));
#139555=CARTESIAN_POINT('Ctrl Pts',(16.6152172172816,17.7715226597539,7.35723638358488));
#139556=CARTESIAN_POINT('Ctrl Pts',(16.5683186145658,17.845927058072,7.36162284559743));
#139557=CARTESIAN_POINT('Ctrl Pts',(16.52142001185,17.9203314563902,7.36600930760997));
#139558=CARTESIAN_POINT('Ctrl Pts',(16.4784327293519,17.9970403100744,7.37039576962251));
#139559=CARTESIAN_POINT('Ctrl Pts',(16.4395601204679,18.0755945044995,7.37478223163505));
#139560=CARTESIAN_POINT('Ctrl Pts',(16.399796394139,18.1559494788318,7.37926924910124));
#139561=CARTESIAN_POINT('Ctrl Pts',(16.3642056179145,18.2385006465143,7.38375626656742));
#139562=CARTESIAN_POINT('Ctrl Pts',(16.3330179090159,18.3228080169392,7.3882432840336));
#139563=CARTESIAN_POINT('Ctrl Pts',(16.3019356806123,18.4068302499339,7.39271512587964));
#139564=CARTESIAN_POINT('Ctrl Pts',(16.2752269677052,18.4925965155752,7.39718696772568));
#139565=CARTESIAN_POINT('Ctrl Pts',(16.2530742870064,18.5796462112197,7.40165880957171));
#139566=CARTESIAN_POINT('Ctrl Pts',(16.2309688572624,18.6665102326658,7.40612111312305));
#139567=CARTESIAN_POINT('Ctrl Pts',(16.2134002030055,18.7546518909164,7.41058341667439));
#139568=CARTESIAN_POINT('Ctrl Pts',(16.2005019648759,18.8435932689479,7.41504572022573));
#139569=CARTESIAN_POINT('Ctrl Pts',(16.1876417930138,18.9322721563783,7.41949485428535));
#139570=CARTESIAN_POINT('Ctrl Pts',(16.1794246278368,19.0217457093711,7.42394398834497));
#139571=CARTESIAN_POINT('Ctrl Pts',(16.1759333991831,19.1115250494595,7.42839312240459));
#139572=CARTESIAN_POINT('Ctrl Pts',(16.1746525201579,19.1444637323753,7.43002544244498));
#139573=CARTESIAN_POINT('Ctrl Pts',(16.1740072831437,19.177443453577,7.43165776248538));
#139574=CARTESIAN_POINT('Ctrl Pts',(16.1740000613162,19.2104396974995,7.43329008252577));
#139575=CARTESIAN_POINT('',(16.1738764730989,19.2121301833587,7.36670989022851));
#139576=CARTESIAN_POINT('Ctrl Pts',(20.2935357313021,17.1808649545431,7.08324142743447));
#139577=CARTESIAN_POINT('Ctrl Pts',(20.2268458566708,17.1296342530998,7.08741703894065));
#139578=CARTESIAN_POINT('Ctrl Pts',(20.1576774870271,17.0817303986562,7.09159265044683));
#139579=CARTESIAN_POINT('Ctrl Pts',(20.0864031281849,17.0373841694366,7.09576826195301));
#139580=CARTESIAN_POINT('Ctrl Pts',(20.0122177785098,16.9912267493648,7.10011441398756));
#139581=CARTESIAN_POINT('Ctrl Pts',(19.93575121291,16.948924058118,7.10446056602211));
#139582=CARTESIAN_POINT('Ctrl Pts',(19.8574497100952,16.910682467813,7.10880671805666));
#139583=CARTESIAN_POINT('Ctrl Pts',(19.7791482072804,16.872440877508,7.11315287009122));
#139584=CARTESIAN_POINT('Ctrl Pts',(19.6990123054848,16.8382605382041,7.11749902212576));
#139585=CARTESIAN_POINT('Ctrl Pts',(19.6175072439402,16.8082900820313,7.12184517416032));
#139586=CARTESIAN_POINT('Ctrl Pts',(19.5390311848803,16.7794334289094,7.12602980855336));
#139587=CARTESIAN_POINT('Ctrl Pts',(19.4589938470389,16.7543718340009,7.13021444294641));
#139588=CARTESIAN_POINT('Ctrl Pts',(19.3777970941006,16.733274167381,7.13439907733946));
#139589=CARTESIAN_POINT('Ctrl Pts',(19.2967159146901,16.7122065306782,7.1385777554234));
#139590=CARTESIAN_POINT('Ctrl Pts',(19.2144790396056,16.6950917298573,7.14275643350734));
#139591=CARTESIAN_POINT('Ctrl Pts',(19.1315065014626,16.6820499053372,7.14693511159128));
#139592=CARTESIAN_POINT('Ctrl Pts',(19.0470467402047,16.6687743154856,7.15118868947672));
#139593=CARTESIAN_POINT('Ctrl Pts',(18.9618251354749,16.6597193207395,7.15544226736216));
#139594=CARTESIAN_POINT('Ctrl Pts',(18.8762989641012,16.654957941501,7.15969584524759));
#139595=CARTESIAN_POINT('Ctrl Pts',(18.7924308844501,16.6502888708901,7.16386695922554));
#139596=CARTESIAN_POINT('Ctrl Pts',(18.7082704224839,16.6497484479464,7.1680380732035));
#139597=CARTESIAN_POINT('Ctrl Pts',(18.6242553740812,16.6533534026215,7.17220918718145));
#139598=CARTESIAN_POINT('Ctrl Pts',(18.5402685177394,16.6569571476192,7.17637890150182));
#139599=CARTESIAN_POINT('Ctrl Pts',(18.4564274372811,16.6647034879404,7.1805486158222));
#139600=CARTESIAN_POINT('Ctrl Pts',(18.3731691163825,16.6765570486934,7.18471833014257));
#139601=CARTESIAN_POINT('Ctrl Pts',(18.2899137581723,16.6884101876458,7.18888789608661));
#139602=CARTESIAN_POINT('Ctrl Pts',(18.2072415736113,16.7043701907562,7.19305746203066));
#139603=CARTESIAN_POINT('Ctrl Pts',(18.1255822535274,16.7243500757491,7.1972270279747));
#139604=CARTESIAN_POINT('Ctrl Pts',(18.041051892487,16.7450324288504,7.20154319071362));
#139605=CARTESIAN_POINT('Ctrl Pts',(17.9576074580676,16.7700224760727,7.20585935345254));
#139606=CARTESIAN_POINT('Ctrl Pts',(17.8757097136975,16.799167131736,7.21017551619146));
#139607=CARTESIAN_POINT('Ctrl Pts',(17.7964797797362,16.8273624033065,7.21435108038314));
#139608=CARTESIAN_POINT('Ctrl Pts',(17.7186977338734,16.8594455439839,7.21852664457482));
#139609=CARTESIAN_POINT('Ctrl Pts',(17.6427597031134,16.8952291532946,7.2227022087665));
#139610=CARTESIAN_POINT('Ctrl Pts',(17.5629862229451,16.9328201076441,7.22708867077904));
#139611=CARTESIAN_POINT('Ctrl Pts',(17.485248450476,16.9744949002993,7.23147513279158));
#139612=CARTESIAN_POINT('Ctrl Pts',(17.409973629261,17.0199833023028,7.23586159480412));
#139613=CARTESIAN_POINT('Ctrl Pts',(17.3346988080461,17.0654717043064,7.24024805681667));
#139614=CARTESIAN_POINT('Ctrl Pts',(17.2618873758783,17.1147733273606,7.24463451882921));
#139615=CARTESIAN_POINT('Ctrl Pts',(17.1919269101811,17.1675689183003,7.24902098084175));
#139616=CARTESIAN_POINT('Ctrl Pts',(17.1258771580207,17.2174132934338,7.25316224442401));
#139617=CARTESIAN_POINT('Ctrl Pts',(17.0621112325389,17.2705657001619,7.25730350800627));
#139618=CARTESIAN_POINT('Ctrl Pts',(17.0009846311416,17.326787238314,7.26144477158852));
#139619=CARTESIAN_POINT('Ctrl Pts',(16.9399453026366,17.3829285067285,7.26558012252321));
#139620=CARTESIAN_POINT('Ctrl Pts',(16.8815381604268,17.4421298917806,7.2697154734579));
#139621=CARTESIAN_POINT('Ctrl Pts',(16.8260879518441,17.5041105435613,7.27385082439259));
#139622=CARTESIAN_POINT('Ctrl Pts',(16.7707013118209,17.5660201402305,7.27798143452813));
#139623=CARTESIAN_POINT('Ctrl Pts',(16.7182651826551,17.6307023247235,7.28211204466367));
#139624=CARTESIAN_POINT('Ctrl Pts',(16.6690684130045,17.6978385608177,7.28624265479921));
#139625=CARTESIAN_POINT('Ctrl Pts',(16.6199019406792,17.7649334517505,7.29037072114092));
#139626=CARTESIAN_POINT('Ctrl Pts',(16.5739711466916,17.8344790168686,7.29449878748264));
#139627=CARTESIAN_POINT('Ctrl Pts',(16.5315246255303,17.9061236744984,7.29862685382436));
#139628=CARTESIAN_POINT('Ctrl Pts',(16.4890908665707,17.977746791056,7.3027536789992));
#139629=CARTESIAN_POINT('Ctrl Pts',(16.4501395400176,18.0514673424197,7.30688050417405));
#139630=CARTESIAN_POINT('Ctrl Pts',(16.4148750854129,18.1269060785424,7.3110073293489));
#139631=CARTESIAN_POINT('Ctrl Pts',(16.3796101195078,18.2023459084537,7.31513421435872));
#139632=CARTESIAN_POINT('Ctrl Pts',(16.3480323287909,18.2795035453344,7.31926109936854));
#139633=CARTESIAN_POINT('Ctrl Pts',(16.3202988339461,18.3579779129531,7.32338798437835));
#139634=CARTESIAN_POINT('Ctrl Pts',(16.2925397363851,18.4365247257132,7.32751867920247));
#139635=CARTESIAN_POINT('Ctrl Pts',(16.2686321752694,18.516390251046,7.33164937402659));
#139636=CARTESIAN_POINT('Ctrl Pts',(16.2486837569799,18.5971570459957,7.33578006885071));
#139637=CARTESIAN_POINT('Ctrl Pts',(16.2287250388403,18.6779655427923,7.33991289645232));
#139638=CARTESIAN_POINT('Ctrl Pts',(16.2127296214478,18.7596757735077,7.34404572405394));
#139639=CARTESIAN_POINT('Ctrl Pts',(16.2007537416511,18.8418612800569,7.34817855165556));
#139640=CARTESIAN_POINT('Ctrl Pts',(16.1887593096482,18.9241741027186,7.35231778154836));
#139641=CARTESIAN_POINT('Ctrl Pts',(16.180796886798,19.0069632027562,7.35645701144116));
#139642=CARTESIAN_POINT('Ctrl Pts',(16.176870697397,19.0897988045885,7.36059624133397));
#139643=CARTESIAN_POINT('Ctrl Pts',(16.1749377014765,19.1305815748691,7.36263412429881));
#139644=CARTESIAN_POINT('Ctrl Pts',(16.1739822581149,19.1713756409971,7.36467200726366));
#139645=CARTESIAN_POINT('Ctrl Pts',(16.1740002494514,19.2121301287168,7.36670989022851));
#139646=CARTESIAN_POINT('Ctrl Pts',(16.1703788196327,19.2121317274208,7.36670989022851));
#139647=CARTESIAN_POINT('Ctrl Pts',(16.1700290407744,19.2754624167648,7.36987218932674));
#139648=CARTESIAN_POINT('Ctrl Pts',(16.2008981366677,20.1874206696652,7.41542642398544));
#139649=CARTESIAN_POINT('Ctrl Pts',(17.2895132664939,21.8712161675055,7.50337259420461));
#139650=CARTESIAN_POINT('Ctrl Pts',(20.1889475365473,21.8655093043776,7.63054840088606));
#139651=CARTESIAN_POINT('Ctrl Pts',(21.7469837784997,19.4347114040786,7.75718985746491));
#139652=CARTESIAN_POINT('Ctrl Pts',(20.9598514275375,17.6886843310748,7.84143937848329));
#139653=CARTESIAN_POINT('Ctrl Pts',(20.2961055579348,17.1775279377483,7.88329696394119));
#139654=CARTESIAN_POINT('Origin',(18.734,19.211,-1.76670989022852));
#139655=CARTESIAN_POINT('',(20.2935357313021,17.1808649545431,8.74981199697632));
#139656=CARTESIAN_POINT('',(20.2935357313021,17.1808649545431,8.68337763228924));
#139657=CARTESIAN_POINT('',(20.2935357313021,17.1808649545432,-1.76670989022852));
#139658=CARTESIAN_POINT('',(16.1740010826189,19.2133543592346,8.23329012251325));
#139659=CARTESIAN_POINT('Ctrl Pts',(16.1740010826189,19.2133543592346,8.23329012251325));
#139660=CARTESIAN_POINT('Ctrl Pts',(16.1741014808466,19.322521792358,8.23871812867197));
#139661=CARTESIAN_POINT('Ctrl Pts',(16.1811885397039,19.4313771444072,8.24414613483068));
#139662=CARTESIAN_POINT('Ctrl Pts',(16.1951208364047,19.5391654958424,8.2495741409894));
#139663=CARTESIAN_POINT('Ctrl Pts',(16.2083299266963,19.6413587018203,8.25472038679463));
#139664=CARTESIAN_POINT('Ctrl Pts',(16.2276915596972,19.7425933354954,8.25986663259986));
#139665=CARTESIAN_POINT('Ctrl Pts',(16.253046772176,19.84224565848,8.2650128784051));
#139666=CARTESIAN_POINT('Ctrl Pts',(16.2736641888712,19.9232772597465,8.26919751279815));
#139667=CARTESIAN_POINT('Ctrl Pts',(16.2982940662942,20.0034485022604,8.27338214719119));
#139668=CARTESIAN_POINT('Ctrl Pts',(16.3268482220627,20.0823324956487,8.27756678158424));
#139669=CARTESIAN_POINT('Ctrl Pts',(16.3553617345248,20.1611042074362,8.28174545966818));
#139670=CARTESIAN_POINT('Ctrl Pts',(16.3877882750863,20.2385918806366,8.28592413775213));
#139671=CARTESIAN_POINT('Ctrl Pts',(16.42398920314,20.3143812207891,8.29010281583607));
#139672=CARTESIAN_POINT('Ctrl Pts',(16.4608390068118,20.391529030395,8.29435639372151));
#139673=CARTESIAN_POINT('Ctrl Pts',(16.5015997218018,20.466916555597,8.29860997160694));
#139674=CARTESIAN_POINT('Ctrl Pts',(16.5460727818106,20.5401254598065,8.30286354949237));
#139675=CARTESIAN_POINT('Ctrl Pts',(16.5896836447691,20.6119150665525,8.30703466347033));
#139676=CARTESIAN_POINT('Ctrl Pts',(16.6368639453123,20.6816093608383,8.31120577744828));
#139677=CARTESIAN_POINT('Ctrl Pts',(16.6873797310323,20.7488379221006,8.31537689142623));
#139678=CARTESIAN_POINT('Ctrl Pts',(16.7378785656926,20.8160439241699,8.3195466057466));
#139679=CARTESIAN_POINT('Ctrl Pts',(16.791710386553,20.8807854689741,8.32371632006698));
#139680=CARTESIAN_POINT('Ctrl Pts',(16.8485987415146,20.9427222913913,8.32788603438735));
#139681=CARTESIAN_POINT('Ctrl Pts',(16.9054850721444,21.0046569098306,8.33205560033139));
#139682=CARTESIAN_POINT('Ctrl Pts',(16.9654274088047,21.0637866660881,8.33622516627544));
#139683=CARTESIAN_POINT('Ctrl Pts',(17.0281108772061,21.1198065121257,8.34039473221948));
#139684=CARTESIAN_POINT('Ctrl Pts',(17.0929982190279,21.177795946842,8.3447108949584));
#139685=CARTESIAN_POINT('Ctrl Pts',(17.1608226421282,21.2324523620818,8.34902705769732));
#139686=CARTESIAN_POINT('Ctrl Pts',(17.2311971876104,21.283482498617,8.35334322043624));
#139687=CARTESIAN_POINT('Ctrl Pts',(17.2992792896757,21.3328503338221,8.35751878462792));
#139688=CARTESIAN_POINT('Ctrl Pts',(17.3697475047297,21.3788242964687,8.3616943488196));
#139689=CARTESIAN_POINT('Ctrl Pts',(17.4422231594137,21.4211838371785,8.36586991301128));
#139690=CARTESIAN_POINT('Ctrl Pts',(17.5183593871213,21.4656828575893,8.37025637502382));
#139691=CARTESIAN_POINT('Ctrl Pts',(17.5967106568094,21.506192463235,8.37464283703637));
#139692=CARTESIAN_POINT('Ctrl Pts',(17.6768123961766,21.5425133219268,8.3790292990489));
#139693=CARTESIAN_POINT('Ctrl Pts',(17.7569141355439,21.5788341806186,8.38341576106144));
#139694=CARTESIAN_POINT('Ctrl Pts',(17.8387657767032,21.6109661511407,8.38780222307398));
#139695=CARTESIAN_POINT('Ctrl Pts',(17.921884774769,21.638770347654,8.39218868508652));
#139696=CARTESIAN_POINT('Ctrl Pts',(18.001179344522,21.66529523187,8.39637331947957));
#139697=CARTESIAN_POINT('Ctrl Pts',(18.0819223576084,21.6879805757247,8.40055795387261));
#139698=CARTESIAN_POINT('Ctrl Pts',(18.1637071353304,21.7066694589843,8.40474258826566));
#139699=CARTESIAN_POINT('Ctrl Pts',(18.2453755025443,21.7253317409318,8.4089212663496));
#139700=CARTESIAN_POINT('Ctrl Pts',(18.3280822444037,21.7400087597643,8.41309994443355));
#139701=CARTESIAN_POINT('Ctrl Pts',(18.4114039612994,21.7505928405582,8.4172786225175));
#139702=CARTESIAN_POINT('Ctrl Pts',(18.4962191600882,21.7613666333938,8.42153220040293));
#139703=CARTESIAN_POINT('Ctrl Pts',(18.5816711403845,21.7678991601646,8.42578577828837));
#139704=CARTESIAN_POINT('Ctrl Pts',(18.6673006671489,21.7701309460434,8.43003935617381));
#139705=CARTESIAN_POINT('Ctrl Pts',(18.7512700984447,21.7723194643981,8.43421047015176));
#139706=CARTESIAN_POINT('Ctrl Pts',(18.8354097724167,21.7703724977257,8.43838158412971));
#139707=CARTESIAN_POINT('Ctrl Pts',(18.9192815899904,21.7642862613523,8.44255269810766));
#139708=CARTESIAN_POINT('Ctrl Pts',(19.0031252635657,21.7582020672744,8.44672241242803));
#139709=CARTESIAN_POINT('Ctrl Pts',(19.0867008008049,21.7479813952832,8.45089212674841));
#139710=CARTESIAN_POINT('Ctrl Pts',(19.1695724543108,21.7336725187875,8.45506184106878));
#139711=CARTESIAN_POINT('Ctrl Pts',(19.2524411588877,21.719364151463,8.45923140701282));
#139712=CARTESIAN_POINT('Ctrl Pts',(19.3346055763514,21.7009679479898,8.46340097295687));
#139713=CARTESIAN_POINT('Ctrl Pts',(19.4156387740957,21.678583551098,8.46757053890091));
#139714=CARTESIAN_POINT('Ctrl Pts',(19.4995209991075,21.6554121464256,8.47188670163983));
#139715=CARTESIAN_POINT('Ctrl Pts',(19.5821904685913,21.6279670209743,8.47620286437875));
#139716=CARTESIAN_POINT('Ctrl Pts',(19.6631911444339,21.5964148102805,8.48051902711767));
#139717=CARTESIAN_POINT('Ctrl Pts',(19.7415532317807,21.5658904095313,8.48469459130935));
#139718=CARTESIAN_POINT('Ctrl Pts',(19.8183531671025,21.5315226265231,8.48887015550103));
#139719=CARTESIAN_POINT('Ctrl Pts',(19.8932005345677,21.4935104864289,8.49304571969271));
#139720=CARTESIAN_POINT('Ctrl Pts',(19.9718282646309,21.4535784435038,8.49743218170526));
#139721=CARTESIAN_POINT('Ctrl Pts',(20.0483004884277,21.409624506264,8.5018186437178));
#139722=CARTESIAN_POINT('Ctrl Pts',(20.1221981349569,21.3619314117615,8.50620510573034));
#139723=CARTESIAN_POINT('Ctrl Pts',(20.196095781486,21.314238317259,8.51059156774288));
#139724=CARTESIAN_POINT('Ctrl Pts',(20.267418424621,21.2628064665597,8.51497802975542));
#139725=CARTESIAN_POINT('Ctrl Pts',(20.3357880909557,21.2079664272773,8.51936449176796));
#139726=CARTESIAN_POINT('Ctrl Pts',(20.4010119675942,21.1556496594946,8.52354912616101));
#139727=CARTESIAN_POINT('Ctrl Pts',(20.463791413314,21.1000367097147,8.52773376055406));
#139728=CARTESIAN_POINT('Ctrl Pts',(20.5237743555653,21.0413845924179,8.53191839494711));
#139729=CARTESIAN_POINT('Ctrl Pts',(20.5836719195227,20.9828159591504,8.53609707303105));
#139730=CARTESIAN_POINT('Ctrl Pts',(20.6407805603833,20.9212170697946,8.540275751115));
#139731=CARTESIAN_POINT('Ctrl Pts',(20.6947805623983,20.8568856540237,8.54445442919894));
#139732=CARTESIAN_POINT('Ctrl Pts',(20.7497484756402,20.7914011438593,8.54870800708438));
#139733=CARTESIAN_POINT('Ctrl Pts',(20.8014948330691,20.723085484341,8.55296158496981));
#139734=CARTESIAN_POINT('Ctrl Pts',(20.8497210505506,20.6522926268656,8.55721516285525));
#139735=CARTESIAN_POINT('Ctrl Pts',(20.8970123087005,20.5828722270733,8.5613862768332));
#139736=CARTESIAN_POINT('Ctrl Pts',(20.940918427529,20.5110702205224,8.56555739081115));
#139737=CARTESIAN_POINT('Ctrl Pts',(20.9811990900047,20.4372529306315,8.56972850478911));
#139738=CARTESIAN_POINT('Ctrl Pts',(21.021466235915,20.3634604108451,8.57389821910948));
#139739=CARTESIAN_POINT('Ctrl Pts',(21.058110121399,20.2876543542439,8.57806793342985));
#139740=CARTESIAN_POINT('Ctrl Pts',(21.0909354749524,20.2102272849111,8.58223764775022));
#139741=CARTESIAN_POINT('Ctrl Pts',(21.1237596604389,20.1328029707657,8.58640721369427));
#139742=CARTESIAN_POINT('Ctrl Pts',(21.1527654053819,20.0537581824513,8.59057677963831));
#139743=CARTESIAN_POINT('Ctrl Pts',(21.1778054030264,19.9735058374459,8.59474634558236));
#139744=CARTESIAN_POINT('Ctrl Pts',(21.2037257760978,19.8904319189922,8.59906250832128));
#139745=CARTESIAN_POINT('Ctrl Pts',(21.2253961847597,19.8060644520148,8.6033786710602));
#139746=CARTESIAN_POINT('Ctrl Pts',(21.242709898346,19.7208770890524,8.60769483379912));
#139747=CARTESIAN_POINT('Ctrl Pts',(21.2594596195334,19.6384646954784,8.6118703979908));
#139748=CARTESIAN_POINT('Ctrl Pts',(21.2721321012068,19.5552854746202,8.61604596218248));
#139749=CARTESIAN_POINT('Ctrl Pts',(21.2806833673555,19.4717754329589,8.62022152637416));
#139750=CARTESIAN_POINT('Ctrl Pts',(21.2896665376286,19.3840474976196,8.6246079883867));
#139751=CARTESIAN_POINT('Ctrl Pts',(21.2941011966021,19.2959550268227,8.62899445039924));
#139752=CARTESIAN_POINT('Ctrl Pts',(21.2939982462078,19.2080034331647,8.63338091241178));
#139753=CARTESIAN_POINT('Ctrl Pts',(21.2938952958136,19.1200518395066,8.63776737442432));
#139754=CARTESIAN_POINT('Ctrl Pts',(21.2892548426303,19.0322416983818,8.64215383643686));
#139755=CARTESIAN_POINT('Ctrl Pts',(21.2801502518719,18.9450697555886,8.6465402984494));
#139756=CARTESIAN_POINT('Ctrl Pts',(21.2712189218945,18.8595566988775,8.65084328588802));
#139757=CARTESIAN_POINT('Ctrl Pts',(21.2579577430371,18.7743304226481,8.65514627332665));
#139758=CARTESIAN_POINT('Ctrl Pts',(21.2403952839669,18.6898640479603,8.65944926076527));
#139759=CARTESIAN_POINT('Ctrl Pts',(21.2233438126719,18.607855261057,8.66362705081729));
#139760=CARTESIAN_POINT('Ctrl Pts',(21.2022379877299,18.5265632615501,8.66780484086931));
#139761=CARTESIAN_POINT('Ctrl Pts',(21.1771565043192,18.4464175679479,8.67198263092133));
#139762=CARTESIAN_POINT('Ctrl Pts',(21.1520996593001,18.3663506041782,8.67615631698851));
#139763=CARTESIAN_POINT('Ctrl Pts',(21.1230750469804,18.2874281469208,8.6803300030557));
#139764=CARTESIAN_POINT('Ctrl Pts',(21.0902120820861,18.2100681220825,8.68450368912288));
#139765=CARTESIAN_POINT('Ctrl Pts',(21.0573715401327,18.1327608812602,8.68867452741549));
#139766=CARTESIAN_POINT('Ctrl Pts',(21.0206980272887,18.0570143773557,8.6928453657081));
#139767=CARTESIAN_POINT('Ctrl Pts',(20.9803698805643,17.9832287022033,8.69701620400071));
#139768=CARTESIAN_POINT('Ctrl Pts',(20.940057152362,17.909471237275,8.70118544767101));
#139769=CARTESIAN_POINT('Ctrl Pts',(20.8960927884101,17.8376735138885,8.70535469134131));
#139770=CARTESIAN_POINT('Ctrl Pts',(20.8487014663918,17.7682118284237,8.70952393501162));
#139771=CARTESIAN_POINT('Ctrl Pts',(20.8012991468732,17.6987340238706,8.71369414618519));
#139772=CARTESIAN_POINT('Ctrl Pts',(20.7504685354779,17.631593723403,8.71786435735875));
#139773=CARTESIAN_POINT('Ctrl Pts',(20.6964775867251,17.5671381683361,8.72203456853232));
#139774=CARTESIAN_POINT('Ctrl Pts',(20.6424782965623,17.5026726551144,8.72620542398872));
#139775=CARTESIAN_POINT('Ctrl Pts',(20.58531800187,17.4408930576723,8.73037627944512));
#139776=CARTESIAN_POINT('Ctrl Pts',(20.5253036550083,17.3821120276097,8.73454713490153));
#139777=CARTESIAN_POINT('Ctrl Pts',(20.4652395196375,17.32328223221,8.73872145054181));
#139778=CARTESIAN_POINT('Ctrl Pts',(20.4023169461193,17.2674562791756,8.74289576618209));
#139779=CARTESIAN_POINT('Ctrl Pts',(20.3368776257449,17.2149079888727,8.74707008182237));
#139780=CARTESIAN_POINT('Ctrl Pts',(20.3225496033287,17.2034024738844,8.74798405354036));
#139781=CARTESIAN_POINT('Ctrl Pts',(20.3081010462363,17.1920539289557,8.74889802525834));
#139782=CARTESIAN_POINT('Ctrl Pts',(20.2935357313021,17.1808649545431,8.74981199697633));
#139783=CARTESIAN_POINT('Ctrl Pts',(20.2909847804557,17.1841769303995,7.94987222326386));
#139784=CARTESIAN_POINT('Ctrl Pts',(19.9669549252628,16.9346420965791,7.97013523718998));
#139785=CARTESIAN_POINT('Ctrl Pts',(18.7905372649548,16.3911014087415,8.03279018667658));
#139786=CARTESIAN_POINT('Ctrl Pts',(16.7471750875427,17.0720885005601,8.12726281551246));
#139787=CARTESIAN_POINT('Ctrl Pts',(16.180230297531,18.573538664413,8.20147243042223));
#139788=CARTESIAN_POINT('Ctrl Pts',(16.1744184457826,19.2133537191784,8.23329010977151));
#139789=CARTESIAN_POINT('',(16.1740010575059,19.2086731074563,8.16670989022852));
#139790=CARTESIAN_POINT('Ctrl Pts',(20.2961055579348,17.1775279377483,7.88329696394119));
#139791=CARTESIAN_POINT('Ctrl Pts',(20.2876322389503,17.1710025620435,7.88383131404377));
#139792=CARTESIAN_POINT('Ctrl Pts',(19.6033699010056,16.6514603046632,7.92675759970683));
#139793=CARTESIAN_POINT('Ctrl Pts',(17.6781136453352,16.37403049238,8.01207582093036));
#139794=CARTESIAN_POINT('Ctrl Pts',(16.2739021846612,17.9910560858828,8.10601244625689));
#139795=CARTESIAN_POINT('Ctrl Pts',(16.1718447049445,19.0247813383249,8.15755713602294));
#139796=CARTESIAN_POINT('Ctrl Pts',(16.1735502234357,19.2086726976739,8.16670989022852));
#139797=CARTESIAN_POINT('Ctrl Pts',(16.1740010575059,19.2086731074563,8.16670989022852));
#139798=CARTESIAN_POINT('Ctrl Pts',(16.1739251952239,19.2921352174732,8.17086478789788));
#139799=CARTESIAN_POINT('Ctrl Pts',(16.1779353066412,19.375721983002,8.17501968556725));
#139800=CARTESIAN_POINT('Ctrl Pts',(16.1860403077383,19.458994771335,8.17917458323661));
#139801=CARTESIAN_POINT('Ctrl Pts',(16.1940671586084,19.5414646248839,8.18328941845664));
#139802=CARTESIAN_POINT('Ctrl Pts',(16.206110236511,19.6236260477268,8.18740425367667));
#139803=CARTESIAN_POINT('Ctrl Pts',(16.2221259449782,19.7050533692914,8.1915190888967));
#139804=CARTESIAN_POINT('Ctrl Pts',(16.238134689091,19.7864452825742,8.19563213480029));
#139805=CARTESIAN_POINT('Ctrl Pts',(16.2581125446655,19.8671032636359,8.19974518070388));
#139806=CARTESIAN_POINT('Ctrl Pts',(16.2819644394347,19.9466096857188,8.20385822660747));
#139807=CARTESIAN_POINT('Ctrl Pts',(16.3058135810413,20.0261069305807,8.20797079775279));
#139808=CARTESIAN_POINT('Ctrl Pts',(16.3335357367831,20.1044524267965,8.21208336889812));
#139809=CARTESIAN_POINT('Ctrl Pts',(16.364985800536,20.1812431255815,8.21619594004344));
#139810=CARTESIAN_POINT('Ctrl Pts',(16.3969970744394,20.2594041147404,8.22038189789759));
#139811=CARTESIAN_POINT('Ctrl Pts',(16.4328704281986,20.3359537977656,8.22456785575174));
#139812=CARTESIAN_POINT('Ctrl Pts',(16.4724022025115,20.4104896424709,8.22875381360589));
#139813=CARTESIAN_POINT('Ctrl Pts',(16.5112918107484,20.4838147044136,8.23287177349698));
#139814=CARTESIAN_POINT('Ctrl Pts',(16.5537215594669,20.555190490736,8.23698973338807));
#139815=CARTESIAN_POINT('Ctrl Pts',(16.5994527799559,20.6242615346786,8.24110769327916));
#139816=CARTESIAN_POINT('Ctrl Pts',(16.6463167081171,20.6950433858238,8.24532765011484));
#139817=CARTESIAN_POINT('Ctrl Pts',(16.696647513794,20.7634043768934,8.24954760695052));
#139818=CARTESIAN_POINT('Ctrl Pts',(16.7501447185242,20.828998214511,8.2537675637862));
#139819=CARTESIAN_POINT('Ctrl Pts',(16.8036419232544,20.8945920521286,8.25798752062187));
#139820=CARTESIAN_POINT('Ctrl Pts',(16.8603051182411,20.9574183953713,8.26220747745755));
#139821=CARTESIAN_POINT('Ctrl Pts',(16.9197953580223,21.0171731691692,8.26642743429323));
#139822=CARTESIAN_POINT('Ctrl Pts',(16.9787876447051,21.0764277756308,8.27061206868628));
#139823=CARTESIAN_POINT('Ctrl Pts',(17.040795780927,21.1328994502153,8.27479670307933));
#139824=CARTESIAN_POINT('Ctrl Pts',(17.1055265727616,21.1862656268913,8.27898133747238));
#139825=CARTESIAN_POINT('Ctrl Pts',(17.170165228326,21.2395558434202,8.28316001555633));
#139826=CARTESIAN_POINT('Ctrl Pts',(17.2375184898922,21.2897490519969,8.28733869364028));
#139827=CARTESIAN_POINT('Ctrl Pts',(17.3072561423607,21.3365592122283,8.29151737172423));
#139828=CARTESIAN_POINT('Ctrl Pts',(17.3782437921302,21.3842084109399,8.29577094960966));
#139829=CARTESIAN_POINT('Ctrl Pts',(17.4517018138305,21.4283517444168,8.30002452749509));
#139830=CARTESIAN_POINT('Ctrl Pts',(17.5272463530815,21.4687301954948,8.30427810538053));
#139831=CARTESIAN_POINT('Ctrl Pts',(17.6013263140261,21.5083258315065,8.30844921935848));
#139832=CARTESIAN_POINT('Ctrl Pts',(17.6774121876527,21.5443010347693,8.31262033333643));
#139833=CARTESIAN_POINT('Ctrl Pts',(17.7551140500804,21.5764560442016,8.31679144731439));
#139834=CARTESIAN_POINT('Ctrl Pts',(17.8327898388977,21.60860026371,8.32096116163476));
#139835=CARTESIAN_POINT('Ctrl Pts',(17.9120801148581,21.6369266595076,8.32513087595513));
#139836=CARTESIAN_POINT('Ctrl Pts',(17.9925737212263,21.6612830598002,8.3293005902755));
#139837=CARTESIAN_POINT('Ctrl Pts',(18.0730644632865,21.6856385933875,8.33347015621954));
#139838=CARTESIAN_POINT('Ctrl Pts',(18.1547580100544,21.7060242799309,8.33763972216358));
#139839=CARTESIAN_POINT('Ctrl Pts',(18.2372280581079,21.7223378183249,8.34180928810762));
#139840=CARTESIAN_POINT('Ctrl Pts',(18.3225976513133,21.7392249206039,8.34612545084654));
#139841=CARTESIAN_POINT('Ctrl Pts',(18.4087988479274,21.7517480910506,8.35044161358546));
#139842=CARTESIAN_POINT('Ctrl Pts',(18.4953492973483,21.7598518674344,8.35475777632438));
#139843=CARTESIAN_POINT('Ctrl Pts',(18.5790803749828,21.7676916641549,8.35893334051606));
#139844=CARTESIAN_POINT('Ctrl Pts',(18.663137828366,21.7713955951849,8.36310890470775));
#139845=CARTESIAN_POINT('Ctrl Pts',(18.7470834485358,21.770966566847,8.36728446889943));
#139846=CARTESIAN_POINT('Ctrl Pts',(18.8352689624187,21.7705158693076,8.37167093091197));
#139847=CARTESIAN_POINT('Ctrl Pts',(18.923330465857,21.7655037616187,8.37605739292451));
#139848=CARTESIAN_POINT('Ctrl Pts',(19.0107666109437,21.7559951361578,8.38044385493705));
#139849=CARTESIAN_POINT('Ctrl Pts',(19.0982027560303,21.7464865106969,8.38483031694959));
#139850=CARTESIAN_POINT('Ctrl Pts',(19.1850129820694,21.7324815349687,8.38921677896212));
#139851=CARTESIAN_POINT('Ctrl Pts',(19.2707112385803,21.7141062794819,8.39360324097466));
#139852=CARTESIAN_POINT('Ctrl Pts',(19.352466391274,21.6965764967386,8.39778787536771));
#139853=CARTESIAN_POINT('Ctrl Pts',(19.4335139608229,21.6750045135588,8.40197250976077));
#139854=CARTESIAN_POINT('Ctrl Pts',(19.5134240199303,21.649462260761,8.40615714415381));
#139855=CARTESIAN_POINT('Ctrl Pts',(19.5932203369594,21.6239563641985,8.41033582223776));
#139856=CARTESIAN_POINT('Ctrl Pts',(19.671881925155,21.5944915619192,8.4145145003217));
#139857=CARTESIAN_POINT('Ctrl Pts',(19.7489895306432,21.5611906843243,8.41869317840565));
#139858=CARTESIAN_POINT('Ctrl Pts',(19.8274792345434,21.5272929124314,8.42294675629109));
#139859=CARTESIAN_POINT('Ctrl Pts',(19.9043582260683,21.489420290332,8.42720033417652));
#139860=CARTESIAN_POINT('Ctrl Pts',(19.9792009396775,21.447755377735,8.43145391206196));
#139861=CARTESIAN_POINT('Ctrl Pts',(20.0525926812398,21.4068982207711,8.43562502603991));
#139862=CARTESIAN_POINT('Ctrl Pts',(20.1240259742958,21.3623947371041,8.43979614001786));
#139863=CARTESIAN_POINT('Ctrl Pts',(20.1931217929876,21.3144646641265,8.44396725399581));
#139864=CARTESIAN_POINT('Ctrl Pts',(20.2621944259099,21.2665506745478,8.44813696831618));
#139865=CARTESIAN_POINT('Ctrl Pts',(20.3289307645448,21.215212641216,8.45230668263655));
#139866=CARTESIAN_POINT('Ctrl Pts',(20.3929803051521,21.1607139141724,8.45647639695692));
#139867=CARTESIAN_POINT('Ctrl Pts',(20.4570275666018,21.1062171264275,8.46064596290097));
#139868=CARTESIAN_POINT('Ctrl Pts',(20.5183878703047,21.0485601673606,8.464815528845));
#139869=CARTESIAN_POINT('Ctrl Pts',(20.5767444472639,20.9880461170375,8.46898509478905));
#139870=CARTESIAN_POINT('Ctrl Pts',(20.6371527694783,20.9254044673573,8.47330125752797));
#139871=CARTESIAN_POINT('Ctrl Pts',(20.6943418467815,20.859701457282,8.47761742026688));
#139872=CARTESIAN_POINT('Ctrl Pts',(20.7480039569823,20.7913126466809,8.48193358300581));
#139873=CARTESIAN_POINT('Ctrl Pts',(20.7999180295875,20.7251515943919,8.48610914719748));
#139874=CARTESIAN_POINT('Ctrl Pts',(20.8485311546646,20.6564774460931,8.49028471138917));
#139875=CARTESIAN_POINT('Ctrl Pts',(20.8936085817709,20.5856602393106,8.49446027558084));
#139876=CARTESIAN_POINT('Ctrl Pts',(20.940962762559,20.5112662237653,8.49884673759338));
#139877=CARTESIAN_POINT('Ctrl Pts',(20.9844143947686,20.4345074765788,8.50323319960592));
#139878=CARTESIAN_POINT('Ctrl Pts',(21.0237466725063,20.3558406770141,8.50761966161847));
#139879=CARTESIAN_POINT('Ctrl Pts',(21.0630789502441,20.2771738774495,8.51200612363101));
#139880=CARTESIAN_POINT('Ctrl Pts',(21.098291710861,20.1965995876304,8.51639258564355));
#139881=CARTESIAN_POINT('Ctrl Pts',(21.1292278697972,20.1145947386671,8.52077904765609));
#139882=CARTESIAN_POINT('Ctrl Pts',(21.1587406102023,20.0363630543649,8.52496368204914));
#139883=CARTESIAN_POINT('Ctrl Pts',(21.1844714983966,19.95653836908,8.52914831644219));
#139884=CARTESIAN_POINT('Ctrl Pts',(21.2062483053234,19.8755211184195,8.53333295083523));
#139885=CARTESIAN_POINT('Ctrl Pts',(21.227994115661,19.7946191857873,8.53751162891917));
#139886=CARTESIAN_POINT('Ctrl Pts',(21.2457969056054,19.7125284999515,8.54169030700312));
#139887=CARTESIAN_POINT('Ctrl Pts',(21.2595330219156,19.6296680728382,8.54586898508706));
#139888=CARTESIAN_POINT('Ctrl Pts',(21.2735153482386,19.5453224321195,8.5501225629725));
#139889=CARTESIAN_POINT('Ctrl Pts',(21.2832836065124,19.4601796345798,8.55437614085793));
#139890=CARTESIAN_POINT('Ctrl Pts',(21.288760950006,19.3746963295995,8.55862971874337));
#139891=CARTESIAN_POINT('Ctrl Pts',(21.2941321045079,19.2908702852932,8.56280083272132));
#139892=CARTESIAN_POINT('Ctrl Pts',(21.2953772042646,19.2067172987632,8.56697194669928));
#139893=CARTESIAN_POINT('Ctrl Pts',(21.2924758541409,19.1226750104568,8.57114306067723));
#139894=CARTESIAN_POINT('Ctrl Pts',(21.2895754775933,19.0386609233518,8.57531277499761));
#139895=CARTESIAN_POINT('Ctrl Pts',(21.2825314303294,18.9547579200746,8.57948248931798));
#139896=CARTESIAN_POINT('Ctrl Pts',(21.2713754270314,18.8714032651847,8.58365220363836));
#139897=CARTESIAN_POINT('Ctrl Pts',(21.2602198207119,18.7880515764115,8.58782176958239));
#139898=CARTESIAN_POINT('Ctrl Pts',(21.2449526111525,18.7052486530838,8.59199133552643));
#139899=CARTESIAN_POINT('Ctrl Pts',(21.2256571796749,18.6234248992897,8.59616090147046));
#139900=CARTESIAN_POINT('Ctrl Pts',(21.20568334463,18.5387243232526,8.60047706420938));
#139901=CARTESIAN_POINT('Ctrl Pts',(21.181392873751,18.4550735664106,8.60479322694831));
#139902=CARTESIAN_POINT('Ctrl Pts',(21.1529349892687,18.3729346578627,8.60910938968723));
#139903=CARTESIAN_POINT('Ctrl Pts',(21.1254041173801,18.2934714156214,8.61328495387891));
#139904=CARTESIAN_POINT('Ctrl Pts',(21.0939733891638,18.2154234566595,8.61746051807059));
#139905=CARTESIAN_POINT('Ctrl Pts',(21.0588268816573,18.1391884632437,8.62163608226227));
#139906=CARTESIAN_POINT('Ctrl Pts',(21.0219052076094,18.0591030215419,8.62602254427481));
#139907=CARTESIAN_POINT('Ctrl Pts',(20.9808827929503,17.9810190212162,8.63040900628736));
#139908=CARTESIAN_POINT('Ctrl Pts',(20.9360262797511,17.9053659535362,8.6347954682999));
#139909=CARTESIAN_POINT('Ctrl Pts',(20.891169766552,17.8297128858561,8.63918193031245));
#139910=CARTESIAN_POINT('Ctrl Pts',(20.842479539431,17.7564911918507,8.64356839232499));
#139911=CARTESIAN_POINT('Ctrl Pts',(20.790271595083,17.6860911085397,8.64795485433753));
#139912=CARTESIAN_POINT('Ctrl Pts',(20.7404694331042,17.6189351154018,8.65213918479511));
#139913=CARTESIAN_POINT('Ctrl Pts',(20.6872812569781,17.5540964632771,8.65632351525269));
#139914=CARTESIAN_POINT('Ctrl Pts',(20.6309504906906,17.4919366399494,8.66050784571027));
#139915=CARTESIAN_POINT('Ctrl Pts',(20.5747060923848,17.4298721218843,8.66468576062977));
#139916=CARTESIAN_POINT('Ctrl Pts',(20.5153289851675,17.3704786083014,8.66886367554927));
#139917=CARTESIAN_POINT('Ctrl Pts',(20.4531043975747,17.3140866993351,8.67304159046877));
#139918=CARTESIAN_POINT('Ctrl Pts',(20.4017904485504,17.2675827102526,8.67648693774226));
#139919=CARTESIAN_POINT('Ctrl Pts',(20.3485409039237,17.2231195485426,8.67993228501575));
#139920=CARTESIAN_POINT('Ctrl Pts',(20.2935357313021,17.1808649545431,8.68337763228924));
#139921=CARTESIAN_POINT('Origin',(18.734,19.211,-1.76670989022852));
#139922=CARTESIAN_POINT('',(20.2954164566376,17.1783794293288,9.5499633233039));
#139923=CARTESIAN_POINT('',(20.2935357313021,17.1808649545431,9.48328065833267));
#139924=CARTESIAN_POINT('',(20.2935357313021,17.1808649545432,-1.76670989022852));
#139925=CARTESIAN_POINT('',(16.1736699135442,19.2103574886798,9.03329016588334));
#139926=CARTESIAN_POINT('Ctrl Pts',(16.1699656655267,19.2103691596404,9.03329079541918));
#139927=CARTESIAN_POINT('Ctrl Pts',(16.1727141287504,20.0241270866321,9.07394170533784));
#139928=CARTESIAN_POINT('Ctrl Pts',(17.0319371680896,21.691475877328,9.15698455081697));
#139929=CARTESIAN_POINT('Ctrl Pts',(19.8732646807496,22.0155260890916,9.28241933185656));
#139930=CARTESIAN_POINT('Ctrl Pts',(21.7088249788763,19.7710954760151,9.40959513853801));
#139931=CARTESIAN_POINT('Ctrl Pts',(21.0821529672139,17.8368644753459,9.49877646902045));
#139932=CARTESIAN_POINT('Ctrl Pts',(20.3656977297167,17.2315280348845,9.54556586394241));
#139933=CARTESIAN_POINT('Ctrl Pts',(20.2954164566376,17.1783794293288,9.5499633233039));
